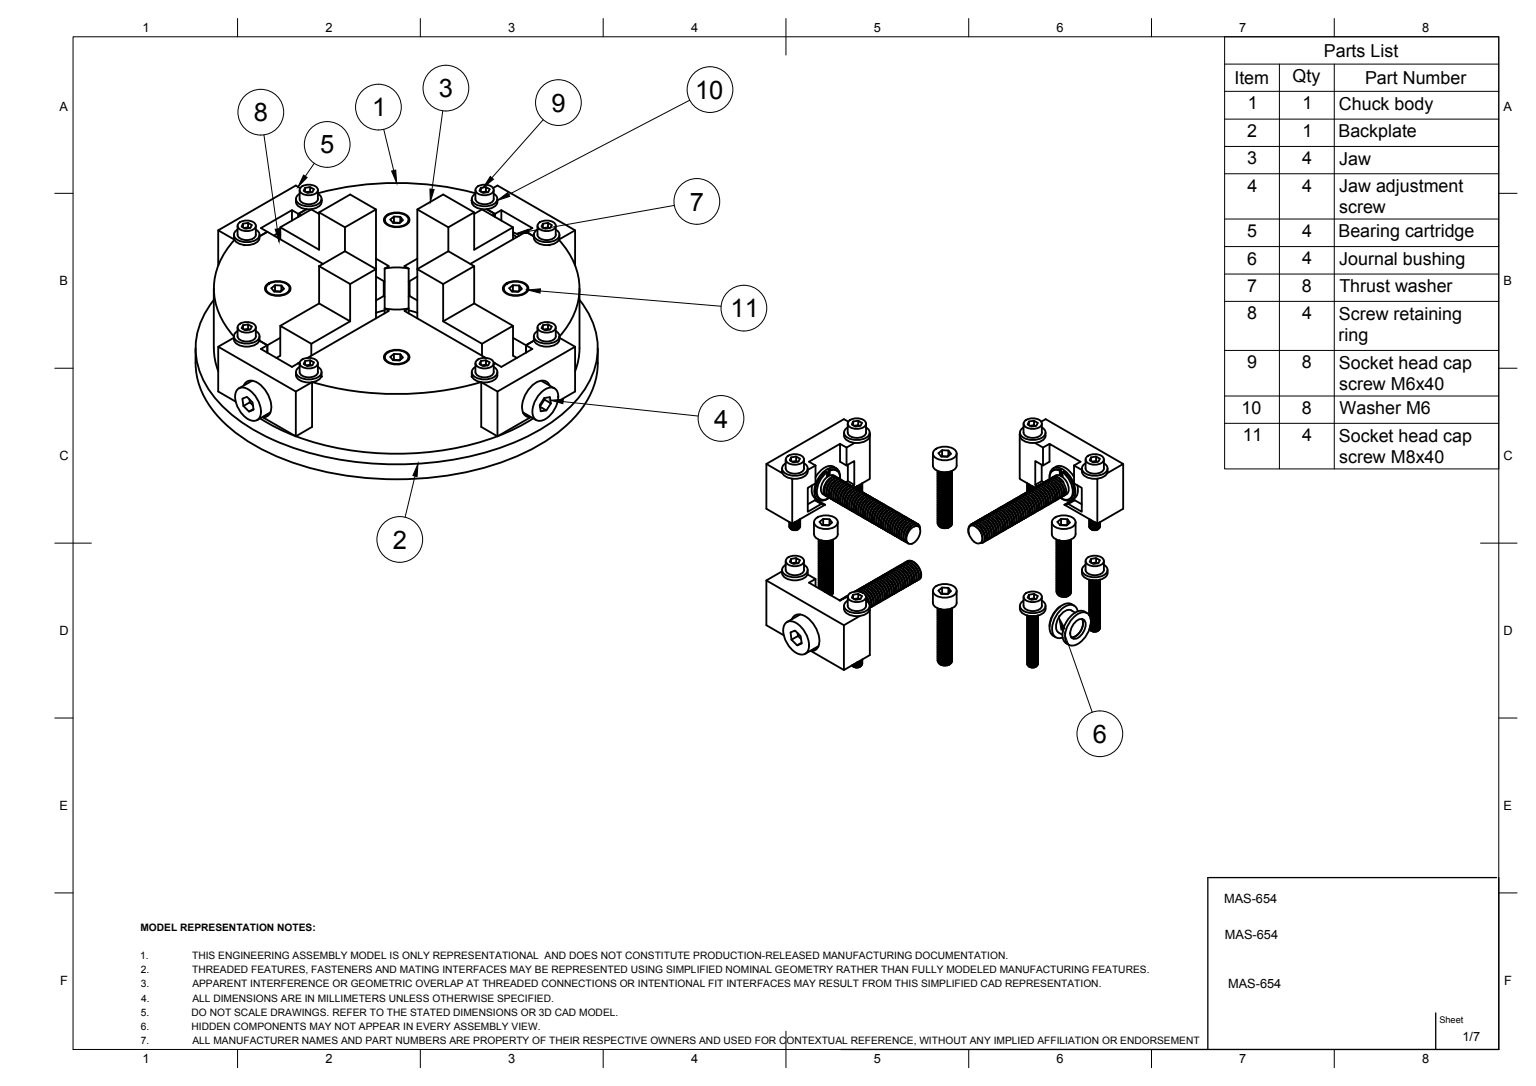
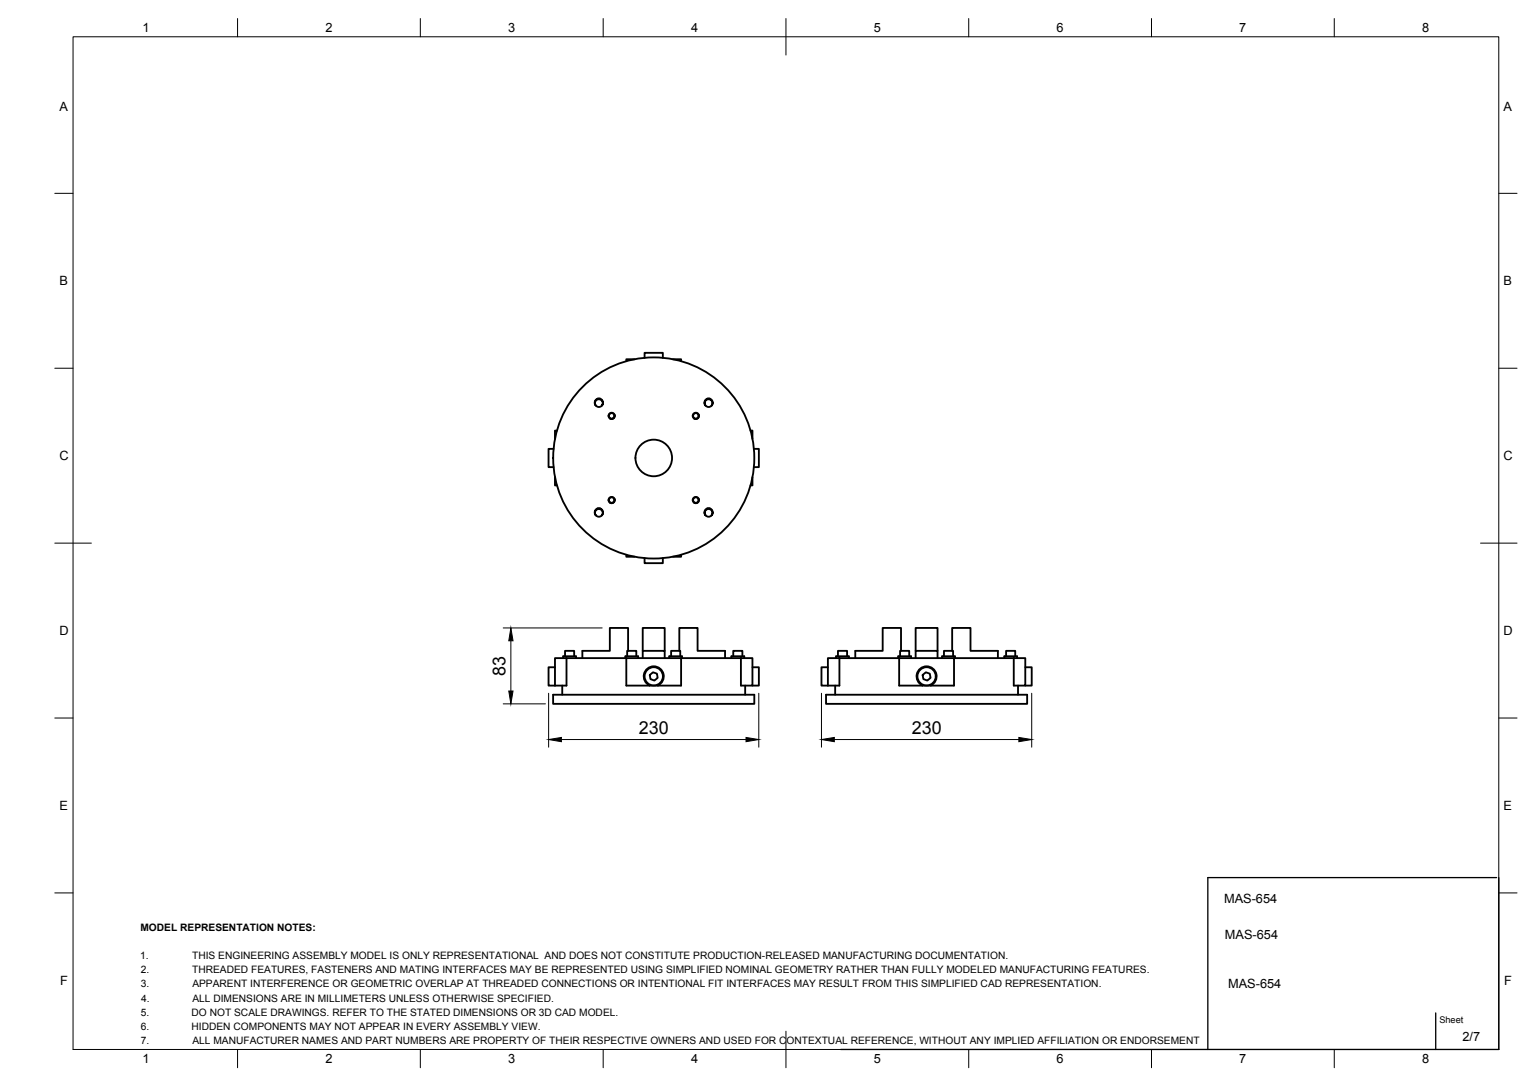
ISO-10303-21;
HEADER;
/* Generated by software containing ST-Developer
 * from STEP Tools, Inc. (www.steptools.com) 
 */

FILE_DESCRIPTION(
/* description */ ('Independent four-jaw lathe chuck,200mm body,40mm bore,36\X2\2013\X0\7
6mm nominal opposed jaw opening. Four shared machined T-jaws and model
ed partial M12x1.75 feed screws, native independent screw/slider links
, removable bolted bronze-bearing cartridges, fully captured ring/wash
er/head thrust stacks and registered bolted backplate. Custom spindle 
interface; no compatibility, speed, grip force or safety rating assign
ed.'),
/* implementation_level */ '2;1');

FILE_NAME(
/* name */ 'MAS-654.step',
/* time_stamp */ '2026-11-09T20:24:54-08:00',
/* author */ (''),
/* organization */ (''),
/* preprocessor_version */ 'ST-DEVELOPER v20.2',
/* originating_system */ 'Autodesk Translation Framework v15.17.0.0',
/* authorisation */ '');

FILE_SCHEMA (('AUTOMOTIVE_DESIGN { 1 0 10303 214 3 1 1 }'));
ENDSEC;

DATA;
#10=MECHANICAL_DESIGN_GEOMETRIC_PRESENTATION_REPRESENTATION('',(#236,#237,
#238,#239,#240,#241,#242,#243,#244,#245,#246),#69491);
#11=ITEM_DEFINED_TRANSFORMATION($,$,#14865,#15813);
#12=ITEM_DEFINED_TRANSFORMATION($,$,#15193,#15814);
#13=ITEM_DEFINED_TRANSFORMATION($,$,#15370,#15815);
#14=ITEM_DEFINED_TRANSFORMATION($,$,#15482,#15816);
#15=ITEM_DEFINED_TRANSFORMATION($,$,#15446,#15817);
#16=ITEM_DEFINED_TRANSFORMATION($,$,#15597,#15818);
#17=ITEM_DEFINED_TRANSFORMATION($,$,#15606,#15819);
#18=ITEM_DEFINED_TRANSFORMATION($,$,#15586,#15820);
#19=ITEM_DEFINED_TRANSFORMATION($,$,#15615,#15821);
#20=ITEM_DEFINED_TRANSFORMATION($,$,#15715,#15822);
#21=ITEM_DEFINED_TRANSFORMATION($,$,#15724,#15823);
#22=ITEM_DEFINED_TRANSFORMATION($,$,#15606,#15824);
#23=ITEM_DEFINED_TRANSFORMATION($,$,#15615,#15825);
#24=ITEM_DEFINED_TRANSFORMATION($,$,#15715,#15826);
#25=ITEM_DEFINED_TRANSFORMATION($,$,#15370,#15827);
#26=ITEM_DEFINED_TRANSFORMATION($,$,#15446,#15828);
#27=ITEM_DEFINED_TRANSFORMATION($,$,#15482,#15829);
#28=ITEM_DEFINED_TRANSFORMATION($,$,#15586,#15830);
#29=ITEM_DEFINED_TRANSFORMATION($,$,#15597,#15831);
#30=ITEM_DEFINED_TRANSFORMATION($,$,#15606,#15832);
#31=ITEM_DEFINED_TRANSFORMATION($,$,#15606,#15833);
#32=ITEM_DEFINED_TRANSFORMATION($,$,#15615,#15834);
#33=ITEM_DEFINED_TRANSFORMATION($,$,#15715,#15835);
#34=ITEM_DEFINED_TRANSFORMATION($,$,#15615,#15836);
#35=ITEM_DEFINED_TRANSFORMATION($,$,#15715,#15837);
#36=ITEM_DEFINED_TRANSFORMATION($,$,#15370,#15838);
#37=ITEM_DEFINED_TRANSFORMATION($,$,#15446,#15839);
#38=ITEM_DEFINED_TRANSFORMATION($,$,#15482,#15840);
#39=ITEM_DEFINED_TRANSFORMATION($,$,#15586,#15841);
#40=ITEM_DEFINED_TRANSFORMATION($,$,#15597,#15842);
#41=ITEM_DEFINED_TRANSFORMATION($,$,#15606,#15843);
#42=ITEM_DEFINED_TRANSFORMATION($,$,#15606,#15844);
#43=ITEM_DEFINED_TRANSFORMATION($,$,#15615,#15845);
#44=ITEM_DEFINED_TRANSFORMATION($,$,#15715,#15846);
#45=ITEM_DEFINED_TRANSFORMATION($,$,#15615,#15847);
#46=ITEM_DEFINED_TRANSFORMATION($,$,#15715,#15848);
#47=ITEM_DEFINED_TRANSFORMATION($,$,#15370,#15849);
#48=ITEM_DEFINED_TRANSFORMATION($,$,#15446,#15850);
#49=ITEM_DEFINED_TRANSFORMATION($,$,#15482,#15851);
#50=ITEM_DEFINED_TRANSFORMATION($,$,#15586,#15852);
#51=ITEM_DEFINED_TRANSFORMATION($,$,#15597,#15853);
#52=ITEM_DEFINED_TRANSFORMATION($,$,#15606,#15854);
#53=ITEM_DEFINED_TRANSFORMATION($,$,#15606,#15855);
#54=ITEM_DEFINED_TRANSFORMATION($,$,#15615,#15856);
#55=ITEM_DEFINED_TRANSFORMATION($,$,#15715,#15857);
#56=ITEM_DEFINED_TRANSFORMATION($,$,#15615,#15858);
#57=ITEM_DEFINED_TRANSFORMATION($,$,#15715,#15859);
#58=ITEM_DEFINED_TRANSFORMATION($,$,#15724,#15860);
#59=ITEM_DEFINED_TRANSFORMATION($,$,#15724,#15861);
#60=ITEM_DEFINED_TRANSFORMATION($,$,#15724,#15862);
#61=(
REPRESENTATION_RELATIONSHIP($,$,#69571,#69570)
REPRESENTATION_RELATIONSHIP_WITH_TRANSFORMATION(#11)
SHAPE_REPRESENTATION_RELATIONSHIP()
);
#62=(
REPRESENTATION_RELATIONSHIP($,$,#69572,#69570)
REPRESENTATION_RELATIONSHIP_WITH_TRANSFORMATION(#12)
SHAPE_REPRESENTATION_RELATIONSHIP()
);
#63=(
REPRESENTATION_RELATIONSHIP($,$,#69573,#69570)
REPRESENTATION_RELATIONSHIP_WITH_TRANSFORMATION(#13)
SHAPE_REPRESENTATION_RELATIONSHIP()
);
#64=(
REPRESENTATION_RELATIONSHIP($,$,#69575,#69570)
REPRESENTATION_RELATIONSHIP_WITH_TRANSFORMATION(#14)
SHAPE_REPRESENTATION_RELATIONSHIP()
);
#65=(
REPRESENTATION_RELATIONSHIP($,$,#69574,#69570)
REPRESENTATION_RELATIONSHIP_WITH_TRANSFORMATION(#15)
SHAPE_REPRESENTATION_RELATIONSHIP()
);
#66=(
REPRESENTATION_RELATIONSHIP($,$,#69577,#69570)
REPRESENTATION_RELATIONSHIP_WITH_TRANSFORMATION(#16)
SHAPE_REPRESENTATION_RELATIONSHIP()
);
#67=(
REPRESENTATION_RELATIONSHIP($,$,#69578,#69570)
REPRESENTATION_RELATIONSHIP_WITH_TRANSFORMATION(#17)
SHAPE_REPRESENTATION_RELATIONSHIP()
);
#68=(
REPRESENTATION_RELATIONSHIP($,$,#69576,#69570)
REPRESENTATION_RELATIONSHIP_WITH_TRANSFORMATION(#18)
SHAPE_REPRESENTATION_RELATIONSHIP()
);
#69=(
REPRESENTATION_RELATIONSHIP($,$,#69579,#69570)
REPRESENTATION_RELATIONSHIP_WITH_TRANSFORMATION(#19)
SHAPE_REPRESENTATION_RELATIONSHIP()
);
#70=(
REPRESENTATION_RELATIONSHIP($,$,#69580,#69570)
REPRESENTATION_RELATIONSHIP_WITH_TRANSFORMATION(#20)
SHAPE_REPRESENTATION_RELATIONSHIP()
);
#71=(
REPRESENTATION_RELATIONSHIP($,$,#69581,#69570)
REPRESENTATION_RELATIONSHIP_WITH_TRANSFORMATION(#21)
SHAPE_REPRESENTATION_RELATIONSHIP()
);
#72=(
REPRESENTATION_RELATIONSHIP($,$,#69578,#69570)
REPRESENTATION_RELATIONSHIP_WITH_TRANSFORMATION(#22)
SHAPE_REPRESENTATION_RELATIONSHIP()
);
#73=(
REPRESENTATION_RELATIONSHIP($,$,#69579,#69570)
REPRESENTATION_RELATIONSHIP_WITH_TRANSFORMATION(#23)
SHAPE_REPRESENTATION_RELATIONSHIP()
);
#74=(
REPRESENTATION_RELATIONSHIP($,$,#69580,#69570)
REPRESENTATION_RELATIONSHIP_WITH_TRANSFORMATION(#24)
SHAPE_REPRESENTATION_RELATIONSHIP()
);
#75=(
REPRESENTATION_RELATIONSHIP($,$,#69573,#69570)
REPRESENTATION_RELATIONSHIP_WITH_TRANSFORMATION(#25)
SHAPE_REPRESENTATION_RELATIONSHIP()
);
#76=(
REPRESENTATION_RELATIONSHIP($,$,#69574,#69570)
REPRESENTATION_RELATIONSHIP_WITH_TRANSFORMATION(#26)
SHAPE_REPRESENTATION_RELATIONSHIP()
);
#77=(
REPRESENTATION_RELATIONSHIP($,$,#69575,#69570)
REPRESENTATION_RELATIONSHIP_WITH_TRANSFORMATION(#27)
SHAPE_REPRESENTATION_RELATIONSHIP()
);
#78=(
REPRESENTATION_RELATIONSHIP($,$,#69576,#69570)
REPRESENTATION_RELATIONSHIP_WITH_TRANSFORMATION(#28)
SHAPE_REPRESENTATION_RELATIONSHIP()
);
#79=(
REPRESENTATION_RELATIONSHIP($,$,#69577,#69570)
REPRESENTATION_RELATIONSHIP_WITH_TRANSFORMATION(#29)
SHAPE_REPRESENTATION_RELATIONSHIP()
);
#80=(
REPRESENTATION_RELATIONSHIP($,$,#69578,#69570)
REPRESENTATION_RELATIONSHIP_WITH_TRANSFORMATION(#30)
SHAPE_REPRESENTATION_RELATIONSHIP()
);
#81=(
REPRESENTATION_RELATIONSHIP($,$,#69578,#69570)
REPRESENTATION_RELATIONSHIP_WITH_TRANSFORMATION(#31)
SHAPE_REPRESENTATION_RELATIONSHIP()
);
#82=(
REPRESENTATION_RELATIONSHIP($,$,#69579,#69570)
REPRESENTATION_RELATIONSHIP_WITH_TRANSFORMATION(#32)
SHAPE_REPRESENTATION_RELATIONSHIP()
);
#83=(
REPRESENTATION_RELATIONSHIP($,$,#69580,#69570)
REPRESENTATION_RELATIONSHIP_WITH_TRANSFORMATION(#33)
SHAPE_REPRESENTATION_RELATIONSHIP()
);
#84=(
REPRESENTATION_RELATIONSHIP($,$,#69579,#69570)
REPRESENTATION_RELATIONSHIP_WITH_TRANSFORMATION(#34)
SHAPE_REPRESENTATION_RELATIONSHIP()
);
#85=(
REPRESENTATION_RELATIONSHIP($,$,#69580,#69570)
REPRESENTATION_RELATIONSHIP_WITH_TRANSFORMATION(#35)
SHAPE_REPRESENTATION_RELATIONSHIP()
);
#86=(
REPRESENTATION_RELATIONSHIP($,$,#69573,#69570)
REPRESENTATION_RELATIONSHIP_WITH_TRANSFORMATION(#36)
SHAPE_REPRESENTATION_RELATIONSHIP()
);
#87=(
REPRESENTATION_RELATIONSHIP($,$,#69574,#69570)
REPRESENTATION_RELATIONSHIP_WITH_TRANSFORMATION(#37)
SHAPE_REPRESENTATION_RELATIONSHIP()
);
#88=(
REPRESENTATION_RELATIONSHIP($,$,#69575,#69570)
REPRESENTATION_RELATIONSHIP_WITH_TRANSFORMATION(#38)
SHAPE_REPRESENTATION_RELATIONSHIP()
);
#89=(
REPRESENTATION_RELATIONSHIP($,$,#69576,#69570)
REPRESENTATION_RELATIONSHIP_WITH_TRANSFORMATION(#39)
SHAPE_REPRESENTATION_RELATIONSHIP()
);
#90=(
REPRESENTATION_RELATIONSHIP($,$,#69577,#69570)
REPRESENTATION_RELATIONSHIP_WITH_TRANSFORMATION(#40)
SHAPE_REPRESENTATION_RELATIONSHIP()
);
#91=(
REPRESENTATION_RELATIONSHIP($,$,#69578,#69570)
REPRESENTATION_RELATIONSHIP_WITH_TRANSFORMATION(#41)
SHAPE_REPRESENTATION_RELATIONSHIP()
);
#92=(
REPRESENTATION_RELATIONSHIP($,$,#69578,#69570)
REPRESENTATION_RELATIONSHIP_WITH_TRANSFORMATION(#42)
SHAPE_REPRESENTATION_RELATIONSHIP()
);
#93=(
REPRESENTATION_RELATIONSHIP($,$,#69579,#69570)
REPRESENTATION_RELATIONSHIP_WITH_TRANSFORMATION(#43)
SHAPE_REPRESENTATION_RELATIONSHIP()
);
#94=(
REPRESENTATION_RELATIONSHIP($,$,#69580,#69570)
REPRESENTATION_RELATIONSHIP_WITH_TRANSFORMATION(#44)
SHAPE_REPRESENTATION_RELATIONSHIP()
);
#95=(
REPRESENTATION_RELATIONSHIP($,$,#69579,#69570)
REPRESENTATION_RELATIONSHIP_WITH_TRANSFORMATION(#45)
SHAPE_REPRESENTATION_RELATIONSHIP()
);
#96=(
REPRESENTATION_RELATIONSHIP($,$,#69580,#69570)
REPRESENTATION_RELATIONSHIP_WITH_TRANSFORMATION(#46)
SHAPE_REPRESENTATION_RELATIONSHIP()
);
#97=(
REPRESENTATION_RELATIONSHIP($,$,#69573,#69570)
REPRESENTATION_RELATIONSHIP_WITH_TRANSFORMATION(#47)
SHAPE_REPRESENTATION_RELATIONSHIP()
);
#98=(
REPRESENTATION_RELATIONSHIP($,$,#69574,#69570)
REPRESENTATION_RELATIONSHIP_WITH_TRANSFORMATION(#48)
SHAPE_REPRESENTATION_RELATIONSHIP()
);
#99=(
REPRESENTATION_RELATIONSHIP($,$,#69575,#69570)
REPRESENTATION_RELATIONSHIP_WITH_TRANSFORMATION(#49)
SHAPE_REPRESENTATION_RELATIONSHIP()
);
#100=(
REPRESENTATION_RELATIONSHIP($,$,#69576,#69570)
REPRESENTATION_RELATIONSHIP_WITH_TRANSFORMATION(#50)
SHAPE_REPRESENTATION_RELATIONSHIP()
);
#101=(
REPRESENTATION_RELATIONSHIP($,$,#69577,#69570)
REPRESENTATION_RELATIONSHIP_WITH_TRANSFORMATION(#51)
SHAPE_REPRESENTATION_RELATIONSHIP()
);
#102=(
REPRESENTATION_RELATIONSHIP($,$,#69578,#69570)
REPRESENTATION_RELATIONSHIP_WITH_TRANSFORMATION(#52)
SHAPE_REPRESENTATION_RELATIONSHIP()
);
#103=(
REPRESENTATION_RELATIONSHIP($,$,#69578,#69570)
REPRESENTATION_RELATIONSHIP_WITH_TRANSFORMATION(#53)
SHAPE_REPRESENTATION_RELATIONSHIP()
);
#104=(
REPRESENTATION_RELATIONSHIP($,$,#69579,#69570)
REPRESENTATION_RELATIONSHIP_WITH_TRANSFORMATION(#54)
SHAPE_REPRESENTATION_RELATIONSHIP()
);
#105=(
REPRESENTATION_RELATIONSHIP($,$,#69580,#69570)
REPRESENTATION_RELATIONSHIP_WITH_TRANSFORMATION(#55)
SHAPE_REPRESENTATION_RELATIONSHIP()
);
#106=(
REPRESENTATION_RELATIONSHIP($,$,#69579,#69570)
REPRESENTATION_RELATIONSHIP_WITH_TRANSFORMATION(#56)
SHAPE_REPRESENTATION_RELATIONSHIP()
);
#107=(
REPRESENTATION_RELATIONSHIP($,$,#69580,#69570)
REPRESENTATION_RELATIONSHIP_WITH_TRANSFORMATION(#57)
SHAPE_REPRESENTATION_RELATIONSHIP()
);
#108=(
REPRESENTATION_RELATIONSHIP($,$,#69581,#69570)
REPRESENTATION_RELATIONSHIP_WITH_TRANSFORMATION(#58)
SHAPE_REPRESENTATION_RELATIONSHIP()
);
#109=(
REPRESENTATION_RELATIONSHIP($,$,#69581,#69570)
REPRESENTATION_RELATIONSHIP_WITH_TRANSFORMATION(#59)
SHAPE_REPRESENTATION_RELATIONSHIP()
);
#110=(
REPRESENTATION_RELATIONSHIP($,$,#69581,#69570)
REPRESENTATION_RELATIONSHIP_WITH_TRANSFORMATION(#60)
SHAPE_REPRESENTATION_RELATIONSHIP()
);
#111=CONTEXT_DEPENDENT_SHAPE_REPRESENTATION(#61,#69520);
#112=CONTEXT_DEPENDENT_SHAPE_REPRESENTATION(#62,#69521);
#113=CONTEXT_DEPENDENT_SHAPE_REPRESENTATION(#63,#69522);
#114=CONTEXT_DEPENDENT_SHAPE_REPRESENTATION(#64,#69523);
#115=CONTEXT_DEPENDENT_SHAPE_REPRESENTATION(#65,#69524);
#116=CONTEXT_DEPENDENT_SHAPE_REPRESENTATION(#66,#69525);
#117=CONTEXT_DEPENDENT_SHAPE_REPRESENTATION(#67,#69526);
#118=CONTEXT_DEPENDENT_SHAPE_REPRESENTATION(#68,#69527);
#119=CONTEXT_DEPENDENT_SHAPE_REPRESENTATION(#69,#69528);
#120=CONTEXT_DEPENDENT_SHAPE_REPRESENTATION(#70,#69529);
#121=CONTEXT_DEPENDENT_SHAPE_REPRESENTATION(#71,#69530);
#122=CONTEXT_DEPENDENT_SHAPE_REPRESENTATION(#72,#69531);
#123=CONTEXT_DEPENDENT_SHAPE_REPRESENTATION(#73,#69532);
#124=CONTEXT_DEPENDENT_SHAPE_REPRESENTATION(#74,#69533);
#125=CONTEXT_DEPENDENT_SHAPE_REPRESENTATION(#75,#69534);
#126=CONTEXT_DEPENDENT_SHAPE_REPRESENTATION(#76,#69535);
#127=CONTEXT_DEPENDENT_SHAPE_REPRESENTATION(#77,#69536);
#128=CONTEXT_DEPENDENT_SHAPE_REPRESENTATION(#78,#69537);
#129=CONTEXT_DEPENDENT_SHAPE_REPRESENTATION(#79,#69538);
#130=CONTEXT_DEPENDENT_SHAPE_REPRESENTATION(#80,#69539);
#131=CONTEXT_DEPENDENT_SHAPE_REPRESENTATION(#81,#69540);
#132=CONTEXT_DEPENDENT_SHAPE_REPRESENTATION(#82,#69541);
#133=CONTEXT_DEPENDENT_SHAPE_REPRESENTATION(#83,#69542);
#134=CONTEXT_DEPENDENT_SHAPE_REPRESENTATION(#84,#69543);
#135=CONTEXT_DEPENDENT_SHAPE_REPRESENTATION(#85,#69544);
#136=CONTEXT_DEPENDENT_SHAPE_REPRESENTATION(#86,#69545);
#137=CONTEXT_DEPENDENT_SHAPE_REPRESENTATION(#87,#69546);
#138=CONTEXT_DEPENDENT_SHAPE_REPRESENTATION(#88,#69547);
#139=CONTEXT_DEPENDENT_SHAPE_REPRESENTATION(#89,#69548);
#140=CONTEXT_DEPENDENT_SHAPE_REPRESENTATION(#90,#69549);
#141=CONTEXT_DEPENDENT_SHAPE_REPRESENTATION(#91,#69550);
#142=CONTEXT_DEPENDENT_SHAPE_REPRESENTATION(#92,#69551);
#143=CONTEXT_DEPENDENT_SHAPE_REPRESENTATION(#93,#69552);
#144=CONTEXT_DEPENDENT_SHAPE_REPRESENTATION(#94,#69553);
#145=CONTEXT_DEPENDENT_SHAPE_REPRESENTATION(#95,#69554);
#146=CONTEXT_DEPENDENT_SHAPE_REPRESENTATION(#96,#69555);
#147=CONTEXT_DEPENDENT_SHAPE_REPRESENTATION(#97,#69556);
#148=CONTEXT_DEPENDENT_SHAPE_REPRESENTATION(#98,#69557);
#149=CONTEXT_DEPENDENT_SHAPE_REPRESENTATION(#99,#69558);
#150=CONTEXT_DEPENDENT_SHAPE_REPRESENTATION(#100,#69559);
#151=CONTEXT_DEPENDENT_SHAPE_REPRESENTATION(#101,#69560);
#152=CONTEXT_DEPENDENT_SHAPE_REPRESENTATION(#102,#69561);
#153=CONTEXT_DEPENDENT_SHAPE_REPRESENTATION(#103,#69562);
#154=CONTEXT_DEPENDENT_SHAPE_REPRESENTATION(#104,#69563);
#155=CONTEXT_DEPENDENT_SHAPE_REPRESENTATION(#105,#69564);
#156=CONTEXT_DEPENDENT_SHAPE_REPRESENTATION(#106,#69565);
#157=CONTEXT_DEPENDENT_SHAPE_REPRESENTATION(#107,#69566);
#158=CONTEXT_DEPENDENT_SHAPE_REPRESENTATION(#108,#69567);
#159=CONTEXT_DEPENDENT_SHAPE_REPRESENTATION(#109,#69568);
#160=CONTEXT_DEPENDENT_SHAPE_REPRESENTATION(#110,#69569);
#161=NEXT_ASSEMBLY_USAGE_OCCURRENCE('Chuck body:1','Chuck body:1',
'Chuck body:1',#69583,#69584,'Chuck body:1');
#162=NEXT_ASSEMBLY_USAGE_OCCURRENCE('Backplate:1','Backplate:1',
'Backplate:1',#69583,#69585,'Backplate:1');
#163=NEXT_ASSEMBLY_USAGE_OCCURRENCE('Jaw:1','Jaw:1','Jaw:1',#69583,#69586,
'Jaw:1');
#164=NEXT_ASSEMBLY_USAGE_OCCURRENCE('Jaw adjustment screw:1',
'Jaw adjustment screw:1','Jaw adjustment screw:1',#69583,#69588,
'Jaw adjustment screw:1');
#165=NEXT_ASSEMBLY_USAGE_OCCURRENCE('Bearing cartridge:1',
'Bearing cartridge:1','Bearing cartridge:1',#69583,#69587,
'Bearing cartridge:1');
#166=NEXT_ASSEMBLY_USAGE_OCCURRENCE('Journal bushing:1',
'Journal bushing:1','Journal bushing:1',#69583,#69590,
'Journal bushing:1');
#167=NEXT_ASSEMBLY_USAGE_OCCURRENCE('Thrust washer:1','Thrust washer:1',
'Thrust washer:1',#69583,#69591,'Thrust washer:1');
#168=NEXT_ASSEMBLY_USAGE_OCCURRENCE('Screw retaining ring:1',
'Screw retaining ring:1','Screw retaining ring:1',#69583,#69589,
'Screw retaining ring:1');
#169=NEXT_ASSEMBLY_USAGE_OCCURRENCE('Socket head cap screw M6x40:1',
'Socket head cap screw M6x40:1','Socket head cap screw M6x40:1',#69583,
#69592,'Socket head cap screw M6x40:1');
#170=NEXT_ASSEMBLY_USAGE_OCCURRENCE('Washer M6:1','Washer M6:1',
'Washer M6:1',#69583,#69593,'Washer M6:1');
#171=NEXT_ASSEMBLY_USAGE_OCCURRENCE('Socket head cap screw M8x40:1',
'Socket head cap screw M8x40:1','Socket head cap screw M8x40:1',#69583,
#69594,'Socket head cap screw M8x40:1');
#172=NEXT_ASSEMBLY_USAGE_OCCURRENCE('Thrust washer:2','Thrust washer:2',
'Thrust washer:2',#69583,#69591,'Thrust washer:2');
#173=NEXT_ASSEMBLY_USAGE_OCCURRENCE('Socket head cap screw M6x40:2',
'Socket head cap screw M6x40:2','Socket head cap screw M6x40:2',#69583,
#69592,'Socket head cap screw M6x40:2');
#174=NEXT_ASSEMBLY_USAGE_OCCURRENCE('Washer M6:2','Washer M6:2',
'Washer M6:2',#69583,#69593,'Washer M6:2');
#175=NEXT_ASSEMBLY_USAGE_OCCURRENCE('Jaw:2','Jaw:2','Jaw:2',#69583,#69586,
'Jaw:2');
#176=NEXT_ASSEMBLY_USAGE_OCCURRENCE('Bearing cartridge:2',
'Bearing cartridge:2','Bearing cartridge:2',#69583,#69587,
'Bearing cartridge:2');
#177=NEXT_ASSEMBLY_USAGE_OCCURRENCE('Jaw adjustment screw:2',
'Jaw adjustment screw:2','Jaw adjustment screw:2',#69583,#69588,
'Jaw adjustment screw:2');
#178=NEXT_ASSEMBLY_USAGE_OCCURRENCE('Screw retaining ring:2',
'Screw retaining ring:2','Screw retaining ring:2',#69583,#69589,
'Screw retaining ring:2');
#179=NEXT_ASSEMBLY_USAGE_OCCURRENCE('Journal bushing:2',
'Journal bushing:2','Journal bushing:2',#69583,#69590,
'Journal bushing:2');
#180=NEXT_ASSEMBLY_USAGE_OCCURRENCE('Thrust washer:3','Thrust washer:3',
'Thrust washer:3',#69583,#69591,'Thrust washer:3');
#181=NEXT_ASSEMBLY_USAGE_OCCURRENCE('Thrust washer:4','Thrust washer:4',
'Thrust washer:4',#69583,#69591,'Thrust washer:4');
#182=NEXT_ASSEMBLY_USAGE_OCCURRENCE('Socket head cap screw M6x40:3',
'Socket head cap screw M6x40:3','Socket head cap screw M6x40:3',#69583,
#69592,'Socket head cap screw M6x40:3');
#183=NEXT_ASSEMBLY_USAGE_OCCURRENCE('Washer M6:3','Washer M6:3',
'Washer M6:3',#69583,#69593,'Washer M6:3');
#184=NEXT_ASSEMBLY_USAGE_OCCURRENCE('Socket head cap screw M6x40:4',
'Socket head cap screw M6x40:4','Socket head cap screw M6x40:4',#69583,
#69592,'Socket head cap screw M6x40:4');
#185=NEXT_ASSEMBLY_USAGE_OCCURRENCE('Washer M6:4','Washer M6:4',
'Washer M6:4',#69583,#69593,'Washer M6:4');
#186=NEXT_ASSEMBLY_USAGE_OCCURRENCE('Jaw:3','Jaw:3','Jaw:3',#69583,#69586,
'Jaw:3');
#187=NEXT_ASSEMBLY_USAGE_OCCURRENCE('Bearing cartridge:3',
'Bearing cartridge:3','Bearing cartridge:3',#69583,#69587,
'Bearing cartridge:3');
#188=NEXT_ASSEMBLY_USAGE_OCCURRENCE('Jaw adjustment screw:3',
'Jaw adjustment screw:3','Jaw adjustment screw:3',#69583,#69588,
'Jaw adjustment screw:3');
#189=NEXT_ASSEMBLY_USAGE_OCCURRENCE('Screw retaining ring:3',
'Screw retaining ring:3','Screw retaining ring:3',#69583,#69589,
'Screw retaining ring:3');
#190=NEXT_ASSEMBLY_USAGE_OCCURRENCE('Journal bushing:3',
'Journal bushing:3','Journal bushing:3',#69583,#69590,
'Journal bushing:3');
#191=NEXT_ASSEMBLY_USAGE_OCCURRENCE('Thrust washer:5','Thrust washer:5',
'Thrust washer:5',#69583,#69591,'Thrust washer:5');
#192=NEXT_ASSEMBLY_USAGE_OCCURRENCE('Thrust washer:6','Thrust washer:6',
'Thrust washer:6',#69583,#69591,'Thrust washer:6');
#193=NEXT_ASSEMBLY_USAGE_OCCURRENCE('Socket head cap screw M6x40:5',
'Socket head cap screw M6x40:5','Socket head cap screw M6x40:5',#69583,
#69592,'Socket head cap screw M6x40:5');
#194=NEXT_ASSEMBLY_USAGE_OCCURRENCE('Washer M6:5','Washer M6:5',
'Washer M6:5',#69583,#69593,'Washer M6:5');
#195=NEXT_ASSEMBLY_USAGE_OCCURRENCE('Socket head cap screw M6x40:6',
'Socket head cap screw M6x40:6','Socket head cap screw M6x40:6',#69583,
#69592,'Socket head cap screw M6x40:6');
#196=NEXT_ASSEMBLY_USAGE_OCCURRENCE('Washer M6:6','Washer M6:6',
'Washer M6:6',#69583,#69593,'Washer M6:6');
#197=NEXT_ASSEMBLY_USAGE_OCCURRENCE('Jaw:4','Jaw:4','Jaw:4',#69583,#69586,
'Jaw:4');
#198=NEXT_ASSEMBLY_USAGE_OCCURRENCE('Bearing cartridge:4',
'Bearing cartridge:4','Bearing cartridge:4',#69583,#69587,
'Bearing cartridge:4');
#199=NEXT_ASSEMBLY_USAGE_OCCURRENCE('Jaw adjustment screw:4',
'Jaw adjustment screw:4','Jaw adjustment screw:4',#69583,#69588,
'Jaw adjustment screw:4');
#200=NEXT_ASSEMBLY_USAGE_OCCURRENCE('Screw retaining ring:4',
'Screw retaining ring:4','Screw retaining ring:4',#69583,#69589,
'Screw retaining ring:4');
#201=NEXT_ASSEMBLY_USAGE_OCCURRENCE('Journal bushing:4',
'Journal bushing:4','Journal bushing:4',#69583,#69590,
'Journal bushing:4');
#202=NEXT_ASSEMBLY_USAGE_OCCURRENCE('Thrust washer:7','Thrust washer:7',
'Thrust washer:7',#69583,#69591,'Thrust washer:7');
#203=NEXT_ASSEMBLY_USAGE_OCCURRENCE('Thrust washer:8','Thrust washer:8',
'Thrust washer:8',#69583,#69591,'Thrust washer:8');
#204=NEXT_ASSEMBLY_USAGE_OCCURRENCE('Socket head cap screw M6x40:7',
'Socket head cap screw M6x40:7','Socket head cap screw M6x40:7',#69583,
#69592,'Socket head cap screw M6x40:7');
#205=NEXT_ASSEMBLY_USAGE_OCCURRENCE('Washer M6:7','Washer M6:7',
'Washer M6:7',#69583,#69593,'Washer M6:7');
#206=NEXT_ASSEMBLY_USAGE_OCCURRENCE('Socket head cap screw M6x40:8',
'Socket head cap screw M6x40:8','Socket head cap screw M6x40:8',#69583,
#69592,'Socket head cap screw M6x40:8');
#207=NEXT_ASSEMBLY_USAGE_OCCURRENCE('Washer M6:8','Washer M6:8',
'Washer M6:8',#69583,#69593,'Washer M6:8');
#208=NEXT_ASSEMBLY_USAGE_OCCURRENCE('Socket head cap screw M8x40:2',
'Socket head cap screw M8x40:2','Socket head cap screw M8x40:2',#69583,
#69594,'Socket head cap screw M8x40:2');
#209=NEXT_ASSEMBLY_USAGE_OCCURRENCE('Socket head cap screw M8x40:3',
'Socket head cap screw M8x40:3','Socket head cap screw M8x40:3',#69583,
#69594,'Socket head cap screw M8x40:3');
#210=NEXT_ASSEMBLY_USAGE_OCCURRENCE('Socket head cap screw M8x40:4',
'Socket head cap screw M8x40:4','Socket head cap screw M8x40:4',#69583,
#69594,'Socket head cap screw M8x40:4');
#211=CONICAL_SURFACE('',#15696,2.5,0.785398163397448);
#212=CONICAL_SURFACE('',#15793,3.5,0.785398163397448);
#213=CONICAL_SURFACE('',#15796,3.5,0.785398163397448);
#214=SHAPE_REPRESENTATION_RELATIONSHIP('SRR','None',#69571,#225);
#215=SHAPE_REPRESENTATION_RELATIONSHIP('SRR','None',#69572,#226);
#216=SHAPE_REPRESENTATION_RELATIONSHIP('SRR','None',#69573,#227);
#217=SHAPE_REPRESENTATION_RELATIONSHIP('SRR','None',#69574,#228);
#218=SHAPE_REPRESENTATION_RELATIONSHIP('SRR','None',#69575,#229);
#219=SHAPE_REPRESENTATION_RELATIONSHIP('SRR','None',#69576,#230);
#220=SHAPE_REPRESENTATION_RELATIONSHIP('SRR','None',#69577,#231);
#221=SHAPE_REPRESENTATION_RELATIONSHIP('SRR','None',#69578,#232);
#222=SHAPE_REPRESENTATION_RELATIONSHIP('SRR','None',#69579,#233);
#223=SHAPE_REPRESENTATION_RELATIONSHIP('SRR','None',#69580,#234);
#224=SHAPE_REPRESENTATION_RELATIONSHIP('SRR','None',#69581,#235);
#225=ADVANCED_BREP_SHAPE_REPRESENTATION('',(#247),#69480);
#226=ADVANCED_BREP_SHAPE_REPRESENTATION('',(#248),#69481);
#227=ADVANCED_BREP_SHAPE_REPRESENTATION('',(#249),#69482);
#228=ADVANCED_BREP_SHAPE_REPRESENTATION('',(#250),#69483);
#229=ADVANCED_BREP_SHAPE_REPRESENTATION('',(#251),#69484);
#230=ADVANCED_BREP_SHAPE_REPRESENTATION('',(#252),#69485);
#231=ADVANCED_BREP_SHAPE_REPRESENTATION('',(#253),#69486);
#232=ADVANCED_BREP_SHAPE_REPRESENTATION('',(#254),#69487);
#233=ADVANCED_BREP_SHAPE_REPRESENTATION('',(#255),#69488);
#234=ADVANCED_BREP_SHAPE_REPRESENTATION('',(#256),#69489);
#235=ADVANCED_BREP_SHAPE_REPRESENTATION('',(#257),#69490);
#236=STYLED_ITEM('',(#69635),#247);
#237=STYLED_ITEM('',(#69636),#248);
#238=STYLED_ITEM('',(#69637),#249);
#239=STYLED_ITEM('',(#69638),#250);
#240=STYLED_ITEM('',(#69639),#251);
#241=STYLED_ITEM('',(#69640),#252);
#242=STYLED_ITEM('',(#69641),#253);
#243=STYLED_ITEM('',(#69642),#254);
#244=STYLED_ITEM('',(#69640),#255);
#245=STYLED_ITEM('',(#69643),#256);
#246=STYLED_ITEM('',(#69640),#257);
#247=MANIFOLD_SOLID_BREP('Body1',#14731);
#248=MANIFOLD_SOLID_BREP('Body1',#14732);
#249=MANIFOLD_SOLID_BREP('Body1',#14733);
#250=MANIFOLD_SOLID_BREP('Body1',#14734);
#251=MANIFOLD_SOLID_BREP('Body1',#14735);
#252=MANIFOLD_SOLID_BREP('Body1',#14736);
#253=MANIFOLD_SOLID_BREP('Body1',#14737);
#254=MANIFOLD_SOLID_BREP('Body1',#14738);
#255=MANIFOLD_SOLID_BREP('Body1',#14739);
#256=MANIFOLD_SOLID_BREP('Body1',#14740);
#257=MANIFOLD_SOLID_BREP('Body1',#14741);
#258=B_SPLINE_SURFACE_WITH_KNOTS('',3,3,((#24006,#24007,#24008,#24009,#24010,
#24011,#24012,#24013,#24014,#24015,#24016,#24017,#24018,#24019,#24020,#24021,
#24022,#24023,#24024,#24025,#24026,#24027,#24028,#24029,#24030,#24031,#24032,
#24033,#24034,#24035,#24036,#24037,#24038,#24039,#24040,#24041,#24042,#24043,
#24044,#24045,#24046,#24047,#24048,#24049,#24050,#24051,#24052,#24053,#24054,
#24055,#24056,#24057,#24058,#24059,#24060,#24061,#24062,#24063,#24064,#24065,
#24066,#24067),(#24068,#24069,#24070,#24071,#24072,#24073,#24074,#24075,
#24076,#24077,#24078,#24079,#24080,#24081,#24082,#24083,#24084,#24085,#24086,
#24087,#24088,#24089,#24090,#24091,#24092,#24093,#24094,#24095,#24096,#24097,
#24098,#24099,#24100,#24101,#24102,#24103,#24104,#24105,#24106,#24107,#24108,
#24109,#24110,#24111,#24112,#24113,#24114,#24115,#24116,#24117,#24118,#24119,
#24120,#24121,#24122,#24123,#24124,#24125,#24126,#24127,#24128,#24129),
(#24130,#24131,#24132,#24133,#24134,#24135,#24136,#24137,#24138,#24139,
#24140,#24141,#24142,#24143,#24144,#24145,#24146,#24147,#24148,#24149,#24150,
#24151,#24152,#24153,#24154,#24155,#24156,#24157,#24158,#24159,#24160,#24161,
#24162,#24163,#24164,#24165,#24166,#24167,#24168,#24169,#24170,#24171,#24172,
#24173,#24174,#24175,#24176,#24177,#24178,#24179,#24180,#24181,#24182,#24183,
#24184,#24185,#24186,#24187,#24188,#24189,#24190,#24191),(#24192,#24193,
#24194,#24195,#24196,#24197,#24198,#24199,#24200,#24201,#24202,#24203,#24204,
#24205,#24206,#24207,#24208,#24209,#24210,#24211,#24212,#24213,#24214,#24215,
#24216,#24217,#24218,#24219,#24220,#24221,#24222,#24223,#24224,#24225,#24226,
#24227,#24228,#24229,#24230,#24231,#24232,#24233,#24234,#24235,#24236,#24237,
#24238,#24239,#24240,#24241,#24242,#24243,#24244,#24245,#24246,#24247,#24248,
#24249,#24250,#24251,#24252,#24253)),.UNSPECIFIED.,.F.,.F.,.F.,(4,4),(4,
1,1,1,1,1,1,1,1,1,1,1,1,1,1,1,1,1,1,1,1,1,1,1,1,1,1,1,1,1,1,1,1,1,1,1,1,
1,1,1,1,1,1,1,1,1,1,1,1,1,1,1,1,1,1,1,1,1,1,4),(0.,0.0642013499338865),
(11.8589888623078,12.8516263649797,13.8442638676517,14.8369013703236,15.8295388729956,
16.8221763756675,17.8148138783395,18.8074513810114,19.8000888836834,20.7927263863553,
21.7853638890272,22.7780013916992,23.7706388943711,24.7632763970431,25.755913899715,
26.748551402387,27.7411889050589,28.7338264077309,29.7264639104028,30.7191014130747,
31.7117389157467,32.7043764184186,33.6970139210906,34.6896514237625,35.6822889264345,
36.6749264291064,37.6675639317784,38.6602014344503,39.6528389371222,40.6454764397942,
41.6381139424661,42.6307514451381,43.62338894781,44.616026450482,45.6086639531539,
46.6013014558259,47.5939389584978,48.5865764611697,49.5792139638417,50.5718514665136,
51.5644889691856,52.5571264718575,53.5497639745295,54.5424014772014,55.5350389798734,
56.5276764825453,57.5203139852172,58.5129514878892,59.5055889905611,60.4982264932331,
61.490863995905,62.483501498577,63.4761390012489,64.4687765039209,65.4614140065928,
66.4540515092648,67.4466890119367,68.4393265146086,69.4319640172806,70.4246015199525),
 .UNSPECIFIED.);
#259=B_SPLINE_SURFACE_WITH_KNOTS('',3,3,((#24370,#24371,#24372,#24373,#24374,
#24375,#24376,#24377,#24378,#24379,#24380,#24381,#24382,#24383,#24384,#24385,
#24386,#24387,#24388,#24389,#24390,#24391,#24392,#24393,#24394,#24395,#24396,
#24397,#24398,#24399,#24400,#24401,#24402,#24403,#24404,#24405,#24406,#24407,
#24408,#24409,#24410,#24411,#24412,#24413,#24414,#24415,#24416,#24417,#24418,
#24419,#24420,#24421,#24422,#24423,#24424,#24425,#24426,#24427,#24428,#24429,
#24430,#24431),(#24432,#24433,#24434,#24435,#24436,#24437,#24438,#24439,
#24440,#24441,#24442,#24443,#24444,#24445,#24446,#24447,#24448,#24449,#24450,
#24451,#24452,#24453,#24454,#24455,#24456,#24457,#24458,#24459,#24460,#24461,
#24462,#24463,#24464,#24465,#24466,#24467,#24468,#24469,#24470,#24471,#24472,
#24473,#24474,#24475,#24476,#24477,#24478,#24479,#24480,#24481,#24482,#24483,
#24484,#24485,#24486,#24487,#24488,#24489,#24490,#24491,#24492,#24493),
(#24494,#24495,#24496,#24497,#24498,#24499,#24500,#24501,#24502,#24503,
#24504,#24505,#24506,#24507,#24508,#24509,#24510,#24511,#24512,#24513,#24514,
#24515,#24516,#24517,#24518,#24519,#24520,#24521,#24522,#24523,#24524,#24525,
#24526,#24527,#24528,#24529,#24530,#24531,#24532,#24533,#24534,#24535,#24536,
#24537,#24538,#24539,#24540,#24541,#24542,#24543,#24544,#24545,#24546,#24547,
#24548,#24549,#24550,#24551,#24552,#24553,#24554,#24555),(#24556,#24557,
#24558,#24559,#24560,#24561,#24562,#24563,#24564,#24565,#24566,#24567,#24568,
#24569,#24570,#24571,#24572,#24573,#24574,#24575,#24576,#24577,#24578,#24579,
#24580,#24581,#24582,#24583,#24584,#24585,#24586,#24587,#24588,#24589,#24590,
#24591,#24592,#24593,#24594,#24595,#24596,#24597,#24598,#24599,#24600,#24601,
#24602,#24603,#24604,#24605,#24606,#24607,#24608,#24609,#24610,#24611,#24612,
#24613,#24614,#24615,#24616,#24617)),.UNSPECIFIED.,.F.,.F.,.F.,(4,4),(4,
1,1,1,1,1,1,1,1,1,1,1,1,1,1,1,1,1,1,1,1,1,1,1,1,1,1,1,1,1,1,1,1,1,1,1,1,
1,1,1,1,1,1,1,1,1,1,1,1,1,1,1,1,1,1,1,1,1,1,4),(0.,0.0642013499338865),
(14.3984001269718,15.3910376296438,16.3836751323157,17.3763126349877,18.3689501376596,
19.3615876403316,20.3542251430035,21.3468626456754,22.3395001483474,23.3321376510193,
24.3247751536913,25.3174126563632,26.3100501590352,27.3026876617071,28.2953251643791,
29.287962667051,30.2806001697229,31.2732376723949,32.2658751750668,33.2585126777388,
34.2511501804107,35.2437876830827,36.2364251857546,37.2290626884266,38.2217001910985,
39.2143376937704,40.2069751964424,41.1996126991143,42.1922502017863,43.1848877044582,
44.1775252071302,45.1701627098021,46.1628002124741,47.155437715146,48.1480752178179,
49.1407127204899,50.1333502231618,51.1259877258338,52.1186252285057,53.1112627311777,
54.1039002338496,55.0965377365216,56.0891752391935,57.0818127418655,58.0744502445374,
59.0670877472093,60.0597252498813,61.0523627525532,62.0450002552252,63.0376377578971,
64.0302752605691,65.022912763241,66.015550265913,67.0081877685849,68.0008252712568,
68.9934627739288,69.9861002766007,70.9787377792727,71.9713752819446,72.9640127846166),
 .UNSPECIFIED.);
#260=B_SPLINE_SURFACE_WITH_KNOTS('',3,3,((#24943,#24944,#24945,#24946,#24947,
#24948,#24949,#24950,#24951,#24952,#24953,#24954,#24955,#24956,#24957,#24958,
#24959,#24960,#24961,#24962,#24963,#24964,#24965,#24966,#24967,#24968,#24969,
#24970,#24971,#24972,#24973,#24974,#24975,#24976,#24977,#24978,#24979,#24980,
#24981,#24982,#24983,#24984,#24985,#24986,#24987,#24988,#24989,#24990,#24991,
#24992,#24993,#24994,#24995,#24996,#24997,#24998,#24999,#25000,#25001,#25002,
#25003,#25004),(#25005,#25006,#25007,#25008,#25009,#25010,#25011,#25012,
#25013,#25014,#25015,#25016,#25017,#25018,#25019,#25020,#25021,#25022,#25023,
#25024,#25025,#25026,#25027,#25028,#25029,#25030,#25031,#25032,#25033,#25034,
#25035,#25036,#25037,#25038,#25039,#25040,#25041,#25042,#25043,#25044,#25045,
#25046,#25047,#25048,#25049,#25050,#25051,#25052,#25053,#25054,#25055,#25056,
#25057,#25058,#25059,#25060,#25061,#25062,#25063,#25064,#25065,#25066),
(#25067,#25068,#25069,#25070,#25071,#25072,#25073,#25074,#25075,#25076,
#25077,#25078,#25079,#25080,#25081,#25082,#25083,#25084,#25085,#25086,#25087,
#25088,#25089,#25090,#25091,#25092,#25093,#25094,#25095,#25096,#25097,#25098,
#25099,#25100,#25101,#25102,#25103,#25104,#25105,#25106,#25107,#25108,#25109,
#25110,#25111,#25112,#25113,#25114,#25115,#25116,#25117,#25118,#25119,#25120,
#25121,#25122,#25123,#25124,#25125,#25126,#25127,#25128),(#25129,#25130,
#25131,#25132,#25133,#25134,#25135,#25136,#25137,#25138,#25139,#25140,#25141,
#25142,#25143,#25144,#25145,#25146,#25147,#25148,#25149,#25150,#25151,#25152,
#25153,#25154,#25155,#25156,#25157,#25158,#25159,#25160,#25161,#25162,#25163,
#25164,#25165,#25166,#25167,#25168,#25169,#25170,#25171,#25172,#25173,#25174,
#25175,#25176,#25177,#25178,#25179,#25180,#25181,#25182,#25183,#25184,#25185,
#25186,#25187,#25188,#25189,#25190)),.UNSPECIFIED.,.F.,.F.,.F.,(4,4),(4,
1,1,1,1,1,1,1,1,1,1,1,1,1,1,1,1,1,1,1,1,1,1,1,1,1,1,1,1,1,1,1,1,1,1,1,1,
1,1,1,1,1,1,1,1,1,1,1,1,1,1,1,1,1,1,1,1,1,1,4),(0.,0.0642013499338865),
(11.8589888623078,12.8516263649797,13.8442638676517,14.8369013703236,15.8295388729956,
16.8221763756675,17.8148138783395,18.8074513810114,19.8000888836834,20.7927263863553,
21.7853638890272,22.7780013916992,23.7706388943711,24.7632763970431,25.755913899715,
26.748551402387,27.7411889050589,28.7338264077309,29.7264639104028,30.7191014130747,
31.7117389157467,32.7043764184186,33.6970139210906,34.6896514237625,35.6822889264345,
36.6749264291064,37.6675639317784,38.6602014344503,39.6528389371222,40.6454764397942,
41.6381139424661,42.6307514451381,43.62338894781,44.616026450482,45.6086639531539,
46.6013014558259,47.5939389584978,48.5865764611697,49.5792139638417,50.5718514665136,
51.5644889691856,52.5571264718575,53.5497639745295,54.5424014772014,55.5350389798734,
56.5276764825453,57.5203139852172,58.5129514878892,59.5055889905611,60.4982264932331,
61.490863995905,62.483501498577,63.4761390012489,64.4687765039209,65.4614140065928,
66.4540515092647,67.4466890119367,68.4393265146086,69.4319640172806,70.4246015199525),
 .UNSPECIFIED.);
#261=B_SPLINE_SURFACE_WITH_KNOTS('',3,3,((#25307,#25308,#25309,#25310,#25311,
#25312,#25313,#25314,#25315,#25316,#25317,#25318,#25319,#25320,#25321,#25322,
#25323,#25324,#25325,#25326,#25327,#25328,#25329,#25330,#25331,#25332,#25333,
#25334,#25335,#25336,#25337,#25338,#25339,#25340,#25341,#25342,#25343,#25344,
#25345,#25346,#25347,#25348,#25349,#25350,#25351,#25352,#25353,#25354,#25355,
#25356,#25357,#25358,#25359,#25360,#25361,#25362,#25363,#25364,#25365,#25366,
#25367,#25368),(#25369,#25370,#25371,#25372,#25373,#25374,#25375,#25376,
#25377,#25378,#25379,#25380,#25381,#25382,#25383,#25384,#25385,#25386,#25387,
#25388,#25389,#25390,#25391,#25392,#25393,#25394,#25395,#25396,#25397,#25398,
#25399,#25400,#25401,#25402,#25403,#25404,#25405,#25406,#25407,#25408,#25409,
#25410,#25411,#25412,#25413,#25414,#25415,#25416,#25417,#25418,#25419,#25420,
#25421,#25422,#25423,#25424,#25425,#25426,#25427,#25428,#25429,#25430),
(#25431,#25432,#25433,#25434,#25435,#25436,#25437,#25438,#25439,#25440,
#25441,#25442,#25443,#25444,#25445,#25446,#25447,#25448,#25449,#25450,#25451,
#25452,#25453,#25454,#25455,#25456,#25457,#25458,#25459,#25460,#25461,#25462,
#25463,#25464,#25465,#25466,#25467,#25468,#25469,#25470,#25471,#25472,#25473,
#25474,#25475,#25476,#25477,#25478,#25479,#25480,#25481,#25482,#25483,#25484,
#25485,#25486,#25487,#25488,#25489,#25490,#25491,#25492),(#25493,#25494,
#25495,#25496,#25497,#25498,#25499,#25500,#25501,#25502,#25503,#25504,#25505,
#25506,#25507,#25508,#25509,#25510,#25511,#25512,#25513,#25514,#25515,#25516,
#25517,#25518,#25519,#25520,#25521,#25522,#25523,#25524,#25525,#25526,#25527,
#25528,#25529,#25530,#25531,#25532,#25533,#25534,#25535,#25536,#25537,#25538,
#25539,#25540,#25541,#25542,#25543,#25544,#25545,#25546,#25547,#25548,#25549,
#25550,#25551,#25552,#25553,#25554)),.UNSPECIFIED.,.F.,.F.,.F.,(4,4),(4,
1,1,1,1,1,1,1,1,1,1,1,1,1,1,1,1,1,1,1,1,1,1,1,1,1,1,1,1,1,1,1,1,1,1,1,1,
1,1,1,1,1,1,1,1,1,1,1,1,1,1,1,1,1,1,1,1,1,1,4),(0.,0.0642013499338865),
(14.3984001269718,15.3910376296438,16.3836751323157,17.3763126349877,18.3689501376596,
19.3615876403316,20.3542251430035,21.3468626456754,22.3395001483474,23.3321376510193,
24.3247751536913,25.3174126563632,26.3100501590352,27.3026876617071,28.2953251643791,
29.287962667051,30.280600169723,31.2732376723949,32.2658751750668,33.2585126777388,
34.2511501804107,35.2437876830827,36.2364251857546,37.2290626884266,38.2217001910985,
39.2143376937705,40.2069751964424,41.1996126991143,42.1922502017863,43.1848877044582,
44.1775252071302,45.1701627098021,46.1628002124741,47.155437715146,48.148075217818,
49.1407127204899,50.1333502231619,51.1259877258338,52.1186252285057,53.1112627311777,
54.1039002338496,55.0965377365216,56.0891752391935,57.0818127418655,58.0744502445374,
59.0670877472094,60.0597252498813,61.0523627525533,62.0450002552252,63.0376377578971,
64.0302752605691,65.022912763241,66.015550265913,67.0081877685849,68.0008252712569,
68.9934627739288,69.9861002766008,70.9787377792727,71.9713752819446,72.9640127846166),
 .UNSPECIFIED.);
#262=B_SPLINE_SURFACE_WITH_KNOTS('',3,3,((#25880,#25881,#25882,#25883,#25884,
#25885,#25886,#25887,#25888,#25889,#25890,#25891,#25892,#25893,#25894,#25895,
#25896,#25897,#25898,#25899,#25900,#25901,#25902,#25903,#25904,#25905,#25906,
#25907,#25908,#25909,#25910,#25911,#25912,#25913,#25914,#25915,#25916,#25917,
#25918,#25919,#25920,#25921,#25922,#25923,#25924,#25925,#25926,#25927,#25928,
#25929,#25930,#25931,#25932,#25933,#25934,#25935,#25936,#25937,#25938,#25939,
#25940,#25941),(#25942,#25943,#25944,#25945,#25946,#25947,#25948,#25949,
#25950,#25951,#25952,#25953,#25954,#25955,#25956,#25957,#25958,#25959,#25960,
#25961,#25962,#25963,#25964,#25965,#25966,#25967,#25968,#25969,#25970,#25971,
#25972,#25973,#25974,#25975,#25976,#25977,#25978,#25979,#25980,#25981,#25982,
#25983,#25984,#25985,#25986,#25987,#25988,#25989,#25990,#25991,#25992,#25993,
#25994,#25995,#25996,#25997,#25998,#25999,#26000,#26001,#26002,#26003),
(#26004,#26005,#26006,#26007,#26008,#26009,#26010,#26011,#26012,#26013,
#26014,#26015,#26016,#26017,#26018,#26019,#26020,#26021,#26022,#26023,#26024,
#26025,#26026,#26027,#26028,#26029,#26030,#26031,#26032,#26033,#26034,#26035,
#26036,#26037,#26038,#26039,#26040,#26041,#26042,#26043,#26044,#26045,#26046,
#26047,#26048,#26049,#26050,#26051,#26052,#26053,#26054,#26055,#26056,#26057,
#26058,#26059,#26060,#26061,#26062,#26063,#26064,#26065),(#26066,#26067,
#26068,#26069,#26070,#26071,#26072,#26073,#26074,#26075,#26076,#26077,#26078,
#26079,#26080,#26081,#26082,#26083,#26084,#26085,#26086,#26087,#26088,#26089,
#26090,#26091,#26092,#26093,#26094,#26095,#26096,#26097,#26098,#26099,#26100,
#26101,#26102,#26103,#26104,#26105,#26106,#26107,#26108,#26109,#26110,#26111,
#26112,#26113,#26114,#26115,#26116,#26117,#26118,#26119,#26120,#26121,#26122,
#26123,#26124,#26125,#26126,#26127)),.UNSPECIFIED.,.F.,.F.,.F.,(4,4),(4,
1,1,1,1,1,1,1,1,1,1,1,1,1,1,1,1,1,1,1,1,1,1,1,1,1,1,1,1,1,1,1,1,1,1,1,1,
1,1,1,1,1,1,1,1,1,1,1,1,1,1,1,1,1,1,1,1,1,1,4),(0.,0.0642013499338865),
(11.8589888623078,12.8516263649797,13.8442638676517,14.8369013703236,15.8295388729956,
16.8221763756675,17.8148138783395,18.8074513810114,19.8000888836834,20.7927263863553,
21.7853638890272,22.7780013916992,23.7706388943711,24.7632763970431,25.755913899715,
26.748551402387,27.7411889050589,28.7338264077309,29.7264639104028,30.7191014130747,
31.7117389157467,32.7043764184186,33.6970139210906,34.6896514237625,35.6822889264345,
36.6749264291064,37.6675639317784,38.6602014344503,39.6528389371222,40.6454764397942,
41.6381139424661,42.6307514451381,43.62338894781,44.616026450482,45.6086639531539,
46.6013014558259,47.5939389584978,48.5865764611697,49.5792139638417,50.5718514665136,
51.5644889691856,52.5571264718575,53.5497639745295,54.5424014772014,55.5350389798734,
56.5276764825453,57.5203139852172,58.5129514878892,59.5055889905611,60.4982264932331,
61.490863995905,62.483501498577,63.4761390012489,64.4687765039209,65.4614140065928,
66.4540515092647,67.4466890119367,68.4393265146086,69.4319640172806,70.4246015199525),
 .UNSPECIFIED.);
#263=B_SPLINE_SURFACE_WITH_KNOTS('',3,3,((#26244,#26245,#26246,#26247,#26248,
#26249,#26250,#26251,#26252,#26253,#26254,#26255,#26256,#26257,#26258,#26259,
#26260,#26261,#26262,#26263,#26264,#26265,#26266,#26267,#26268,#26269,#26270,
#26271,#26272,#26273,#26274,#26275,#26276,#26277,#26278,#26279,#26280,#26281,
#26282,#26283,#26284,#26285,#26286,#26287,#26288,#26289,#26290,#26291,#26292,
#26293,#26294,#26295,#26296,#26297,#26298,#26299,#26300,#26301,#26302,#26303,
#26304,#26305),(#26306,#26307,#26308,#26309,#26310,#26311,#26312,#26313,
#26314,#26315,#26316,#26317,#26318,#26319,#26320,#26321,#26322,#26323,#26324,
#26325,#26326,#26327,#26328,#26329,#26330,#26331,#26332,#26333,#26334,#26335,
#26336,#26337,#26338,#26339,#26340,#26341,#26342,#26343,#26344,#26345,#26346,
#26347,#26348,#26349,#26350,#26351,#26352,#26353,#26354,#26355,#26356,#26357,
#26358,#26359,#26360,#26361,#26362,#26363,#26364,#26365,#26366,#26367),
(#26368,#26369,#26370,#26371,#26372,#26373,#26374,#26375,#26376,#26377,
#26378,#26379,#26380,#26381,#26382,#26383,#26384,#26385,#26386,#26387,#26388,
#26389,#26390,#26391,#26392,#26393,#26394,#26395,#26396,#26397,#26398,#26399,
#26400,#26401,#26402,#26403,#26404,#26405,#26406,#26407,#26408,#26409,#26410,
#26411,#26412,#26413,#26414,#26415,#26416,#26417,#26418,#26419,#26420,#26421,
#26422,#26423,#26424,#26425,#26426,#26427,#26428,#26429),(#26430,#26431,
#26432,#26433,#26434,#26435,#26436,#26437,#26438,#26439,#26440,#26441,#26442,
#26443,#26444,#26445,#26446,#26447,#26448,#26449,#26450,#26451,#26452,#26453,
#26454,#26455,#26456,#26457,#26458,#26459,#26460,#26461,#26462,#26463,#26464,
#26465,#26466,#26467,#26468,#26469,#26470,#26471,#26472,#26473,#26474,#26475,
#26476,#26477,#26478,#26479,#26480,#26481,#26482,#26483,#26484,#26485,#26486,
#26487,#26488,#26489,#26490,#26491)),.UNSPECIFIED.,.F.,.F.,.F.,(4,4),(4,
1,1,1,1,1,1,1,1,1,1,1,1,1,1,1,1,1,1,1,1,1,1,1,1,1,1,1,1,1,1,1,1,1,1,1,1,
1,1,1,1,1,1,1,1,1,1,1,1,1,1,1,1,1,1,1,1,1,1,4),(0.,0.0642013499338865),
(14.3984001269718,15.3910376296438,16.3836751323157,17.3763126349877,18.3689501376596,
19.3615876403316,20.3542251430035,21.3468626456755,22.3395001483474,23.3321376510193,
24.3247751536913,25.3174126563632,26.3100501590352,27.3026876617071,28.2953251643791,
29.287962667051,30.280600169723,31.2732376723949,32.2658751750668,33.2585126777388,
34.2511501804107,35.2437876830827,36.2364251857546,37.2290626884266,38.2217001910985,
39.2143376937705,40.2069751964424,41.1996126991143,42.1922502017863,43.1848877044582,
44.1775252071302,45.1701627098021,46.1628002124741,47.155437715146,48.148075217818,
49.1407127204899,50.1333502231619,51.1259877258338,52.1186252285057,53.1112627311777,
54.1039002338496,55.0965377365216,56.0891752391935,57.0818127418655,58.0744502445374,
59.0670877472094,60.0597252498813,61.0523627525533,62.0450002552252,63.0376377578971,
64.0302752605691,65.022912763241,66.015550265913,67.0081877685849,68.0008252712569,
68.9934627739288,69.9861002766008,70.9787377792727,71.9713752819446,72.9640127846166),
 .UNSPECIFIED.);
#264=B_SPLINE_SURFACE_WITH_KNOTS('',3,3,((#26817,#26818,#26819,#26820,#26821,
#26822,#26823,#26824,#26825,#26826,#26827,#26828,#26829,#26830,#26831,#26832,
#26833,#26834,#26835,#26836,#26837,#26838,#26839,#26840,#26841,#26842,#26843,
#26844,#26845,#26846,#26847,#26848,#26849,#26850,#26851,#26852,#26853,#26854,
#26855,#26856,#26857,#26858,#26859,#26860,#26861,#26862,#26863,#26864,#26865,
#26866,#26867,#26868,#26869,#26870,#26871,#26872,#26873,#26874,#26875,#26876,
#26877,#26878),(#26879,#26880,#26881,#26882,#26883,#26884,#26885,#26886,
#26887,#26888,#26889,#26890,#26891,#26892,#26893,#26894,#26895,#26896,#26897,
#26898,#26899,#26900,#26901,#26902,#26903,#26904,#26905,#26906,#26907,#26908,
#26909,#26910,#26911,#26912,#26913,#26914,#26915,#26916,#26917,#26918,#26919,
#26920,#26921,#26922,#26923,#26924,#26925,#26926,#26927,#26928,#26929,#26930,
#26931,#26932,#26933,#26934,#26935,#26936,#26937,#26938,#26939,#26940),
(#26941,#26942,#26943,#26944,#26945,#26946,#26947,#26948,#26949,#26950,
#26951,#26952,#26953,#26954,#26955,#26956,#26957,#26958,#26959,#26960,#26961,
#26962,#26963,#26964,#26965,#26966,#26967,#26968,#26969,#26970,#26971,#26972,
#26973,#26974,#26975,#26976,#26977,#26978,#26979,#26980,#26981,#26982,#26983,
#26984,#26985,#26986,#26987,#26988,#26989,#26990,#26991,#26992,#26993,#26994,
#26995,#26996,#26997,#26998,#26999,#27000,#27001,#27002),(#27003,#27004,
#27005,#27006,#27007,#27008,#27009,#27010,#27011,#27012,#27013,#27014,#27015,
#27016,#27017,#27018,#27019,#27020,#27021,#27022,#27023,#27024,#27025,#27026,
#27027,#27028,#27029,#27030,#27031,#27032,#27033,#27034,#27035,#27036,#27037,
#27038,#27039,#27040,#27041,#27042,#27043,#27044,#27045,#27046,#27047,#27048,
#27049,#27050,#27051,#27052,#27053,#27054,#27055,#27056,#27057,#27058,#27059,
#27060,#27061,#27062,#27063,#27064)),.UNSPECIFIED.,.F.,.F.,.F.,(4,4),(4,
1,1,1,1,1,1,1,1,1,1,1,1,1,1,1,1,1,1,1,1,1,1,1,1,1,1,1,1,1,1,1,1,1,1,1,1,
1,1,1,1,1,1,1,1,1,1,1,1,1,1,1,1,1,1,1,1,1,1,4),(0.,0.0642013499338865),
(11.8589888623078,12.8516263649797,13.8442638676517,14.8369013703236,15.8295388729956,
16.8221763756675,17.8148138783395,18.8074513810114,19.8000888836834,20.7927263863553,
21.7853638890272,22.7780013916992,23.7706388943711,24.7632763970431,25.755913899715,
26.748551402387,27.7411889050589,28.7338264077309,29.7264639104028,30.7191014130747,
31.7117389157467,32.7043764184186,33.6970139210906,34.6896514237625,35.6822889264345,
36.6749264291064,37.6675639317784,38.6602014344503,39.6528389371222,40.6454764397942,
41.6381139424661,42.6307514451381,43.62338894781,44.616026450482,45.6086639531539,
46.6013014558259,47.5939389584978,48.5865764611697,49.5792139638417,50.5718514665136,
51.5644889691856,52.5571264718575,53.5497639745295,54.5424014772014,55.5350389798734,
56.5276764825453,57.5203139852172,58.5129514878892,59.5055889905611,60.4982264932331,
61.490863995905,62.483501498577,63.4761390012489,64.4687765039209,65.4614140065928,
66.4540515092647,67.4466890119367,68.4393265146086,69.4319640172806,70.4246015199525),
 .UNSPECIFIED.);
#265=B_SPLINE_SURFACE_WITH_KNOTS('',3,3,((#27181,#27182,#27183,#27184,#27185,
#27186,#27187,#27188,#27189,#27190,#27191,#27192,#27193,#27194,#27195,#27196,
#27197,#27198,#27199,#27200,#27201,#27202,#27203,#27204,#27205,#27206,#27207,
#27208,#27209,#27210,#27211,#27212,#27213,#27214,#27215,#27216,#27217,#27218,
#27219,#27220,#27221,#27222,#27223,#27224,#27225,#27226,#27227,#27228,#27229,
#27230,#27231,#27232,#27233,#27234,#27235,#27236,#27237,#27238,#27239,#27240,
#27241,#27242),(#27243,#27244,#27245,#27246,#27247,#27248,#27249,#27250,
#27251,#27252,#27253,#27254,#27255,#27256,#27257,#27258,#27259,#27260,#27261,
#27262,#27263,#27264,#27265,#27266,#27267,#27268,#27269,#27270,#27271,#27272,
#27273,#27274,#27275,#27276,#27277,#27278,#27279,#27280,#27281,#27282,#27283,
#27284,#27285,#27286,#27287,#27288,#27289,#27290,#27291,#27292,#27293,#27294,
#27295,#27296,#27297,#27298,#27299,#27300,#27301,#27302,#27303,#27304),
(#27305,#27306,#27307,#27308,#27309,#27310,#27311,#27312,#27313,#27314,
#27315,#27316,#27317,#27318,#27319,#27320,#27321,#27322,#27323,#27324,#27325,
#27326,#27327,#27328,#27329,#27330,#27331,#27332,#27333,#27334,#27335,#27336,
#27337,#27338,#27339,#27340,#27341,#27342,#27343,#27344,#27345,#27346,#27347,
#27348,#27349,#27350,#27351,#27352,#27353,#27354,#27355,#27356,#27357,#27358,
#27359,#27360,#27361,#27362,#27363,#27364,#27365,#27366),(#27367,#27368,
#27369,#27370,#27371,#27372,#27373,#27374,#27375,#27376,#27377,#27378,#27379,
#27380,#27381,#27382,#27383,#27384,#27385,#27386,#27387,#27388,#27389,#27390,
#27391,#27392,#27393,#27394,#27395,#27396,#27397,#27398,#27399,#27400,#27401,
#27402,#27403,#27404,#27405,#27406,#27407,#27408,#27409,#27410,#27411,#27412,
#27413,#27414,#27415,#27416,#27417,#27418,#27419,#27420,#27421,#27422,#27423,
#27424,#27425,#27426,#27427,#27428)),.UNSPECIFIED.,.F.,.F.,.F.,(4,4),(4,
1,1,1,1,1,1,1,1,1,1,1,1,1,1,1,1,1,1,1,1,1,1,1,1,1,1,1,1,1,1,1,1,1,1,1,1,
1,1,1,1,1,1,1,1,1,1,1,1,1,1,1,1,1,1,1,1,1,1,4),(0.,0.0642013499338865),
(14.3984001269718,15.3910376296438,16.3836751323157,17.3763126349877,18.3689501376596,
19.3615876403316,20.3542251430035,21.3468626456754,22.3395001483474,23.3321376510193,
24.3247751536913,25.3174126563632,26.3100501590352,27.3026876617071,28.2953251643791,
29.287962667051,30.2806001697229,31.2732376723949,32.2658751750668,33.2585126777388,
34.2511501804107,35.2437876830827,36.2364251857546,37.2290626884266,38.2217001910985,
39.2143376937704,40.2069751964424,41.1996126991143,42.1922502017863,43.1848877044582,
44.1775252071302,45.1701627098021,46.1628002124741,47.155437715146,48.1480752178179,
49.1407127204899,50.1333502231618,51.1259877258338,52.1186252285057,53.1112627311777,
54.1039002338496,55.0965377365216,56.0891752391935,57.0818127418654,58.0744502445374,
59.0670877472093,60.0597252498813,61.0523627525532,62.0450002552252,63.0376377578971,
64.0302752605691,65.022912763241,66.0155502659129,67.0081877685849,68.0008252712568,
68.9934627739288,69.9861002766007,70.9787377792727,71.9713752819446,72.9640127846166),
 .UNSPECIFIED.);
#266=B_SPLINE_SURFACE_WITH_KNOTS('',3,3,((#27754,#27755,#27756,#27757,#27758,
#27759,#27760,#27761,#27762,#27763,#27764,#27765,#27766,#27767,#27768,#27769,
#27770,#27771,#27772,#27773,#27774,#27775,#27776,#27777,#27778,#27779,#27780,
#27781,#27782,#27783,#27784,#27785,#27786,#27787,#27788,#27789,#27790,#27791,
#27792,#27793,#27794,#27795,#27796,#27797,#27798,#27799,#27800,#27801,#27802,
#27803,#27804,#27805,#27806,#27807,#27808,#27809,#27810,#27811,#27812,#27813,
#27814,#27815),(#27816,#27817,#27818,#27819,#27820,#27821,#27822,#27823,
#27824,#27825,#27826,#27827,#27828,#27829,#27830,#27831,#27832,#27833,#27834,
#27835,#27836,#27837,#27838,#27839,#27840,#27841,#27842,#27843,#27844,#27845,
#27846,#27847,#27848,#27849,#27850,#27851,#27852,#27853,#27854,#27855,#27856,
#27857,#27858,#27859,#27860,#27861,#27862,#27863,#27864,#27865,#27866,#27867,
#27868,#27869,#27870,#27871,#27872,#27873,#27874,#27875,#27876,#27877),
(#27878,#27879,#27880,#27881,#27882,#27883,#27884,#27885,#27886,#27887,
#27888,#27889,#27890,#27891,#27892,#27893,#27894,#27895,#27896,#27897,#27898,
#27899,#27900,#27901,#27902,#27903,#27904,#27905,#27906,#27907,#27908,#27909,
#27910,#27911,#27912,#27913,#27914,#27915,#27916,#27917,#27918,#27919,#27920,
#27921,#27922,#27923,#27924,#27925,#27926,#27927,#27928,#27929,#27930,#27931,
#27932,#27933,#27934,#27935,#27936,#27937,#27938,#27939),(#27940,#27941,
#27942,#27943,#27944,#27945,#27946,#27947,#27948,#27949,#27950,#27951,#27952,
#27953,#27954,#27955,#27956,#27957,#27958,#27959,#27960,#27961,#27962,#27963,
#27964,#27965,#27966,#27967,#27968,#27969,#27970,#27971,#27972,#27973,#27974,
#27975,#27976,#27977,#27978,#27979,#27980,#27981,#27982,#27983,#27984,#27985,
#27986,#27987,#27988,#27989,#27990,#27991,#27992,#27993,#27994,#27995,#27996,
#27997,#27998,#27999,#28000,#28001)),.UNSPECIFIED.,.F.,.F.,.F.,(4,4),(4,
1,1,1,1,1,1,1,1,1,1,1,1,1,1,1,1,1,1,1,1,1,1,1,1,1,1,1,1,1,1,1,1,1,1,1,1,
1,1,1,1,1,1,1,1,1,1,1,1,1,1,1,1,1,1,1,1,1,1,4),(0.,0.0642013499338865),
(11.8589888623078,12.8516263649797,13.8442638676517,14.8369013703236,15.8295388729956,
16.8221763756675,17.8148138783395,18.8074513810114,19.8000888836834,20.7927263863553,
21.7853638890272,22.7780013916992,23.7706388943711,24.7632763970431,25.755913899715,
26.748551402387,27.7411889050589,28.7338264077309,29.7264639104028,30.7191014130747,
31.7117389157467,32.7043764184186,33.6970139210906,34.6896514237625,35.6822889264345,
36.6749264291064,37.6675639317784,38.6602014344503,39.6528389371222,40.6454764397942,
41.6381139424661,42.6307514451381,43.62338894781,44.616026450482,45.6086639531539,
46.6013014558259,47.5939389584978,48.5865764611697,49.5792139638417,50.5718514665136,
51.5644889691856,52.5571264718575,53.5497639745295,54.5424014772014,55.5350389798734,
56.5276764825453,57.5203139852172,58.5129514878892,59.5055889905611,60.4982264932331,
61.490863995905,62.483501498577,63.4761390012489,64.4687765039209,65.4614140065928,
66.4540515092647,67.4466890119367,68.4393265146086,69.4319640172806,70.4246015199525),
 .UNSPECIFIED.);
#267=B_SPLINE_SURFACE_WITH_KNOTS('',3,3,((#28118,#28119,#28120,#28121,#28122,
#28123,#28124,#28125,#28126,#28127,#28128,#28129,#28130,#28131,#28132,#28133,
#28134,#28135,#28136,#28137,#28138,#28139,#28140,#28141,#28142,#28143,#28144,
#28145,#28146,#28147,#28148,#28149,#28150,#28151,#28152,#28153,#28154,#28155,
#28156,#28157,#28158,#28159,#28160,#28161,#28162,#28163,#28164,#28165,#28166,
#28167,#28168,#28169,#28170,#28171,#28172,#28173,#28174,#28175,#28176,#28177,
#28178,#28179),(#28180,#28181,#28182,#28183,#28184,#28185,#28186,#28187,
#28188,#28189,#28190,#28191,#28192,#28193,#28194,#28195,#28196,#28197,#28198,
#28199,#28200,#28201,#28202,#28203,#28204,#28205,#28206,#28207,#28208,#28209,
#28210,#28211,#28212,#28213,#28214,#28215,#28216,#28217,#28218,#28219,#28220,
#28221,#28222,#28223,#28224,#28225,#28226,#28227,#28228,#28229,#28230,#28231,
#28232,#28233,#28234,#28235,#28236,#28237,#28238,#28239,#28240,#28241),
(#28242,#28243,#28244,#28245,#28246,#28247,#28248,#28249,#28250,#28251,
#28252,#28253,#28254,#28255,#28256,#28257,#28258,#28259,#28260,#28261,#28262,
#28263,#28264,#28265,#28266,#28267,#28268,#28269,#28270,#28271,#28272,#28273,
#28274,#28275,#28276,#28277,#28278,#28279,#28280,#28281,#28282,#28283,#28284,
#28285,#28286,#28287,#28288,#28289,#28290,#28291,#28292,#28293,#28294,#28295,
#28296,#28297,#28298,#28299,#28300,#28301,#28302,#28303),(#28304,#28305,
#28306,#28307,#28308,#28309,#28310,#28311,#28312,#28313,#28314,#28315,#28316,
#28317,#28318,#28319,#28320,#28321,#28322,#28323,#28324,#28325,#28326,#28327,
#28328,#28329,#28330,#28331,#28332,#28333,#28334,#28335,#28336,#28337,#28338,
#28339,#28340,#28341,#28342,#28343,#28344,#28345,#28346,#28347,#28348,#28349,
#28350,#28351,#28352,#28353,#28354,#28355,#28356,#28357,#28358,#28359,#28360,
#28361,#28362,#28363,#28364,#28365)),.UNSPECIFIED.,.F.,.F.,.F.,(4,4),(4,
1,1,1,1,1,1,1,1,1,1,1,1,1,1,1,1,1,1,1,1,1,1,1,1,1,1,1,1,1,1,1,1,1,1,1,1,
1,1,1,1,1,1,1,1,1,1,1,1,1,1,1,1,1,1,1,1,1,1,4),(0.,0.0642013499338865),
(14.3984001269718,15.3910376296438,16.3836751323157,17.3763126349877,18.3689501376596,
19.3615876403316,20.3542251430035,21.3468626456754,22.3395001483474,23.3321376510193,
24.3247751536913,25.3174126563632,26.3100501590352,27.3026876617071,28.2953251643791,
29.287962667051,30.280600169723,31.2732376723949,32.2658751750668,33.2585126777388,
34.2511501804107,35.2437876830827,36.2364251857546,37.2290626884266,38.2217001910985,
39.2143376937705,40.2069751964424,41.1996126991143,42.1922502017863,43.1848877044582,
44.1775252071302,45.1701627098021,46.1628002124741,47.155437715146,48.148075217818,
49.1407127204899,50.1333502231619,51.1259877258338,52.1186252285057,53.1112627311777,
54.1039002338496,55.0965377365216,56.0891752391935,57.0818127418655,58.0744502445374,
59.0670877472094,60.0597252498813,61.0523627525533,62.0450002552252,63.0376377578971,
64.0302752605691,65.022912763241,66.015550265913,67.0081877685849,68.0008252712569,
68.9934627739288,69.9861002766008,70.9787377792727,71.9713752819446,72.9640127846166),
 .UNSPECIFIED.);
#268=B_SPLINE_SURFACE_WITH_KNOTS('',3,3,((#28691,#28692,#28693,#28694,#28695,
#28696,#28697,#28698,#28699,#28700,#28701,#28702,#28703,#28704,#28705,#28706,
#28707,#28708,#28709,#28710,#28711,#28712,#28713,#28714,#28715,#28716,#28717,
#28718,#28719,#28720,#28721,#28722,#28723,#28724,#28725,#28726,#28727,#28728,
#28729,#28730,#28731,#28732,#28733,#28734,#28735,#28736,#28737,#28738,#28739,
#28740,#28741,#28742,#28743,#28744,#28745,#28746,#28747,#28748,#28749,#28750,
#28751,#28752),(#28753,#28754,#28755,#28756,#28757,#28758,#28759,#28760,
#28761,#28762,#28763,#28764,#28765,#28766,#28767,#28768,#28769,#28770,#28771,
#28772,#28773,#28774,#28775,#28776,#28777,#28778,#28779,#28780,#28781,#28782,
#28783,#28784,#28785,#28786,#28787,#28788,#28789,#28790,#28791,#28792,#28793,
#28794,#28795,#28796,#28797,#28798,#28799,#28800,#28801,#28802,#28803,#28804,
#28805,#28806,#28807,#28808,#28809,#28810,#28811,#28812,#28813,#28814),
(#28815,#28816,#28817,#28818,#28819,#28820,#28821,#28822,#28823,#28824,
#28825,#28826,#28827,#28828,#28829,#28830,#28831,#28832,#28833,#28834,#28835,
#28836,#28837,#28838,#28839,#28840,#28841,#28842,#28843,#28844,#28845,#28846,
#28847,#28848,#28849,#28850,#28851,#28852,#28853,#28854,#28855,#28856,#28857,
#28858,#28859,#28860,#28861,#28862,#28863,#28864,#28865,#28866,#28867,#28868,
#28869,#28870,#28871,#28872,#28873,#28874,#28875,#28876),(#28877,#28878,
#28879,#28880,#28881,#28882,#28883,#28884,#28885,#28886,#28887,#28888,#28889,
#28890,#28891,#28892,#28893,#28894,#28895,#28896,#28897,#28898,#28899,#28900,
#28901,#28902,#28903,#28904,#28905,#28906,#28907,#28908,#28909,#28910,#28911,
#28912,#28913,#28914,#28915,#28916,#28917,#28918,#28919,#28920,#28921,#28922,
#28923,#28924,#28925,#28926,#28927,#28928,#28929,#28930,#28931,#28932,#28933,
#28934,#28935,#28936,#28937,#28938)),.UNSPECIFIED.,.F.,.F.,.F.,(4,4),(4,
1,1,1,1,1,1,1,1,1,1,1,1,1,1,1,1,1,1,1,1,1,1,1,1,1,1,1,1,1,1,1,1,1,1,1,1,
1,1,1,1,1,1,1,1,1,1,1,1,1,1,1,1,1,1,1,1,1,1,4),(0.,0.0642013499338865),
(11.8589888623078,12.8516263649797,13.8442638676517,14.8369013703236,15.8295388729956,
16.8221763756675,17.8148138783395,18.8074513810114,19.8000888836834,20.7927263863553,
21.7853638890272,22.7780013916992,23.7706388943711,24.7632763970431,25.755913899715,
26.748551402387,27.7411889050589,28.7338264077309,29.7264639104028,30.7191014130747,
31.7117389157467,32.7043764184186,33.6970139210906,34.6896514237625,35.6822889264345,
36.6749264291064,37.6675639317784,38.6602014344503,39.6528389371222,40.6454764397942,
41.6381139424661,42.6307514451381,43.62338894781,44.616026450482,45.6086639531539,
46.6013014558259,47.5939389584978,48.5865764611697,49.5792139638417,50.5718514665136,
51.5644889691856,52.5571264718575,53.5497639745295,54.5424014772014,55.5350389798734,
56.5276764825453,57.5203139852172,58.5129514878892,59.5055889905611,60.4982264932331,
61.490863995905,62.483501498577,63.4761390012489,64.4687765039209,65.4614140065928,
66.4540515092647,67.4466890119367,68.4393265146086,69.4319640172806,70.4246015199525),
 .UNSPECIFIED.);
#269=B_SPLINE_SURFACE_WITH_KNOTS('',3,3,((#29055,#29056,#29057,#29058,#29059,
#29060,#29061,#29062,#29063,#29064,#29065,#29066,#29067,#29068,#29069,#29070,
#29071,#29072,#29073,#29074,#29075,#29076,#29077,#29078,#29079,#29080,#29081,
#29082,#29083,#29084,#29085,#29086,#29087,#29088,#29089,#29090,#29091,#29092,
#29093,#29094,#29095,#29096,#29097,#29098,#29099,#29100,#29101,#29102,#29103,
#29104,#29105,#29106,#29107,#29108,#29109,#29110,#29111,#29112,#29113,#29114,
#29115,#29116),(#29117,#29118,#29119,#29120,#29121,#29122,#29123,#29124,
#29125,#29126,#29127,#29128,#29129,#29130,#29131,#29132,#29133,#29134,#29135,
#29136,#29137,#29138,#29139,#29140,#29141,#29142,#29143,#29144,#29145,#29146,
#29147,#29148,#29149,#29150,#29151,#29152,#29153,#29154,#29155,#29156,#29157,
#29158,#29159,#29160,#29161,#29162,#29163,#29164,#29165,#29166,#29167,#29168,
#29169,#29170,#29171,#29172,#29173,#29174,#29175,#29176,#29177,#29178),
(#29179,#29180,#29181,#29182,#29183,#29184,#29185,#29186,#29187,#29188,
#29189,#29190,#29191,#29192,#29193,#29194,#29195,#29196,#29197,#29198,#29199,
#29200,#29201,#29202,#29203,#29204,#29205,#29206,#29207,#29208,#29209,#29210,
#29211,#29212,#29213,#29214,#29215,#29216,#29217,#29218,#29219,#29220,#29221,
#29222,#29223,#29224,#29225,#29226,#29227,#29228,#29229,#29230,#29231,#29232,
#29233,#29234,#29235,#29236,#29237,#29238,#29239,#29240),(#29241,#29242,
#29243,#29244,#29245,#29246,#29247,#29248,#29249,#29250,#29251,#29252,#29253,
#29254,#29255,#29256,#29257,#29258,#29259,#29260,#29261,#29262,#29263,#29264,
#29265,#29266,#29267,#29268,#29269,#29270,#29271,#29272,#29273,#29274,#29275,
#29276,#29277,#29278,#29279,#29280,#29281,#29282,#29283,#29284,#29285,#29286,
#29287,#29288,#29289,#29290,#29291,#29292,#29293,#29294,#29295,#29296,#29297,
#29298,#29299,#29300,#29301,#29302)),.UNSPECIFIED.,.F.,.F.,.F.,(4,4),(4,
1,1,1,1,1,1,1,1,1,1,1,1,1,1,1,1,1,1,1,1,1,1,1,1,1,1,1,1,1,1,1,1,1,1,1,1,
1,1,1,1,1,1,1,1,1,1,1,1,1,1,1,1,1,1,1,1,1,1,4),(0.,0.0642013499338865),
(14.3984001269718,15.3910376296438,16.3836751323157,17.3763126349877,18.3689501376596,
19.3615876403316,20.3542251430035,21.3468626456754,22.3395001483474,23.3321376510193,
24.3247751536913,25.3174126563632,26.3100501590352,27.3026876617071,28.2953251643791,
29.287962667051,30.280600169723,31.2732376723949,32.2658751750668,33.2585126777388,
34.2511501804107,35.2437876830827,36.2364251857546,37.2290626884266,38.2217001910985,
39.2143376937705,40.2069751964424,41.1996126991143,42.1922502017863,43.1848877044582,
44.1775252071302,45.1701627098021,46.1628002124741,47.155437715146,48.148075217818,
49.1407127204899,50.1333502231619,51.1259877258338,52.1186252285057,53.1112627311777,
54.1039002338496,55.0965377365216,56.0891752391935,57.0818127418655,58.0744502445374,
59.0670877472094,60.0597252498813,61.0523627525533,62.0450002552252,63.0376377578971,
64.0302752605691,65.022912763241,66.015550265913,67.0081877685849,68.0008252712569,
68.9934627739288,69.9861002766008,70.9787377792727,71.9713752819446,72.9640127846166),
 .UNSPECIFIED.);
#270=B_SPLINE_SURFACE_WITH_KNOTS('',3,3,((#29628,#29629,#29630,#29631,#29632,
#29633,#29634,#29635,#29636,#29637,#29638,#29639,#29640,#29641,#29642,#29643,
#29644,#29645,#29646,#29647,#29648,#29649,#29650,#29651,#29652,#29653,#29654,
#29655,#29656,#29657,#29658,#29659,#29660,#29661,#29662,#29663,#29664,#29665,
#29666,#29667,#29668,#29669,#29670,#29671,#29672,#29673,#29674,#29675,#29676,
#29677,#29678,#29679,#29680,#29681,#29682,#29683,#29684,#29685,#29686,#29687,
#29688,#29689),(#29690,#29691,#29692,#29693,#29694,#29695,#29696,#29697,
#29698,#29699,#29700,#29701,#29702,#29703,#29704,#29705,#29706,#29707,#29708,
#29709,#29710,#29711,#29712,#29713,#29714,#29715,#29716,#29717,#29718,#29719,
#29720,#29721,#29722,#29723,#29724,#29725,#29726,#29727,#29728,#29729,#29730,
#29731,#29732,#29733,#29734,#29735,#29736,#29737,#29738,#29739,#29740,#29741,
#29742,#29743,#29744,#29745,#29746,#29747,#29748,#29749,#29750,#29751),
(#29752,#29753,#29754,#29755,#29756,#29757,#29758,#29759,#29760,#29761,
#29762,#29763,#29764,#29765,#29766,#29767,#29768,#29769,#29770,#29771,#29772,
#29773,#29774,#29775,#29776,#29777,#29778,#29779,#29780,#29781,#29782,#29783,
#29784,#29785,#29786,#29787,#29788,#29789,#29790,#29791,#29792,#29793,#29794,
#29795,#29796,#29797,#29798,#29799,#29800,#29801,#29802,#29803,#29804,#29805,
#29806,#29807,#29808,#29809,#29810,#29811,#29812,#29813),(#29814,#29815,
#29816,#29817,#29818,#29819,#29820,#29821,#29822,#29823,#29824,#29825,#29826,
#29827,#29828,#29829,#29830,#29831,#29832,#29833,#29834,#29835,#29836,#29837,
#29838,#29839,#29840,#29841,#29842,#29843,#29844,#29845,#29846,#29847,#29848,
#29849,#29850,#29851,#29852,#29853,#29854,#29855,#29856,#29857,#29858,#29859,
#29860,#29861,#29862,#29863,#29864,#29865,#29866,#29867,#29868,#29869,#29870,
#29871,#29872,#29873,#29874,#29875)),.UNSPECIFIED.,.F.,.F.,.F.,(4,4),(4,
1,1,1,1,1,1,1,1,1,1,1,1,1,1,1,1,1,1,1,1,1,1,1,1,1,1,1,1,1,1,1,1,1,1,1,1,
1,1,1,1,1,1,1,1,1,1,1,1,1,1,1,1,1,1,1,1,1,1,4),(0.,0.0642013499338865),
(11.8589888623078,12.8516263649797,13.8442638676517,14.8369013703236,15.8295388729956,
16.8221763756675,17.8148138783395,18.8074513810114,19.8000888836834,20.7927263863553,
21.7853638890272,22.7780013916992,23.7706388943711,24.7632763970431,25.755913899715,
26.748551402387,27.7411889050589,28.7338264077309,29.7264639104028,30.7191014130747,
31.7117389157467,32.7043764184186,33.6970139210906,34.6896514237625,35.6822889264345,
36.6749264291064,37.6675639317784,38.6602014344503,39.6528389371222,40.6454764397942,
41.6381139424661,42.6307514451381,43.62338894781,44.616026450482,45.6086639531539,
46.6013014558259,47.5939389584978,48.5865764611697,49.5792139638417,50.5718514665136,
51.5644889691856,52.5571264718575,53.5497639745295,54.5424014772014,55.5350389798734,
56.5276764825453,57.5203139852172,58.5129514878892,59.5055889905611,60.4982264932331,
61.490863995905,62.483501498577,63.4761390012489,64.4687765039209,65.4614140065928,
66.4540515092647,67.4466890119367,68.4393265146086,69.4319640172806,70.4246015199525),
 .UNSPECIFIED.);
#271=B_SPLINE_SURFACE_WITH_KNOTS('',3,3,((#29992,#29993,#29994,#29995,#29996,
#29997,#29998,#29999,#30000,#30001,#30002,#30003,#30004,#30005,#30006,#30007,
#30008,#30009,#30010,#30011,#30012,#30013,#30014,#30015,#30016,#30017,#30018,
#30019,#30020,#30021,#30022,#30023,#30024,#30025,#30026,#30027,#30028,#30029,
#30030,#30031,#30032,#30033,#30034,#30035,#30036,#30037,#30038,#30039,#30040,
#30041,#30042,#30043,#30044,#30045,#30046,#30047,#30048,#30049,#30050,#30051,
#30052,#30053),(#30054,#30055,#30056,#30057,#30058,#30059,#30060,#30061,
#30062,#30063,#30064,#30065,#30066,#30067,#30068,#30069,#30070,#30071,#30072,
#30073,#30074,#30075,#30076,#30077,#30078,#30079,#30080,#30081,#30082,#30083,
#30084,#30085,#30086,#30087,#30088,#30089,#30090,#30091,#30092,#30093,#30094,
#30095,#30096,#30097,#30098,#30099,#30100,#30101,#30102,#30103,#30104,#30105,
#30106,#30107,#30108,#30109,#30110,#30111,#30112,#30113,#30114,#30115),
(#30116,#30117,#30118,#30119,#30120,#30121,#30122,#30123,#30124,#30125,
#30126,#30127,#30128,#30129,#30130,#30131,#30132,#30133,#30134,#30135,#30136,
#30137,#30138,#30139,#30140,#30141,#30142,#30143,#30144,#30145,#30146,#30147,
#30148,#30149,#30150,#30151,#30152,#30153,#30154,#30155,#30156,#30157,#30158,
#30159,#30160,#30161,#30162,#30163,#30164,#30165,#30166,#30167,#30168,#30169,
#30170,#30171,#30172,#30173,#30174,#30175,#30176,#30177),(#30178,#30179,
#30180,#30181,#30182,#30183,#30184,#30185,#30186,#30187,#30188,#30189,#30190,
#30191,#30192,#30193,#30194,#30195,#30196,#30197,#30198,#30199,#30200,#30201,
#30202,#30203,#30204,#30205,#30206,#30207,#30208,#30209,#30210,#30211,#30212,
#30213,#30214,#30215,#30216,#30217,#30218,#30219,#30220,#30221,#30222,#30223,
#30224,#30225,#30226,#30227,#30228,#30229,#30230,#30231,#30232,#30233,#30234,
#30235,#30236,#30237,#30238,#30239)),.UNSPECIFIED.,.F.,.F.,.F.,(4,4),(4,
1,1,1,1,1,1,1,1,1,1,1,1,1,1,1,1,1,1,1,1,1,1,1,1,1,1,1,1,1,1,1,1,1,1,1,1,
1,1,1,1,1,1,1,1,1,1,1,1,1,1,1,1,1,1,1,1,1,1,4),(0.,0.0642013499338865),
(14.3984001269718,15.3910376296438,16.3836751323157,17.3763126349877,18.3689501376596,
19.3615876403316,20.3542251430035,21.3468626456754,22.3395001483474,23.3321376510193,
24.3247751536913,25.3174126563632,26.3100501590352,27.3026876617071,28.2953251643791,
29.287962667051,30.2806001697229,31.2732376723949,32.2658751750668,33.2585126777388,
34.2511501804107,35.2437876830827,36.2364251857546,37.2290626884266,38.2217001910985,
39.2143376937704,40.2069751964424,41.1996126991143,42.1922502017863,43.1848877044582,
44.1775252071302,45.1701627098021,46.1628002124741,47.155437715146,48.1480752178179,
49.1407127204899,50.1333502231618,51.1259877258338,52.1186252285057,53.1112627311777,
54.1039002338496,55.0965377365216,56.0891752391935,57.0818127418654,58.0744502445374,
59.0670877472093,60.0597252498813,61.0523627525532,62.0450002552252,63.0376377578971,
64.0302752605691,65.022912763241,66.0155502659129,67.0081877685849,68.0008252712568,
68.9934627739288,69.9861002766007,70.9787377792727,71.9713752819446,72.9640127846166),
 .UNSPECIFIED.);
#272=B_SPLINE_SURFACE_WITH_KNOTS('',3,3,((#30565,#30566,#30567,#30568,#30569,
#30570,#30571,#30572,#30573,#30574,#30575,#30576,#30577,#30578,#30579,#30580,
#30581,#30582,#30583,#30584,#30585,#30586,#30587,#30588,#30589,#30590,#30591,
#30592,#30593,#30594,#30595,#30596,#30597,#30598,#30599,#30600,#30601,#30602,
#30603,#30604,#30605,#30606,#30607,#30608,#30609,#30610,#30611,#30612,#30613,
#30614,#30615,#30616,#30617,#30618,#30619,#30620,#30621,#30622,#30623,#30624,
#30625,#30626),(#30627,#30628,#30629,#30630,#30631,#30632,#30633,#30634,
#30635,#30636,#30637,#30638,#30639,#30640,#30641,#30642,#30643,#30644,#30645,
#30646,#30647,#30648,#30649,#30650,#30651,#30652,#30653,#30654,#30655,#30656,
#30657,#30658,#30659,#30660,#30661,#30662,#30663,#30664,#30665,#30666,#30667,
#30668,#30669,#30670,#30671,#30672,#30673,#30674,#30675,#30676,#30677,#30678,
#30679,#30680,#30681,#30682,#30683,#30684,#30685,#30686,#30687,#30688),
(#30689,#30690,#30691,#30692,#30693,#30694,#30695,#30696,#30697,#30698,
#30699,#30700,#30701,#30702,#30703,#30704,#30705,#30706,#30707,#30708,#30709,
#30710,#30711,#30712,#30713,#30714,#30715,#30716,#30717,#30718,#30719,#30720,
#30721,#30722,#30723,#30724,#30725,#30726,#30727,#30728,#30729,#30730,#30731,
#30732,#30733,#30734,#30735,#30736,#30737,#30738,#30739,#30740,#30741,#30742,
#30743,#30744,#30745,#30746,#30747,#30748,#30749,#30750),(#30751,#30752,
#30753,#30754,#30755,#30756,#30757,#30758,#30759,#30760,#30761,#30762,#30763,
#30764,#30765,#30766,#30767,#30768,#30769,#30770,#30771,#30772,#30773,#30774,
#30775,#30776,#30777,#30778,#30779,#30780,#30781,#30782,#30783,#30784,#30785,
#30786,#30787,#30788,#30789,#30790,#30791,#30792,#30793,#30794,#30795,#30796,
#30797,#30798,#30799,#30800,#30801,#30802,#30803,#30804,#30805,#30806,#30807,
#30808,#30809,#30810,#30811,#30812)),.UNSPECIFIED.,.F.,.F.,.F.,(4,4),(4,
1,1,1,1,1,1,1,1,1,1,1,1,1,1,1,1,1,1,1,1,1,1,1,1,1,1,1,1,1,1,1,1,1,1,1,1,
1,1,1,1,1,1,1,1,1,1,1,1,1,1,1,1,1,1,1,1,1,1,4),(0.,0.0642013499338865),
(11.8589888623078,12.8516263649797,13.8442638676517,14.8369013703236,15.8295388729956,
16.8221763756675,17.8148138783395,18.8074513810114,19.8000888836834,20.7927263863553,
21.7853638890272,22.7780013916992,23.7706388943711,24.7632763970431,25.755913899715,
26.748551402387,27.7411889050589,28.7338264077309,29.7264639104028,30.7191014130747,
31.7117389157467,32.7043764184186,33.6970139210906,34.6896514237625,35.6822889264345,
36.6749264291064,37.6675639317784,38.6602014344503,39.6528389371222,40.6454764397942,
41.6381139424661,42.6307514451381,43.62338894781,44.616026450482,45.6086639531539,
46.6013014558259,47.5939389584978,48.5865764611697,49.5792139638417,50.5718514665136,
51.5644889691856,52.5571264718575,53.5497639745295,54.5424014772014,55.5350389798734,
56.5276764825453,57.5203139852172,58.5129514878892,59.5055889905611,60.4982264932331,
61.490863995905,62.483501498577,63.4761390012489,64.4687765039209,65.4614140065928,
66.4540515092647,67.4466890119367,68.4393265146086,69.4319640172806,70.4246015199525),
 .UNSPECIFIED.);
#273=B_SPLINE_SURFACE_WITH_KNOTS('',3,3,((#30929,#30930,#30931,#30932,#30933,
#30934,#30935,#30936,#30937,#30938,#30939,#30940,#30941,#30942,#30943,#30944,
#30945,#30946,#30947,#30948,#30949,#30950,#30951,#30952,#30953,#30954,#30955,
#30956,#30957,#30958,#30959,#30960,#30961,#30962,#30963,#30964,#30965,#30966,
#30967,#30968,#30969,#30970,#30971,#30972,#30973,#30974,#30975,#30976,#30977,
#30978,#30979,#30980,#30981,#30982,#30983,#30984,#30985,#30986,#30987,#30988,
#30989,#30990),(#30991,#30992,#30993,#30994,#30995,#30996,#30997,#30998,
#30999,#31000,#31001,#31002,#31003,#31004,#31005,#31006,#31007,#31008,#31009,
#31010,#31011,#31012,#31013,#31014,#31015,#31016,#31017,#31018,#31019,#31020,
#31021,#31022,#31023,#31024,#31025,#31026,#31027,#31028,#31029,#31030,#31031,
#31032,#31033,#31034,#31035,#31036,#31037,#31038,#31039,#31040,#31041,#31042,
#31043,#31044,#31045,#31046,#31047,#31048,#31049,#31050,#31051,#31052),
(#31053,#31054,#31055,#31056,#31057,#31058,#31059,#31060,#31061,#31062,
#31063,#31064,#31065,#31066,#31067,#31068,#31069,#31070,#31071,#31072,#31073,
#31074,#31075,#31076,#31077,#31078,#31079,#31080,#31081,#31082,#31083,#31084,
#31085,#31086,#31087,#31088,#31089,#31090,#31091,#31092,#31093,#31094,#31095,
#31096,#31097,#31098,#31099,#31100,#31101,#31102,#31103,#31104,#31105,#31106,
#31107,#31108,#31109,#31110,#31111,#31112,#31113,#31114),(#31115,#31116,
#31117,#31118,#31119,#31120,#31121,#31122,#31123,#31124,#31125,#31126,#31127,
#31128,#31129,#31130,#31131,#31132,#31133,#31134,#31135,#31136,#31137,#31138,
#31139,#31140,#31141,#31142,#31143,#31144,#31145,#31146,#31147,#31148,#31149,
#31150,#31151,#31152,#31153,#31154,#31155,#31156,#31157,#31158,#31159,#31160,
#31161,#31162,#31163,#31164,#31165,#31166,#31167,#31168,#31169,#31170,#31171,
#31172,#31173,#31174,#31175,#31176)),.UNSPECIFIED.,.F.,.F.,.F.,(4,4),(4,
1,1,1,1,1,1,1,1,1,1,1,1,1,1,1,1,1,1,1,1,1,1,1,1,1,1,1,1,1,1,1,1,1,1,1,1,
1,1,1,1,1,1,1,1,1,1,1,1,1,1,1,1,1,1,1,1,1,1,4),(0.,0.0642013499338865),
(14.3984001269718,15.3910376296438,16.3836751323157,17.3763126349877,18.3689501376596,
19.3615876403316,20.3542251430035,21.3468626456754,22.3395001483474,23.3321376510193,
24.3247751536913,25.3174126563632,26.3100501590352,27.3026876617071,28.2953251643791,
29.287962667051,30.2806001697229,31.2732376723949,32.2658751750668,33.2585126777388,
34.2511501804107,35.2437876830827,36.2364251857546,37.2290626884266,38.2217001910985,
39.2143376937704,40.2069751964424,41.1996126991143,42.1922502017863,43.1848877044582,
44.1775252071302,45.1701627098021,46.1628002124741,47.155437715146,48.1480752178179,
49.1407127204899,50.1333502231618,51.1259877258338,52.1186252285057,53.1112627311777,
54.1039002338496,55.0965377365216,56.0891752391935,57.0818127418655,58.0744502445374,
59.0670877472093,60.0597252498813,61.0523627525532,62.0450002552252,63.0376377578971,
64.0302752605691,65.022912763241,66.015550265913,67.0081877685849,68.0008252712568,
68.9934627739288,69.9861002766007,70.9787377792727,71.9713752819446,72.9640127846166),
 .UNSPECIFIED.);
#274=B_SPLINE_SURFACE_WITH_KNOTS('',3,3,((#35745,#35746,#35747,#35748,#35749,
#35750,#35751,#35752,#35753,#35754,#35755,#35756,#35757,#35758,#35759,#35760,
#35761,#35762,#35763,#35764,#35765,#35766,#35767,#35768,#35769,#35770,#35771,
#35772,#35773,#35774,#35775,#35776,#35777,#35778,#35779,#35780,#35781,#35782,
#35783,#35784,#35785,#35786,#35787,#35788,#35789,#35790,#35791,#35792,#35793,
#35794,#35795,#35796,#35797,#35798,#35799,#35800,#35801,#35802,#35803,#35804,
#35805,#35806,#35807,#35808),(#35809,#35810,#35811,#35812,#35813,#35814,
#35815,#35816,#35817,#35818,#35819,#35820,#35821,#35822,#35823,#35824,#35825,
#35826,#35827,#35828,#35829,#35830,#35831,#35832,#35833,#35834,#35835,#35836,
#35837,#35838,#35839,#35840,#35841,#35842,#35843,#35844,#35845,#35846,#35847,
#35848,#35849,#35850,#35851,#35852,#35853,#35854,#35855,#35856,#35857,#35858,
#35859,#35860,#35861,#35862,#35863,#35864,#35865,#35866,#35867,#35868,#35869,
#35870,#35871,#35872),(#35873,#35874,#35875,#35876,#35877,#35878,#35879,
#35880,#35881,#35882,#35883,#35884,#35885,#35886,#35887,#35888,#35889,#35890,
#35891,#35892,#35893,#35894,#35895,#35896,#35897,#35898,#35899,#35900,#35901,
#35902,#35903,#35904,#35905,#35906,#35907,#35908,#35909,#35910,#35911,#35912,
#35913,#35914,#35915,#35916,#35917,#35918,#35919,#35920,#35921,#35922,#35923,
#35924,#35925,#35926,#35927,#35928,#35929,#35930,#35931,#35932,#35933,#35934,
#35935,#35936),(#35937,#35938,#35939,#35940,#35941,#35942,#35943,#35944,
#35945,#35946,#35947,#35948,#35949,#35950,#35951,#35952,#35953,#35954,#35955,
#35956,#35957,#35958,#35959,#35960,#35961,#35962,#35963,#35964,#35965,#35966,
#35967,#35968,#35969,#35970,#35971,#35972,#35973,#35974,#35975,#35976,#35977,
#35978,#35979,#35980,#35981,#35982,#35983,#35984,#35985,#35986,#35987,#35988,
#35989,#35990,#35991,#35992,#35993,#35994,#35995,#35996,#35997,#35998,#35999,
#36000)),.UNSPECIFIED.,.F.,.F.,.F.,(4,4),(4,1,1,1,1,1,1,1,1,1,1,1,1,1,1,
1,1,1,1,1,1,1,1,1,1,1,1,1,1,1,1,1,1,1,1,1,1,1,1,1,1,1,1,1,1,1,1,1,1,1,1,
1,1,1,1,1,1,1,1,1,1,4),(0.,0.0965329650085053),(11.8529428644271,12.3426821320026,
12.8324213995782,13.3221606671538,13.8118999347294,14.301639202305,14.7913784698806,
15.2811177374562,15.7708570050318,16.2605962726074,16.750335540183,17.2400748077586,
17.7298140753341,18.2195533429097,18.7092926104853,19.1990318780609,19.6887711456365,
20.1785104132121,20.6682496807877,21.1579889483633,21.6477282159389,22.1374674835145,
22.6272067510901,23.1169460186656,23.6066852862412,24.0964245538168,24.5861638213924,
25.075903088968,25.5656423565436,26.0553816241192,26.5451208916948,27.524599426846,
28.5040779619971,29.4835564971483,29.9732957647239,30.4630350322995,30.9527742998751,
31.4425135674507,31.9322528350263,32.4219921026019,32.9117313701775,33.4014706377531,
33.8912099053287,34.3809491729042,34.8706884404798,35.3604277080554,35.850166975631,
36.3399062432066,36.8296455107822,37.3193847783578,37.8091240459334,38.298863313509,
38.7886025810846,39.2783418486601,39.7680811162357,40.2578203838113,40.7475596513869,
41.2372989189625,41.7270381865381,42.2167774541137,42.7065167216893,43.1962559892649),
 .UNSPECIFIED.);
#275=B_SPLINE_SURFACE_WITH_KNOTS('',3,3,((#36150,#36151,#36152,#36153,#36154,
#36155,#36156,#36157,#36158,#36159,#36160,#36161,#36162,#36163,#36164,#36165,
#36166,#36167,#36168,#36169,#36170,#36171,#36172,#36173,#36174,#36175,#36176,
#36177,#36178,#36179,#36180,#36181,#36182,#36183,#36184,#36185,#36186,#36187,
#36188,#36189,#36190,#36191,#36192,#36193,#36194,#36195,#36196,#36197,#36198,
#36199,#36200,#36201,#36202,#36203,#36204,#36205,#36206,#36207,#36208,#36209,
#36210,#36211,#36212,#36213),(#36214,#36215,#36216,#36217,#36218,#36219,
#36220,#36221,#36222,#36223,#36224,#36225,#36226,#36227,#36228,#36229,#36230,
#36231,#36232,#36233,#36234,#36235,#36236,#36237,#36238,#36239,#36240,#36241,
#36242,#36243,#36244,#36245,#36246,#36247,#36248,#36249,#36250,#36251,#36252,
#36253,#36254,#36255,#36256,#36257,#36258,#36259,#36260,#36261,#36262,#36263,
#36264,#36265,#36266,#36267,#36268,#36269,#36270,#36271,#36272,#36273,#36274,
#36275,#36276,#36277),(#36278,#36279,#36280,#36281,#36282,#36283,#36284,
#36285,#36286,#36287,#36288,#36289,#36290,#36291,#36292,#36293,#36294,#36295,
#36296,#36297,#36298,#36299,#36300,#36301,#36302,#36303,#36304,#36305,#36306,
#36307,#36308,#36309,#36310,#36311,#36312,#36313,#36314,#36315,#36316,#36317,
#36318,#36319,#36320,#36321,#36322,#36323,#36324,#36325,#36326,#36327,#36328,
#36329,#36330,#36331,#36332,#36333,#36334,#36335,#36336,#36337,#36338,#36339,
#36340,#36341),(#36342,#36343,#36344,#36345,#36346,#36347,#36348,#36349,
#36350,#36351,#36352,#36353,#36354,#36355,#36356,#36357,#36358,#36359,#36360,
#36361,#36362,#36363,#36364,#36365,#36366,#36367,#36368,#36369,#36370,#36371,
#36372,#36373,#36374,#36375,#36376,#36377,#36378,#36379,#36380,#36381,#36382,
#36383,#36384,#36385,#36386,#36387,#36388,#36389,#36390,#36391,#36392,#36393,
#36394,#36395,#36396,#36397,#36398,#36399,#36400,#36401,#36402,#36403,#36404,
#36405)),.UNSPECIFIED.,.F.,.F.,.F.,(4,4),(4,1,1,1,1,1,1,1,1,1,1,1,1,1,1,
1,1,1,1,1,1,1,1,1,1,1,1,1,1,1,1,1,1,1,1,1,1,1,1,1,1,1,1,1,1,1,1,1,1,1,1,
1,1,1,1,1,1,1,1,1,1,4),(0.,0.0965329650085053),(14.399609326548,14.8893485941236,
15.3790878616992,15.8688271292748,16.3585663968504,16.848305664426,17.3380449320016,
17.8277841995772,18.3175234671527,18.8072627347283,19.2970020023039,19.7867412698795,
20.2764805374551,20.7662198050307,21.2559590726063,21.7456983401819,22.2354376077575,
22.7251768753331,23.2149161429087,23.7046554104842,24.1943946780598,24.6841339456354,
25.173873213211,25.6636124807866,26.1533517483622,26.6430910159378,27.1328302835134,
27.622569551089,28.1123088186646,28.6020480862402,29.0917873538157,30.0712658889669,
31.0507444241181,32.0302229592693,32.5199622268449,33.0097014944205,33.4994407619961,
33.9891800295717,34.4789192971472,34.9686585647228,35.4583978322984,35.948137099874,
36.4378763674496,36.9276156350252,37.4173549026008,37.9070941701764,38.396833437752,
38.8865727053276,39.3763119729032,39.8660512404787,40.3557905080543,40.8455297756299,
41.3352690432055,41.8250083107811,42.3147475783567,42.8044868459323,43.2942261135079,
43.7839653810835,44.2737046486591,44.7634439162347,45.2531831838103,45.7429224513858),
 .UNSPECIFIED.);
#276=B_SPLINE_SURFACE_WITH_KNOTS('',3,3,((#36810,#36811,#36812,#36813,#36814,
#36815,#36816,#36817,#36818,#36819,#36820,#36821,#36822,#36823,#36824,#36825,
#36826,#36827,#36828,#36829,#36830,#36831,#36832,#36833,#36834,#36835,#36836,
#36837,#36838,#36839,#36840,#36841,#36842,#36843,#36844,#36845,#36846,#36847,
#36848,#36849,#36850,#36851,#36852,#36853,#36854,#36855,#36856,#36857,#36858,
#36859,#36860,#36861,#36862,#36863,#36864,#36865,#36866,#36867,#36868,#36869,
#36870,#36871,#36872,#36873),(#36874,#36875,#36876,#36877,#36878,#36879,
#36880,#36881,#36882,#36883,#36884,#36885,#36886,#36887,#36888,#36889,#36890,
#36891,#36892,#36893,#36894,#36895,#36896,#36897,#36898,#36899,#36900,#36901,
#36902,#36903,#36904,#36905,#36906,#36907,#36908,#36909,#36910,#36911,#36912,
#36913,#36914,#36915,#36916,#36917,#36918,#36919,#36920,#36921,#36922,#36923,
#36924,#36925,#36926,#36927,#36928,#36929,#36930,#36931,#36932,#36933,#36934,
#36935,#36936,#36937),(#36938,#36939,#36940,#36941,#36942,#36943,#36944,
#36945,#36946,#36947,#36948,#36949,#36950,#36951,#36952,#36953,#36954,#36955,
#36956,#36957,#36958,#36959,#36960,#36961,#36962,#36963,#36964,#36965,#36966,
#36967,#36968,#36969,#36970,#36971,#36972,#36973,#36974,#36975,#36976,#36977,
#36978,#36979,#36980,#36981,#36982,#36983,#36984,#36985,#36986,#36987,#36988,
#36989,#36990,#36991,#36992,#36993,#36994,#36995,#36996,#36997,#36998,#36999,
#37000,#37001),(#37002,#37003,#37004,#37005,#37006,#37007,#37008,#37009,
#37010,#37011,#37012,#37013,#37014,#37015,#37016,#37017,#37018,#37019,#37020,
#37021,#37022,#37023,#37024,#37025,#37026,#37027,#37028,#37029,#37030,#37031,
#37032,#37033,#37034,#37035,#37036,#37037,#37038,#37039,#37040,#37041,#37042,
#37043,#37044,#37045,#37046,#37047,#37048,#37049,#37050,#37051,#37052,#37053,
#37054,#37055,#37056,#37057,#37058,#37059,#37060,#37061,#37062,#37063,#37064,
#37065)),.UNSPECIFIED.,.F.,.F.,.F.,(4,4),(4,1,1,1,1,1,1,1,1,1,1,1,1,1,1,
1,1,1,1,1,1,1,1,1,1,1,1,1,1,1,1,1,1,1,1,1,1,1,1,1,1,1,1,1,1,1,1,1,1,1,1,
1,1,1,1,1,1,1,1,1,1,4),(0.,0.0965329650085053),(11.8529428644271,12.3426821320026,
12.8324213995782,13.3221606671538,13.8118999347294,14.301639202305,14.7913784698806,
15.2811177374562,15.7708570050318,16.2605962726074,16.750335540183,17.2400748077586,
17.7298140753341,18.2195533429097,18.7092926104853,19.1990318780609,19.6887711456365,
20.1785104132121,20.6682496807877,21.1579889483633,21.6477282159389,22.1374674835145,
22.6272067510901,23.1169460186656,23.6066852862412,24.0964245538168,24.5861638213924,
25.075903088968,25.5656423565436,26.0553816241192,26.5451208916948,27.524599426846,
28.5040779619971,29.4835564971483,29.9732957647239,30.4630350322995,30.9527742998751,
31.4425135674507,31.9322528350263,32.4219921026019,32.9117313701775,33.4014706377531,
33.8912099053287,34.3809491729042,34.8706884404798,35.3604277080554,35.850166975631,
36.3399062432066,36.8296455107822,37.3193847783578,37.8091240459334,38.298863313509,
38.7886025810846,39.2783418486601,39.7680811162357,40.2578203838113,40.7475596513869,
41.2372989189625,41.7270381865381,42.2167774541137,42.7065167216893,43.1962559892649),
 .UNSPECIFIED.);
#277=B_SPLINE_SURFACE_WITH_KNOTS('',3,3,((#37215,#37216,#37217,#37218,#37219,
#37220,#37221,#37222,#37223,#37224,#37225,#37226,#37227,#37228,#37229,#37230,
#37231,#37232,#37233,#37234,#37235,#37236,#37237,#37238,#37239,#37240,#37241,
#37242,#37243,#37244,#37245,#37246,#37247,#37248,#37249,#37250,#37251,#37252,
#37253,#37254,#37255,#37256,#37257,#37258,#37259,#37260,#37261,#37262,#37263,
#37264,#37265,#37266,#37267,#37268,#37269,#37270,#37271,#37272,#37273,#37274,
#37275,#37276,#37277,#37278),(#37279,#37280,#37281,#37282,#37283,#37284,
#37285,#37286,#37287,#37288,#37289,#37290,#37291,#37292,#37293,#37294,#37295,
#37296,#37297,#37298,#37299,#37300,#37301,#37302,#37303,#37304,#37305,#37306,
#37307,#37308,#37309,#37310,#37311,#37312,#37313,#37314,#37315,#37316,#37317,
#37318,#37319,#37320,#37321,#37322,#37323,#37324,#37325,#37326,#37327,#37328,
#37329,#37330,#37331,#37332,#37333,#37334,#37335,#37336,#37337,#37338,#37339,
#37340,#37341,#37342),(#37343,#37344,#37345,#37346,#37347,#37348,#37349,
#37350,#37351,#37352,#37353,#37354,#37355,#37356,#37357,#37358,#37359,#37360,
#37361,#37362,#37363,#37364,#37365,#37366,#37367,#37368,#37369,#37370,#37371,
#37372,#37373,#37374,#37375,#37376,#37377,#37378,#37379,#37380,#37381,#37382,
#37383,#37384,#37385,#37386,#37387,#37388,#37389,#37390,#37391,#37392,#37393,
#37394,#37395,#37396,#37397,#37398,#37399,#37400,#37401,#37402,#37403,#37404,
#37405,#37406),(#37407,#37408,#37409,#37410,#37411,#37412,#37413,#37414,
#37415,#37416,#37417,#37418,#37419,#37420,#37421,#37422,#37423,#37424,#37425,
#37426,#37427,#37428,#37429,#37430,#37431,#37432,#37433,#37434,#37435,#37436,
#37437,#37438,#37439,#37440,#37441,#37442,#37443,#37444,#37445,#37446,#37447,
#37448,#37449,#37450,#37451,#37452,#37453,#37454,#37455,#37456,#37457,#37458,
#37459,#37460,#37461,#37462,#37463,#37464,#37465,#37466,#37467,#37468,#37469,
#37470)),.UNSPECIFIED.,.F.,.F.,.F.,(4,4),(4,1,1,1,1,1,1,1,1,1,1,1,1,1,1,
1,1,1,1,1,1,1,1,1,1,1,1,1,1,1,1,1,1,1,1,1,1,1,1,1,1,1,1,1,1,1,1,1,1,1,1,
1,1,1,1,1,1,1,1,1,1,4),(0.,0.0965329650085053),(14.399609326548,14.8893485941236,
15.3790878616992,15.8688271292748,16.3585663968504,16.848305664426,17.3380449320016,
17.8277841995772,18.3175234671527,18.8072627347283,19.2970020023039,19.7867412698795,
20.2764805374551,20.7662198050307,21.2559590726063,21.7456983401819,22.2354376077575,
22.7251768753331,23.2149161429087,23.7046554104842,24.1943946780598,24.6841339456354,
25.173873213211,25.6636124807866,26.1533517483622,26.6430910159378,27.1328302835134,
27.622569551089,28.1123088186646,28.6020480862402,29.0917873538157,30.0712658889669,
31.0507444241181,32.0302229592693,32.5199622268449,33.0097014944205,33.4994407619961,
33.9891800295717,34.4789192971472,34.9686585647228,35.4583978322984,35.948137099874,
36.4378763674496,36.9276156350252,37.4173549026008,37.9070941701764,38.396833437752,
38.8865727053276,39.3763119729032,39.8660512404787,40.3557905080543,40.8455297756299,
41.3352690432055,41.8250083107811,42.3147475783567,42.8044868459323,43.2942261135079,
43.7839653810835,44.2737046486591,44.7634439162347,45.2531831838103,45.7429224513858),
 .UNSPECIFIED.);
#278=B_SPLINE_SURFACE_WITH_KNOTS('',3,3,((#37875,#37876,#37877,#37878,#37879,
#37880,#37881,#37882,#37883,#37884,#37885,#37886,#37887,#37888,#37889,#37890,
#37891,#37892,#37893,#37894,#37895,#37896,#37897,#37898,#37899,#37900,#37901,
#37902,#37903,#37904,#37905,#37906,#37907,#37908,#37909,#37910,#37911,#37912,
#37913,#37914,#37915,#37916,#37917,#37918,#37919,#37920,#37921,#37922,#37923,
#37924,#37925,#37926,#37927,#37928,#37929,#37930,#37931,#37932,#37933,#37934,
#37935,#37936,#37937,#37938),(#37939,#37940,#37941,#37942,#37943,#37944,
#37945,#37946,#37947,#37948,#37949,#37950,#37951,#37952,#37953,#37954,#37955,
#37956,#37957,#37958,#37959,#37960,#37961,#37962,#37963,#37964,#37965,#37966,
#37967,#37968,#37969,#37970,#37971,#37972,#37973,#37974,#37975,#37976,#37977,
#37978,#37979,#37980,#37981,#37982,#37983,#37984,#37985,#37986,#37987,#37988,
#37989,#37990,#37991,#37992,#37993,#37994,#37995,#37996,#37997,#37998,#37999,
#38000,#38001,#38002),(#38003,#38004,#38005,#38006,#38007,#38008,#38009,
#38010,#38011,#38012,#38013,#38014,#38015,#38016,#38017,#38018,#38019,#38020,
#38021,#38022,#38023,#38024,#38025,#38026,#38027,#38028,#38029,#38030,#38031,
#38032,#38033,#38034,#38035,#38036,#38037,#38038,#38039,#38040,#38041,#38042,
#38043,#38044,#38045,#38046,#38047,#38048,#38049,#38050,#38051,#38052,#38053,
#38054,#38055,#38056,#38057,#38058,#38059,#38060,#38061,#38062,#38063,#38064,
#38065,#38066),(#38067,#38068,#38069,#38070,#38071,#38072,#38073,#38074,
#38075,#38076,#38077,#38078,#38079,#38080,#38081,#38082,#38083,#38084,#38085,
#38086,#38087,#38088,#38089,#38090,#38091,#38092,#38093,#38094,#38095,#38096,
#38097,#38098,#38099,#38100,#38101,#38102,#38103,#38104,#38105,#38106,#38107,
#38108,#38109,#38110,#38111,#38112,#38113,#38114,#38115,#38116,#38117,#38118,
#38119,#38120,#38121,#38122,#38123,#38124,#38125,#38126,#38127,#38128,#38129,
#38130)),.UNSPECIFIED.,.F.,.F.,.F.,(4,4),(4,1,1,1,1,1,1,1,1,1,1,1,1,1,1,
1,1,1,1,1,1,1,1,1,1,1,1,1,1,1,1,1,1,1,1,1,1,1,1,1,1,1,1,1,1,1,1,1,1,1,1,
1,1,1,1,1,1,1,1,1,1,4),(0.,0.0965329650085053),(11.8529428644271,12.3426821320026,
12.8324213995782,13.3221606671538,13.8118999347294,14.301639202305,14.7913784698806,
15.2811177374562,15.7708570050318,16.2605962726074,16.750335540183,17.2400748077586,
17.7298140753341,18.2195533429097,18.7092926104853,19.1990318780609,19.6887711456365,
20.1785104132121,20.6682496807877,21.1579889483633,21.6477282159389,22.1374674835145,
22.6272067510901,23.1169460186656,23.6066852862412,24.0964245538168,24.5861638213924,
25.075903088968,25.5656423565436,26.0553816241192,26.5451208916948,27.524599426846,
28.5040779619971,29.4835564971483,29.9732957647239,30.4630350322995,30.9527742998751,
31.4425135674507,31.9322528350263,32.4219921026019,32.9117313701775,33.4014706377531,
33.8912099053287,34.3809491729042,34.8706884404798,35.3604277080554,35.850166975631,
36.3399062432066,36.8296455107822,37.3193847783578,37.8091240459334,38.298863313509,
38.7886025810846,39.2783418486601,39.7680811162357,40.2578203838113,40.7475596513869,
41.2372989189625,41.7270381865381,42.2167774541137,42.7065167216893,43.1962559892649),
 .UNSPECIFIED.);
#279=B_SPLINE_SURFACE_WITH_KNOTS('',3,3,((#38280,#38281,#38282,#38283,#38284,
#38285,#38286,#38287,#38288,#38289,#38290,#38291,#38292,#38293,#38294,#38295,
#38296,#38297,#38298,#38299,#38300,#38301,#38302,#38303,#38304,#38305,#38306,
#38307,#38308,#38309,#38310,#38311,#38312,#38313,#38314,#38315,#38316,#38317,
#38318,#38319,#38320,#38321,#38322,#38323,#38324,#38325,#38326,#38327,#38328,
#38329,#38330,#38331,#38332,#38333,#38334,#38335,#38336,#38337,#38338,#38339,
#38340,#38341,#38342,#38343),(#38344,#38345,#38346,#38347,#38348,#38349,
#38350,#38351,#38352,#38353,#38354,#38355,#38356,#38357,#38358,#38359,#38360,
#38361,#38362,#38363,#38364,#38365,#38366,#38367,#38368,#38369,#38370,#38371,
#38372,#38373,#38374,#38375,#38376,#38377,#38378,#38379,#38380,#38381,#38382,
#38383,#38384,#38385,#38386,#38387,#38388,#38389,#38390,#38391,#38392,#38393,
#38394,#38395,#38396,#38397,#38398,#38399,#38400,#38401,#38402,#38403,#38404,
#38405,#38406,#38407),(#38408,#38409,#38410,#38411,#38412,#38413,#38414,
#38415,#38416,#38417,#38418,#38419,#38420,#38421,#38422,#38423,#38424,#38425,
#38426,#38427,#38428,#38429,#38430,#38431,#38432,#38433,#38434,#38435,#38436,
#38437,#38438,#38439,#38440,#38441,#38442,#38443,#38444,#38445,#38446,#38447,
#38448,#38449,#38450,#38451,#38452,#38453,#38454,#38455,#38456,#38457,#38458,
#38459,#38460,#38461,#38462,#38463,#38464,#38465,#38466,#38467,#38468,#38469,
#38470,#38471),(#38472,#38473,#38474,#38475,#38476,#38477,#38478,#38479,
#38480,#38481,#38482,#38483,#38484,#38485,#38486,#38487,#38488,#38489,#38490,
#38491,#38492,#38493,#38494,#38495,#38496,#38497,#38498,#38499,#38500,#38501,
#38502,#38503,#38504,#38505,#38506,#38507,#38508,#38509,#38510,#38511,#38512,
#38513,#38514,#38515,#38516,#38517,#38518,#38519,#38520,#38521,#38522,#38523,
#38524,#38525,#38526,#38527,#38528,#38529,#38530,#38531,#38532,#38533,#38534,
#38535)),.UNSPECIFIED.,.F.,.F.,.F.,(4,4),(4,1,1,1,1,1,1,1,1,1,1,1,1,1,1,
1,1,1,1,1,1,1,1,1,1,1,1,1,1,1,1,1,1,1,1,1,1,1,1,1,1,1,1,1,1,1,1,1,1,1,1,
1,1,1,1,1,1,1,1,1,1,4),(0.,0.0965329650085053),(14.399609326548,14.8893485941236,
15.3790878616992,15.8688271292748,16.3585663968504,16.848305664426,17.3380449320016,
17.8277841995772,18.3175234671527,18.8072627347283,19.2970020023039,19.7867412698795,
20.2764805374551,20.7662198050307,21.2559590726063,21.7456983401819,22.2354376077575,
22.7251768753331,23.2149161429087,23.7046554104842,24.1943946780598,24.6841339456354,
25.173873213211,25.6636124807866,26.1533517483622,26.6430910159378,27.1328302835134,
27.622569551089,28.1123088186646,28.6020480862402,29.0917873538157,30.0712658889669,
31.0507444241181,32.0302229592693,32.5199622268449,33.0097014944205,33.4994407619961,
33.9891800295717,34.4789192971472,34.9686585647228,35.4583978322984,35.948137099874,
36.4378763674496,36.9276156350252,37.4173549026008,37.9070941701764,38.396833437752,
38.8865727053276,39.3763119729032,39.8660512404787,40.3557905080543,40.8455297756299,
41.3352690432055,41.8250083107811,42.3147475783567,42.8044868459323,43.2942261135079,
43.7839653810835,44.2737046486591,44.7634439162347,45.2531831838103,45.7429224513858),
 .UNSPECIFIED.);
#280=B_SPLINE_SURFACE_WITH_KNOTS('',3,3,((#38940,#38941,#38942,#38943,#38944,
#38945,#38946,#38947,#38948,#38949,#38950,#38951,#38952,#38953,#38954,#38955,
#38956,#38957,#38958,#38959,#38960,#38961,#38962,#38963,#38964,#38965,#38966,
#38967,#38968,#38969,#38970,#38971,#38972,#38973,#38974,#38975,#38976,#38977,
#38978,#38979,#38980,#38981,#38982,#38983,#38984,#38985,#38986,#38987,#38988,
#38989,#38990,#38991,#38992,#38993,#38994,#38995,#38996,#38997,#38998,#38999,
#39000,#39001,#39002,#39003),(#39004,#39005,#39006,#39007,#39008,#39009,
#39010,#39011,#39012,#39013,#39014,#39015,#39016,#39017,#39018,#39019,#39020,
#39021,#39022,#39023,#39024,#39025,#39026,#39027,#39028,#39029,#39030,#39031,
#39032,#39033,#39034,#39035,#39036,#39037,#39038,#39039,#39040,#39041,#39042,
#39043,#39044,#39045,#39046,#39047,#39048,#39049,#39050,#39051,#39052,#39053,
#39054,#39055,#39056,#39057,#39058,#39059,#39060,#39061,#39062,#39063,#39064,
#39065,#39066,#39067),(#39068,#39069,#39070,#39071,#39072,#39073,#39074,
#39075,#39076,#39077,#39078,#39079,#39080,#39081,#39082,#39083,#39084,#39085,
#39086,#39087,#39088,#39089,#39090,#39091,#39092,#39093,#39094,#39095,#39096,
#39097,#39098,#39099,#39100,#39101,#39102,#39103,#39104,#39105,#39106,#39107,
#39108,#39109,#39110,#39111,#39112,#39113,#39114,#39115,#39116,#39117,#39118,
#39119,#39120,#39121,#39122,#39123,#39124,#39125,#39126,#39127,#39128,#39129,
#39130,#39131),(#39132,#39133,#39134,#39135,#39136,#39137,#39138,#39139,
#39140,#39141,#39142,#39143,#39144,#39145,#39146,#39147,#39148,#39149,#39150,
#39151,#39152,#39153,#39154,#39155,#39156,#39157,#39158,#39159,#39160,#39161,
#39162,#39163,#39164,#39165,#39166,#39167,#39168,#39169,#39170,#39171,#39172,
#39173,#39174,#39175,#39176,#39177,#39178,#39179,#39180,#39181,#39182,#39183,
#39184,#39185,#39186,#39187,#39188,#39189,#39190,#39191,#39192,#39193,#39194,
#39195)),.UNSPECIFIED.,.F.,.F.,.F.,(4,4),(4,1,1,1,1,1,1,1,1,1,1,1,1,1,1,
1,1,1,1,1,1,1,1,1,1,1,1,1,1,1,1,1,1,1,1,1,1,1,1,1,1,1,1,1,1,1,1,1,1,1,1,
1,1,1,1,1,1,1,1,1,1,4),(0.,0.0965329650085053),(11.8529428644271,12.3426821320026,
12.8324213995782,13.3221606671538,13.8118999347294,14.301639202305,14.7913784698806,
15.2811177374562,15.7708570050318,16.2605962726074,16.750335540183,17.2400748077586,
17.7298140753341,18.2195533429097,18.7092926104853,19.1990318780609,19.6887711456365,
20.1785104132121,20.6682496807877,21.1579889483633,21.6477282159389,22.1374674835145,
22.6272067510901,23.1169460186656,23.6066852862412,24.0964245538168,24.5861638213924,
25.075903088968,25.5656423565436,26.0553816241192,26.5451208916948,27.524599426846,
28.5040779619972,29.4835564971483,29.9732957647239,30.4630350322995,30.9527742998751,
31.4425135674507,31.9322528350263,32.4219921026019,32.9117313701775,33.4014706377531,
33.8912099053287,34.3809491729042,34.8706884404798,35.3604277080554,35.850166975631,
36.3399062432066,36.8296455107822,37.3193847783578,37.8091240459334,38.298863313509,
38.7886025810846,39.2783418486602,39.7680811162357,40.2578203838113,40.7475596513869,
41.2372989189625,41.7270381865381,42.2167774541137,42.7065167216893,43.1962559892649),
 .UNSPECIFIED.);
#281=B_SPLINE_SURFACE_WITH_KNOTS('',3,3,((#39345,#39346,#39347,#39348,#39349,
#39350,#39351,#39352,#39353,#39354,#39355,#39356,#39357,#39358,#39359,#39360,
#39361,#39362,#39363,#39364,#39365,#39366,#39367,#39368,#39369,#39370,#39371,
#39372,#39373,#39374,#39375,#39376,#39377,#39378,#39379,#39380,#39381,#39382,
#39383,#39384,#39385,#39386,#39387,#39388,#39389,#39390,#39391,#39392,#39393,
#39394,#39395,#39396,#39397,#39398,#39399,#39400,#39401,#39402,#39403,#39404,
#39405,#39406,#39407,#39408),(#39409,#39410,#39411,#39412,#39413,#39414,
#39415,#39416,#39417,#39418,#39419,#39420,#39421,#39422,#39423,#39424,#39425,
#39426,#39427,#39428,#39429,#39430,#39431,#39432,#39433,#39434,#39435,#39436,
#39437,#39438,#39439,#39440,#39441,#39442,#39443,#39444,#39445,#39446,#39447,
#39448,#39449,#39450,#39451,#39452,#39453,#39454,#39455,#39456,#39457,#39458,
#39459,#39460,#39461,#39462,#39463,#39464,#39465,#39466,#39467,#39468,#39469,
#39470,#39471,#39472),(#39473,#39474,#39475,#39476,#39477,#39478,#39479,
#39480,#39481,#39482,#39483,#39484,#39485,#39486,#39487,#39488,#39489,#39490,
#39491,#39492,#39493,#39494,#39495,#39496,#39497,#39498,#39499,#39500,#39501,
#39502,#39503,#39504,#39505,#39506,#39507,#39508,#39509,#39510,#39511,#39512,
#39513,#39514,#39515,#39516,#39517,#39518,#39519,#39520,#39521,#39522,#39523,
#39524,#39525,#39526,#39527,#39528,#39529,#39530,#39531,#39532,#39533,#39534,
#39535,#39536),(#39537,#39538,#39539,#39540,#39541,#39542,#39543,#39544,
#39545,#39546,#39547,#39548,#39549,#39550,#39551,#39552,#39553,#39554,#39555,
#39556,#39557,#39558,#39559,#39560,#39561,#39562,#39563,#39564,#39565,#39566,
#39567,#39568,#39569,#39570,#39571,#39572,#39573,#39574,#39575,#39576,#39577,
#39578,#39579,#39580,#39581,#39582,#39583,#39584,#39585,#39586,#39587,#39588,
#39589,#39590,#39591,#39592,#39593,#39594,#39595,#39596,#39597,#39598,#39599,
#39600)),.UNSPECIFIED.,.F.,.F.,.F.,(4,4),(4,1,1,1,1,1,1,1,1,1,1,1,1,1,1,
1,1,1,1,1,1,1,1,1,1,1,1,1,1,1,1,1,1,1,1,1,1,1,1,1,1,1,1,1,1,1,1,1,1,1,1,
1,1,1,1,1,1,1,1,1,1,4),(0.,0.0965329650085053),(14.399609326548,14.8893485941236,
15.3790878616992,15.8688271292748,16.3585663968504,16.848305664426,17.3380449320016,
17.8277841995772,18.3175234671527,18.8072627347283,19.2970020023039,19.7867412698795,
20.2764805374551,20.7662198050307,21.2559590726063,21.7456983401819,22.2354376077575,
22.7251768753331,23.2149161429087,23.7046554104842,24.1943946780598,24.6841339456354,
25.173873213211,25.6636124807866,26.1533517483622,26.6430910159378,27.1328302835134,
27.622569551089,28.1123088186646,28.6020480862402,29.0917873538157,30.0712658889669,
31.0507444241181,32.0302229592693,32.5199622268449,33.0097014944205,33.4994407619961,
33.9891800295717,34.4789192971472,34.9686585647228,35.4583978322984,35.948137099874,
36.4378763674496,36.9276156350252,37.4173549026008,37.9070941701764,38.396833437752,
38.8865727053276,39.3763119729032,39.8660512404787,40.3557905080543,40.8455297756299,
41.3352690432055,41.8250083107811,42.3147475783567,42.8044868459323,43.2942261135079,
43.7839653810835,44.2737046486591,44.7634439162347,45.2531831838103,45.7429224513858),
 .UNSPECIFIED.);
#282=B_SPLINE_SURFACE_WITH_KNOTS('',3,3,((#39975,#39976,#39977,#39978,#39979,
#39980,#39981,#39982,#39983,#39984,#39985,#39986,#39987,#39988,#39989,#39990,
#39991,#39992,#39993,#39994,#39995,#39996,#39997,#39998,#39999,#40000,#40001,
#40002,#40003,#40004,#40005,#40006,#40007,#40008,#40009,#40010,#40011,#40012,
#40013,#40014,#40015,#40016,#40017,#40018,#40019,#40020,#40021,#40022,#40023,
#40024,#40025),(#40026,#40027,#40028,#40029,#40030,#40031,#40032,#40033,
#40034,#40035,#40036,#40037,#40038,#40039,#40040,#40041,#40042,#40043,#40044,
#40045,#40046,#40047,#40048,#40049,#40050,#40051,#40052,#40053,#40054,#40055,
#40056,#40057,#40058,#40059,#40060,#40061,#40062,#40063,#40064,#40065,#40066,
#40067,#40068,#40069,#40070,#40071,#40072,#40073,#40074,#40075,#40076),
(#40077,#40078,#40079,#40080,#40081,#40082,#40083,#40084,#40085,#40086,
#40087,#40088,#40089,#40090,#40091,#40092,#40093,#40094,#40095,#40096,#40097,
#40098,#40099,#40100,#40101,#40102,#40103,#40104,#40105,#40106,#40107,#40108,
#40109,#40110,#40111,#40112,#40113,#40114,#40115,#40116,#40117,#40118,#40119,
#40120,#40121,#40122,#40123,#40124,#40125,#40126,#40127),(#40128,#40129,
#40130,#40131,#40132,#40133,#40134,#40135,#40136,#40137,#40138,#40139,#40140,
#40141,#40142,#40143,#40144,#40145,#40146,#40147,#40148,#40149,#40150,#40151,
#40152,#40153,#40154,#40155,#40156,#40157,#40158,#40159,#40160,#40161,#40162,
#40163,#40164,#40165,#40166,#40167,#40168,#40169,#40170,#40171,#40172,#40173,
#40174,#40175,#40176,#40177,#40178)),.UNSPECIFIED.,.F.,.F.,.F.,(4,4),(4,
1,1,1,1,1,1,1,1,1,1,1,1,1,1,1,1,1,1,1,1,1,1,1,1,1,1,1,1,1,1,1,1,1,1,1,1,
1,1,1,1,1,1,1,1,1,1,1,4),(0.,0.0802805549308171),(11.8575378228164,12.8420504191595,
13.8265630155026,14.8110756118456,15.7955882081887,16.7801008045318,17.7646134008748,
18.7491259972179,19.733638593561,20.718151189904,21.7026637862471,22.6871763825902,
23.6716889789332,24.6562015752763,25.6407141716194,26.6252267679624,27.6097393643055,
28.5942519606485,29.5787645569916,30.5632771533347,31.5477897496777,32.5323023460208,
33.5168149423639,34.5013275387069,35.48584013505,36.4703527313931,37.4548653277361,
38.4393779240792,39.4238905204223,40.4084031167653,41.3929157131084,42.3774283094515,
43.3619409057945,44.3464535021376,45.3309660984807,46.3154786948237,47.2999912911668,
48.2845038875099,49.2690164838529,50.253529080196,51.2380416765391,52.2225542728821,
53.2070668692252,54.1915794655683,55.1760920619113,56.1606046582544,57.1451172545975,
58.1296298509405,59.1141424472836),.UNSPECIFIED.);
#283=B_SPLINE_SURFACE_WITH_KNOTS('',3,3,((#40298,#40299,#40300,#40301,#40302,
#40303,#40304,#40305,#40306,#40307,#40308,#40309,#40310,#40311,#40312,#40313,
#40314,#40315,#40316,#40317,#40318,#40319,#40320,#40321,#40322,#40323,#40324,
#40325,#40326,#40327,#40328,#40329,#40330,#40331,#40332,#40333,#40334,#40335,
#40336,#40337,#40338,#40339,#40340,#40341,#40342,#40343,#40344,#40345,#40346,
#40347,#40348),(#40349,#40350,#40351,#40352,#40353,#40354,#40355,#40356,
#40357,#40358,#40359,#40360,#40361,#40362,#40363,#40364,#40365,#40366,#40367,
#40368,#40369,#40370,#40371,#40372,#40373,#40374,#40375,#40376,#40377,#40378,
#40379,#40380,#40381,#40382,#40383,#40384,#40385,#40386,#40387,#40388,#40389,
#40390,#40391,#40392,#40393,#40394,#40395,#40396,#40397,#40398,#40399),
(#40400,#40401,#40402,#40403,#40404,#40405,#40406,#40407,#40408,#40409,
#40410,#40411,#40412,#40413,#40414,#40415,#40416,#40417,#40418,#40419,#40420,
#40421,#40422,#40423,#40424,#40425,#40426,#40427,#40428,#40429,#40430,#40431,
#40432,#40433,#40434,#40435,#40436,#40437,#40438,#40439,#40440,#40441,#40442,
#40443,#40444,#40445,#40446,#40447,#40448,#40449,#40450),(#40451,#40452,
#40453,#40454,#40455,#40456,#40457,#40458,#40459,#40460,#40461,#40462,#40463,
#40464,#40465,#40466,#40467,#40468,#40469,#40470,#40471,#40472,#40473,#40474,
#40475,#40476,#40477,#40478,#40479,#40480,#40481,#40482,#40483,#40484,#40485,
#40486,#40487,#40488,#40489,#40490,#40491,#40492,#40493,#40494,#40495,#40496,
#40497,#40498,#40499,#40500,#40501)),.UNSPECIFIED.,.F.,.F.,.F.,(4,4),(4,
1,1,1,1,1,1,1,1,1,1,1,1,1,1,1,1,1,1,1,1,1,1,1,1,1,1,1,1,1,1,1,1,1,1,1,1,
1,1,1,1,1,1,1,1,1,1,1,4),(0.,0.0802805549308171),(14.3991256467175,15.3836382430606,
16.3681508394037,17.3526634357467,18.3371760320898,19.3216886284329,20.3062012247759,
21.290713821119,22.2752264174621,23.2597390138051,24.2442516101482,25.2287642064913,
26.2132768028343,27.1977893991774,28.1823019955205,29.1668145918635,30.1513271882066,
31.1358397845497,32.1203523808927,33.1048649772358,34.0893775735789,35.0738901699219,
36.058402766265,37.0429153626081,38.0274279589511,39.0119405552942,39.9964531516373,
40.9809657479803,41.9654783443234,42.9499909406665,43.9345035370095,44.9190161333526,
45.9035287296957,46.8880413260387,47.8725539223818,48.8570665187248,49.8415791150679,
50.826091711411,51.810604307754,52.7951169040971,53.7796295004402,54.7641420967832,
55.7486546931263,56.7331672894694,57.7176798858124,58.7021924821555,59.6867050784986,
60.6712176748416,61.6557302711847),.UNSPECIFIED.);
#284=B_SPLINE_SURFACE_WITH_KNOTS('',3,3,((#40848,#40849,#40850,#40851,#40852,
#40853,#40854,#40855,#40856,#40857,#40858,#40859,#40860,#40861,#40862,#40863,
#40864,#40865,#40866,#40867,#40868,#40869,#40870,#40871,#40872,#40873,#40874,
#40875,#40876,#40877,#40878,#40879,#40880,#40881,#40882,#40883,#40884,#40885,
#40886,#40887,#40888,#40889,#40890,#40891,#40892,#40893,#40894,#40895,#40896,
#40897,#40898),(#40899,#40900,#40901,#40902,#40903,#40904,#40905,#40906,
#40907,#40908,#40909,#40910,#40911,#40912,#40913,#40914,#40915,#40916,#40917,
#40918,#40919,#40920,#40921,#40922,#40923,#40924,#40925,#40926,#40927,#40928,
#40929,#40930,#40931,#40932,#40933,#40934,#40935,#40936,#40937,#40938,#40939,
#40940,#40941,#40942,#40943,#40944,#40945,#40946,#40947,#40948,#40949),
(#40950,#40951,#40952,#40953,#40954,#40955,#40956,#40957,#40958,#40959,
#40960,#40961,#40962,#40963,#40964,#40965,#40966,#40967,#40968,#40969,#40970,
#40971,#40972,#40973,#40974,#40975,#40976,#40977,#40978,#40979,#40980,#40981,
#40982,#40983,#40984,#40985,#40986,#40987,#40988,#40989,#40990,#40991,#40992,
#40993,#40994,#40995,#40996,#40997,#40998,#40999,#41000),(#41001,#41002,
#41003,#41004,#41005,#41006,#41007,#41008,#41009,#41010,#41011,#41012,#41013,
#41014,#41015,#41016,#41017,#41018,#41019,#41020,#41021,#41022,#41023,#41024,
#41025,#41026,#41027,#41028,#41029,#41030,#41031,#41032,#41033,#41034,#41035,
#41036,#41037,#41038,#41039,#41040,#41041,#41042,#41043,#41044,#41045,#41046,
#41047,#41048,#41049,#41050,#41051)),.UNSPECIFIED.,.F.,.F.,.F.,(4,4),(4,
1,1,1,1,1,1,1,1,1,1,1,1,1,1,1,1,1,1,1,1,1,1,1,1,1,1,1,1,1,1,1,1,1,1,1,1,
1,1,1,1,1,1,1,1,1,1,1,4),(0.,0.0802805549308171),(11.8575378228164,12.8420504191595,
13.8265630155026,14.8110756118456,15.7955882081887,16.7801008045318,17.7646134008748,
18.7491259972179,19.733638593561,20.718151189904,21.7026637862471,22.6871763825901,
23.6716889789332,24.6562015752763,25.6407141716193,26.6252267679624,27.6097393643055,
28.5942519606485,29.5787645569916,30.5632771533347,31.5477897496777,32.5323023460208,
33.5168149423639,34.5013275387069,35.48584013505,36.4703527313931,37.4548653277361,
38.4393779240792,39.4238905204223,40.4084031167653,41.3929157131084,42.3774283094515,
43.3619409057945,44.3464535021376,45.3309660984807,46.3154786948237,47.2999912911668,
48.2845038875099,49.2690164838529,50.253529080196,51.2380416765391,52.2225542728821,
53.2070668692252,54.1915794655683,55.1760920619113,56.1606046582544,57.1451172545975,
58.1296298509405,59.1141424472836),.UNSPECIFIED.);
#285=B_SPLINE_SURFACE_WITH_KNOTS('',3,3,((#41171,#41172,#41173,#41174,#41175,
#41176,#41177,#41178,#41179,#41180,#41181,#41182,#41183,#41184,#41185,#41186,
#41187,#41188,#41189,#41190,#41191,#41192,#41193,#41194,#41195,#41196,#41197,
#41198,#41199,#41200,#41201,#41202,#41203,#41204,#41205,#41206,#41207,#41208,
#41209,#41210,#41211,#41212,#41213,#41214,#41215,#41216,#41217,#41218,#41219,
#41220,#41221),(#41222,#41223,#41224,#41225,#41226,#41227,#41228,#41229,
#41230,#41231,#41232,#41233,#41234,#41235,#41236,#41237,#41238,#41239,#41240,
#41241,#41242,#41243,#41244,#41245,#41246,#41247,#41248,#41249,#41250,#41251,
#41252,#41253,#41254,#41255,#41256,#41257,#41258,#41259,#41260,#41261,#41262,
#41263,#41264,#41265,#41266,#41267,#41268,#41269,#41270,#41271,#41272),
(#41273,#41274,#41275,#41276,#41277,#41278,#41279,#41280,#41281,#41282,
#41283,#41284,#41285,#41286,#41287,#41288,#41289,#41290,#41291,#41292,#41293,
#41294,#41295,#41296,#41297,#41298,#41299,#41300,#41301,#41302,#41303,#41304,
#41305,#41306,#41307,#41308,#41309,#41310,#41311,#41312,#41313,#41314,#41315,
#41316,#41317,#41318,#41319,#41320,#41321,#41322,#41323),(#41324,#41325,
#41326,#41327,#41328,#41329,#41330,#41331,#41332,#41333,#41334,#41335,#41336,
#41337,#41338,#41339,#41340,#41341,#41342,#41343,#41344,#41345,#41346,#41347,
#41348,#41349,#41350,#41351,#41352,#41353,#41354,#41355,#41356,#41357,#41358,
#41359,#41360,#41361,#41362,#41363,#41364,#41365,#41366,#41367,#41368,#41369,
#41370,#41371,#41372,#41373,#41374)),.UNSPECIFIED.,.F.,.F.,.F.,(4,4),(4,
1,1,1,1,1,1,1,1,1,1,1,1,1,1,1,1,1,1,1,1,1,1,1,1,1,1,1,1,1,1,1,1,1,1,1,1,
1,1,1,1,1,1,1,1,1,1,1,4),(0.,0.0802805549308171),(14.3991256467175,15.3836382430606,
16.3681508394037,17.3526634357467,18.3371760320898,19.3216886284329,20.3062012247759,
21.290713821119,22.2752264174621,23.2597390138051,24.2442516101482,25.2287642064913,
26.2132768028343,27.1977893991774,28.1823019955205,29.1668145918635,30.1513271882066,
31.1358397845497,32.1203523808927,33.1048649772358,34.0893775735789,35.0738901699219,
36.058402766265,37.0429153626081,38.0274279589511,39.0119405552942,39.9964531516373,
40.9809657479803,41.9654783443234,42.9499909406665,43.9345035370095,44.9190161333526,
45.9035287296957,46.8880413260387,47.8725539223818,48.8570665187248,49.8415791150679,
50.826091711411,51.810604307754,52.7951169040971,53.7796295004402,54.7641420967832,
55.7486546931263,56.7331672894694,57.7176798858124,58.7021924821555,59.6867050784986,
60.6712176748416,61.6557302711847),.UNSPECIFIED.);
#286=B_SPLINE_SURFACE_WITH_KNOTS('',3,3,((#41721,#41722,#41723,#41724,#41725,
#41726,#41727,#41728,#41729,#41730,#41731,#41732,#41733,#41734,#41735,#41736,
#41737,#41738,#41739,#41740,#41741,#41742,#41743,#41744,#41745,#41746,#41747,
#41748,#41749,#41750,#41751,#41752,#41753,#41754,#41755,#41756,#41757,#41758,
#41759,#41760,#41761,#41762,#41763,#41764,#41765,#41766,#41767,#41768,#41769,
#41770,#41771),(#41772,#41773,#41774,#41775,#41776,#41777,#41778,#41779,
#41780,#41781,#41782,#41783,#41784,#41785,#41786,#41787,#41788,#41789,#41790,
#41791,#41792,#41793,#41794,#41795,#41796,#41797,#41798,#41799,#41800,#41801,
#41802,#41803,#41804,#41805,#41806,#41807,#41808,#41809,#41810,#41811,#41812,
#41813,#41814,#41815,#41816,#41817,#41818,#41819,#41820,#41821,#41822),
(#41823,#41824,#41825,#41826,#41827,#41828,#41829,#41830,#41831,#41832,
#41833,#41834,#41835,#41836,#41837,#41838,#41839,#41840,#41841,#41842,#41843,
#41844,#41845,#41846,#41847,#41848,#41849,#41850,#41851,#41852,#41853,#41854,
#41855,#41856,#41857,#41858,#41859,#41860,#41861,#41862,#41863,#41864,#41865,
#41866,#41867,#41868,#41869,#41870,#41871,#41872,#41873),(#41874,#41875,
#41876,#41877,#41878,#41879,#41880,#41881,#41882,#41883,#41884,#41885,#41886,
#41887,#41888,#41889,#41890,#41891,#41892,#41893,#41894,#41895,#41896,#41897,
#41898,#41899,#41900,#41901,#41902,#41903,#41904,#41905,#41906,#41907,#41908,
#41909,#41910,#41911,#41912,#41913,#41914,#41915,#41916,#41917,#41918,#41919,
#41920,#41921,#41922,#41923,#41924)),.UNSPECIFIED.,.F.,.F.,.F.,(4,4),(4,
1,1,1,1,1,1,1,1,1,1,1,1,1,1,1,1,1,1,1,1,1,1,1,1,1,1,1,1,1,1,1,1,1,1,1,1,
1,1,1,1,1,1,1,1,1,1,1,4),(0.,0.0802805549308171),(11.8575378228164,12.8420504191595,
13.8265630155026,14.8110756118456,15.7955882081887,16.7801008045318,17.7646134008748,
18.7491259972179,19.733638593561,20.718151189904,21.7026637862471,22.6871763825901,
23.6716889789332,24.6562015752763,25.6407141716193,26.6252267679624,27.6097393643055,
28.5942519606485,29.5787645569916,30.5632771533347,31.5477897496777,32.5323023460208,
33.5168149423639,34.5013275387069,35.48584013505,36.4703527313931,37.4548653277361,
38.4393779240792,39.4238905204223,40.4084031167653,41.3929157131084,42.3774283094515,
43.3619409057945,44.3464535021376,45.3309660984807,46.3154786948237,47.2999912911668,
48.2845038875099,49.2690164838529,50.253529080196,51.2380416765391,52.2225542728821,
53.2070668692252,54.1915794655683,55.1760920619113,56.1606046582544,57.1451172545975,
58.1296298509405,59.1141424472836),.UNSPECIFIED.);
#287=B_SPLINE_SURFACE_WITH_KNOTS('',3,3,((#42044,#42045,#42046,#42047,#42048,
#42049,#42050,#42051,#42052,#42053,#42054,#42055,#42056,#42057,#42058,#42059,
#42060,#42061,#42062,#42063,#42064,#42065,#42066,#42067,#42068,#42069,#42070,
#42071,#42072,#42073,#42074,#42075,#42076,#42077,#42078,#42079,#42080,#42081,
#42082,#42083,#42084,#42085,#42086,#42087,#42088,#42089,#42090,#42091,#42092,
#42093,#42094),(#42095,#42096,#42097,#42098,#42099,#42100,#42101,#42102,
#42103,#42104,#42105,#42106,#42107,#42108,#42109,#42110,#42111,#42112,#42113,
#42114,#42115,#42116,#42117,#42118,#42119,#42120,#42121,#42122,#42123,#42124,
#42125,#42126,#42127,#42128,#42129,#42130,#42131,#42132,#42133,#42134,#42135,
#42136,#42137,#42138,#42139,#42140,#42141,#42142,#42143,#42144,#42145),
(#42146,#42147,#42148,#42149,#42150,#42151,#42152,#42153,#42154,#42155,
#42156,#42157,#42158,#42159,#42160,#42161,#42162,#42163,#42164,#42165,#42166,
#42167,#42168,#42169,#42170,#42171,#42172,#42173,#42174,#42175,#42176,#42177,
#42178,#42179,#42180,#42181,#42182,#42183,#42184,#42185,#42186,#42187,#42188,
#42189,#42190,#42191,#42192,#42193,#42194,#42195,#42196),(#42197,#42198,
#42199,#42200,#42201,#42202,#42203,#42204,#42205,#42206,#42207,#42208,#42209,
#42210,#42211,#42212,#42213,#42214,#42215,#42216,#42217,#42218,#42219,#42220,
#42221,#42222,#42223,#42224,#42225,#42226,#42227,#42228,#42229,#42230,#42231,
#42232,#42233,#42234,#42235,#42236,#42237,#42238,#42239,#42240,#42241,#42242,
#42243,#42244,#42245,#42246,#42247)),.UNSPECIFIED.,.F.,.F.,.F.,(4,4),(4,
1,1,1,1,1,1,1,1,1,1,1,1,1,1,1,1,1,1,1,1,1,1,1,1,1,1,1,1,1,1,1,1,1,1,1,1,
1,1,1,1,1,1,1,1,1,1,1,4),(0.,0.0802805549308171),(14.3991256467175,15.3836382430606,
16.3681508394037,17.3526634357467,18.3371760320898,19.3216886284329,20.3062012247759,
21.290713821119,22.2752264174621,23.2597390138051,24.2442516101482,25.2287642064913,
26.2132768028343,27.1977893991774,28.1823019955205,29.1668145918635,30.1513271882066,
31.1358397845496,32.1203523808927,33.1048649772358,34.0893775735788,35.0738901699219,
36.058402766265,37.042915362608,38.0274279589511,39.0119405552942,39.9964531516372,
40.9809657479803,41.9654783443234,42.9499909406664,43.9345035370095,44.9190161333526,
45.9035287296956,46.8880413260387,47.8725539223818,48.8570665187248,49.8415791150679,
50.826091711411,51.810604307754,52.7951169040971,53.7796295004402,54.7641420967832,
55.7486546931263,56.7331672894694,57.7176798858124,58.7021924821555,59.6867050784986,
60.6712176748416,61.6557302711847),.UNSPECIFIED.);
#288=B_SPLINE_SURFACE_WITH_KNOTS('',3,3,((#42594,#42595,#42596,#42597,#42598,
#42599,#42600,#42601,#42602,#42603,#42604,#42605,#42606,#42607,#42608,#42609,
#42610,#42611,#42612,#42613,#42614,#42615,#42616,#42617,#42618,#42619,#42620,
#42621,#42622,#42623,#42624,#42625,#42626,#42627,#42628,#42629,#42630,#42631,
#42632,#42633,#42634,#42635,#42636,#42637,#42638,#42639,#42640,#42641,#42642,
#42643,#42644),(#42645,#42646,#42647,#42648,#42649,#42650,#42651,#42652,
#42653,#42654,#42655,#42656,#42657,#42658,#42659,#42660,#42661,#42662,#42663,
#42664,#42665,#42666,#42667,#42668,#42669,#42670,#42671,#42672,#42673,#42674,
#42675,#42676,#42677,#42678,#42679,#42680,#42681,#42682,#42683,#42684,#42685,
#42686,#42687,#42688,#42689,#42690,#42691,#42692,#42693,#42694,#42695),
(#42696,#42697,#42698,#42699,#42700,#42701,#42702,#42703,#42704,#42705,
#42706,#42707,#42708,#42709,#42710,#42711,#42712,#42713,#42714,#42715,#42716,
#42717,#42718,#42719,#42720,#42721,#42722,#42723,#42724,#42725,#42726,#42727,
#42728,#42729,#42730,#42731,#42732,#42733,#42734,#42735,#42736,#42737,#42738,
#42739,#42740,#42741,#42742,#42743,#42744,#42745,#42746),(#42747,#42748,
#42749,#42750,#42751,#42752,#42753,#42754,#42755,#42756,#42757,#42758,#42759,
#42760,#42761,#42762,#42763,#42764,#42765,#42766,#42767,#42768,#42769,#42770,
#42771,#42772,#42773,#42774,#42775,#42776,#42777,#42778,#42779,#42780,#42781,
#42782,#42783,#42784,#42785,#42786,#42787,#42788,#42789,#42790,#42791,#42792,
#42793,#42794,#42795,#42796,#42797)),.UNSPECIFIED.,.F.,.F.,.F.,(4,4),(4,
1,1,1,1,1,1,1,1,1,1,1,1,1,1,1,1,1,1,1,1,1,1,1,1,1,1,1,1,1,1,1,1,1,1,1,1,
1,1,1,1,1,1,1,1,1,1,1,4),(0.,0.0802805549308171),(11.8575378228164,12.8420504191595,
13.8265630155026,14.8110756118456,15.7955882081887,16.7801008045318,17.7646134008748,
18.7491259972179,19.733638593561,20.718151189904,21.7026637862471,22.6871763825901,
23.6716889789332,24.6562015752763,25.6407141716193,26.6252267679624,27.6097393643055,
28.5942519606485,29.5787645569916,30.5632771533347,31.5477897496777,32.5323023460208,
33.5168149423639,34.5013275387069,35.48584013505,36.4703527313931,37.4548653277361,
38.4393779240792,39.4238905204223,40.4084031167653,41.3929157131084,42.3774283094515,
43.3619409057945,44.3464535021376,45.3309660984807,46.3154786948237,47.2999912911668,
48.2845038875099,49.2690164838529,50.253529080196,51.2380416765391,52.2225542728821,
53.2070668692252,54.1915794655683,55.1760920619113,56.1606046582544,57.1451172545975,
58.1296298509405,59.1141424472836),.UNSPECIFIED.);
#289=B_SPLINE_SURFACE_WITH_KNOTS('',3,3,((#42917,#42918,#42919,#42920,#42921,
#42922,#42923,#42924,#42925,#42926,#42927,#42928,#42929,#42930,#42931,#42932,
#42933,#42934,#42935,#42936,#42937,#42938,#42939,#42940,#42941,#42942,#42943,
#42944,#42945,#42946,#42947,#42948,#42949,#42950,#42951,#42952,#42953,#42954,
#42955,#42956,#42957,#42958,#42959,#42960,#42961,#42962,#42963,#42964,#42965,
#42966,#42967),(#42968,#42969,#42970,#42971,#42972,#42973,#42974,#42975,
#42976,#42977,#42978,#42979,#42980,#42981,#42982,#42983,#42984,#42985,#42986,
#42987,#42988,#42989,#42990,#42991,#42992,#42993,#42994,#42995,#42996,#42997,
#42998,#42999,#43000,#43001,#43002,#43003,#43004,#43005,#43006,#43007,#43008,
#43009,#43010,#43011,#43012,#43013,#43014,#43015,#43016,#43017,#43018),
(#43019,#43020,#43021,#43022,#43023,#43024,#43025,#43026,#43027,#43028,
#43029,#43030,#43031,#43032,#43033,#43034,#43035,#43036,#43037,#43038,#43039,
#43040,#43041,#43042,#43043,#43044,#43045,#43046,#43047,#43048,#43049,#43050,
#43051,#43052,#43053,#43054,#43055,#43056,#43057,#43058,#43059,#43060,#43061,
#43062,#43063,#43064,#43065,#43066,#43067,#43068,#43069),(#43070,#43071,
#43072,#43073,#43074,#43075,#43076,#43077,#43078,#43079,#43080,#43081,#43082,
#43083,#43084,#43085,#43086,#43087,#43088,#43089,#43090,#43091,#43092,#43093,
#43094,#43095,#43096,#43097,#43098,#43099,#43100,#43101,#43102,#43103,#43104,
#43105,#43106,#43107,#43108,#43109,#43110,#43111,#43112,#43113,#43114,#43115,
#43116,#43117,#43118,#43119,#43120)),.UNSPECIFIED.,.F.,.F.,.F.,(4,4),(4,
1,1,1,1,1,1,1,1,1,1,1,1,1,1,1,1,1,1,1,1,1,1,1,1,1,1,1,1,1,1,1,1,1,1,1,1,
1,1,1,1,1,1,1,1,1,1,1,4),(0.,0.0802805549308171),(14.3991256467175,15.3836382430606,
16.3681508394037,17.3526634357467,18.3371760320898,19.3216886284329,20.3062012247759,
21.290713821119,22.2752264174621,23.2597390138051,24.2442516101482,25.2287642064913,
26.2132768028343,27.1977893991774,28.1823019955205,29.1668145918635,30.1513271882066,
31.1358397845497,32.1203523808927,33.1048649772358,34.0893775735789,35.0738901699219,
36.058402766265,37.0429153626081,38.0274279589511,39.0119405552942,39.9964531516373,
40.9809657479803,41.9654783443234,42.9499909406665,43.9345035370095,44.9190161333526,
45.9035287296957,46.8880413260387,47.8725539223818,48.8570665187248,49.8415791150679,
50.826091711411,51.810604307754,52.7951169040971,53.7796295004402,54.7641420967832,
55.7486546931263,56.7331672894694,57.7176798858124,58.7021924821555,59.6867050784986,
60.6712176748416,61.6557302711847),.UNSPECIFIED.);
#290=B_SPLINE_SURFACE_WITH_KNOTS('',3,3,((#46765,#46766,#46767,#46768,#46769,
#46770,#46771,#46772,#46773,#46774,#46775,#46776,#46777,#46778,#46779,#46780,
#46781,#46782,#46783,#46784,#46785,#46786,#46787,#46788,#46789,#46790,#46791,
#46792,#46793,#46794,#46795,#46796,#46797,#46798,#46799,#46800,#46801,#46802,
#46803,#46804,#46805,#46806,#46807,#46808,#46809,#46810,#46811,#46812,#46813,
#46814,#46815,#46816,#46817,#46818,#46819,#46820,#46821,#46822,#46823,#46824,
#46825,#46826,#46827,#46828,#46829,#46830,#46831,#46832,#46833,#46834,#46835,
#46836,#46837,#46838,#46839,#46840,#46841,#46842,#46843,#46844,#46845,#46846,
#46847,#46848,#46849,#46850,#46851,#46852,#46853,#46854,#46855,#46856,#46857,
#46858,#46859,#46860,#46861,#46862,#46863,#46864,#46865,#46866,#46867,#46868,
#46869,#46870,#46871,#46872,#46873,#46874,#46875,#46876,#46877,#46878,#46879,
#46880,#46881,#46882,#46883,#46884,#46885,#46886,#46887,#46888,#46889,#46890,
#46891,#46892,#46893,#46894,#46895,#46896,#46897,#46898,#46899,#46900,#46901,
#46902,#46903,#46904,#46905,#46906,#46907,#46908,#46909,#46910,#46911,#46912,
#46913,#46914,#46915,#46916,#46917,#46918,#46919,#46920,#46921,#46922,#46923,
#46924,#46925,#46926,#46927,#46928,#46929,#46930,#46931,#46932,#46933,#46934,
#46935,#46936,#46937,#46938,#46939,#46940,#46941,#46942,#46943,#46944,#46945,
#46946,#46947,#46948,#46949,#46950,#46951,#46952,#46953,#46954,#46955,#46956,
#46957,#46958,#46959,#46960,#46961,#46962,#46963,#46964,#46965,#46966,#46967,
#46968,#46969,#46970,#46971,#46972,#46973,#46974,#46975,#46976,#46977,#46978,
#46979,#46980,#46981,#46982,#46983,#46984,#46985,#46986,#46987,#46988,#46989,
#46990,#46991,#46992,#46993,#46994,#46995,#46996,#46997,#46998,#46999,#47000,
#47001,#47002,#47003,#47004,#47005,#47006,#47007,#47008,#47009,#47010,#47011,
#47012,#47013,#47014,#47015,#47016,#47017,#47018,#47019,#47020,#47021,#47022,
#47023,#47024,#47025,#47026,#47027,#47028,#47029,#47030,#47031,#47032,#47033,
#47034,#47035,#47036,#47037,#47038,#47039,#47040,#47041,#47042,#47043,#47044,
#47045,#47046,#47047,#47048,#47049,#47050,#47051,#47052,#47053,#47054,#47055,
#47056,#47057,#47058,#47059,#47060,#47061,#47062,#47063,#47064,#47065,#47066,
#47067,#47068,#47069,#47070,#47071,#47072,#47073,#47074,#47075,#47076,#47077,
#47078,#47079,#47080,#47081,#47082,#47083,#47084,#47085,#47086,#47087,#47088,
#47089,#47090,#47091,#47092,#47093,#47094,#47095,#47096,#47097,#47098,#47099,
#47100,#47101,#47102,#47103,#47104,#47105,#47106,#47107,#47108,#47109,#47110,
#47111,#47112,#47113,#47114,#47115,#47116,#47117,#47118,#47119,#47120,#47121,
#47122,#47123,#47124,#47125,#47126,#47127,#47128,#47129,#47130,#47131),
(#47132,#47133,#47134,#47135,#47136,#47137,#47138,#47139,#47140,#47141,
#47142,#47143,#47144,#47145,#47146,#47147,#47148,#47149,#47150,#47151,#47152,
#47153,#47154,#47155,#47156,#47157,#47158,#47159,#47160,#47161,#47162,#47163,
#47164,#47165,#47166,#47167,#47168,#47169,#47170,#47171,#47172,#47173,#47174,
#47175,#47176,#47177,#47178,#47179,#47180,#47181,#47182,#47183,#47184,#47185,
#47186,#47187,#47188,#47189,#47190,#47191,#47192,#47193,#47194,#47195,#47196,
#47197,#47198,#47199,#47200,#47201,#47202,#47203,#47204,#47205,#47206,#47207,
#47208,#47209,#47210,#47211,#47212,#47213,#47214,#47215,#47216,#47217,#47218,
#47219,#47220,#47221,#47222,#47223,#47224,#47225,#47226,#47227,#47228,#47229,
#47230,#47231,#47232,#47233,#47234,#47235,#47236,#47237,#47238,#47239,#47240,
#47241,#47242,#47243,#47244,#47245,#47246,#47247,#47248,#47249,#47250,#47251,
#47252,#47253,#47254,#47255,#47256,#47257,#47258,#47259,#47260,#47261,#47262,
#47263,#47264,#47265,#47266,#47267,#47268,#47269,#47270,#47271,#47272,#47273,
#47274,#47275,#47276,#47277,#47278,#47279,#47280,#47281,#47282,#47283,#47284,
#47285,#47286,#47287,#47288,#47289,#47290,#47291,#47292,#47293,#47294,#47295,
#47296,#47297,#47298,#47299,#47300,#47301,#47302,#47303,#47304,#47305,#47306,
#47307,#47308,#47309,#47310,#47311,#47312,#47313,#47314,#47315,#47316,#47317,
#47318,#47319,#47320,#47321,#47322,#47323,#47324,#47325,#47326,#47327,#47328,
#47329,#47330,#47331,#47332,#47333,#47334,#47335,#47336,#47337,#47338,#47339,
#47340,#47341,#47342,#47343,#47344,#47345,#47346,#47347,#47348,#47349,#47350,
#47351,#47352,#47353,#47354,#47355,#47356,#47357,#47358,#47359,#47360,#47361,
#47362,#47363,#47364,#47365,#47366,#47367,#47368,#47369,#47370,#47371,#47372,
#47373,#47374,#47375,#47376,#47377,#47378,#47379,#47380,#47381,#47382,#47383,
#47384,#47385,#47386,#47387,#47388,#47389,#47390,#47391,#47392,#47393,#47394,
#47395,#47396,#47397,#47398,#47399,#47400,#47401,#47402,#47403,#47404,#47405,
#47406,#47407,#47408,#47409,#47410,#47411,#47412,#47413,#47414,#47415,#47416,
#47417,#47418,#47419,#47420,#47421,#47422,#47423,#47424,#47425,#47426,#47427,
#47428,#47429,#47430,#47431,#47432,#47433,#47434,#47435,#47436,#47437,#47438,
#47439,#47440,#47441,#47442,#47443,#47444,#47445,#47446,#47447,#47448,#47449,
#47450,#47451,#47452,#47453,#47454,#47455,#47456,#47457,#47458,#47459,#47460,
#47461,#47462,#47463,#47464,#47465,#47466,#47467,#47468,#47469,#47470,#47471,
#47472,#47473,#47474,#47475,#47476,#47477,#47478,#47479,#47480,#47481,#47482,
#47483,#47484,#47485,#47486,#47487,#47488,#47489,#47490,#47491,#47492,#47493,
#47494,#47495,#47496,#47497,#47498),(#47499,#47500,#47501,#47502,#47503,
#47504,#47505,#47506,#47507,#47508,#47509,#47510,#47511,#47512,#47513,#47514,
#47515,#47516,#47517,#47518,#47519,#47520,#47521,#47522,#47523,#47524,#47525,
#47526,#47527,#47528,#47529,#47530,#47531,#47532,#47533,#47534,#47535,#47536,
#47537,#47538,#47539,#47540,#47541,#47542,#47543,#47544,#47545,#47546,#47547,
#47548,#47549,#47550,#47551,#47552,#47553,#47554,#47555,#47556,#47557,#47558,
#47559,#47560,#47561,#47562,#47563,#47564,#47565,#47566,#47567,#47568,#47569,
#47570,#47571,#47572,#47573,#47574,#47575,#47576,#47577,#47578,#47579,#47580,
#47581,#47582,#47583,#47584,#47585,#47586,#47587,#47588,#47589,#47590,#47591,
#47592,#47593,#47594,#47595,#47596,#47597,#47598,#47599,#47600,#47601,#47602,
#47603,#47604,#47605,#47606,#47607,#47608,#47609,#47610,#47611,#47612,#47613,
#47614,#47615,#47616,#47617,#47618,#47619,#47620,#47621,#47622,#47623,#47624,
#47625,#47626,#47627,#47628,#47629,#47630,#47631,#47632,#47633,#47634,#47635,
#47636,#47637,#47638,#47639,#47640,#47641,#47642,#47643,#47644,#47645,#47646,
#47647,#47648,#47649,#47650,#47651,#47652,#47653,#47654,#47655,#47656,#47657,
#47658,#47659,#47660,#47661,#47662,#47663,#47664,#47665,#47666,#47667,#47668,
#47669,#47670,#47671,#47672,#47673,#47674,#47675,#47676,#47677,#47678,#47679,
#47680,#47681,#47682,#47683,#47684,#47685,#47686,#47687,#47688,#47689,#47690,
#47691,#47692,#47693,#47694,#47695,#47696,#47697,#47698,#47699,#47700,#47701,
#47702,#47703,#47704,#47705,#47706,#47707,#47708,#47709,#47710,#47711,#47712,
#47713,#47714,#47715,#47716,#47717,#47718,#47719,#47720,#47721,#47722,#47723,
#47724,#47725,#47726,#47727,#47728,#47729,#47730,#47731,#47732,#47733,#47734,
#47735,#47736,#47737,#47738,#47739,#47740,#47741,#47742,#47743,#47744,#47745,
#47746,#47747,#47748,#47749,#47750,#47751,#47752,#47753,#47754,#47755,#47756,
#47757,#47758,#47759,#47760,#47761,#47762,#47763,#47764,#47765,#47766,#47767,
#47768,#47769,#47770,#47771,#47772,#47773,#47774,#47775,#47776,#47777,#47778,
#47779,#47780,#47781,#47782,#47783,#47784,#47785,#47786,#47787,#47788,#47789,
#47790,#47791,#47792,#47793,#47794,#47795,#47796,#47797,#47798,#47799,#47800,
#47801,#47802,#47803,#47804,#47805,#47806,#47807,#47808,#47809,#47810,#47811,
#47812,#47813,#47814,#47815,#47816,#47817,#47818,#47819,#47820,#47821,#47822,
#47823,#47824,#47825,#47826,#47827,#47828,#47829,#47830,#47831,#47832,#47833,
#47834,#47835,#47836,#47837,#47838,#47839,#47840,#47841,#47842,#47843,#47844,
#47845,#47846,#47847,#47848,#47849,#47850,#47851,#47852,#47853,#47854,#47855,
#47856,#47857,#47858,#47859,#47860,#47861,#47862,#47863,#47864,#47865),
(#47866,#47867,#47868,#47869,#47870,#47871,#47872,#47873,#47874,#47875,
#47876,#47877,#47878,#47879,#47880,#47881,#47882,#47883,#47884,#47885,#47886,
#47887,#47888,#47889,#47890,#47891,#47892,#47893,#47894,#47895,#47896,#47897,
#47898,#47899,#47900,#47901,#47902,#47903,#47904,#47905,#47906,#47907,#47908,
#47909,#47910,#47911,#47912,#47913,#47914,#47915,#47916,#47917,#47918,#47919,
#47920,#47921,#47922,#47923,#47924,#47925,#47926,#47927,#47928,#47929,#47930,
#47931,#47932,#47933,#47934,#47935,#47936,#47937,#47938,#47939,#47940,#47941,
#47942,#47943,#47944,#47945,#47946,#47947,#47948,#47949,#47950,#47951,#47952,
#47953,#47954,#47955,#47956,#47957,#47958,#47959,#47960,#47961,#47962,#47963,
#47964,#47965,#47966,#47967,#47968,#47969,#47970,#47971,#47972,#47973,#47974,
#47975,#47976,#47977,#47978,#47979,#47980,#47981,#47982,#47983,#47984,#47985,
#47986,#47987,#47988,#47989,#47990,#47991,#47992,#47993,#47994,#47995,#47996,
#47997,#47998,#47999,#48000,#48001,#48002,#48003,#48004,#48005,#48006,#48007,
#48008,#48009,#48010,#48011,#48012,#48013,#48014,#48015,#48016,#48017,#48018,
#48019,#48020,#48021,#48022,#48023,#48024,#48025,#48026,#48027,#48028,#48029,
#48030,#48031,#48032,#48033,#48034,#48035,#48036,#48037,#48038,#48039,#48040,
#48041,#48042,#48043,#48044,#48045,#48046,#48047,#48048,#48049,#48050,#48051,
#48052,#48053,#48054,#48055,#48056,#48057,#48058,#48059,#48060,#48061,#48062,
#48063,#48064,#48065,#48066,#48067,#48068,#48069,#48070,#48071,#48072,#48073,
#48074,#48075,#48076,#48077,#48078,#48079,#48080,#48081,#48082,#48083,#48084,
#48085,#48086,#48087,#48088,#48089,#48090,#48091,#48092,#48093,#48094,#48095,
#48096,#48097,#48098,#48099,#48100,#48101,#48102,#48103,#48104,#48105,#48106,
#48107,#48108,#48109,#48110,#48111,#48112,#48113,#48114,#48115,#48116,#48117,
#48118,#48119,#48120,#48121,#48122,#48123,#48124,#48125,#48126,#48127,#48128,
#48129,#48130,#48131,#48132,#48133,#48134,#48135,#48136,#48137,#48138,#48139,
#48140,#48141,#48142,#48143,#48144,#48145,#48146,#48147,#48148,#48149,#48150,
#48151,#48152,#48153,#48154,#48155,#48156,#48157,#48158,#48159,#48160,#48161,
#48162,#48163,#48164,#48165,#48166,#48167,#48168,#48169,#48170,#48171,#48172,
#48173,#48174,#48175,#48176,#48177,#48178,#48179,#48180,#48181,#48182,#48183,
#48184,#48185,#48186,#48187,#48188,#48189,#48190,#48191,#48192,#48193,#48194,
#48195,#48196,#48197,#48198,#48199,#48200,#48201,#48202,#48203,#48204,#48205,
#48206,#48207,#48208,#48209,#48210,#48211,#48212,#48213,#48214,#48215,#48216,
#48217,#48218,#48219,#48220,#48221,#48222,#48223,#48224,#48225,#48226,#48227,
#48228,#48229,#48230,#48231,#48232)),.UNSPECIFIED.,.F.,.F.,.F.,(4,4),(4,
1,1,1,1,1,1,1,1,1,1,1,1,1,1,1,1,1,1,1,1,1,1,1,1,1,1,1,1,1,1,1,1,1,1,1,1,
1,1,1,1,1,1,1,1,1,1,1,1,1,1,1,1,1,1,1,1,1,1,1,1,1,1,1,1,1,1,1,1,1,1,1,1,
1,1,1,1,1,1,1,1,1,1,1,1,1,1,1,1,1,1,1,1,1,1,1,1,1,1,1,1,1,1,1,1,1,1,1,1,
1,1,1,1,1,1,1,1,1,1,1,1,1,1,1,1,1,1,1,1,1,1,1,1,1,1,1,1,1,1,1,1,1,1,1,1,
1,1,1,1,1,1,1,1,1,1,1,1,1,1,1,1,1,1,1,1,1,1,1,1,1,1,1,1,1,1,1,1,1,1,1,1,
1,1,1,1,1,1,1,1,1,1,1,1,1,1,1,1,1,1,1,1,1,1,1,1,1,1,1,1,1,1,1,1,1,1,1,1,
1,1,1,1,1,1,1,1,1,1,1,1,1,1,1,1,1,1,1,1,1,1,1,1,1,1,1,1,1,1,1,1,1,1,1,1,
1,1,1,1,1,1,1,1,1,1,1,1,1,1,1,1,1,1,1,1,1,1,1,1,1,1,1,1,1,1,1,1,1,1,1,1,
1,1,1,1,1,1,1,1,1,1,1,1,1,1,1,1,1,1,1,1,1,1,1,1,1,1,1,1,1,1,1,1,1,1,1,1,
1,1,1,1,1,1,1,1,1,1,1,1,1,1,1,1,1,1,1,1,1,1,1,1,1,1,1,1,1,1,1,1,1,1,1,1,
1,1,1,4),(0.,0.112756507572734),(11.8517336648509,12.3504803140147,12.8492269631785,
13.3479736123423,13.8467202615061,14.3454669106698,14.8442135598336,15.3429602089974,
15.8417068581612,16.340453507325,16.8392001564888,17.3379468056525,17.8366934548163,
18.3354401039801,18.8341867531439,19.3329334023077,19.8316800514714,20.3304267006352,
20.829173349799,21.3279199989628,21.8266666481266,22.3254132972903,22.8241599464541,
23.3229065956179,23.8216532447817,24.3203998939455,24.8191465431093,25.317893192273,
25.8166398414368,26.3153864906006,26.8141331397644,27.3128797889282,27.8116264380919,
28.3103730872557,28.8091197364195,29.3078663855833,29.8066130347471,30.3053596839108,
30.8041063330746,31.3028529822384,31.8015996314022,32.300346280566,32.7990929297298,
33.2978395788935,33.7965862280573,34.2953328772211,34.7940795263849,35.2928261755487,
35.7915728247124,36.2903194738762,36.78906612304,37.2878127722038,37.7865594213676,
38.2853060705313,38.7840527196951,39.2827993688589,39.7815460180227,40.2802926671865,
40.7790393163503,41.277785965514,41.7765326146778,42.2752792638416,42.7740259130054,
43.2727725621692,43.7715192113329,44.2702658604967,44.7690125096605,45.2677591588243,
45.7665058079881,46.2652524571519,46.7639991063156,47.2627457554794,47.7614924046432,
48.260239053807,48.7589857029708,49.2577323521345,49.7564790012983,50.2552256504621,
50.7539722996259,51.2527189487897,51.7514655979534,52.2502122471172,52.748958896281,
53.2477055454448,53.7464521946086,54.2451988437724,54.7439454929361,55.2426921420999,
55.7414387912637,56.2401854404275,56.7389320895913,57.237678738755,57.7364253879188,
58.2351720370826,58.7339186862464,59.2326653354102,59.731411984574,60.2301586337377,
60.7289052829015,61.2276519320653,61.7263985812291,62.2251452303929,62.7238918795566,
63.2226385287204,63.7213851778842,64.220131827048,64.7188784762118,65.2176251253755,
65.7163717745393,66.2151184237031,66.7138650728669,67.2126117220307,67.7113583711945,
68.2101050203582,68.708851669522,69.2075983186858,69.7063449678496,70.2050916170134,
70.7038382661771,71.2025849153409,71.7013315645047,72.2000782136685,72.6988248628323,
73.197571511996,73.6963181611598,74.1950648103236,74.6938114594874,75.1925581086512,
75.6913047578149,76.1900514069787,76.6887980561425,77.1875447053063,77.6862913544701,
78.1850380036339,78.6837846527976,79.1825313019614,79.6812779511252,80.180024600289,
80.6787712494528,81.1775178986165,81.6762645477803,82.1750111969441,82.6737578461079,
83.1725044952717,83.6712511444355,84.1699977935992,84.668744442763,85.1674910919268,
85.6662377410906,86.1649843902544,86.6637310394181,87.1624776885819,87.6612243377457,
88.1599709869095,88.6587176360733,89.1574642852371,89.6562109344008,90.1549575835646,
90.6537042327284,91.1524508818922,91.651197531056,92.1499441802197,92.6486908293835,
93.1474374785473,93.6461841277111,94.1449307768749,94.6436774260386,95.1424240752024,
95.6411707243662,96.13991737353,96.6386640226938,97.1374106718576,97.6361573210213,
98.1349039701851,98.6336506193489,99.1323972685127,99.6311439176765,100.12989056684,
100.628637216004,101.127383865168,101.626130514332,102.124877163495,102.623623812659,
103.122370461823,103.621117110987,104.11986376015,104.618610409314,105.117357058478,
105.616103707642,106.114850356806,106.613597005969,107.112343655133,107.611090304297,
108.109836953461,108.608583602625,109.107330251788,109.606076900952,110.104823550116,
110.60357019928,111.102316848443,111.601063497607,112.099810146771,112.598556795935,
113.097303445099,113.596050094262,114.094796743426,114.59354339259,115.092290041754,
115.591036690917,116.089783340081,116.588529989245,117.087276638409,117.586023287573,
118.084769936736,118.5835165859,119.082263235064,119.581009884228,120.079756533392,
120.578503182555,121.077249831719,121.575996480883,122.074743130047,122.57348977921,
123.072236428374,123.570983077538,124.069729726702,124.568476375866,125.067223025029,
125.565969674193,126.064716323357,126.563462972521,127.062209621684,127.560956270848,
128.059702920012,128.558449569176,129.05719621834,129.555942867503,130.054689516667,
130.553436165831,131.052182814995,131.550929464158,132.049676113322,132.548422762486,
133.04716941165,133.545916060814,134.044662709977,134.543409359141,135.042156008305,
135.540902657469,136.039649306632,136.538395955796,137.03714260496,137.535889254124,
138.034635903288,138.533382552451,139.032129201615,139.530875850779,140.029622499943,
140.528369149107,141.02711579827,141.525862447434,142.024609096598,142.523355745762,
143.022102394925,143.520849044089,144.019595693253,144.518342342417,145.017088991581,
145.515835640744,146.014582289908,146.513328939072,147.012075588236,147.510822237399,
148.009568886563,148.508315535727,149.007062184891,149.505808834055,150.004555483218,
150.503302132382,151.002048781546,151.50079543071,151.999542079873,152.498288729037,
152.997035378201,153.495782027365,153.994528676529,154.493275325692,154.992021974856,
155.49076862402,155.989515273184,156.488261922348,156.987008571511,157.485755220675,
157.984501869839,158.483248519003,158.981995168166,159.48074181733,159.979488466494,
160.478235115658,160.976981764822,161.475728413985,161.974475063149,162.473221712313,
162.971968361477,163.47071501064,163.969461659804,164.468208308968,164.966954958132,
165.465701607296,165.964448256459,166.463194905623,166.961941554787,167.460688203951,
167.959434853114,168.458181502278,168.956928151442,169.455674800606,169.95442144977,
170.453168098933,170.951914748097,171.450661397261,171.949408046425,172.448154695589,
172.946901344752,173.445647993916,173.94439464308,174.443141292244,174.941887941407,
175.440634590571,175.939381239735,176.438127888899,176.936874538063,177.435621187226,
177.93436783639,178.433114485554,178.931861134718,179.430607783881,179.929354433045,
180.428101082209,180.926847731373,181.425594380537,181.9243410297,182.423087678864,
182.921834328028,183.420580977192,183.919327626356,184.418074275519,184.916820924683,
185.415567573847,185.914314223011,186.413060872174,186.911807521338,187.410554170502,
187.909300819666,188.40804746883,188.906794117993,189.405540767157,189.904287416321,
190.403034065485,190.901780714648,191.400527363812,191.899274012976,192.39802066214,
192.896767311304,193.395513960467),.UNSPECIFIED.);
#291=B_SPLINE_SURFACE_WITH_KNOTS('',3,3,((#48500,#48501,#48502,#48503,#48504,
#48505,#48506,#48507,#48508,#48509,#48510,#48511,#48512,#48513,#48514,#48515,
#48516,#48517,#48518,#48519,#48520,#48521,#48522,#48523,#48524,#48525,#48526,
#48527,#48528,#48529,#48530,#48531,#48532,#48533,#48534,#48535,#48536,#48537,
#48538,#48539,#48540,#48541,#48542,#48543,#48544,#48545,#48546,#48547,#48548,
#48549,#48550,#48551,#48552,#48553,#48554,#48555,#48556,#48557,#48558,#48559,
#48560,#48561,#48562,#48563,#48564,#48565,#48566,#48567,#48568,#48569,#48570,
#48571,#48572,#48573,#48574,#48575,#48576,#48577,#48578,#48579,#48580,#48581,
#48582,#48583,#48584,#48585,#48586,#48587,#48588,#48589,#48590,#48591,#48592,
#48593,#48594,#48595,#48596,#48597,#48598,#48599,#48600,#48601,#48602,#48603,
#48604,#48605,#48606,#48607,#48608,#48609,#48610,#48611,#48612,#48613,#48614,
#48615,#48616,#48617,#48618,#48619,#48620,#48621,#48622,#48623,#48624,#48625,
#48626,#48627,#48628,#48629,#48630,#48631,#48632,#48633,#48634,#48635,#48636,
#48637,#48638,#48639,#48640,#48641,#48642,#48643,#48644,#48645,#48646,#48647,
#48648,#48649,#48650,#48651,#48652,#48653,#48654,#48655,#48656,#48657,#48658,
#48659,#48660,#48661,#48662,#48663,#48664,#48665,#48666,#48667,#48668,#48669,
#48670,#48671,#48672,#48673,#48674,#48675,#48676,#48677,#48678,#48679,#48680,
#48681,#48682,#48683,#48684,#48685,#48686,#48687,#48688,#48689,#48690,#48691,
#48692,#48693,#48694,#48695,#48696,#48697,#48698,#48699,#48700,#48701,#48702,
#48703,#48704,#48705,#48706,#48707,#48708,#48709,#48710,#48711,#48712,#48713,
#48714,#48715,#48716,#48717,#48718,#48719,#48720,#48721,#48722,#48723,#48724,
#48725,#48726,#48727,#48728,#48729,#48730,#48731,#48732,#48733,#48734,#48735,
#48736,#48737,#48738,#48739,#48740,#48741,#48742,#48743,#48744,#48745,#48746,
#48747,#48748,#48749,#48750,#48751,#48752,#48753,#48754,#48755,#48756,#48757,
#48758,#48759,#48760,#48761,#48762,#48763,#48764,#48765,#48766,#48767,#48768,
#48769,#48770,#48771,#48772,#48773,#48774,#48775,#48776,#48777,#48778,#48779,
#48780,#48781,#48782,#48783,#48784,#48785,#48786,#48787,#48788,#48789,#48790,
#48791,#48792,#48793,#48794,#48795,#48796,#48797,#48798,#48799,#48800,#48801,
#48802,#48803,#48804,#48805,#48806,#48807,#48808,#48809,#48810,#48811,#48812,
#48813,#48814,#48815,#48816,#48817,#48818,#48819,#48820,#48821,#48822,#48823,
#48824,#48825,#48826,#48827,#48828,#48829,#48830,#48831,#48832,#48833,#48834,
#48835,#48836,#48837,#48838,#48839,#48840,#48841,#48842,#48843,#48844,#48845,
#48846,#48847,#48848,#48849,#48850,#48851,#48852,#48853,#48854,#48855,#48856,
#48857,#48858,#48859,#48860,#48861,#48862,#48863,#48864,#48865,#48866),
(#48867,#48868,#48869,#48870,#48871,#48872,#48873,#48874,#48875,#48876,
#48877,#48878,#48879,#48880,#48881,#48882,#48883,#48884,#48885,#48886,#48887,
#48888,#48889,#48890,#48891,#48892,#48893,#48894,#48895,#48896,#48897,#48898,
#48899,#48900,#48901,#48902,#48903,#48904,#48905,#48906,#48907,#48908,#48909,
#48910,#48911,#48912,#48913,#48914,#48915,#48916,#48917,#48918,#48919,#48920,
#48921,#48922,#48923,#48924,#48925,#48926,#48927,#48928,#48929,#48930,#48931,
#48932,#48933,#48934,#48935,#48936,#48937,#48938,#48939,#48940,#48941,#48942,
#48943,#48944,#48945,#48946,#48947,#48948,#48949,#48950,#48951,#48952,#48953,
#48954,#48955,#48956,#48957,#48958,#48959,#48960,#48961,#48962,#48963,#48964,
#48965,#48966,#48967,#48968,#48969,#48970,#48971,#48972,#48973,#48974,#48975,
#48976,#48977,#48978,#48979,#48980,#48981,#48982,#48983,#48984,#48985,#48986,
#48987,#48988,#48989,#48990,#48991,#48992,#48993,#48994,#48995,#48996,#48997,
#48998,#48999,#49000,#49001,#49002,#49003,#49004,#49005,#49006,#49007,#49008,
#49009,#49010,#49011,#49012,#49013,#49014,#49015,#49016,#49017,#49018,#49019,
#49020,#49021,#49022,#49023,#49024,#49025,#49026,#49027,#49028,#49029,#49030,
#49031,#49032,#49033,#49034,#49035,#49036,#49037,#49038,#49039,#49040,#49041,
#49042,#49043,#49044,#49045,#49046,#49047,#49048,#49049,#49050,#49051,#49052,
#49053,#49054,#49055,#49056,#49057,#49058,#49059,#49060,#49061,#49062,#49063,
#49064,#49065,#49066,#49067,#49068,#49069,#49070,#49071,#49072,#49073,#49074,
#49075,#49076,#49077,#49078,#49079,#49080,#49081,#49082,#49083,#49084,#49085,
#49086,#49087,#49088,#49089,#49090,#49091,#49092,#49093,#49094,#49095,#49096,
#49097,#49098,#49099,#49100,#49101,#49102,#49103,#49104,#49105,#49106,#49107,
#49108,#49109,#49110,#49111,#49112,#49113,#49114,#49115,#49116,#49117,#49118,
#49119,#49120,#49121,#49122,#49123,#49124,#49125,#49126,#49127,#49128,#49129,
#49130,#49131,#49132,#49133,#49134,#49135,#49136,#49137,#49138,#49139,#49140,
#49141,#49142,#49143,#49144,#49145,#49146,#49147,#49148,#49149,#49150,#49151,
#49152,#49153,#49154,#49155,#49156,#49157,#49158,#49159,#49160,#49161,#49162,
#49163,#49164,#49165,#49166,#49167,#49168,#49169,#49170,#49171,#49172,#49173,
#49174,#49175,#49176,#49177,#49178,#49179,#49180,#49181,#49182,#49183,#49184,
#49185,#49186,#49187,#49188,#49189,#49190,#49191,#49192,#49193,#49194,#49195,
#49196,#49197,#49198,#49199,#49200,#49201,#49202,#49203,#49204,#49205,#49206,
#49207,#49208,#49209,#49210,#49211,#49212,#49213,#49214,#49215,#49216,#49217,
#49218,#49219,#49220,#49221,#49222,#49223,#49224,#49225,#49226,#49227,#49228,
#49229,#49230,#49231,#49232,#49233),(#49234,#49235,#49236,#49237,#49238,
#49239,#49240,#49241,#49242,#49243,#49244,#49245,#49246,#49247,#49248,#49249,
#49250,#49251,#49252,#49253,#49254,#49255,#49256,#49257,#49258,#49259,#49260,
#49261,#49262,#49263,#49264,#49265,#49266,#49267,#49268,#49269,#49270,#49271,
#49272,#49273,#49274,#49275,#49276,#49277,#49278,#49279,#49280,#49281,#49282,
#49283,#49284,#49285,#49286,#49287,#49288,#49289,#49290,#49291,#49292,#49293,
#49294,#49295,#49296,#49297,#49298,#49299,#49300,#49301,#49302,#49303,#49304,
#49305,#49306,#49307,#49308,#49309,#49310,#49311,#49312,#49313,#49314,#49315,
#49316,#49317,#49318,#49319,#49320,#49321,#49322,#49323,#49324,#49325,#49326,
#49327,#49328,#49329,#49330,#49331,#49332,#49333,#49334,#49335,#49336,#49337,
#49338,#49339,#49340,#49341,#49342,#49343,#49344,#49345,#49346,#49347,#49348,
#49349,#49350,#49351,#49352,#49353,#49354,#49355,#49356,#49357,#49358,#49359,
#49360,#49361,#49362,#49363,#49364,#49365,#49366,#49367,#49368,#49369,#49370,
#49371,#49372,#49373,#49374,#49375,#49376,#49377,#49378,#49379,#49380,#49381,
#49382,#49383,#49384,#49385,#49386,#49387,#49388,#49389,#49390,#49391,#49392,
#49393,#49394,#49395,#49396,#49397,#49398,#49399,#49400,#49401,#49402,#49403,
#49404,#49405,#49406,#49407,#49408,#49409,#49410,#49411,#49412,#49413,#49414,
#49415,#49416,#49417,#49418,#49419,#49420,#49421,#49422,#49423,#49424,#49425,
#49426,#49427,#49428,#49429,#49430,#49431,#49432,#49433,#49434,#49435,#49436,
#49437,#49438,#49439,#49440,#49441,#49442,#49443,#49444,#49445,#49446,#49447,
#49448,#49449,#49450,#49451,#49452,#49453,#49454,#49455,#49456,#49457,#49458,
#49459,#49460,#49461,#49462,#49463,#49464,#49465,#49466,#49467,#49468,#49469,
#49470,#49471,#49472,#49473,#49474,#49475,#49476,#49477,#49478,#49479,#49480,
#49481,#49482,#49483,#49484,#49485,#49486,#49487,#49488,#49489,#49490,#49491,
#49492,#49493,#49494,#49495,#49496,#49497,#49498,#49499,#49500,#49501,#49502,
#49503,#49504,#49505,#49506,#49507,#49508,#49509,#49510,#49511,#49512,#49513,
#49514,#49515,#49516,#49517,#49518,#49519,#49520,#49521,#49522,#49523,#49524,
#49525,#49526,#49527,#49528,#49529,#49530,#49531,#49532,#49533,#49534,#49535,
#49536,#49537,#49538,#49539,#49540,#49541,#49542,#49543,#49544,#49545,#49546,
#49547,#49548,#49549,#49550,#49551,#49552,#49553,#49554,#49555,#49556,#49557,
#49558,#49559,#49560,#49561,#49562,#49563,#49564,#49565,#49566,#49567,#49568,
#49569,#49570,#49571,#49572,#49573,#49574,#49575,#49576,#49577,#49578,#49579,
#49580,#49581,#49582,#49583,#49584,#49585,#49586,#49587,#49588,#49589,#49590,
#49591,#49592,#49593,#49594,#49595,#49596,#49597,#49598,#49599,#49600),
(#49601,#49602,#49603,#49604,#49605,#49606,#49607,#49608,#49609,#49610,
#49611,#49612,#49613,#49614,#49615,#49616,#49617,#49618,#49619,#49620,#49621,
#49622,#49623,#49624,#49625,#49626,#49627,#49628,#49629,#49630,#49631,#49632,
#49633,#49634,#49635,#49636,#49637,#49638,#49639,#49640,#49641,#49642,#49643,
#49644,#49645,#49646,#49647,#49648,#49649,#49650,#49651,#49652,#49653,#49654,
#49655,#49656,#49657,#49658,#49659,#49660,#49661,#49662,#49663,#49664,#49665,
#49666,#49667,#49668,#49669,#49670,#49671,#49672,#49673,#49674,#49675,#49676,
#49677,#49678,#49679,#49680,#49681,#49682,#49683,#49684,#49685,#49686,#49687,
#49688,#49689,#49690,#49691,#49692,#49693,#49694,#49695,#49696,#49697,#49698,
#49699,#49700,#49701,#49702,#49703,#49704,#49705,#49706,#49707,#49708,#49709,
#49710,#49711,#49712,#49713,#49714,#49715,#49716,#49717,#49718,#49719,#49720,
#49721,#49722,#49723,#49724,#49725,#49726,#49727,#49728,#49729,#49730,#49731,
#49732,#49733,#49734,#49735,#49736,#49737,#49738,#49739,#49740,#49741,#49742,
#49743,#49744,#49745,#49746,#49747,#49748,#49749,#49750,#49751,#49752,#49753,
#49754,#49755,#49756,#49757,#49758,#49759,#49760,#49761,#49762,#49763,#49764,
#49765,#49766,#49767,#49768,#49769,#49770,#49771,#49772,#49773,#49774,#49775,
#49776,#49777,#49778,#49779,#49780,#49781,#49782,#49783,#49784,#49785,#49786,
#49787,#49788,#49789,#49790,#49791,#49792,#49793,#49794,#49795,#49796,#49797,
#49798,#49799,#49800,#49801,#49802,#49803,#49804,#49805,#49806,#49807,#49808,
#49809,#49810,#49811,#49812,#49813,#49814,#49815,#49816,#49817,#49818,#49819,
#49820,#49821,#49822,#49823,#49824,#49825,#49826,#49827,#49828,#49829,#49830,
#49831,#49832,#49833,#49834,#49835,#49836,#49837,#49838,#49839,#49840,#49841,
#49842,#49843,#49844,#49845,#49846,#49847,#49848,#49849,#49850,#49851,#49852,
#49853,#49854,#49855,#49856,#49857,#49858,#49859,#49860,#49861,#49862,#49863,
#49864,#49865,#49866,#49867,#49868,#49869,#49870,#49871,#49872,#49873,#49874,
#49875,#49876,#49877,#49878,#49879,#49880,#49881,#49882,#49883,#49884,#49885,
#49886,#49887,#49888,#49889,#49890,#49891,#49892,#49893,#49894,#49895,#49896,
#49897,#49898,#49899,#49900,#49901,#49902,#49903,#49904,#49905,#49906,#49907,
#49908,#49909,#49910,#49911,#49912,#49913,#49914,#49915,#49916,#49917,#49918,
#49919,#49920,#49921,#49922,#49923,#49924,#49925,#49926,#49927,#49928,#49929,
#49930,#49931,#49932,#49933,#49934,#49935,#49936,#49937,#49938,#49939,#49940,
#49941,#49942,#49943,#49944,#49945,#49946,#49947,#49948,#49949,#49950,#49951,
#49952,#49953,#49954,#49955,#49956,#49957,#49958,#49959,#49960,#49961,#49962,
#49963,#49964,#49965,#49966,#49967)),.UNSPECIFIED.,.F.,.F.,.F.,(4,4),(4,
1,1,1,1,1,1,1,1,1,1,1,1,1,1,1,1,1,1,1,1,1,1,1,1,1,1,1,1,1,1,1,1,1,1,1,1,
1,1,1,1,1,1,1,1,1,1,1,1,1,1,1,1,1,1,1,1,1,1,1,1,1,1,1,1,1,1,1,1,1,1,1,1,
1,1,1,1,1,1,1,1,1,1,1,1,1,1,1,1,1,1,1,1,1,1,1,1,1,1,1,1,1,1,1,1,1,1,1,1,
1,1,1,1,1,1,1,1,1,1,1,1,1,1,1,1,1,1,1,1,1,1,1,1,1,1,1,1,1,1,1,1,1,1,1,1,
1,1,1,1,1,1,1,1,1,1,1,1,1,1,1,1,1,1,1,1,1,1,1,1,1,1,1,1,1,1,1,1,1,1,1,1,
1,1,1,1,1,1,1,1,1,1,1,1,1,1,1,1,1,1,1,1,1,1,1,1,1,1,1,1,1,1,1,1,1,1,1,1,
1,1,1,1,1,1,1,1,1,1,1,1,1,1,1,1,1,1,1,1,1,1,1,1,1,1,1,1,1,1,1,1,1,1,1,1,
1,1,1,1,1,1,1,1,1,1,1,1,1,1,1,1,1,1,1,1,1,1,1,1,1,1,1,1,1,1,1,1,1,1,1,1,
1,1,1,1,1,1,1,1,1,1,1,1,1,1,1,1,1,1,1,1,1,1,1,1,1,1,1,1,1,1,1,1,1,1,1,1,
1,1,1,1,1,1,1,1,1,1,1,1,1,1,1,1,1,1,1,1,1,1,1,1,1,1,1,1,1,1,1,1,1,1,1,1,
1,1,1,4),(0.,0.112756507572734),(14.3984001269719,14.8971467761357,15.3958934252995,
15.8946400744633,16.393386723627,16.8921333727908,17.3908800219546,17.8896266711184,
18.3883733202822,18.887119969446,19.3858666186097,19.8846132677735,20.3833599169373,
20.8821065661011,21.3808532152649,21.8795998644286,22.3783465135924,22.8770931627562,
23.37583981192,23.8745864610838,24.3733331102476,24.8720797594113,25.3708264085751,
25.8695730577389,26.3683197069027,26.8670663560665,27.3658130052302,27.864559654394,
28.3633063035578,28.8620529527216,29.3607996018854,29.8595462510491,30.3582929002129,
30.8570395493767,31.3557861985405,31.8545328477043,32.353279496868,32.8520261460318,
33.3507727951956,33.8495194443594,34.3482660935232,34.847012742687,35.3457593918507,
35.8445060410145,36.3432526901783,36.8419993393421,37.3407459885059,37.8394926376697,
38.3382392868334,38.8369859359972,39.335732585161,39.8344792343248,40.3332258834886,
40.8319725326523,41.3307191818161,41.8294658309799,42.3282124801437,42.8269591293075,
43.3257057784712,43.824452427635,44.3231990767988,44.8219457259626,45.3206923751264,
45.8194390242901,46.3181856734539,46.8169323226177,47.3156789717815,47.8144256209453,
48.313172270109,48.8119189192728,49.3106655684366,49.8094122176004,50.3081588667642,
50.806905515928,51.3056521650917,51.8043988142555,52.3031454634193,52.8018921125831,
53.3006387617469,53.7993854109106,54.2981320600744,54.7968787092382,55.295625358402,
55.7943720075658,56.2931186567296,56.7918653058933,57.2906119550571,57.7893586042209,
58.2881052533847,58.7868519025485,59.2855985517122,59.784345200876,60.2830918500398,
60.7818384992036,61.2805851483674,61.7793317975311,62.2780784466949,62.7768250958587,
63.2755717450225,63.7743183941863,64.2730650433501,64.7718116925138,65.2705583416776,
65.7693049908414,66.2680516400052,66.766798289169,67.2655449383327,67.7642915874965,
68.2630382366603,68.7617848858241,69.2605315349879,69.7592781841516,70.2580248333154,
70.7567714824792,71.255518131643,71.7542647808068,72.2530114299706,72.7517580791343,
73.2505047282981,73.7492513774619,74.2479980266257,74.7467446757895,75.2454913249532,
75.744237974117,76.2429846232808,76.7417312724446,77.2404779216084,77.7392245707722,
78.2379712199359,78.7367178690997,79.2354645182635,79.7342111674273,80.2329578165911,
80.7317044657548,81.2304511149186,81.7291977640824,82.2279444132462,82.72669106241,
83.2254377115737,83.7241843607375,84.2229310099013,84.7216776590651,85.2204243082289,
85.7191709573926,86.2179176065564,86.7166642557202,87.215410904884,87.7141575540478,
88.2129042032116,88.7116508523753,89.2103975015391,89.7091441507029,90.2078907998667,
90.7066374490305,91.2053840981942,91.704130747358,92.2028773965218,92.7016240456856,
93.2003706948494,93.6991173440131,94.1978639931769,94.6966106423407,95.1953572915045,
95.6941039406683,96.1928505898321,96.6915972389958,97.1903438881596,97.6890905373234,
98.1878371864872,98.686583835651,99.1853304848147,99.6840771339785,100.182823783142,
100.681570432306,101.18031708147,101.679063730634,102.177810379797,102.676557028961,
103.175303678125,103.674050327289,104.172796976453,104.671543625616,105.17029027478,
105.669036923944,106.167783573108,106.666530222271,107.165276871435,107.664023520599,
108.162770169763,108.661516818927,109.16026346809,109.659010117254,110.157756766418,
110.656503415582,111.155250064746,111.653996713909,112.152743363073,112.651490012237,
113.150236661401,113.648983310564,114.147729959728,114.646476608892,115.145223258056,
115.64396990722,116.142716556383,116.641463205547,117.140209854711,117.638956503875,
118.137703153038,118.636449802202,119.135196451366,119.63394310053,120.132689749694,
120.631436398857,121.130183048021,121.628929697185,122.127676346349,122.626422995512,
123.125169644676,123.62391629384,124.122662943004,124.621409592168,125.120156241331,
125.618902890495,126.117649539659,126.616396188823,127.115142837986,127.61388948715,
128.112636136314,128.611382785478,129.110129434642,129.608876083805,130.107622732969,
130.606369382133,131.105116031297,131.603862680461,132.102609329624,132.601355978788,
133.100102627952,133.598849277116,134.097595926279,134.596342575443,135.095089224607,
135.593835873771,136.092582522935,136.591329172098,137.090075821262,137.588822470426,
138.08756911959,138.586315768753,139.085062417917,139.583809067081,140.082555716245,
140.581302365409,141.080049014572,141.578795663736,142.0775423129,142.576288962064,
143.075035611227,143.573782260391,144.072528909555,144.571275558719,145.070022207883,
145.568768857046,146.06751550621,146.566262155374,147.065008804538,147.563755453702,
148.062502102865,148.561248752029,149.059995401193,149.558742050357,150.05748869952,
150.556235348684,151.054981997848,151.553728647012,152.052475296176,152.551221945339,
153.049968594503,153.548715243667,154.047461892831,154.546208541994,155.044955191158,
155.543701840322,156.042448489486,156.54119513865,157.039941787813,157.538688436977,
158.037435086141,158.536181735305,159.034928384469,159.533675033632,160.032421682796,
160.53116833196,161.029914981124,161.528661630287,162.027408279451,162.526154928615,
163.024901577779,163.523648226943,164.022394876106,164.52114152527,165.019888174434,
165.518634823598,166.017381472761,166.516128121925,167.014874771089,167.513621420253,
168.012368069417,168.51111471858,169.009861367744,169.508608016908,170.007354666072,
170.506101315235,171.004847964399,171.503594613563,172.002341262727,172.501087911891,
172.999834561054,173.498581210218,173.997327859382,174.496074508546,174.99482115771,
175.493567806873,175.992314456037,176.491061105201,176.989807754365,177.488554403528,
177.987301052692,178.486047701856,178.98479435102,179.483541000184,179.982287649347,
180.481034298511,180.979780947675,181.478527596839,181.977274246002,182.476020895166,
182.97476754433,183.473514193494,183.972260842658,184.471007491821,184.969754140985,
185.468500790149,185.967247439313,186.465994088476,186.96474073764,187.463487386804,
187.962234035968,188.460980685132,188.959727334295,189.458473983459,189.957220632623,
190.455967281787,190.954713930951,191.453460580114,191.952207229278,192.450953878442,
192.949700527606,193.448447176769,193.947193825933,194.445940475097,194.944687124261,
195.443433773425,195.942180422588),.UNSPECIFIED.);
#292=B_SPLINE_SURFACE_WITH_KNOTS('',3,3,((#55167,#55168,#55169,#55170,#55171,
#55172,#55173,#55174,#55175,#55176,#55177,#55178,#55179,#55180,#55181,#55182,
#55183,#55184,#55185,#55186,#55187,#55188,#55189,#55190,#55191,#55192,#55193,
#55194,#55195,#55196,#55197,#55198,#55199,#55200,#55201,#55202,#55203,#55204,
#55205,#55206,#55207,#55208,#55209,#55210,#55211,#55212,#55213,#55214,#55215,
#55216,#55217,#55218,#55219,#55220,#55221,#55222,#55223,#55224,#55225,#55226,
#55227,#55228,#55229,#55230,#55231,#55232,#55233,#55234,#55235,#55236,#55237,
#55238,#55239,#55240,#55241,#55242,#55243,#55244,#55245,#55246,#55247,#55248,
#55249,#55250,#55251,#55252,#55253,#55254,#55255,#55256,#55257,#55258,#55259,
#55260,#55261,#55262,#55263,#55264,#55265,#55266,#55267,#55268,#55269,#55270,
#55271,#55272,#55273,#55274,#55275,#55276,#55277,#55278,#55279,#55280,#55281,
#55282,#55283,#55284,#55285,#55286,#55287,#55288,#55289,#55290,#55291,#55292,
#55293,#55294,#55295,#55296,#55297,#55298,#55299,#55300,#55301,#55302,#55303,
#55304,#55305,#55306,#55307,#55308,#55309,#55310,#55311,#55312,#55313,#55314,
#55315,#55316,#55317,#55318,#55319,#55320,#55321,#55322,#55323,#55324,#55325,
#55326,#55327,#55328,#55329,#55330,#55331,#55332,#55333,#55334,#55335,#55336,
#55337,#55338,#55339,#55340,#55341,#55342,#55343,#55344,#55345,#55346,#55347,
#55348,#55349,#55350,#55351,#55352,#55353,#55354,#55355,#55356,#55357,#55358,
#55359,#55360,#55361,#55362,#55363,#55364,#55365,#55366,#55367,#55368,#55369,
#55370,#55371,#55372,#55373,#55374,#55375,#55376,#55377,#55378,#55379,#55380,
#55381,#55382,#55383,#55384,#55385,#55386,#55387,#55388,#55389,#55390,#55391,
#55392,#55393,#55394,#55395,#55396,#55397,#55398,#55399,#55400,#55401,#55402,
#55403,#55404,#55405,#55406,#55407,#55408,#55409,#55410,#55411,#55412,#55413,
#55414,#55415,#55416,#55417,#55418,#55419,#55420,#55421,#55422,#55423,#55424,
#55425,#55426,#55427,#55428,#55429,#55430,#55431,#55432,#55433,#55434,#55435,
#55436,#55437,#55438,#55439,#55440,#55441,#55442,#55443,#55444,#55445,#55446,
#55447,#55448,#55449,#55450,#55451,#55452,#55453,#55454,#55455,#55456,#55457,
#55458,#55459,#55460,#55461,#55462,#55463,#55464,#55465,#55466,#55467,#55468,
#55469,#55470,#55471,#55472,#55473,#55474,#55475,#55476,#55477,#55478,#55479,
#55480,#55481,#55482,#55483,#55484,#55485,#55486,#55487,#55488,#55489,#55490,
#55491,#55492,#55493,#55494,#55495,#55496,#55497,#55498,#55499,#55500,#55501,
#55502,#55503,#55504,#55505,#55506,#55507,#55508,#55509,#55510,#55511,#55512,
#55513,#55514,#55515,#55516,#55517,#55518,#55519,#55520,#55521,#55522,#55523,
#55524,#55525,#55526,#55527,#55528,#55529,#55530,#55531,#55532,#55533,#55534,
#55535,#55536,#55537,#55538,#55539,#55540,#55541,#55542,#55543,#55544,#55545,
#55546,#55547,#55548,#55549,#55550,#55551,#55552,#55553,#55554,#55555,#55556,
#55557,#55558,#55559,#55560,#55561,#55562,#55563,#55564,#55565,#55566,#55567,
#55568,#55569,#55570,#55571,#55572,#55573,#55574,#55575,#55576,#55577,#55578,
#55579,#55580,#55581,#55582,#55583,#55584,#55585,#55586,#55587,#55588,#55589,
#55590,#55591,#55592,#55593,#55594,#55595,#55596,#55597,#55598,#55599,#55600,
#55601,#55602,#55603,#55604,#55605,#55606,#55607,#55608,#55609,#55610,#55611,
#55612,#55613,#55614,#55615,#55616,#55617,#55618,#55619,#55620,#55621,#55622,
#55623,#55624,#55625,#55626,#55627,#55628,#55629,#55630,#55631,#55632,#55633),
(#55634,#55635,#55636,#55637,#55638,#55639,#55640,#55641,#55642,#55643,
#55644,#55645,#55646,#55647,#55648,#55649,#55650,#55651,#55652,#55653,#55654,
#55655,#55656,#55657,#55658,#55659,#55660,#55661,#55662,#55663,#55664,#55665,
#55666,#55667,#55668,#55669,#55670,#55671,#55672,#55673,#55674,#55675,#55676,
#55677,#55678,#55679,#55680,#55681,#55682,#55683,#55684,#55685,#55686,#55687,
#55688,#55689,#55690,#55691,#55692,#55693,#55694,#55695,#55696,#55697,#55698,
#55699,#55700,#55701,#55702,#55703,#55704,#55705,#55706,#55707,#55708,#55709,
#55710,#55711,#55712,#55713,#55714,#55715,#55716,#55717,#55718,#55719,#55720,
#55721,#55722,#55723,#55724,#55725,#55726,#55727,#55728,#55729,#55730,#55731,
#55732,#55733,#55734,#55735,#55736,#55737,#55738,#55739,#55740,#55741,#55742,
#55743,#55744,#55745,#55746,#55747,#55748,#55749,#55750,#55751,#55752,#55753,
#55754,#55755,#55756,#55757,#55758,#55759,#55760,#55761,#55762,#55763,#55764,
#55765,#55766,#55767,#55768,#55769,#55770,#55771,#55772,#55773,#55774,#55775,
#55776,#55777,#55778,#55779,#55780,#55781,#55782,#55783,#55784,#55785,#55786,
#55787,#55788,#55789,#55790,#55791,#55792,#55793,#55794,#55795,#55796,#55797,
#55798,#55799,#55800,#55801,#55802,#55803,#55804,#55805,#55806,#55807,#55808,
#55809,#55810,#55811,#55812,#55813,#55814,#55815,#55816,#55817,#55818,#55819,
#55820,#55821,#55822,#55823,#55824,#55825,#55826,#55827,#55828,#55829,#55830,
#55831,#55832,#55833,#55834,#55835,#55836,#55837,#55838,#55839,#55840,#55841,
#55842,#55843,#55844,#55845,#55846,#55847,#55848,#55849,#55850,#55851,#55852,
#55853,#55854,#55855,#55856,#55857,#55858,#55859,#55860,#55861,#55862,#55863,
#55864,#55865,#55866,#55867,#55868,#55869,#55870,#55871,#55872,#55873,#55874,
#55875,#55876,#55877,#55878,#55879,#55880,#55881,#55882,#55883,#55884,#55885,
#55886,#55887,#55888,#55889,#55890,#55891,#55892,#55893,#55894,#55895,#55896,
#55897,#55898,#55899,#55900,#55901,#55902,#55903,#55904,#55905,#55906,#55907,
#55908,#55909,#55910,#55911,#55912,#55913,#55914,#55915,#55916,#55917,#55918,
#55919,#55920,#55921,#55922,#55923,#55924,#55925,#55926,#55927,#55928,#55929,
#55930,#55931,#55932,#55933,#55934,#55935,#55936,#55937,#55938,#55939,#55940,
#55941,#55942,#55943,#55944,#55945,#55946,#55947,#55948,#55949,#55950,#55951,
#55952,#55953,#55954,#55955,#55956,#55957,#55958,#55959,#55960,#55961,#55962,
#55963,#55964,#55965,#55966,#55967,#55968,#55969,#55970,#55971,#55972,#55973,
#55974,#55975,#55976,#55977,#55978,#55979,#55980,#55981,#55982,#55983,#55984,
#55985,#55986,#55987,#55988,#55989,#55990,#55991,#55992,#55993,#55994,#55995,
#55996,#55997,#55998,#55999,#56000,#56001,#56002,#56003,#56004,#56005,#56006,
#56007,#56008,#56009,#56010,#56011,#56012,#56013,#56014,#56015,#56016,#56017,
#56018,#56019,#56020,#56021,#56022,#56023,#56024,#56025,#56026,#56027,#56028,
#56029,#56030,#56031,#56032,#56033,#56034,#56035,#56036,#56037,#56038,#56039,
#56040,#56041,#56042,#56043,#56044,#56045,#56046,#56047,#56048,#56049,#56050,
#56051,#56052,#56053,#56054,#56055,#56056,#56057,#56058,#56059,#56060,#56061,
#56062,#56063,#56064,#56065,#56066,#56067,#56068,#56069,#56070,#56071,#56072,
#56073,#56074,#56075,#56076,#56077,#56078,#56079,#56080,#56081,#56082,#56083,
#56084,#56085,#56086,#56087,#56088,#56089,#56090,#56091,#56092,#56093,#56094,
#56095,#56096,#56097,#56098,#56099,#56100),(#56101,#56102,#56103,#56104,
#56105,#56106,#56107,#56108,#56109,#56110,#56111,#56112,#56113,#56114,#56115,
#56116,#56117,#56118,#56119,#56120,#56121,#56122,#56123,#56124,#56125,#56126,
#56127,#56128,#56129,#56130,#56131,#56132,#56133,#56134,#56135,#56136,#56137,
#56138,#56139,#56140,#56141,#56142,#56143,#56144,#56145,#56146,#56147,#56148,
#56149,#56150,#56151,#56152,#56153,#56154,#56155,#56156,#56157,#56158,#56159,
#56160,#56161,#56162,#56163,#56164,#56165,#56166,#56167,#56168,#56169,#56170,
#56171,#56172,#56173,#56174,#56175,#56176,#56177,#56178,#56179,#56180,#56181,
#56182,#56183,#56184,#56185,#56186,#56187,#56188,#56189,#56190,#56191,#56192,
#56193,#56194,#56195,#56196,#56197,#56198,#56199,#56200,#56201,#56202,#56203,
#56204,#56205,#56206,#56207,#56208,#56209,#56210,#56211,#56212,#56213,#56214,
#56215,#56216,#56217,#56218,#56219,#56220,#56221,#56222,#56223,#56224,#56225,
#56226,#56227,#56228,#56229,#56230,#56231,#56232,#56233,#56234,#56235,#56236,
#56237,#56238,#56239,#56240,#56241,#56242,#56243,#56244,#56245,#56246,#56247,
#56248,#56249,#56250,#56251,#56252,#56253,#56254,#56255,#56256,#56257,#56258,
#56259,#56260,#56261,#56262,#56263,#56264,#56265,#56266,#56267,#56268,#56269,
#56270,#56271,#56272,#56273,#56274,#56275,#56276,#56277,#56278,#56279,#56280,
#56281,#56282,#56283,#56284,#56285,#56286,#56287,#56288,#56289,#56290,#56291,
#56292,#56293,#56294,#56295,#56296,#56297,#56298,#56299,#56300,#56301,#56302,
#56303,#56304,#56305,#56306,#56307,#56308,#56309,#56310,#56311,#56312,#56313,
#56314,#56315,#56316,#56317,#56318,#56319,#56320,#56321,#56322,#56323,#56324,
#56325,#56326,#56327,#56328,#56329,#56330,#56331,#56332,#56333,#56334,#56335,
#56336,#56337,#56338,#56339,#56340,#56341,#56342,#56343,#56344,#56345,#56346,
#56347,#56348,#56349,#56350,#56351,#56352,#56353,#56354,#56355,#56356,#56357,
#56358,#56359,#56360,#56361,#56362,#56363,#56364,#56365,#56366,#56367,#56368,
#56369,#56370,#56371,#56372,#56373,#56374,#56375,#56376,#56377,#56378,#56379,
#56380,#56381,#56382,#56383,#56384,#56385,#56386,#56387,#56388,#56389,#56390,
#56391,#56392,#56393,#56394,#56395,#56396,#56397,#56398,#56399,#56400,#56401,
#56402,#56403,#56404,#56405,#56406,#56407,#56408,#56409,#56410,#56411,#56412,
#56413,#56414,#56415,#56416,#56417,#56418,#56419,#56420,#56421,#56422,#56423,
#56424,#56425,#56426,#56427,#56428,#56429,#56430,#56431,#56432,#56433,#56434,
#56435,#56436,#56437,#56438,#56439,#56440,#56441,#56442,#56443,#56444,#56445,
#56446,#56447,#56448,#56449,#56450,#56451,#56452,#56453,#56454,#56455,#56456,
#56457,#56458,#56459,#56460,#56461,#56462,#56463,#56464,#56465,#56466,#56467,
#56468,#56469,#56470,#56471,#56472,#56473,#56474,#56475,#56476,#56477,#56478,
#56479,#56480,#56481,#56482,#56483,#56484,#56485,#56486,#56487,#56488,#56489,
#56490,#56491,#56492,#56493,#56494,#56495,#56496,#56497,#56498,#56499,#56500,
#56501,#56502,#56503,#56504,#56505,#56506,#56507,#56508,#56509,#56510,#56511,
#56512,#56513,#56514,#56515,#56516,#56517,#56518,#56519,#56520,#56521,#56522,
#56523,#56524,#56525,#56526,#56527,#56528,#56529,#56530,#56531,#56532,#56533,
#56534,#56535,#56536,#56537,#56538,#56539,#56540,#56541,#56542,#56543,#56544,
#56545,#56546,#56547,#56548,#56549,#56550,#56551,#56552,#56553,#56554,#56555,
#56556,#56557,#56558,#56559,#56560,#56561,#56562,#56563,#56564,#56565,#56566,
#56567),(#56568,#56569,#56570,#56571,#56572,#56573,#56574,#56575,#56576,
#56577,#56578,#56579,#56580,#56581,#56582,#56583,#56584,#56585,#56586,#56587,
#56588,#56589,#56590,#56591,#56592,#56593,#56594,#56595,#56596,#56597,#56598,
#56599,#56600,#56601,#56602,#56603,#56604,#56605,#56606,#56607,#56608,#56609,
#56610,#56611,#56612,#56613,#56614,#56615,#56616,#56617,#56618,#56619,#56620,
#56621,#56622,#56623,#56624,#56625,#56626,#56627,#56628,#56629,#56630,#56631,
#56632,#56633,#56634,#56635,#56636,#56637,#56638,#56639,#56640,#56641,#56642,
#56643,#56644,#56645,#56646,#56647,#56648,#56649,#56650,#56651,#56652,#56653,
#56654,#56655,#56656,#56657,#56658,#56659,#56660,#56661,#56662,#56663,#56664,
#56665,#56666,#56667,#56668,#56669,#56670,#56671,#56672,#56673,#56674,#56675,
#56676,#56677,#56678,#56679,#56680,#56681,#56682,#56683,#56684,#56685,#56686,
#56687,#56688,#56689,#56690,#56691,#56692,#56693,#56694,#56695,#56696,#56697,
#56698,#56699,#56700,#56701,#56702,#56703,#56704,#56705,#56706,#56707,#56708,
#56709,#56710,#56711,#56712,#56713,#56714,#56715,#56716,#56717,#56718,#56719,
#56720,#56721,#56722,#56723,#56724,#56725,#56726,#56727,#56728,#56729,#56730,
#56731,#56732,#56733,#56734,#56735,#56736,#56737,#56738,#56739,#56740,#56741,
#56742,#56743,#56744,#56745,#56746,#56747,#56748,#56749,#56750,#56751,#56752,
#56753,#56754,#56755,#56756,#56757,#56758,#56759,#56760,#56761,#56762,#56763,
#56764,#56765,#56766,#56767,#56768,#56769,#56770,#56771,#56772,#56773,#56774,
#56775,#56776,#56777,#56778,#56779,#56780,#56781,#56782,#56783,#56784,#56785,
#56786,#56787,#56788,#56789,#56790,#56791,#56792,#56793,#56794,#56795,#56796,
#56797,#56798,#56799,#56800,#56801,#56802,#56803,#56804,#56805,#56806,#56807,
#56808,#56809,#56810,#56811,#56812,#56813,#56814,#56815,#56816,#56817,#56818,
#56819,#56820,#56821,#56822,#56823,#56824,#56825,#56826,#56827,#56828,#56829,
#56830,#56831,#56832,#56833,#56834,#56835,#56836,#56837,#56838,#56839,#56840,
#56841,#56842,#56843,#56844,#56845,#56846,#56847,#56848,#56849,#56850,#56851,
#56852,#56853,#56854,#56855,#56856,#56857,#56858,#56859,#56860,#56861,#56862,
#56863,#56864,#56865,#56866,#56867,#56868,#56869,#56870,#56871,#56872,#56873,
#56874,#56875,#56876,#56877,#56878,#56879,#56880,#56881,#56882,#56883,#56884,
#56885,#56886,#56887,#56888,#56889,#56890,#56891,#56892,#56893,#56894,#56895,
#56896,#56897,#56898,#56899,#56900,#56901,#56902,#56903,#56904,#56905,#56906,
#56907,#56908,#56909,#56910,#56911,#56912,#56913,#56914,#56915,#56916,#56917,
#56918,#56919,#56920,#56921,#56922,#56923,#56924,#56925,#56926,#56927,#56928,
#56929,#56930,#56931,#56932,#56933,#56934,#56935,#56936,#56937,#56938,#56939,
#56940,#56941,#56942,#56943,#56944,#56945,#56946,#56947,#56948,#56949,#56950,
#56951,#56952,#56953,#56954,#56955,#56956,#56957,#56958,#56959,#56960,#56961,
#56962,#56963,#56964,#56965,#56966,#56967,#56968,#56969,#56970,#56971,#56972,
#56973,#56974,#56975,#56976,#56977,#56978,#56979,#56980,#56981,#56982,#56983,
#56984,#56985,#56986,#56987,#56988,#56989,#56990,#56991,#56992,#56993,#56994,
#56995,#56996,#56997,#56998,#56999,#57000,#57001,#57002,#57003,#57004,#57005,
#57006,#57007,#57008,#57009,#57010,#57011,#57012,#57013,#57014,#57015,#57016,
#57017,#57018,#57019,#57020,#57021,#57022,#57023,#57024,#57025,#57026,#57027,
#57028,#57029,#57030,#57031,#57032,#57033,#57034)),.UNSPECIFIED.,.F.,.F.,
 .F.,(4,4),(4,1,1,1,1,1,1,1,1,1,1,1,1,1,1,1,1,1,1,1,1,1,1,1,1,1,1,1,1,1,
1,1,1,1,1,1,1,1,1,1,1,1,1,1,1,1,1,1,1,1,1,1,1,1,1,1,1,1,1,1,1,1,1,1,1,1,
1,1,1,1,1,1,1,1,1,1,1,1,1,1,1,1,1,1,1,1,1,1,1,1,1,1,1,1,1,1,1,1,1,1,1,1,
1,1,1,1,1,1,1,1,1,1,1,1,1,1,1,1,1,1,1,1,1,1,1,1,1,1,1,1,1,1,1,1,1,1,1,1,
1,1,1,1,1,1,1,1,1,1,1,1,1,1,1,1,1,1,1,1,1,1,1,1,1,1,1,1,1,1,1,1,1,1,1,1,
1,1,1,1,1,1,1,1,1,1,1,1,1,1,1,1,1,1,1,1,1,1,1,1,1,1,1,1,1,1,1,1,1,1,1,1,
1,1,1,1,1,1,1,1,1,1,1,1,1,1,1,1,1,1,1,1,1,1,1,1,1,1,1,1,1,1,1,1,1,1,1,1,
1,1,1,1,1,1,1,1,1,1,1,1,1,1,1,1,1,1,1,1,1,1,1,1,1,1,1,1,1,1,1,1,1,1,1,1,
1,1,1,1,1,1,1,1,1,1,1,1,1,1,1,1,1,1,1,1,1,1,1,1,1,1,1,1,1,1,1,1,1,1,1,1,
1,1,1,1,1,1,1,1,1,1,1,1,1,1,1,1,1,1,1,1,1,1,1,1,1,1,1,1,1,1,1,1,1,1,1,1,
1,1,1,1,1,1,1,1,1,1,1,1,1,1,1,1,1,1,1,1,1,1,1,1,1,1,1,1,1,1,1,1,1,1,1,1,
1,1,1,1,1,1,1,1,1,1,1,1,1,1,1,1,1,1,1,1,1,1,1,1,1,1,1,1,1,1,1,1,1,1,1,1,
1,1,1,1,1,1,1,1,1,1,1,1,1,1,1,1,1,1,1,1,1,1,1,1,1,1,1,1,1,1,1,1,1,1,1,1,
1,1,4),(0.,0.115296848757168),(8.30592286723195,8.80561008027367,9.30529729331538,
9.80498450635709,10.3046717193988,10.8043589324405,11.3040461454822,11.8037333585239,
12.3034205715656,12.8031077846074,13.3027949976491,13.8024822106908,14.3021694237325,
14.8018566367742,15.3015438498159,15.8012310628576,16.3009182758993,16.800605488941,
17.3002927019828,17.7999799150245,18.2996671280662,18.7993543411079,19.2990415541496,
19.7987287671913,20.298415980233,20.7981031932747,21.2977904063164,21.7974776193581,
22.2971648323999,22.7968520454416,23.2965392584833,23.796226471525,24.2959136845667,
24.7956008976084,25.2952881106501,25.7949753236918,26.2946625367335,26.7943497497753,
27.294036962817,27.7937241758587,28.2934113889004,28.7930986019421,29.2927858149838,
29.7924730280255,30.2921602410672,30.7918474541089,31.2915346671507,31.7912218801924,
32.2909090932341,32.7905963062758,33.2902835193175,33.7899707323592,34.2896579454009,
34.7893451584426,35.2890323714843,35.7887195845261,36.2884067975678,36.7880940106095,
37.2877812236512,37.7874684366929,38.2871556497346,38.7868428627763,39.286530075818,
39.7862172888597,40.2859045019015,40.7855917149432,41.2852789279849,41.7849661410266,
42.2846533540683,42.78434056711,43.2840277801517,43.7837149931934,44.2834022062351,
44.7830894192769,45.2827766323186,45.7824638453603,46.282151058402,46.7818382714437,
47.2815254844854,47.7812126975271,48.2808999105688,48.7805871236105,49.2802743366523,
49.779961549694,50.2796487627357,50.7793359757774,51.2790231888191,51.7787104018608,
52.2783976149025,52.7780848279442,53.2777720409859,53.7774592540276,54.2771464670694,
54.7768336801111,55.2765208931528,55.7762081061945,56.2758953192362,56.7755825322779,
57.2752697453196,57.7749569583613,58.274644171403,58.7743313844448,59.2740185974865,
59.7737058105282,60.2733930235699,60.7730802366116,61.2727674496533,61.772454662695,
62.2721418757367,62.7718290887784,63.2715163018202,63.7712035148619,64.2708907279036,
64.7705779409453,65.270265153987,65.7699523670287,66.2696395800704,66.7693267931121,
67.2690140061538,67.7687012191955,68.2683884322373,68.768075645279,69.2677628583207,
69.7674500713624,70.2671372844041,70.7668244974458,71.2665117104875,71.7661989235292,
72.265886136571,72.7655733496127,73.2652605626544,73.7649477756961,74.2646349887378,
74.7643222017795,75.2640094148212,75.7636966278629,76.2633838409046,76.7630710539463,
77.2627582669881,77.7624454800298,78.2621326930715,78.7618199061132,79.2615071191549,
79.7611943321966,80.2608815452383,80.76056875828,81.2602559713218,81.7599431843635,
82.2596303974052,82.7593176104469,83.2590048234886,83.7586920365303,84.258379249572,
84.7580664626137,85.2577536756554,85.7574408886971,86.2571281017389,86.7568153147806,
87.2565025278223,87.756189740864,88.2558769539057,88.7555641669474,89.2552513799891,
89.7549385930308,90.2546258060726,90.7543130191143,91.254000232156,91.7536874451977,
92.2533746582394,92.7530618712811,93.2527490843228,93.7524362973645,94.2521235104062,
94.7518107234479,95.2514979364897,95.7511851495314,96.2508723625731,96.7505595756148,
97.2502467886565,97.7499340016982,98.2496212147399,98.7493084277816,99.2489956408234,
99.7486828538651,100.248370066907,100.748057279948,101.24774449299,101.747431706032,
102.247118919074,102.746806132115,103.246493345157,103.746180558199,104.24586777124,
104.745554984282,105.245242197324,105.744929410366,106.244616623407,106.744303836449,
107.243991049491,107.743678262532,108.243365475574,108.743052688616,109.242739901658,
109.742427114699,110.242114327741,110.741801540783,111.241488753824,111.741175966866,
112.240863179908,112.74055039295,113.240237605991,113.739924819033,114.239612032075,
114.739299245116,115.238986458158,115.7386736712,116.238360884242,116.738048097283,
117.237735310325,117.737422523367,118.237109736408,118.73679694945,119.236484162492,
119.736171375533,120.235858588575,120.735545801617,121.235233014659,121.7349202277,
122.234607440742,122.734294653784,123.233981866825,123.733669079867,124.233356292909,
124.733043505951,125.232730718992,125.732417932034,126.232105145076,126.731792358117,
127.231479571159,127.731166784201,128.230853997243,128.730541210284,129.230228423326,
129.729915636368,130.229602849409,130.729290062451,131.228977275493,131.728664488535,
132.228351701576,132.728038914618,133.22772612766,133.727413340701,134.227100553743,
134.726787766785,135.226474979827,135.726162192868,136.22584940591,136.725536618952,
137.225223831993,137.724911045035,138.224598258077,138.724285471118,139.22397268416,
139.723659897202,140.223347110244,140.723034323285,141.222721536327,141.722408749369,
142.22209596241,142.721783175452,143.221470388494,143.721157601536,144.220844814577,
144.720532027619,145.220219240661,145.719906453702,146.219593666744,146.719280879786,
147.218968092828,147.718655305869,148.218342518911,148.718029731953,149.217716944994,
149.717404158036,150.217091371078,150.71677858412,151.216465797161,151.716153010203,
152.215840223245,152.715527436286,153.215214649328,153.71490186237,154.214589075412,
154.714276288453,155.213963501495,155.713650714537,156.213337927578,156.71302514062,
157.212712353662,157.712399566704,158.212086779745,158.711773992787,159.211461205829,
159.71114841887,160.210835631912,160.710522844954,161.210210057995,161.709897271037,
162.209584484079,162.709271697121,163.208958910162,163.708646123204,164.208333336246,
164.708020549287,165.207707762329,165.707394975371,166.207082188413,166.706769401454,
167.206456614496,167.706143827538,168.205831040579,168.705518253621,169.205205466663,
169.704892679705,170.204579892746,170.704267105788,171.20395431883,171.703641531871,
172.203328744913,172.703015957955,173.202703170997,173.702390384038,174.20207759708,
174.701764810122,175.201452023163,175.701139236205,176.200826449247,176.700513662289,
177.20020087533,177.699888088372,178.199575301414,178.699262514455,179.198949727497,
179.698636940539,180.198324153581,180.698011366622,181.197698579664,181.697385792706,
182.197073005747,182.696760218789,183.196447431831,183.696134644872,184.195821857914,
184.695509070956,185.195196283998,185.694883497039,186.194570710081,186.694257923123,
187.193945136164,187.693632349206,188.193319562248,188.69300677529,189.192693988331,
189.692381201373,190.192068414415,190.691755627456,191.191442840498,191.69113005354,
192.190817266582,192.690504479623,193.190191692665,193.689878905707,194.189566118748,
194.68925333179,195.188940544832,195.688627757874,196.188314970915,196.688002183957,
197.187689396999,197.68737661004,198.187063823082,198.686751036124,199.186438249166,
199.686125462207,200.185812675249,200.685499888291,201.185187101332,201.684874314374,
202.184561527416,202.684248740457,203.183935953499,203.683623166541,204.183310379583,
204.682997592624,205.182684805666,205.682372018708,206.182059231749,206.681746444791,
207.181433657833,207.681120870875,208.180808083916,208.680495296958,209.18018251,
209.679869723041,210.179556936083,210.679244149125,211.178931362167,211.678618575208,
212.17830578825,212.677993001292,213.177680214333,213.677367427375,214.177054640417,
214.676741853459,215.1764290665,215.676116279542,216.175803492584,216.675490705625,
217.175177918667,217.674865131709,218.174552344751,218.674239557792,219.173926770834,
219.673613983876,220.173301196917,220.672988409959,221.172675623001,221.672362836043,
222.172050049084,222.671737262126,223.171424475168,223.671111688209,224.170798901251,
224.670486114293,225.170173327334,225.669860540376,226.169547753418,226.66923496646,
227.168922179501,227.668609392543,228.168296605585,228.667983818626,229.167671031668,
229.66735824471,230.167045457752,230.666732670793,231.166419883835,231.666107096877,
232.165794309918,232.66548152296,233.165168736002,233.664855949044,234.164543162085,
234.664230375127,235.163917588169,235.66360480121,236.163292014252,236.662979227294,
237.162666440336,237.662353653377,238.162040866419,238.661728079461,239.161415292502,
239.661102505544,240.160789718586),.UNSPECIFIED.);
#293=B_SPLINE_SURFACE_WITH_KNOTS('',3,3,((#57211,#57212,#57213,#57214,#57215,
#57216,#57217,#57218,#57219,#57220,#57221,#57222,#57223,#57224,#57225,#57226,
#57227,#57228,#57229,#57230,#57231,#57232,#57233,#57234,#57235,#57236,#57237,
#57238,#57239,#57240,#57241,#57242,#57243,#57244,#57245,#57246,#57247,#57248,
#57249,#57250,#57251,#57252,#57253,#57254,#57255,#57256,#57257,#57258,#57259,
#57260,#57261,#57262,#57263,#57264,#57265,#57266,#57267,#57268,#57269,#57270,
#57271,#57272,#57273,#57274,#57275,#57276,#57277,#57278,#57279,#57280,#57281,
#57282,#57283,#57284,#57285,#57286,#57287,#57288,#57289,#57290,#57291,#57292,
#57293,#57294,#57295,#57296,#57297,#57298,#57299,#57300,#57301,#57302,#57303,
#57304,#57305,#57306,#57307,#57308,#57309,#57310,#57311,#57312,#57313,#57314,
#57315,#57316,#57317,#57318,#57319,#57320,#57321,#57322,#57323,#57324,#57325,
#57326,#57327,#57328,#57329,#57330,#57331,#57332,#57333,#57334,#57335,#57336,
#57337,#57338,#57339,#57340,#57341,#57342,#57343,#57344,#57345,#57346,#57347,
#57348,#57349,#57350,#57351,#57352,#57353,#57354,#57355,#57356,#57357,#57358,
#57359,#57360,#57361,#57362,#57363,#57364,#57365,#57366,#57367,#57368,#57369,
#57370,#57371,#57372,#57373,#57374,#57375,#57376,#57377,#57378,#57379,#57380,
#57381,#57382,#57383,#57384,#57385,#57386,#57387,#57388,#57389,#57390,#57391,
#57392,#57393,#57394,#57395,#57396,#57397,#57398,#57399,#57400,#57401,#57402,
#57403,#57404,#57405,#57406,#57407,#57408,#57409,#57410,#57411,#57412,#57413,
#57414,#57415,#57416,#57417,#57418,#57419,#57420,#57421,#57422,#57423,#57424,
#57425,#57426,#57427,#57428,#57429,#57430,#57431,#57432,#57433,#57434,#57435,
#57436,#57437,#57438,#57439,#57440,#57441,#57442,#57443,#57444,#57445,#57446,
#57447,#57448,#57449,#57450,#57451,#57452,#57453,#57454,#57455,#57456,#57457,
#57458,#57459,#57460,#57461,#57462,#57463,#57464,#57465,#57466,#57467,#57468,
#57469,#57470,#57471,#57472,#57473,#57474,#57475,#57476,#57477,#57478,#57479,
#57480,#57481,#57482,#57483,#57484,#57485,#57486,#57487,#57488,#57489,#57490,
#57491,#57492,#57493,#57494,#57495,#57496,#57497,#57498,#57499,#57500,#57501,
#57502,#57503,#57504,#57505,#57506,#57507,#57508,#57509,#57510,#57511,#57512,
#57513,#57514,#57515,#57516,#57517,#57518,#57519,#57520,#57521,#57522,#57523,
#57524,#57525,#57526,#57527,#57528,#57529,#57530,#57531,#57532,#57533,#57534,
#57535,#57536,#57537,#57538,#57539,#57540,#57541,#57542,#57543,#57544,#57545,
#57546,#57547,#57548,#57549,#57550,#57551,#57552,#57553,#57554,#57555,#57556,
#57557,#57558,#57559,#57560,#57561,#57562,#57563,#57564,#57565,#57566,#57567,
#57568,#57569,#57570,#57571,#57572,#57573,#57574,#57575,#57576,#57577,#57578,
#57579,#57580,#57581,#57582,#57583,#57584,#57585,#57586,#57587,#57588,#57589,
#57590,#57591,#57592,#57593,#57594,#57595,#57596,#57597,#57598,#57599,#57600,
#57601,#57602,#57603,#57604,#57605,#57606,#57607,#57608,#57609,#57610,#57611,
#57612,#57613,#57614,#57615,#57616,#57617,#57618,#57619,#57620,#57621,#57622,
#57623,#57624,#57625,#57626,#57627,#57628,#57629,#57630,#57631,#57632,#57633,
#57634,#57635,#57636,#57637,#57638,#57639,#57640,#57641,#57642,#57643,#57644,
#57645,#57646,#57647,#57648,#57649,#57650,#57651,#57652,#57653,#57654,#57655,
#57656,#57657,#57658,#57659,#57660,#57661,#57662,#57663,#57664,#57665,#57666,
#57667,#57668,#57669,#57670,#57671,#57672,#57673,#57674,#57675,#57676,#57677),
(#57678,#57679,#57680,#57681,#57682,#57683,#57684,#57685,#57686,#57687,
#57688,#57689,#57690,#57691,#57692,#57693,#57694,#57695,#57696,#57697,#57698,
#57699,#57700,#57701,#57702,#57703,#57704,#57705,#57706,#57707,#57708,#57709,
#57710,#57711,#57712,#57713,#57714,#57715,#57716,#57717,#57718,#57719,#57720,
#57721,#57722,#57723,#57724,#57725,#57726,#57727,#57728,#57729,#57730,#57731,
#57732,#57733,#57734,#57735,#57736,#57737,#57738,#57739,#57740,#57741,#57742,
#57743,#57744,#57745,#57746,#57747,#57748,#57749,#57750,#57751,#57752,#57753,
#57754,#57755,#57756,#57757,#57758,#57759,#57760,#57761,#57762,#57763,#57764,
#57765,#57766,#57767,#57768,#57769,#57770,#57771,#57772,#57773,#57774,#57775,
#57776,#57777,#57778,#57779,#57780,#57781,#57782,#57783,#57784,#57785,#57786,
#57787,#57788,#57789,#57790,#57791,#57792,#57793,#57794,#57795,#57796,#57797,
#57798,#57799,#57800,#57801,#57802,#57803,#57804,#57805,#57806,#57807,#57808,
#57809,#57810,#57811,#57812,#57813,#57814,#57815,#57816,#57817,#57818,#57819,
#57820,#57821,#57822,#57823,#57824,#57825,#57826,#57827,#57828,#57829,#57830,
#57831,#57832,#57833,#57834,#57835,#57836,#57837,#57838,#57839,#57840,#57841,
#57842,#57843,#57844,#57845,#57846,#57847,#57848,#57849,#57850,#57851,#57852,
#57853,#57854,#57855,#57856,#57857,#57858,#57859,#57860,#57861,#57862,#57863,
#57864,#57865,#57866,#57867,#57868,#57869,#57870,#57871,#57872,#57873,#57874,
#57875,#57876,#57877,#57878,#57879,#57880,#57881,#57882,#57883,#57884,#57885,
#57886,#57887,#57888,#57889,#57890,#57891,#57892,#57893,#57894,#57895,#57896,
#57897,#57898,#57899,#57900,#57901,#57902,#57903,#57904,#57905,#57906,#57907,
#57908,#57909,#57910,#57911,#57912,#57913,#57914,#57915,#57916,#57917,#57918,
#57919,#57920,#57921,#57922,#57923,#57924,#57925,#57926,#57927,#57928,#57929,
#57930,#57931,#57932,#57933,#57934,#57935,#57936,#57937,#57938,#57939,#57940,
#57941,#57942,#57943,#57944,#57945,#57946,#57947,#57948,#57949,#57950,#57951,
#57952,#57953,#57954,#57955,#57956,#57957,#57958,#57959,#57960,#57961,#57962,
#57963,#57964,#57965,#57966,#57967,#57968,#57969,#57970,#57971,#57972,#57973,
#57974,#57975,#57976,#57977,#57978,#57979,#57980,#57981,#57982,#57983,#57984,
#57985,#57986,#57987,#57988,#57989,#57990,#57991,#57992,#57993,#57994,#57995,
#57996,#57997,#57998,#57999,#58000,#58001,#58002,#58003,#58004,#58005,#58006,
#58007,#58008,#58009,#58010,#58011,#58012,#58013,#58014,#58015,#58016,#58017,
#58018,#58019,#58020,#58021,#58022,#58023,#58024,#58025,#58026,#58027,#58028,
#58029,#58030,#58031,#58032,#58033,#58034,#58035,#58036,#58037,#58038,#58039,
#58040,#58041,#58042,#58043,#58044,#58045,#58046,#58047,#58048,#58049,#58050,
#58051,#58052,#58053,#58054,#58055,#58056,#58057,#58058,#58059,#58060,#58061,
#58062,#58063,#58064,#58065,#58066,#58067,#58068,#58069,#58070,#58071,#58072,
#58073,#58074,#58075,#58076,#58077,#58078,#58079,#58080,#58081,#58082,#58083,
#58084,#58085,#58086,#58087,#58088,#58089,#58090,#58091,#58092,#58093,#58094,
#58095,#58096,#58097,#58098,#58099,#58100,#58101,#58102,#58103,#58104,#58105,
#58106,#58107,#58108,#58109,#58110,#58111,#58112,#58113,#58114,#58115,#58116,
#58117,#58118,#58119,#58120,#58121,#58122,#58123,#58124,#58125,#58126,#58127,
#58128,#58129,#58130,#58131,#58132,#58133,#58134,#58135,#58136,#58137,#58138,
#58139,#58140,#58141,#58142,#58143,#58144),(#58145,#58146,#58147,#58148,
#58149,#58150,#58151,#58152,#58153,#58154,#58155,#58156,#58157,#58158,#58159,
#58160,#58161,#58162,#58163,#58164,#58165,#58166,#58167,#58168,#58169,#58170,
#58171,#58172,#58173,#58174,#58175,#58176,#58177,#58178,#58179,#58180,#58181,
#58182,#58183,#58184,#58185,#58186,#58187,#58188,#58189,#58190,#58191,#58192,
#58193,#58194,#58195,#58196,#58197,#58198,#58199,#58200,#58201,#58202,#58203,
#58204,#58205,#58206,#58207,#58208,#58209,#58210,#58211,#58212,#58213,#58214,
#58215,#58216,#58217,#58218,#58219,#58220,#58221,#58222,#58223,#58224,#58225,
#58226,#58227,#58228,#58229,#58230,#58231,#58232,#58233,#58234,#58235,#58236,
#58237,#58238,#58239,#58240,#58241,#58242,#58243,#58244,#58245,#58246,#58247,
#58248,#58249,#58250,#58251,#58252,#58253,#58254,#58255,#58256,#58257,#58258,
#58259,#58260,#58261,#58262,#58263,#58264,#58265,#58266,#58267,#58268,#58269,
#58270,#58271,#58272,#58273,#58274,#58275,#58276,#58277,#58278,#58279,#58280,
#58281,#58282,#58283,#58284,#58285,#58286,#58287,#58288,#58289,#58290,#58291,
#58292,#58293,#58294,#58295,#58296,#58297,#58298,#58299,#58300,#58301,#58302,
#58303,#58304,#58305,#58306,#58307,#58308,#58309,#58310,#58311,#58312,#58313,
#58314,#58315,#58316,#58317,#58318,#58319,#58320,#58321,#58322,#58323,#58324,
#58325,#58326,#58327,#58328,#58329,#58330,#58331,#58332,#58333,#58334,#58335,
#58336,#58337,#58338,#58339,#58340,#58341,#58342,#58343,#58344,#58345,#58346,
#58347,#58348,#58349,#58350,#58351,#58352,#58353,#58354,#58355,#58356,#58357,
#58358,#58359,#58360,#58361,#58362,#58363,#58364,#58365,#58366,#58367,#58368,
#58369,#58370,#58371,#58372,#58373,#58374,#58375,#58376,#58377,#58378,#58379,
#58380,#58381,#58382,#58383,#58384,#58385,#58386,#58387,#58388,#58389,#58390,
#58391,#58392,#58393,#58394,#58395,#58396,#58397,#58398,#58399,#58400,#58401,
#58402,#58403,#58404,#58405,#58406,#58407,#58408,#58409,#58410,#58411,#58412,
#58413,#58414,#58415,#58416,#58417,#58418,#58419,#58420,#58421,#58422,#58423,
#58424,#58425,#58426,#58427,#58428,#58429,#58430,#58431,#58432,#58433,#58434,
#58435,#58436,#58437,#58438,#58439,#58440,#58441,#58442,#58443,#58444,#58445,
#58446,#58447,#58448,#58449,#58450,#58451,#58452,#58453,#58454,#58455,#58456,
#58457,#58458,#58459,#58460,#58461,#58462,#58463,#58464,#58465,#58466,#58467,
#58468,#58469,#58470,#58471,#58472,#58473,#58474,#58475,#58476,#58477,#58478,
#58479,#58480,#58481,#58482,#58483,#58484,#58485,#58486,#58487,#58488,#58489,
#58490,#58491,#58492,#58493,#58494,#58495,#58496,#58497,#58498,#58499,#58500,
#58501,#58502,#58503,#58504,#58505,#58506,#58507,#58508,#58509,#58510,#58511,
#58512,#58513,#58514,#58515,#58516,#58517,#58518,#58519,#58520,#58521,#58522,
#58523,#58524,#58525,#58526,#58527,#58528,#58529,#58530,#58531,#58532,#58533,
#58534,#58535,#58536,#58537,#58538,#58539,#58540,#58541,#58542,#58543,#58544,
#58545,#58546,#58547,#58548,#58549,#58550,#58551,#58552,#58553,#58554,#58555,
#58556,#58557,#58558,#58559,#58560,#58561,#58562,#58563,#58564,#58565,#58566,
#58567,#58568,#58569,#58570,#58571,#58572,#58573,#58574,#58575,#58576,#58577,
#58578,#58579,#58580,#58581,#58582,#58583,#58584,#58585,#58586,#58587,#58588,
#58589,#58590,#58591,#58592,#58593,#58594,#58595,#58596,#58597,#58598,#58599,
#58600,#58601,#58602,#58603,#58604,#58605,#58606,#58607,#58608,#58609,#58610,
#58611),(#58612,#58613,#58614,#58615,#58616,#58617,#58618,#58619,#58620,
#58621,#58622,#58623,#58624,#58625,#58626,#58627,#58628,#58629,#58630,#58631,
#58632,#58633,#58634,#58635,#58636,#58637,#58638,#58639,#58640,#58641,#58642,
#58643,#58644,#58645,#58646,#58647,#58648,#58649,#58650,#58651,#58652,#58653,
#58654,#58655,#58656,#58657,#58658,#58659,#58660,#58661,#58662,#58663,#58664,
#58665,#58666,#58667,#58668,#58669,#58670,#58671,#58672,#58673,#58674,#58675,
#58676,#58677,#58678,#58679,#58680,#58681,#58682,#58683,#58684,#58685,#58686,
#58687,#58688,#58689,#58690,#58691,#58692,#58693,#58694,#58695,#58696,#58697,
#58698,#58699,#58700,#58701,#58702,#58703,#58704,#58705,#58706,#58707,#58708,
#58709,#58710,#58711,#58712,#58713,#58714,#58715,#58716,#58717,#58718,#58719,
#58720,#58721,#58722,#58723,#58724,#58725,#58726,#58727,#58728,#58729,#58730,
#58731,#58732,#58733,#58734,#58735,#58736,#58737,#58738,#58739,#58740,#58741,
#58742,#58743,#58744,#58745,#58746,#58747,#58748,#58749,#58750,#58751,#58752,
#58753,#58754,#58755,#58756,#58757,#58758,#58759,#58760,#58761,#58762,#58763,
#58764,#58765,#58766,#58767,#58768,#58769,#58770,#58771,#58772,#58773,#58774,
#58775,#58776,#58777,#58778,#58779,#58780,#58781,#58782,#58783,#58784,#58785,
#58786,#58787,#58788,#58789,#58790,#58791,#58792,#58793,#58794,#58795,#58796,
#58797,#58798,#58799,#58800,#58801,#58802,#58803,#58804,#58805,#58806,#58807,
#58808,#58809,#58810,#58811,#58812,#58813,#58814,#58815,#58816,#58817,#58818,
#58819,#58820,#58821,#58822,#58823,#58824,#58825,#58826,#58827,#58828,#58829,
#58830,#58831,#58832,#58833,#58834,#58835,#58836,#58837,#58838,#58839,#58840,
#58841,#58842,#58843,#58844,#58845,#58846,#58847,#58848,#58849,#58850,#58851,
#58852,#58853,#58854,#58855,#58856,#58857,#58858,#58859,#58860,#58861,#58862,
#58863,#58864,#58865,#58866,#58867,#58868,#58869,#58870,#58871,#58872,#58873,
#58874,#58875,#58876,#58877,#58878,#58879,#58880,#58881,#58882,#58883,#58884,
#58885,#58886,#58887,#58888,#58889,#58890,#58891,#58892,#58893,#58894,#58895,
#58896,#58897,#58898,#58899,#58900,#58901,#58902,#58903,#58904,#58905,#58906,
#58907,#58908,#58909,#58910,#58911,#58912,#58913,#58914,#58915,#58916,#58917,
#58918,#58919,#58920,#58921,#58922,#58923,#58924,#58925,#58926,#58927,#58928,
#58929,#58930,#58931,#58932,#58933,#58934,#58935,#58936,#58937,#58938,#58939,
#58940,#58941,#58942,#58943,#58944,#58945,#58946,#58947,#58948,#58949,#58950,
#58951,#58952,#58953,#58954,#58955,#58956,#58957,#58958,#58959,#58960,#58961,
#58962,#58963,#58964,#58965,#58966,#58967,#58968,#58969,#58970,#58971,#58972,
#58973,#58974,#58975,#58976,#58977,#58978,#58979,#58980,#58981,#58982,#58983,
#58984,#58985,#58986,#58987,#58988,#58989,#58990,#58991,#58992,#58993,#58994,
#58995,#58996,#58997,#58998,#58999,#59000,#59001,#59002,#59003,#59004,#59005,
#59006,#59007,#59008,#59009,#59010,#59011,#59012,#59013,#59014,#59015,#59016,
#59017,#59018,#59019,#59020,#59021,#59022,#59023,#59024,#59025,#59026,#59027,
#59028,#59029,#59030,#59031,#59032,#59033,#59034,#59035,#59036,#59037,#59038,
#59039,#59040,#59041,#59042,#59043,#59044,#59045,#59046,#59047,#59048,#59049,
#59050,#59051,#59052,#59053,#59054,#59055,#59056,#59057,#59058,#59059,#59060,
#59061,#59062,#59063,#59064,#59065,#59066,#59067,#59068,#59069,#59070,#59071,
#59072,#59073,#59074,#59075,#59076,#59077,#59078)),.UNSPECIFIED.,.F.,.F.,
 .F.,(4,4),(4,1,1,1,1,1,1,1,1,1,1,1,1,1,1,1,1,1,1,1,1,1,1,1,1,1,1,1,1,1,
1,1,1,1,1,1,1,1,1,1,1,1,1,1,1,1,1,1,1,1,1,1,1,1,1,1,1,1,1,1,1,1,1,1,1,1,
1,1,1,1,1,1,1,1,1,1,1,1,1,1,1,1,1,1,1,1,1,1,1,1,1,1,1,1,1,1,1,1,1,1,1,1,
1,1,1,1,1,1,1,1,1,1,1,1,1,1,1,1,1,1,1,1,1,1,1,1,1,1,1,1,1,1,1,1,1,1,1,1,
1,1,1,1,1,1,1,1,1,1,1,1,1,1,1,1,1,1,1,1,1,1,1,1,1,1,1,1,1,1,1,1,1,1,1,1,
1,1,1,1,1,1,1,1,1,1,1,1,1,1,1,1,1,1,1,1,1,1,1,1,1,1,1,1,1,1,1,1,1,1,1,1,
1,1,1,1,1,1,1,1,1,1,1,1,1,1,1,1,1,1,1,1,1,1,1,1,1,1,1,1,1,1,1,1,1,1,1,1,
1,1,1,1,1,1,1,1,1,1,1,1,1,1,1,1,1,1,1,1,1,1,1,1,1,1,1,1,1,1,1,1,1,1,1,1,
1,1,1,1,1,1,1,1,1,1,1,1,1,1,1,1,1,1,1,1,1,1,1,1,1,1,1,1,1,1,1,1,1,1,1,1,
1,1,1,1,1,1,1,1,1,1,1,1,1,1,1,1,1,1,1,1,1,1,1,1,1,1,1,1,1,1,1,1,1,1,1,1,
1,1,1,1,1,1,1,1,1,1,1,1,1,1,1,1,1,1,1,1,1,1,1,1,1,1,1,1,1,1,1,1,1,1,1,1,
1,1,1,1,1,1,1,1,1,1,1,1,1,1,1,1,1,1,1,1,1,1,1,1,1,1,1,1,1,1,1,1,1,1,1,1,
1,1,1,1,1,1,1,1,1,1,1,1,1,1,1,1,1,1,1,1,1,1,1,1,1,1,1,1,1,1,1,1,1,1,1,1,
1,1,4),(0.,0.115296848757168),(11.6154215191109,12.1151087321526,12.6147959451943,
13.114483158236,13.6141703712778,14.1138575843195,14.6135447973612,15.1132320104029,
15.6129192234446,16.1126064364863,16.612293649528,17.1119808625697,17.6116680756114,
18.1113552886532,18.6110425016949,19.1107297147366,19.6104169277783,20.11010414082,
20.6097913538617,21.1094785669034,21.6091657799451,22.1088529929868,22.6085402060286,
23.1082274190703,23.607914632112,24.1076018451537,24.6072890581954,25.1069762712371,
25.6066634842788,26.1063506973205,26.6060379103622,27.1057251234039,27.6054123364457,
28.1050995494874,28.6047867625291,29.1044739755708,29.6041611886125,30.1038484016542,
30.6035356146959,31.1032228277376,31.6029100407793,32.1025972538211,32.6022844668628,
33.1019716799045,33.6016588929462,34.1013461059879,34.6010333190296,35.1007205320713,
35.600407745113,36.1000949581547,36.5997821711965,37.0994693842382,37.5991565972799,
38.0988438103216,38.5985310233633,39.098218236405,39.5979054494467,40.0975926624884,
40.5972798755301,41.0969670885719,41.5966543016136,42.0963415146553,42.596028727697,
43.0957159407387,43.5954031537804,44.0950903668221,44.5947775798638,45.0944647929055,
45.5941520059473,46.093839218989,46.5935264320307,47.0932136450724,47.5929008581141,
48.0925880711558,48.5922752841975,49.0919624972392,49.5916497102809,50.0913369233227,
50.5910241363644,51.0907113494061,51.5903985624478,52.0900857754895,52.5897729885312,
53.0894602015729,53.5891474146146,54.0888346276563,54.588521840698,55.0882090537398,
55.5878962667815,56.0875834798232,56.5872706928649,57.0869579059066,57.5866451189483,
58.08633233199,58.5860195450317,59.0857067580734,59.5853939711152,60.0850811841569,
60.5847683971986,61.0844556102403,61.584142823282,62.0838300363237,62.5835172493654,
63.0832044624071,63.5828916754488,64.0825788884906,64.5822661015323,65.081953314574,
65.5816405276157,66.0813277406574,66.5810149536991,67.0807021667408,67.5803893797825,
68.0800765928242,68.579763805866,69.0794510189077,69.5791382319494,70.0788254449911,
70.5785126580328,71.0781998710745,71.5778870841162,72.0775742971579,72.5772615101996,
73.0769487232413,73.5766359362831,74.0763231493248,74.5760103623665,75.0756975754082,
75.5753847884499,76.0750720014916,76.5747592145333,77.074446427575,77.5741336406168,
78.0738208536585,78.5735080667002,79.0731952797419,79.5728824927836,80.0725697058253,
80.572256918867,81.0719441319087,81.5716313449504,82.0713185579921,82.5710057710339,
83.0706929840756,83.5703801971173,84.070067410159,84.5697546232007,85.0694418362424,
85.5691290492841,86.0688162623258,86.5685034753675,87.0681906884093,87.567877901451,
88.0675651144927,88.5672523275344,89.0669395405761,89.5666267536178,90.0663139666595,
90.5660011797012,91.0656883927429,91.5653756057847,92.0650628188264,92.5647500318681,
93.0644372449098,93.5641244579515,94.0638116709932,94.5634988840349,95.0631860970766,
95.5628733101183,96.06256052316,96.5622477362018,97.0619349492435,97.5616221622852,
98.0613093753269,98.5609965883686,99.0606838014103,99.560371014452,100.060058227494,
100.559745440535,101.059432653577,101.559119866619,102.058807079661,102.558494292702,
103.058181505744,103.557868718786,104.057555931827,104.557243144869,105.056930357911,
105.556617570953,106.056304783994,106.555991997036,107.055679210078,107.555366423119,
108.055053636161,108.554740849203,109.054428062245,109.554115275286,110.053802488328,
110.55348970137,111.053176914411,111.552864127453,112.052551340495,112.552238553537,
113.051925766578,113.55161297962,114.051300192662,114.550987405703,115.050674618745,
115.550361831787,116.050049044828,116.54973625787,117.049423470912,117.549110683954,
118.048797896995,118.548485110037,119.048172323079,119.54785953612,120.047546749162,
120.547233962204,121.046921175246,121.546608388287,122.046295601329,122.545982814371,
123.045670027412,123.545357240454,124.045044453496,124.544731666538,125.044418879579,
125.544106092621,126.043793305663,126.543480518704,127.043167731746,127.542854944788,
128.04254215783,128.542229370871,129.041916583913,129.541603796955,130.041291009996,
130.540978223038,131.04066543608,131.540352649122,132.040039862163,132.539727075205,
133.039414288247,133.539101501288,134.03878871433,134.538475927372,135.038163140414,
135.537850353455,136.037537566497,136.537224779539,137.03691199258,137.536599205622,
138.036286418664,138.535973631705,139.035660844747,139.535348057789,140.035035270831,
140.534722483872,141.034409696914,141.534096909956,142.033784122997,142.533471336039,
143.033158549081,143.532845762123,144.032532975164,144.532220188206,145.031907401248,
145.531594614289,146.031281827331,146.530969040373,147.030656253415,147.530343466456,
148.030030679498,148.52971789254,149.029405105581,149.529092318623,150.028779531665,
150.528466744707,151.028153957748,151.52784117079,152.027528383832,152.527215596873,
153.026902809915,153.526590022957,154.026277235998,154.52596444904,155.025651662082,
155.525338875124,156.025026088165,156.524713301207,157.024400514249,157.52408772729,
158.023774940332,158.523462153374,159.023149366416,159.522836579457,160.022523792499,
160.522211005541,161.021898218582,161.521585431624,162.021272644666,162.520959857708,
163.020647070749,163.520334283791,164.020021496833,164.519708709874,165.019395922916,
165.519083135958,166.018770349,166.518457562041,167.018144775083,167.517831988125,
168.017519201166,168.517206414208,169.01689362725,169.516580840292,170.016268053333,
170.515955266375,171.015642479417,171.515329692458,172.0150169055,172.514704118542,
173.014391331584,173.514078544625,174.013765757667,174.513452970709,175.01314018375,
175.512827396792,176.012514609834,176.512201822876,177.011889035917,177.511576248959,
178.011263462001,178.510950675042,179.010637888084,179.510325101126,180.010012314167,
180.509699527209,181.009386740251,181.509073953293,182.008761166334,182.508448379376,
183.008135592418,183.507822805459,184.007510018501,184.507197231543,185.006884444585,
185.506571657626,186.006258870668,186.50594608371,187.005633296751,187.505320509793,
188.005007722835,188.504694935877,189.004382148918,189.50406936196,190.003756575002,
190.503443788043,191.003131001085,191.502818214127,192.002505427169,192.50219264021,
193.001879853252,193.501567066294,194.001254279335,194.500941492377,195.000628705419,
195.500315918461,196.000003131502,196.499690344544,196.999377557586,197.499064770627,
197.998751983669,198.498439196711,198.998126409752,199.497813622794,199.997500835836,
200.497188048878,200.996875261919,201.496562474961,201.996249688003,202.495936901044,
202.995624114086,203.495311327128,203.99499854017,204.494685753211,204.994372966253,
205.494060179295,205.993747392336,206.493434605378,206.99312181842,207.492809031462,
207.992496244503,208.492183457545,208.991870670587,209.491557883628,209.99124509667,
210.490932309712,210.990619522754,211.490306735795,211.989993948837,212.489681161879,
212.98936837492,213.489055587962,213.988742801004,214.488430014046,214.988117227087,
215.487804440129,215.987491653171,216.487178866212,216.986866079254,217.486553292296,
217.986240505338,218.485927718379,218.985614931421,219.485302144463,219.984989357504,
220.484676570546,220.984363783588,221.484050996629,221.983738209671,222.483425422713,
222.983112635755,223.482799848796,223.982487061838,224.48217427488,224.981861487921,
225.481548700963,225.981235914005,226.480923127047,226.980610340088,227.48029755313,
227.979984766172,228.479671979213,228.979359192255,229.479046405297,229.978733618339,
230.47842083138,230.978108044422,231.477795257464,231.977482470505,232.477169683547,
232.976856896589,233.476544109631,233.976231322672,234.475918535714,234.975605748756,
235.475292961797,235.974980174839,236.474667387881,236.974354600923,237.474041813964,
237.973729027006,238.473416240048,238.973103453089,239.472790666131,239.972477879173,
240.472165092214,240.971852305256,241.471539518298,241.97122673134,242.470913944381,
242.970601157423,243.470288370465),.UNSPECIFIED.);
#294=B_SPLINE_SURFACE_WITH_KNOTS('',3,3,((#62492,#62493,#62494,#62495,#62496,
#62497,#62498,#62499,#62500,#62501,#62502,#62503,#62504,#62505,#62506,#62507,
#62508,#62509,#62510,#62511,#62512,#62513,#62514,#62515,#62516,#62517,#62518,
#62519,#62520,#62521,#62522,#62523,#62524,#62525,#62526,#62527,#62528,#62529,
#62530,#62531,#62532,#62533,#62534,#62535,#62536,#62537,#62538,#62539,#62540,
#62541,#62542,#62543,#62544,#62545,#62546,#62547,#62548,#62549,#62550,#62551,
#62552,#62553,#62554,#62555,#62556,#62557,#62558,#62559,#62560,#62561,#62562,
#62563,#62564,#62565,#62566,#62567,#62568,#62569,#62570,#62571,#62572,#62573,
#62574,#62575,#62576,#62577,#62578,#62579,#62580,#62581,#62582,#62583,#62584,
#62585,#62586,#62587,#62588,#62589,#62590,#62591,#62592,#62593,#62594,#62595,
#62596,#62597,#62598,#62599,#62600,#62601,#62602,#62603,#62604,#62605,#62606,
#62607,#62608,#62609,#62610,#62611,#62612,#62613,#62614,#62615,#62616,#62617,
#62618,#62619,#62620,#62621,#62622,#62623,#62624,#62625,#62626,#62627,#62628,
#62629,#62630,#62631,#62632,#62633,#62634,#62635,#62636,#62637,#62638,#62639,
#62640,#62641,#62642,#62643,#62644,#62645,#62646,#62647,#62648,#62649,#62650,
#62651,#62652,#62653,#62654,#62655,#62656,#62657,#62658,#62659,#62660,#62661,
#62662,#62663,#62664,#62665,#62666,#62667,#62668,#62669,#62670,#62671,#62672,
#62673,#62674,#62675,#62676,#62677,#62678,#62679,#62680,#62681,#62682,#62683,
#62684,#62685,#62686,#62687,#62688,#62689,#62690,#62691,#62692,#62693,#62694,
#62695,#62696,#62697,#62698,#62699,#62700,#62701,#62702,#62703,#62704,#62705,
#62706,#62707,#62708,#62709,#62710,#62711,#62712,#62713,#62714,#62715,#62716,
#62717,#62718,#62719,#62720,#62721,#62722,#62723,#62724,#62725,#62726,#62727,
#62728,#62729,#62730,#62731,#62732,#62733,#62734,#62735,#62736,#62737,#62738,
#62739,#62740,#62741,#62742,#62743),(#62744,#62745,#62746,#62747,#62748,
#62749,#62750,#62751,#62752,#62753,#62754,#62755,#62756,#62757,#62758,#62759,
#62760,#62761,#62762,#62763,#62764,#62765,#62766,#62767,#62768,#62769,#62770,
#62771,#62772,#62773,#62774,#62775,#62776,#62777,#62778,#62779,#62780,#62781,
#62782,#62783,#62784,#62785,#62786,#62787,#62788,#62789,#62790,#62791,#62792,
#62793,#62794,#62795,#62796,#62797,#62798,#62799,#62800,#62801,#62802,#62803,
#62804,#62805,#62806,#62807,#62808,#62809,#62810,#62811,#62812,#62813,#62814,
#62815,#62816,#62817,#62818,#62819,#62820,#62821,#62822,#62823,#62824,#62825,
#62826,#62827,#62828,#62829,#62830,#62831,#62832,#62833,#62834,#62835,#62836,
#62837,#62838,#62839,#62840,#62841,#62842,#62843,#62844,#62845,#62846,#62847,
#62848,#62849,#62850,#62851,#62852,#62853,#62854,#62855,#62856,#62857,#62858,
#62859,#62860,#62861,#62862,#62863,#62864,#62865,#62866,#62867,#62868,#62869,
#62870,#62871,#62872,#62873,#62874,#62875,#62876,#62877,#62878,#62879,#62880,
#62881,#62882,#62883,#62884,#62885,#62886,#62887,#62888,#62889,#62890,#62891,
#62892,#62893,#62894,#62895,#62896,#62897,#62898,#62899,#62900,#62901,#62902,
#62903,#62904,#62905,#62906,#62907,#62908,#62909,#62910,#62911,#62912,#62913,
#62914,#62915,#62916,#62917,#62918,#62919,#62920,#62921,#62922,#62923,#62924,
#62925,#62926,#62927,#62928,#62929,#62930,#62931,#62932,#62933,#62934,#62935,
#62936,#62937,#62938,#62939,#62940,#62941,#62942,#62943,#62944,#62945,#62946,
#62947,#62948,#62949,#62950,#62951,#62952,#62953,#62954,#62955,#62956,#62957,
#62958,#62959,#62960,#62961,#62962,#62963,#62964,#62965,#62966,#62967,#62968,
#62969,#62970,#62971,#62972,#62973,#62974,#62975,#62976,#62977,#62978,#62979,
#62980,#62981,#62982,#62983,#62984,#62985,#62986,#62987,#62988,#62989,#62990,
#62991,#62992,#62993,#62994,#62995),(#62996,#62997,#62998,#62999,#63000,
#63001,#63002,#63003,#63004,#63005,#63006,#63007,#63008,#63009,#63010,#63011,
#63012,#63013,#63014,#63015,#63016,#63017,#63018,#63019,#63020,#63021,#63022,
#63023,#63024,#63025,#63026,#63027,#63028,#63029,#63030,#63031,#63032,#63033,
#63034,#63035,#63036,#63037,#63038,#63039,#63040,#63041,#63042,#63043,#63044,
#63045,#63046,#63047,#63048,#63049,#63050,#63051,#63052,#63053,#63054,#63055,
#63056,#63057,#63058,#63059,#63060,#63061,#63062,#63063,#63064,#63065,#63066,
#63067,#63068,#63069,#63070,#63071,#63072,#63073,#63074,#63075,#63076,#63077,
#63078,#63079,#63080,#63081,#63082,#63083,#63084,#63085,#63086,#63087,#63088,
#63089,#63090,#63091,#63092,#63093,#63094,#63095,#63096,#63097,#63098,#63099,
#63100,#63101,#63102,#63103,#63104,#63105,#63106,#63107,#63108,#63109,#63110,
#63111,#63112,#63113,#63114,#63115,#63116,#63117,#63118,#63119,#63120,#63121,
#63122,#63123,#63124,#63125,#63126,#63127,#63128,#63129,#63130,#63131,#63132,
#63133,#63134,#63135,#63136,#63137,#63138,#63139,#63140,#63141,#63142,#63143,
#63144,#63145,#63146,#63147,#63148,#63149,#63150,#63151,#63152,#63153,#63154,
#63155,#63156,#63157,#63158,#63159,#63160,#63161,#63162,#63163,#63164,#63165,
#63166,#63167,#63168,#63169,#63170,#63171,#63172,#63173,#63174,#63175,#63176,
#63177,#63178,#63179,#63180,#63181,#63182,#63183,#63184,#63185,#63186,#63187,
#63188,#63189,#63190,#63191,#63192,#63193,#63194,#63195,#63196,#63197,#63198,
#63199,#63200,#63201,#63202,#63203,#63204,#63205,#63206,#63207,#63208,#63209,
#63210,#63211,#63212,#63213,#63214,#63215,#63216,#63217,#63218,#63219,#63220,
#63221,#63222,#63223,#63224,#63225,#63226,#63227,#63228,#63229,#63230,#63231,
#63232,#63233,#63234,#63235,#63236,#63237,#63238,#63239,#63240,#63241,#63242,
#63243,#63244,#63245,#63246,#63247),(#63248,#63249,#63250,#63251,#63252,
#63253,#63254,#63255,#63256,#63257,#63258,#63259,#63260,#63261,#63262,#63263,
#63264,#63265,#63266,#63267,#63268,#63269,#63270,#63271,#63272,#63273,#63274,
#63275,#63276,#63277,#63278,#63279,#63280,#63281,#63282,#63283,#63284,#63285,
#63286,#63287,#63288,#63289,#63290,#63291,#63292,#63293,#63294,#63295,#63296,
#63297,#63298,#63299,#63300,#63301,#63302,#63303,#63304,#63305,#63306,#63307,
#63308,#63309,#63310,#63311,#63312,#63313,#63314,#63315,#63316,#63317,#63318,
#63319,#63320,#63321,#63322,#63323,#63324,#63325,#63326,#63327,#63328,#63329,
#63330,#63331,#63332,#63333,#63334,#63335,#63336,#63337,#63338,#63339,#63340,
#63341,#63342,#63343,#63344,#63345,#63346,#63347,#63348,#63349,#63350,#63351,
#63352,#63353,#63354,#63355,#63356,#63357,#63358,#63359,#63360,#63361,#63362,
#63363,#63364,#63365,#63366,#63367,#63368,#63369,#63370,#63371,#63372,#63373,
#63374,#63375,#63376,#63377,#63378,#63379,#63380,#63381,#63382,#63383,#63384,
#63385,#63386,#63387,#63388,#63389,#63390,#63391,#63392,#63393,#63394,#63395,
#63396,#63397,#63398,#63399,#63400,#63401,#63402,#63403,#63404,#63405,#63406,
#63407,#63408,#63409,#63410,#63411,#63412,#63413,#63414,#63415,#63416,#63417,
#63418,#63419,#63420,#63421,#63422,#63423,#63424,#63425,#63426,#63427,#63428,
#63429,#63430,#63431,#63432,#63433,#63434,#63435,#63436,#63437,#63438,#63439,
#63440,#63441,#63442,#63443,#63444,#63445,#63446,#63447,#63448,#63449,#63450,
#63451,#63452,#63453,#63454,#63455,#63456,#63457,#63458,#63459,#63460,#63461,
#63462,#63463,#63464,#63465,#63466,#63467,#63468,#63469,#63470,#63471,#63472,
#63473,#63474,#63475,#63476,#63477,#63478,#63479,#63480,#63481,#63482,#63483,
#63484,#63485,#63486,#63487,#63488,#63489,#63490,#63491,#63492,#63493,#63494,
#63495,#63496,#63497,#63498,#63499)),.UNSPECIFIED.,.F.,.F.,.F.,(4,4),(4,
1,1,1,1,1,1,1,1,1,1,1,1,1,1,1,1,1,1,1,1,1,1,1,1,1,1,1,1,1,1,1,1,1,1,1,1,
1,1,1,1,1,1,1,1,1,1,1,1,1,1,1,1,1,1,1,1,1,1,1,1,1,1,1,1,1,1,1,1,1,1,1,1,
1,1,1,1,1,1,1,1,1,1,1,1,1,1,1,1,1,1,1,1,1,1,1,1,1,1,1,1,1,1,1,1,1,1,1,1,
1,1,1,1,1,1,1,1,1,1,1,1,1,1,1,1,1,1,1,1,1,1,1,1,1,1,1,1,1,1,1,1,1,1,1,1,
1,1,1,1,1,1,1,1,1,1,1,1,1,1,1,1,1,1,1,1,1,1,1,1,1,1,1,1,1,1,1,1,1,1,1,1,
1,1,1,1,1,1,1,1,1,1,1,1,1,1,1,1,1,1,1,1,1,1,1,1,1,1,1,1,1,1,1,1,1,1,1,1,
1,1,1,1,1,1,1,1,1,1,1,1,1,1,1,1,1,1,1,1,1,1,1,1,1,1,1,1,1,1,1,1,4),(0.,
0.0658467982010768),(11.6150328478187,12.6149992660887,13.6149656843588,
14.6149321026288,15.6148985208988,16.6148649391689,17.6148313574389,18.614797775709,
19.614764193979,20.614730612249,21.6146970305191,22.6146634487891,23.6146298670591,
24.6145962853292,25.6145627035992,26.6145291218693,27.6144955401393,28.6144619584093,
29.6144283766794,30.6143947949494,31.6143612132194,32.6143276314895,33.6142940497595,
34.6142604680296,35.6142268862996,36.6141933045696,37.6141597228397,38.6141261411097,
39.6140925593798,40.6140589776498,41.6140253959198,42.6139918141899,43.6139582324599,
44.6139246507299,45.613891069,46.61385748727,47.6138239055401,48.6137903238101,
49.6137567420801,50.6137231603502,51.6136895786202,52.6136559968902,53.6136224151603,
54.6135888334303,55.6135552517004,56.6135216699704,57.6134880882404,58.6134545065105,
59.6134209247805,60.6133873430505,61.6133537613206,62.6133201795906,63.6132865978607,
64.6132530161307,65.6132194344007,66.6131858526708,67.6131522709408,68.6131186892109,
69.6130851074809,70.6130515257509,71.613017944021,72.612984362291,73.612950780561,
74.6129171988311,75.6128836171011,76.6128500353712,77.6128164536412,78.6127828719112,
79.6127492901813,80.6127157084513,81.6126821267214,82.6126485449914,83.6126149632614,
84.6125813815315,85.6125477998015,86.6125142180715,87.6124806363416,88.6124470546116,
89.6124134728817,90.6123798911517,91.6123463094217,92.6123127276918,93.6122791459618,
94.6122455642318,95.6122119825019,96.6121784007719,97.612144819042,98.612111237312,
99.612077655582,100.612044073852,101.612010492122,102.611976910392,103.611943328662,
104.611909746932,105.611876165202,106.611842583472,107.611809001742,108.611775420012,
109.611741838282,110.611708256552,111.611674674822,112.611641093093,113.611607511363,
114.611573929633,115.611540347903,116.611506766173,117.611473184443,118.611439602713,
119.611406020983,120.611372439253,121.611338857523,122.611305275793,123.611271694063,
124.611238112333,125.611204530603,126.611170948873,127.611137367143,128.611103785413,
129.611070203683,130.611036621953,131.611003040223,132.610969458493,133.610935876763,
134.610902295033,135.610868713303,136.610835131573,137.610801549843,138.610767968113,
139.610734386384,140.610700804654,141.610667222924,142.610633641194,143.610600059464,
144.610566477734,145.610532896004,146.610499314274,147.610465732544,148.610432150814,
149.610398569084,150.610364987354,151.610331405624,152.610297823894,153.610264242164,
154.610230660434,155.610197078704,156.610163496974,157.610129915244,158.610096333514,
159.610062751784,160.610029170054,161.609995588324,162.609962006594,163.609928424864,
164.609894843134,165.609861261405,166.609827679675,167.609794097945,168.609760516215,
169.609726934485,170.609693352755,171.609659771025,172.609626189295,173.609592607565,
174.609559025835,175.609525444105,176.609491862375,177.609458280645,178.609424698915,
179.609391117185,180.609357535455,181.609323953725,182.609290371995,183.609256790265,
184.609223208535,185.609189626805,186.609156045075,187.609122463345,188.609088881615,
189.609055299885,190.609021718155,191.608988136425,192.608954554696,193.608920972966,
194.608887391236,195.608853809506,196.608820227776,197.608786646046,198.608753064316,
199.608719482586,200.608685900856,201.608652319126,202.608618737396,203.608585155666,
204.608551573936,205.608517992206,206.608484410476,207.608450828746,208.608417247016,
209.608383665286,210.608350083556,211.608316501826,212.608282920096,213.608249338366,
214.608215756636,215.608182174906,216.608148593176,217.608115011447,218.608081429717,
219.608047847987,220.608014266257,221.607980684527,222.607947102797,223.607913521067,
224.607879939337,225.607846357607,226.607812775877,227.607779194147,228.607745612417,
229.607712030687,230.607678448957,231.607644867227,232.607611285497,233.607577703767,
234.607544122037,235.607510540307,236.607476958577,237.607443376847,238.607409795117,
239.607376213387,240.607342631657,241.607309049927,242.607275468197,243.607241886467,
244.607208304738,245.607174723008,246.607141141278,247.607107559548,248.607073977818,
249.607040396088,250.607006814358,251.606973232628,252.606939650898,253.606906069168,
254.606872487438,255.606838905708,256.606805323978,257.606771742248,258.606738160518,
259.606704578788,260.606670997058),.UNSPECIFIED.);
#295=B_SPLINE_SURFACE_WITH_KNOTS('',3,3,((#63634,#63635,#63636,#63637,#63638,
#63639,#63640,#63641,#63642,#63643,#63644,#63645,#63646,#63647,#63648,#63649,
#63650,#63651,#63652,#63653,#63654,#63655,#63656,#63657,#63658,#63659,#63660,
#63661,#63662,#63663,#63664,#63665,#63666,#63667,#63668,#63669,#63670,#63671,
#63672,#63673,#63674,#63675,#63676,#63677,#63678,#63679,#63680,#63681,#63682,
#63683,#63684,#63685,#63686,#63687,#63688,#63689,#63690,#63691,#63692,#63693,
#63694,#63695,#63696,#63697,#63698,#63699,#63700,#63701,#63702,#63703,#63704,
#63705,#63706,#63707,#63708,#63709,#63710,#63711,#63712,#63713,#63714,#63715,
#63716,#63717,#63718,#63719,#63720,#63721,#63722,#63723,#63724,#63725,#63726,
#63727,#63728,#63729,#63730,#63731,#63732,#63733,#63734,#63735,#63736,#63737,
#63738,#63739,#63740,#63741,#63742,#63743,#63744,#63745,#63746,#63747,#63748,
#63749,#63750,#63751,#63752,#63753,#63754,#63755,#63756,#63757,#63758,#63759,
#63760,#63761,#63762,#63763,#63764,#63765,#63766,#63767,#63768,#63769,#63770,
#63771,#63772,#63773,#63774,#63775,#63776,#63777,#63778,#63779,#63780,#63781,
#63782,#63783,#63784,#63785,#63786,#63787,#63788,#63789,#63790,#63791,#63792,
#63793,#63794,#63795,#63796,#63797,#63798,#63799,#63800,#63801,#63802,#63803,
#63804,#63805,#63806,#63807,#63808,#63809,#63810,#63811,#63812,#63813,#63814,
#63815,#63816,#63817,#63818,#63819,#63820,#63821,#63822,#63823,#63824,#63825,
#63826,#63827,#63828,#63829,#63830,#63831,#63832,#63833,#63834,#63835,#63836,
#63837,#63838,#63839,#63840,#63841,#63842,#63843,#63844,#63845,#63846,#63847,
#63848,#63849,#63850,#63851,#63852,#63853,#63854,#63855,#63856,#63857,#63858,
#63859,#63860,#63861,#63862,#63863,#63864,#63865,#63866,#63867,#63868,#63869,
#63870,#63871,#63872,#63873,#63874,#63875,#63876,#63877,#63878,#63879,#63880,
#63881,#63882,#63883,#63884,#63885,#63886,#63887,#63888),(#63889,#63890,
#63891,#63892,#63893,#63894,#63895,#63896,#63897,#63898,#63899,#63900,#63901,
#63902,#63903,#63904,#63905,#63906,#63907,#63908,#63909,#63910,#63911,#63912,
#63913,#63914,#63915,#63916,#63917,#63918,#63919,#63920,#63921,#63922,#63923,
#63924,#63925,#63926,#63927,#63928,#63929,#63930,#63931,#63932,#63933,#63934,
#63935,#63936,#63937,#63938,#63939,#63940,#63941,#63942,#63943,#63944,#63945,
#63946,#63947,#63948,#63949,#63950,#63951,#63952,#63953,#63954,#63955,#63956,
#63957,#63958,#63959,#63960,#63961,#63962,#63963,#63964,#63965,#63966,#63967,
#63968,#63969,#63970,#63971,#63972,#63973,#63974,#63975,#63976,#63977,#63978,
#63979,#63980,#63981,#63982,#63983,#63984,#63985,#63986,#63987,#63988,#63989,
#63990,#63991,#63992,#63993,#63994,#63995,#63996,#63997,#63998,#63999,#64000,
#64001,#64002,#64003,#64004,#64005,#64006,#64007,#64008,#64009,#64010,#64011,
#64012,#64013,#64014,#64015,#64016,#64017,#64018,#64019,#64020,#64021,#64022,
#64023,#64024,#64025,#64026,#64027,#64028,#64029,#64030,#64031,#64032,#64033,
#64034,#64035,#64036,#64037,#64038,#64039,#64040,#64041,#64042,#64043,#64044,
#64045,#64046,#64047,#64048,#64049,#64050,#64051,#64052,#64053,#64054,#64055,
#64056,#64057,#64058,#64059,#64060,#64061,#64062,#64063,#64064,#64065,#64066,
#64067,#64068,#64069,#64070,#64071,#64072,#64073,#64074,#64075,#64076,#64077,
#64078,#64079,#64080,#64081,#64082,#64083,#64084,#64085,#64086,#64087,#64088,
#64089,#64090,#64091,#64092,#64093,#64094,#64095,#64096,#64097,#64098,#64099,
#64100,#64101,#64102,#64103,#64104,#64105,#64106,#64107,#64108,#64109,#64110,
#64111,#64112,#64113,#64114,#64115,#64116,#64117,#64118,#64119,#64120,#64121,
#64122,#64123,#64124,#64125,#64126,#64127,#64128,#64129,#64130,#64131,#64132,
#64133,#64134,#64135,#64136,#64137,#64138,#64139,#64140,#64141,#64142,#64143),
(#64144,#64145,#64146,#64147,#64148,#64149,#64150,#64151,#64152,#64153,
#64154,#64155,#64156,#64157,#64158,#64159,#64160,#64161,#64162,#64163,#64164,
#64165,#64166,#64167,#64168,#64169,#64170,#64171,#64172,#64173,#64174,#64175,
#64176,#64177,#64178,#64179,#64180,#64181,#64182,#64183,#64184,#64185,#64186,
#64187,#64188,#64189,#64190,#64191,#64192,#64193,#64194,#64195,#64196,#64197,
#64198,#64199,#64200,#64201,#64202,#64203,#64204,#64205,#64206,#64207,#64208,
#64209,#64210,#64211,#64212,#64213,#64214,#64215,#64216,#64217,#64218,#64219,
#64220,#64221,#64222,#64223,#64224,#64225,#64226,#64227,#64228,#64229,#64230,
#64231,#64232,#64233,#64234,#64235,#64236,#64237,#64238,#64239,#64240,#64241,
#64242,#64243,#64244,#64245,#64246,#64247,#64248,#64249,#64250,#64251,#64252,
#64253,#64254,#64255,#64256,#64257,#64258,#64259,#64260,#64261,#64262,#64263,
#64264,#64265,#64266,#64267,#64268,#64269,#64270,#64271,#64272,#64273,#64274,
#64275,#64276,#64277,#64278,#64279,#64280,#64281,#64282,#64283,#64284,#64285,
#64286,#64287,#64288,#64289,#64290,#64291,#64292,#64293,#64294,#64295,#64296,
#64297,#64298,#64299,#64300,#64301,#64302,#64303,#64304,#64305,#64306,#64307,
#64308,#64309,#64310,#64311,#64312,#64313,#64314,#64315,#64316,#64317,#64318,
#64319,#64320,#64321,#64322,#64323,#64324,#64325,#64326,#64327,#64328,#64329,
#64330,#64331,#64332,#64333,#64334,#64335,#64336,#64337,#64338,#64339,#64340,
#64341,#64342,#64343,#64344,#64345,#64346,#64347,#64348,#64349,#64350,#64351,
#64352,#64353,#64354,#64355,#64356,#64357,#64358,#64359,#64360,#64361,#64362,
#64363,#64364,#64365,#64366,#64367,#64368,#64369,#64370,#64371,#64372,#64373,
#64374,#64375,#64376,#64377,#64378,#64379,#64380,#64381,#64382,#64383,#64384,
#64385,#64386,#64387,#64388,#64389,#64390,#64391,#64392,#64393,#64394,#64395,
#64396,#64397,#64398),(#64399,#64400,#64401,#64402,#64403,#64404,#64405,
#64406,#64407,#64408,#64409,#64410,#64411,#64412,#64413,#64414,#64415,#64416,
#64417,#64418,#64419,#64420,#64421,#64422,#64423,#64424,#64425,#64426,#64427,
#64428,#64429,#64430,#64431,#64432,#64433,#64434,#64435,#64436,#64437,#64438,
#64439,#64440,#64441,#64442,#64443,#64444,#64445,#64446,#64447,#64448,#64449,
#64450,#64451,#64452,#64453,#64454,#64455,#64456,#64457,#64458,#64459,#64460,
#64461,#64462,#64463,#64464,#64465,#64466,#64467,#64468,#64469,#64470,#64471,
#64472,#64473,#64474,#64475,#64476,#64477,#64478,#64479,#64480,#64481,#64482,
#64483,#64484,#64485,#64486,#64487,#64488,#64489,#64490,#64491,#64492,#64493,
#64494,#64495,#64496,#64497,#64498,#64499,#64500,#64501,#64502,#64503,#64504,
#64505,#64506,#64507,#64508,#64509,#64510,#64511,#64512,#64513,#64514,#64515,
#64516,#64517,#64518,#64519,#64520,#64521,#64522,#64523,#64524,#64525,#64526,
#64527,#64528,#64529,#64530,#64531,#64532,#64533,#64534,#64535,#64536,#64537,
#64538,#64539,#64540,#64541,#64542,#64543,#64544,#64545,#64546,#64547,#64548,
#64549,#64550,#64551,#64552,#64553,#64554,#64555,#64556,#64557,#64558,#64559,
#64560,#64561,#64562,#64563,#64564,#64565,#64566,#64567,#64568,#64569,#64570,
#64571,#64572,#64573,#64574,#64575,#64576,#64577,#64578,#64579,#64580,#64581,
#64582,#64583,#64584,#64585,#64586,#64587,#64588,#64589,#64590,#64591,#64592,
#64593,#64594,#64595,#64596,#64597,#64598,#64599,#64600,#64601,#64602,#64603,
#64604,#64605,#64606,#64607,#64608,#64609,#64610,#64611,#64612,#64613,#64614,
#64615,#64616,#64617,#64618,#64619,#64620,#64621,#64622,#64623,#64624,#64625,
#64626,#64627,#64628,#64629,#64630,#64631,#64632,#64633,#64634,#64635,#64636,
#64637,#64638,#64639,#64640,#64641,#64642,#64643,#64644,#64645,#64646,#64647,
#64648,#64649,#64650,#64651,#64652,#64653)),.UNSPECIFIED.,.F.,.F.,.F.,(4,
4),(4,1,1,1,1,1,1,1,1,1,1,1,1,1,1,1,1,1,1,1,1,1,1,1,1,1,1,1,1,1,1,1,1,1,
1,1,1,1,1,1,1,1,1,1,1,1,1,1,1,1,1,1,1,1,1,1,1,1,1,1,1,1,1,1,1,1,1,1,1,1,
1,1,1,1,1,1,1,1,1,1,1,1,1,1,1,1,1,1,1,1,1,1,1,1,1,1,1,1,1,1,1,1,1,1,1,1,
1,1,1,1,1,1,1,1,1,1,1,1,1,1,1,1,1,1,1,1,1,1,1,1,1,1,1,1,1,1,1,1,1,1,1,1,
1,1,1,1,1,1,1,1,1,1,1,1,1,1,1,1,1,1,1,1,1,1,1,1,1,1,1,1,1,1,1,1,1,1,1,1,
1,1,1,1,1,1,1,1,1,1,1,1,1,1,1,1,1,1,1,1,1,1,1,1,1,1,1,1,1,1,1,1,1,1,1,1,
1,1,1,1,1,1,1,1,1,1,1,1,1,1,1,1,1,1,1,1,1,1,1,1,1,1,1,1,1,1,1,1,1,1,1,1,
1,1,4),(0.,0.0658467982010768),(8.30747755240138,9.30374849019562,10.3000194279899,
11.2962903657841,12.2925613035783,13.2888322413726,14.2851031791668,15.2813741169611,
16.2776450547553,17.2739159925495,18.2701869303438,19.266457868138,20.2627288059323,
21.2589997437265,22.2552706815207,23.251541619315,24.2478125571092,25.2440834949035,
26.2403544326977,27.236625370492,28.2328963082862,29.2291672460804,30.2254381838747,
31.2217091216689,32.2179800594632,33.2142509972574,34.2105219350516,35.2067928728459,
36.2030638106401,37.1993347484344,38.1956056862286,39.1918766240228,40.1881475618171,
41.1844184996113,42.1806894374056,43.1769603751998,44.1732313129941,45.1695022507883,
46.1657731885825,47.1620441263768,48.158315064171,49.1545860019653,50.1508569397595,
51.1471278775537,52.143398815348,53.1396697531422,54.1359406909365,55.1322116287307,
56.1284825665249,57.1247535043192,58.1210244421134,59.1172953799077,60.1135663177019,
61.1098372554961,62.1061081932904,63.1023791310846,64.0986500688789,65.0949210066731,
66.0911919444674,67.0874628822616,68.0837338200558,69.0800047578501,70.0762756956443,
71.0725466334385,72.0688175712328,73.065088509027,74.0613594468213,75.0576303846155,
76.0539013224098,77.050172260204,78.0464431979982,79.0427141357925,80.0389850735867,
81.035256011381,82.0315269491752,83.0277978869695,84.0240688247637,85.0203397625579,
86.0166107003522,87.0128816381464,88.0091525759407,89.0054235137349,90.0016944515291,
90.9979653893234,91.9942363271176,92.9905072649119,93.9867782027061,94.9830491405003,
95.9793200782946,96.9755910160888,97.9718619538831,98.9681328916773,99.9644038294716,
100.960674767266,101.95694570506,102.953216642854,103.949487580649,104.945758518443,
105.942029456237,106.938300394031,107.934571331825,108.93084226962,109.927113207414,
110.923384145208,111.919655083002,112.915926020797,113.912196958591,114.908467896385,
115.904738834179,116.901009771974,117.897280709768,118.893551647562,119.889822585356,
120.886093523151,121.882364460945,122.878635398739,123.874906336533,124.871177274328,
125.867448212122,126.863719149916,127.85999008771,128.856261025505,129.852531963299,
130.848802901093,131.845073838887,132.841344776681,133.837615714476,134.83388665227,
135.830157590064,136.826428527858,137.822699465653,138.818970403447,139.815241341241,
140.811512279035,141.80778321683,142.804054154624,143.800325092418,144.796596030212,
145.792866968007,146.789137905801,147.785408843595,148.781679781389,149.777950719184,
150.774221656978,151.770492594772,152.766763532566,153.763034470361,154.759305408155,
155.755576345949,156.751847283743,157.748118221538,158.744389159332,159.740660097126,
160.73693103492,161.733201972714,162.729472910509,163.725743848303,164.722014786097,
165.718285723891,166.714556661686,167.71082759948,168.707098537274,169.703369475068,
170.699640412863,171.695911350657,172.692182288451,173.688453226245,174.68472416404,
175.680995101834,176.677266039628,177.673536977422,178.669807915217,179.666078853011,
180.662349790805,181.658620728599,182.654891666394,183.651162604188,184.647433541982,
185.643704479776,186.63997541757,187.636246355365,188.632517293159,189.628788230953,
190.625059168747,191.621330106542,192.617601044336,193.61387198213,194.610142919924,
195.606413857719,196.602684795513,197.598955733307,198.595226671101,199.591497608896,
200.58776854669,201.584039484484,202.580310422278,203.576581360073,204.572852297867,
205.569123235661,206.565394173455,207.56166511125,208.557936049044,209.554206986838,
210.550477924632,211.546748862427,212.543019800221,213.539290738015,214.535561675809,
215.531832613603,216.528103551398,217.524374489192,218.520645426986,219.51691636478,
220.513187302575,221.509458240369,222.505729178163,223.502000115957,224.498271053752,
225.494541991546,226.49081292934,227.487083867134,228.483354804929,229.479625742723,
230.475896680517,231.472167618311,232.468438556106,233.4647094939,234.460980431694,
235.457251369488,236.453522307283,237.449793245077,238.446064182871,239.442335120665,
240.438606058459,241.434876996254,242.431147934048,243.427418871842,244.423689809636,
245.419960747431,246.416231685225,247.412502623019,248.408773560813,249.405044498608,
250.401315436402,251.397586374196,252.39385731199,253.390128249785,254.386399187579,
255.382670125373,256.378941063167,257.375212000962,258.371482938756,259.36775387655),
 .UNSPECIFIED.);
#296=B_SPLINE_SURFACE_WITH_KNOTS('',3,3,((#67508,#67509,#67510,#67511,#67512,
#67513,#67514,#67515,#67516,#67517,#67518,#67519,#67520,#67521,#67522,#67523,
#67524,#67525,#67526,#67527,#67528,#67529,#67530,#67531,#67532,#67533,#67534,
#67535,#67536,#67537,#67538,#67539,#67540,#67541,#67542,#67543,#67544,#67545,
#67546,#67547,#67548,#67549,#67550,#67551,#67552,#67553,#67554,#67555,#67556,
#67557,#67558,#67559,#67560,#67561,#67562,#67563,#67564,#67565,#67566,#67567,
#67568,#67569,#67570,#67571,#67572,#67573,#67574,#67575,#67576,#67577,#67578,
#67579,#67580,#67581,#67582,#67583,#67584,#67585,#67586,#67587,#67588,#67589,
#67590,#67591,#67592,#67593,#67594,#67595,#67596,#67597,#67598,#67599,#67600,
#67601,#67602,#67603,#67604,#67605,#67606,#67607,#67608,#67609,#67610,#67611,
#67612,#67613,#67614,#67615,#67616,#67617,#67618,#67619,#67620,#67621,#67622,
#67623,#67624,#67625,#67626,#67627,#67628,#67629,#67630,#67631,#67632,#67633,
#67634,#67635,#67636,#67637,#67638,#67639,#67640,#67641,#67642,#67643,#67644,
#67645,#67646,#67647,#67648,#67649,#67650,#67651,#67652,#67653,#67654,#67655,
#67656,#67657,#67658,#67659,#67660,#67661,#67662,#67663,#67664,#67665,#67666,
#67667,#67668,#67669,#67670,#67671,#67672,#67673,#67674,#67675,#67676,#67677,
#67678,#67679,#67680,#67681,#67682,#67683,#67684,#67685,#67686,#67687,#67688,
#67689,#67690,#67691,#67692,#67693,#67694,#67695,#67696,#67697,#67698,#67699,
#67700,#67701,#67702,#67703,#67704,#67705,#67706,#67707,#67708,#67709,#67710),
(#67711,#67712,#67713,#67714,#67715,#67716,#67717,#67718,#67719,#67720,
#67721,#67722,#67723,#67724,#67725,#67726,#67727,#67728,#67729,#67730,#67731,
#67732,#67733,#67734,#67735,#67736,#67737,#67738,#67739,#67740,#67741,#67742,
#67743,#67744,#67745,#67746,#67747,#67748,#67749,#67750,#67751,#67752,#67753,
#67754,#67755,#67756,#67757,#67758,#67759,#67760,#67761,#67762,#67763,#67764,
#67765,#67766,#67767,#67768,#67769,#67770,#67771,#67772,#67773,#67774,#67775,
#67776,#67777,#67778,#67779,#67780,#67781,#67782,#67783,#67784,#67785,#67786,
#67787,#67788,#67789,#67790,#67791,#67792,#67793,#67794,#67795,#67796,#67797,
#67798,#67799,#67800,#67801,#67802,#67803,#67804,#67805,#67806,#67807,#67808,
#67809,#67810,#67811,#67812,#67813,#67814,#67815,#67816,#67817,#67818,#67819,
#67820,#67821,#67822,#67823,#67824,#67825,#67826,#67827,#67828,#67829,#67830,
#67831,#67832,#67833,#67834,#67835,#67836,#67837,#67838,#67839,#67840,#67841,
#67842,#67843,#67844,#67845,#67846,#67847,#67848,#67849,#67850,#67851,#67852,
#67853,#67854,#67855,#67856,#67857,#67858,#67859,#67860,#67861,#67862,#67863,
#67864,#67865,#67866,#67867,#67868,#67869,#67870,#67871,#67872,#67873,#67874,
#67875,#67876,#67877,#67878,#67879,#67880,#67881,#67882,#67883,#67884,#67885,
#67886,#67887,#67888,#67889,#67890,#67891,#67892,#67893,#67894,#67895,#67896,
#67897,#67898,#67899,#67900,#67901,#67902,#67903,#67904,#67905,#67906,#67907,
#67908,#67909,#67910,#67911,#67912,#67913),(#67914,#67915,#67916,#67917,
#67918,#67919,#67920,#67921,#67922,#67923,#67924,#67925,#67926,#67927,#67928,
#67929,#67930,#67931,#67932,#67933,#67934,#67935,#67936,#67937,#67938,#67939,
#67940,#67941,#67942,#67943,#67944,#67945,#67946,#67947,#67948,#67949,#67950,
#67951,#67952,#67953,#67954,#67955,#67956,#67957,#67958,#67959,#67960,#67961,
#67962,#67963,#67964,#67965,#67966,#67967,#67968,#67969,#67970,#67971,#67972,
#67973,#67974,#67975,#67976,#67977,#67978,#67979,#67980,#67981,#67982,#67983,
#67984,#67985,#67986,#67987,#67988,#67989,#67990,#67991,#67992,#67993,#67994,
#67995,#67996,#67997,#67998,#67999,#68000,#68001,#68002,#68003,#68004,#68005,
#68006,#68007,#68008,#68009,#68010,#68011,#68012,#68013,#68014,#68015,#68016,
#68017,#68018,#68019,#68020,#68021,#68022,#68023,#68024,#68025,#68026,#68027,
#68028,#68029,#68030,#68031,#68032,#68033,#68034,#68035,#68036,#68037,#68038,
#68039,#68040,#68041,#68042,#68043,#68044,#68045,#68046,#68047,#68048,#68049,
#68050,#68051,#68052,#68053,#68054,#68055,#68056,#68057,#68058,#68059,#68060,
#68061,#68062,#68063,#68064,#68065,#68066,#68067,#68068,#68069,#68070,#68071,
#68072,#68073,#68074,#68075,#68076,#68077,#68078,#68079,#68080,#68081,#68082,
#68083,#68084,#68085,#68086,#68087,#68088,#68089,#68090,#68091,#68092,#68093,
#68094,#68095,#68096,#68097,#68098,#68099,#68100,#68101,#68102,#68103,#68104,
#68105,#68106,#68107,#68108,#68109,#68110,#68111,#68112,#68113,#68114,#68115,
#68116),(#68117,#68118,#68119,#68120,#68121,#68122,#68123,#68124,#68125,
#68126,#68127,#68128,#68129,#68130,#68131,#68132,#68133,#68134,#68135,#68136,
#68137,#68138,#68139,#68140,#68141,#68142,#68143,#68144,#68145,#68146,#68147,
#68148,#68149,#68150,#68151,#68152,#68153,#68154,#68155,#68156,#68157,#68158,
#68159,#68160,#68161,#68162,#68163,#68164,#68165,#68166,#68167,#68168,#68169,
#68170,#68171,#68172,#68173,#68174,#68175,#68176,#68177,#68178,#68179,#68180,
#68181,#68182,#68183,#68184,#68185,#68186,#68187,#68188,#68189,#68190,#68191,
#68192,#68193,#68194,#68195,#68196,#68197,#68198,#68199,#68200,#68201,#68202,
#68203,#68204,#68205,#68206,#68207,#68208,#68209,#68210,#68211,#68212,#68213,
#68214,#68215,#68216,#68217,#68218,#68219,#68220,#68221,#68222,#68223,#68224,
#68225,#68226,#68227,#68228,#68229,#68230,#68231,#68232,#68233,#68234,#68235,
#68236,#68237,#68238,#68239,#68240,#68241,#68242,#68243,#68244,#68245,#68246,
#68247,#68248,#68249,#68250,#68251,#68252,#68253,#68254,#68255,#68256,#68257,
#68258,#68259,#68260,#68261,#68262,#68263,#68264,#68265,#68266,#68267,#68268,
#68269,#68270,#68271,#68272,#68273,#68274,#68275,#68276,#68277,#68278,#68279,
#68280,#68281,#68282,#68283,#68284,#68285,#68286,#68287,#68288,#68289,#68290,
#68291,#68292,#68293,#68294,#68295,#68296,#68297,#68298,#68299,#68300,#68301,
#68302,#68303,#68304,#68305,#68306,#68307,#68308,#68309,#68310,#68311,#68312,
#68313,#68314,#68315,#68316,#68317,#68318,#68319)),.UNSPECIFIED.,.F.,.F.,
 .F.,(4,4),(4,1,1,1,1,1,1,1,1,1,1,1,1,1,1,1,1,1,1,1,1,1,1,1,1,1,1,1,1,1,
1,1,1,1,1,1,1,1,1,1,1,1,1,1,1,1,1,1,1,1,1,1,1,1,1,1,1,1,1,1,1,1,1,1,1,1,
1,1,1,1,1,1,1,1,1,1,1,1,1,1,1,1,1,1,1,1,1,1,1,1,1,1,1,1,1,1,1,1,1,1,1,1,
1,1,1,1,1,1,1,1,1,1,1,1,1,1,1,1,1,1,1,1,1,1,1,1,1,1,1,1,1,1,1,1,1,1,1,1,
1,1,1,1,1,1,1,1,1,1,1,1,1,1,1,1,1,1,1,1,1,1,1,1,1,1,1,1,1,1,1,1,1,1,1,1,
1,1,1,1,1,1,1,1,1,1,1,1,1,1,1,1,1,1,1,1,1,1,1,1,1,1,4),(0.,0.0820126057383863),
(11.6152142277549,12.614925558795,13.614636889835,14.6143482208751,15.6140595519151,
16.6137708829551,17.6134822139952,18.6131935450352,19.6129048760753,20.6126162071153,
21.6123275381553,22.6120388691954,23.6117502002354,24.6114615312754,25.6111728623155,
26.6108841933555,27.6105955243956,28.6103068554356,29.6100181864756,30.6097295175157,
31.6094408485557,32.6091521795958,33.6088635106358,34.6085748416758,35.6082861727159,
36.6079975037559,37.6077088347959,38.607420165836,39.607131496876,40.6068428279161,
41.6065541589561,42.6062654899961,43.6059768210362,44.6056881520762,45.6053994831162,
46.6051108141563,47.6048221451963,48.6045334762364,49.6042448072764,50.6039561383164,
51.6036674693565,52.6033788003965,53.6030901314366,54.6028014624766,55.6025127935166,
56.6022241245567,57.6019354555967,58.6016467866367,59.6013581176768,60.6010694487168,
61.6007807797569,62.6004921107969,63.6002034418369,64.599914772877,65.599626103917,
66.5993374349571,67.5990487659971,68.5987600970371,69.5984714280772,70.5981827591172,
71.5978940901573,72.5976054211973,73.5973167522373,74.5970280832774,75.5967394143174,
76.5964507453574,77.5961620763975,78.5958734074375,79.5955847384776,80.5952960695176,
81.5950074005576,82.5947187315977,83.5944300626377,84.5941413936777,85.5938527247178,
86.5935640557578,87.5932753867979,88.5929867178379,89.5926980488779,90.592409379918,
91.592120710958,92.5918320419981,93.5915433730381,94.5912547040781,95.5909660351182,
96.5906773661582,97.5903886971983,98.5901000282383,99.5898113592783,100.589522690318,
101.589234021358,102.588945352398,103.588656683438,104.588368014479,105.588079345519,
106.587790676559,107.587502007599,108.587213338639,109.586924669679,110.586636000719,
111.586347331759,112.586058662799,113.585769993839,114.585481324879,115.585192655919,
116.584903986959,117.584615317999,118.584326649039,119.584037980079,120.583749311119,
121.583460642159,122.583171973199,123.582883304239,124.582594635279,125.582305966319,
126.582017297359,127.581728628399,128.581439959439,129.581151290479,130.58086262152,
131.58057395256,132.5802852836,133.57999661464,134.57970794568,135.57941927672,
136.57913060776,137.5788419388,138.57855326984,139.57826460088,140.57797593192,
141.57768726296,142.577398594,143.57710992504,144.57682125608,145.57653258712,
146.57624391816,147.5759552492,148.57566658024,149.57537791128,150.57508924232,
151.57480057336,152.5745119044,153.57422323544,154.57393456648,155.57364589752,
156.57335722856,157.573068559601,158.572779890641,159.572491221681,160.572202552721,
161.571913883761,162.571625214801,163.571336545841,164.571047876881,165.570759207921,
166.570470538961,167.570181870001,168.569893201041,169.569604532081,170.569315863121,
171.569027194161,172.568738525201,173.568449856241,174.568161187281,175.567872518321,
176.567583849361,177.567295180401,178.567006511441,179.566717842481,180.566429173521,
181.566140504561,182.565851835602,183.565563166642,184.565274497682,185.564985828722,
186.564697159762,187.564408490802,188.564119821842,189.563831152882,190.563542483922,
191.563253814962,192.562965146002,193.562676477042,194.562387808082,195.562099139122,
196.561810470162,197.561521801202,198.561233132242,199.560944463282,200.560655794322,
201.560367125362,202.560078456402,203.559789787442,204.559501118482,205.559212449522,
206.558923780562,207.558635111602,208.558346442642,209.558057773683,210.557769104723,
211.557480435763),.UNSPECIFIED.);
#297=B_SPLINE_SURFACE_WITH_KNOTS('',3,3,((#68438,#68439,#68440,#68441,#68442,
#68443,#68444,#68445,#68446,#68447,#68448,#68449,#68450,#68451,#68452,#68453,
#68454,#68455,#68456,#68457,#68458,#68459,#68460,#68461,#68462,#68463,#68464,
#68465,#68466,#68467,#68468,#68469,#68470,#68471,#68472,#68473,#68474,#68475,
#68476,#68477,#68478,#68479,#68480,#68481,#68482,#68483,#68484,#68485,#68486,
#68487,#68488,#68489,#68490,#68491,#68492,#68493,#68494,#68495,#68496,#68497,
#68498,#68499,#68500,#68501,#68502,#68503,#68504,#68505,#68506,#68507,#68508,
#68509,#68510,#68511,#68512,#68513,#68514,#68515,#68516,#68517,#68518,#68519,
#68520,#68521,#68522,#68523,#68524,#68525,#68526,#68527,#68528,#68529,#68530,
#68531,#68532,#68533,#68534,#68535,#68536,#68537,#68538,#68539,#68540,#68541,
#68542,#68543,#68544,#68545,#68546,#68547,#68548,#68549,#68550,#68551,#68552,
#68553,#68554,#68555,#68556,#68557,#68558,#68559,#68560,#68561,#68562,#68563,
#68564,#68565,#68566,#68567,#68568,#68569,#68570,#68571,#68572,#68573,#68574,
#68575,#68576,#68577,#68578,#68579,#68580,#68581,#68582,#68583,#68584,#68585,
#68586,#68587,#68588,#68589,#68590,#68591,#68592,#68593,#68594,#68595,#68596,
#68597,#68598,#68599,#68600,#68601,#68602,#68603,#68604,#68605,#68606,#68607,
#68608,#68609,#68610,#68611,#68612,#68613,#68614,#68615,#68616,#68617,#68618,
#68619,#68620,#68621,#68622,#68623,#68624,#68625,#68626,#68627,#68628,#68629,
#68630,#68631,#68632,#68633,#68634,#68635,#68636,#68637,#68638,#68639,#68640,
#68641,#68642,#68643),(#68644,#68645,#68646,#68647,#68648,#68649,#68650,
#68651,#68652,#68653,#68654,#68655,#68656,#68657,#68658,#68659,#68660,#68661,
#68662,#68663,#68664,#68665,#68666,#68667,#68668,#68669,#68670,#68671,#68672,
#68673,#68674,#68675,#68676,#68677,#68678,#68679,#68680,#68681,#68682,#68683,
#68684,#68685,#68686,#68687,#68688,#68689,#68690,#68691,#68692,#68693,#68694,
#68695,#68696,#68697,#68698,#68699,#68700,#68701,#68702,#68703,#68704,#68705,
#68706,#68707,#68708,#68709,#68710,#68711,#68712,#68713,#68714,#68715,#68716,
#68717,#68718,#68719,#68720,#68721,#68722,#68723,#68724,#68725,#68726,#68727,
#68728,#68729,#68730,#68731,#68732,#68733,#68734,#68735,#68736,#68737,#68738,
#68739,#68740,#68741,#68742,#68743,#68744,#68745,#68746,#68747,#68748,#68749,
#68750,#68751,#68752,#68753,#68754,#68755,#68756,#68757,#68758,#68759,#68760,
#68761,#68762,#68763,#68764,#68765,#68766,#68767,#68768,#68769,#68770,#68771,
#68772,#68773,#68774,#68775,#68776,#68777,#68778,#68779,#68780,#68781,#68782,
#68783,#68784,#68785,#68786,#68787,#68788,#68789,#68790,#68791,#68792,#68793,
#68794,#68795,#68796,#68797,#68798,#68799,#68800,#68801,#68802,#68803,#68804,
#68805,#68806,#68807,#68808,#68809,#68810,#68811,#68812,#68813,#68814,#68815,
#68816,#68817,#68818,#68819,#68820,#68821,#68822,#68823,#68824,#68825,#68826,
#68827,#68828,#68829,#68830,#68831,#68832,#68833,#68834,#68835,#68836,#68837,
#68838,#68839,#68840,#68841,#68842,#68843,#68844,#68845,#68846,#68847,#68848,
#68849),(#68850,#68851,#68852,#68853,#68854,#68855,#68856,#68857,#68858,
#68859,#68860,#68861,#68862,#68863,#68864,#68865,#68866,#68867,#68868,#68869,
#68870,#68871,#68872,#68873,#68874,#68875,#68876,#68877,#68878,#68879,#68880,
#68881,#68882,#68883,#68884,#68885,#68886,#68887,#68888,#68889,#68890,#68891,
#68892,#68893,#68894,#68895,#68896,#68897,#68898,#68899,#68900,#68901,#68902,
#68903,#68904,#68905,#68906,#68907,#68908,#68909,#68910,#68911,#68912,#68913,
#68914,#68915,#68916,#68917,#68918,#68919,#68920,#68921,#68922,#68923,#68924,
#68925,#68926,#68927,#68928,#68929,#68930,#68931,#68932,#68933,#68934,#68935,
#68936,#68937,#68938,#68939,#68940,#68941,#68942,#68943,#68944,#68945,#68946,
#68947,#68948,#68949,#68950,#68951,#68952,#68953,#68954,#68955,#68956,#68957,
#68958,#68959,#68960,#68961,#68962,#68963,#68964,#68965,#68966,#68967,#68968,
#68969,#68970,#68971,#68972,#68973,#68974,#68975,#68976,#68977,#68978,#68979,
#68980,#68981,#68982,#68983,#68984,#68985,#68986,#68987,#68988,#68989,#68990,
#68991,#68992,#68993,#68994,#68995,#68996,#68997,#68998,#68999,#69000,#69001,
#69002,#69003,#69004,#69005,#69006,#69007,#69008,#69009,#69010,#69011,#69012,
#69013,#69014,#69015,#69016,#69017,#69018,#69019,#69020,#69021,#69022,#69023,
#69024,#69025,#69026,#69027,#69028,#69029,#69030,#69031,#69032,#69033,#69034,
#69035,#69036,#69037,#69038,#69039,#69040,#69041,#69042,#69043,#69044,#69045,
#69046,#69047,#69048,#69049,#69050,#69051,#69052,#69053,#69054,#69055),
(#69056,#69057,#69058,#69059,#69060,#69061,#69062,#69063,#69064,#69065,
#69066,#69067,#69068,#69069,#69070,#69071,#69072,#69073,#69074,#69075,#69076,
#69077,#69078,#69079,#69080,#69081,#69082,#69083,#69084,#69085,#69086,#69087,
#69088,#69089,#69090,#69091,#69092,#69093,#69094,#69095,#69096,#69097,#69098,
#69099,#69100,#69101,#69102,#69103,#69104,#69105,#69106,#69107,#69108,#69109,
#69110,#69111,#69112,#69113,#69114,#69115,#69116,#69117,#69118,#69119,#69120,
#69121,#69122,#69123,#69124,#69125,#69126,#69127,#69128,#69129,#69130,#69131,
#69132,#69133,#69134,#69135,#69136,#69137,#69138,#69139,#69140,#69141,#69142,
#69143,#69144,#69145,#69146,#69147,#69148,#69149,#69150,#69151,#69152,#69153,
#69154,#69155,#69156,#69157,#69158,#69159,#69160,#69161,#69162,#69163,#69164,
#69165,#69166,#69167,#69168,#69169,#69170,#69171,#69172,#69173,#69174,#69175,
#69176,#69177,#69178,#69179,#69180,#69181,#69182,#69183,#69184,#69185,#69186,
#69187,#69188,#69189,#69190,#69191,#69192,#69193,#69194,#69195,#69196,#69197,
#69198,#69199,#69200,#69201,#69202,#69203,#69204,#69205,#69206,#69207,#69208,
#69209,#69210,#69211,#69212,#69213,#69214,#69215,#69216,#69217,#69218,#69219,
#69220,#69221,#69222,#69223,#69224,#69225,#69226,#69227,#69228,#69229,#69230,
#69231,#69232,#69233,#69234,#69235,#69236,#69237,#69238,#69239,#69240,#69241,
#69242,#69243,#69244,#69245,#69246,#69247,#69248,#69249,#69250,#69251,#69252,
#69253,#69254,#69255,#69256,#69257,#69258,#69259,#69260,#69261)),
 .UNSPECIFIED.,.F.,.F.,.F.,(4,4),(4,1,1,1,1,1,1,1,1,1,1,1,1,1,1,1,1,1,1,
1,1,1,1,1,1,1,1,1,1,1,1,1,1,1,1,1,1,1,1,1,1,1,1,1,1,1,1,1,1,1,1,1,1,1,1,
1,1,1,1,1,1,1,1,1,1,1,1,1,1,1,1,1,1,1,1,1,1,1,1,1,1,1,1,1,1,1,1,1,1,1,1,
1,1,1,1,1,1,1,1,1,1,1,1,1,1,1,1,1,1,1,1,1,1,1,1,1,1,1,1,1,1,1,1,1,1,1,1,
1,1,1,1,1,1,1,1,1,1,1,1,1,1,1,1,1,1,1,1,1,1,1,1,1,1,1,1,1,1,1,1,1,1,1,1,
1,1,1,1,1,1,1,1,1,1,1,1,1,1,1,1,1,1,1,1,1,1,1,1,1,1,1,1,1,1,1,1,1,1,1,1,
1,1,1,1,4),(0.,0.0820126057383863),(8.31473274985819,9.30982372426964,10.3049146986811,
11.3000056730925,12.295096647504,13.2901876219154,14.2852785963269,15.2803695707383,
16.2754605451498,17.2705515195612,18.2656424939726,19.2607334683841,20.2558244427955,
21.250915417207,22.2460063916184,23.2410973660299,24.2361883404413,25.2312793148528,
26.2263702892642,27.2214612636757,28.2165522380871,29.2116432124985,30.20673418691,
31.2018251613214,32.1969161357329,33.1920071101443,34.1870980845558,35.1821890589672,
36.1772800333787,37.1723710077901,38.1674619822016,39.162552956613,40.1576439310244,
41.1527349054359,42.1478258798473,43.1429168542588,44.1380078286702,45.1330988030817,
46.1281897774931,47.1232807519046,48.118371726316,49.1134627007275,50.1085536751389,
51.1036446495503,52.0987356239618,53.0938265983732,54.0889175727847,55.0840085471961,
56.0790995216076,57.074190496019,58.0692814704305,59.0643724448419,60.0594634192534,
61.0545543936648,62.0496453680762,63.0447363424877,64.0398273168991,65.0349182913106,
66.030009265722,67.0251002401335,68.0201912145449,69.0152821889564,70.0103731633678,
71.0054641377792,72.0005551121907,72.9956460866021,73.9907370610136,74.985828035425,
75.9809190098365,76.9760099842479,77.9711009586594,78.9661919330708,79.9612829074823,
80.9563738818937,81.9514648563052,82.9465558307166,83.941646805128,84.9367377795395,
85.9318287539509,86.9269197283624,87.9220107027738,88.9171016771853,89.9121926515967,
90.9072836260082,91.9023746004196,92.897465574831,93.8925565492425,94.8876475236539,
95.8827384980654,96.8778294724768,97.8729204468883,98.8680114212997,99.8631023957112,
100.858193370123,101.853284344534,102.848375318946,103.843466293357,104.838557267768,
105.83364824218,106.828739216591,107.823830191003,108.818921165414,109.814012139826,
110.809103114237,111.804194088649,112.79928506306,113.794376037471,114.789467011883,
115.784557986294,116.779648960706,117.774739935117,118.769830909529,119.76492188394,
120.760012858352,121.755103832763,122.750194807174,123.745285781586,124.740376755997,
125.735467730409,126.73055870482,127.725649679232,128.720740653643,129.715831628055,
130.710922602466,131.706013576877,132.701104551289,133.6961955257,134.691286500112,
135.686377474523,136.681468448935,137.676559423346,138.671650397758,139.666741372169,
140.66183234658,141.656923320992,142.652014295403,143.647105269815,144.642196244226,
145.637287218638,146.632378193049,147.627469167461,148.622560141872,149.617651116283,
150.612742090695,151.607833065106,152.602924039518,153.598015013929,154.593105988341,
155.588196962752,156.583287937164,157.578378911575,158.573469885986,159.568560860398,
160.563651834809,161.558742809221,162.553833783632,163.548924758044,164.544015732455,
165.539106706867,166.534197681278,167.529288655689,168.524379630101,169.519470604512,
170.514561578924,171.509652553335,172.504743527747,173.499834502158,174.49492547657,
175.490016450981,176.485107425392,177.480198399804,178.475289374215,179.470380348627,
180.465471323038,181.46056229745,182.455653271861,183.450744246273,184.445835220684,
185.440926195095,186.436017169507,187.431108143918,188.42619911833,189.421290092741,
190.416381067153,191.411472041564,192.406563015976,193.401653990387,194.396744964798,
195.39183593921,196.386926913621,197.382017888033,198.377108862444,199.372199836856,
200.367290811267,201.362381785679,202.35747276009,203.352563734501,204.347654708913,
205.342745683324,206.337836657736,207.332927632147,208.328018606559,209.32310958097,
210.318200555382),.UNSPECIFIED.);
#298=FACE_BOUND('',#1449,.T.);
#299=FACE_BOUND('',#1452,.T.);
#300=FACE_BOUND('',#1455,.T.);
#301=FACE_BOUND('',#1458,.T.);
#302=FACE_BOUND('',#1507,.T.);
#303=FACE_BOUND('',#1508,.T.);
#304=FACE_BOUND('',#1513,.T.);
#305=FACE_BOUND('',#1514,.T.);
#306=FACE_BOUND('',#1518,.T.);
#307=FACE_BOUND('',#1520,.T.);
#308=FACE_BOUND('',#1528,.T.);
#309=FACE_BOUND('',#1542,.T.);
#310=FACE_BOUND('',#1543,.T.);
#311=FACE_BOUND('',#1550,.T.);
#312=FACE_BOUND('',#1551,.T.);
#313=FACE_BOUND('',#1559,.T.);
#314=FACE_BOUND('',#1575,.T.);
#315=FACE_BOUND('',#1577,.T.);
#316=FACE_BOUND('',#1578,.T.);
#317=FACE_BOUND('',#1579,.T.);
#318=FACE_BOUND('',#1580,.T.);
#319=FACE_BOUND('',#1581,.T.);
#320=FACE_BOUND('',#1582,.T.);
#321=FACE_BOUND('',#1583,.T.);
#322=FACE_BOUND('',#1584,.T.);
#323=FACE_BOUND('',#1585,.T.);
#324=FACE_BOUND('',#1586,.T.);
#325=FACE_BOUND('',#1587,.T.);
#326=FACE_BOUND('',#1588,.T.);
#327=FACE_BOUND('',#1589,.T.);
#328=FACE_BOUND('',#1728,.T.);
#329=FACE_BOUND('',#1732,.T.);
#330=FACE_BOUND('',#1733,.T.);
#331=FACE_BOUND('',#1734,.T.);
#332=FACE_BOUND('',#1735,.T.);
#333=FACE_BOUND('',#1736,.T.);
#334=FACE_BOUND('',#1738,.T.);
#335=FACE_BOUND('',#1739,.T.);
#336=FACE_BOUND('',#1740,.T.);
#337=FACE_BOUND('',#1741,.T.);
#338=FACE_BOUND('',#1742,.T.);
#339=FACE_BOUND('',#1743,.T.);
#340=FACE_BOUND('',#1744,.T.);
#341=FACE_BOUND('',#1745,.T.);
#342=FACE_BOUND('',#1746,.T.);
#343=FACE_BOUND('',#1808,.T.);
#344=FACE_BOUND('',#1820,.T.);
#345=FACE_BOUND('',#1827,.T.);
#346=FACE_BOUND('',#1832,.T.);
#347=FACE_BOUND('',#1835,.T.);
#348=FACE_BOUND('',#1836,.T.);
#349=FACE_BOUND('',#1849,.T.);
#350=FACE_BOUND('',#1850,.T.);
#351=FACE_BOUND('',#1933,.T.);
#352=FACE_BOUND('',#1935,.T.);
#353=FACE_BOUND('',#1943,.T.);
#354=FACE_BOUND('',#1946,.T.);
#355=FACE_BOUND('',#1957,.T.);
#356=FACE_BOUND('',#1959,.T.);
#357=FACE_BOUND('',#1963,.T.);
#358=FACE_BOUND('',#1965,.T.);
#359=FACE_BOUND('',#2057,.T.);
#360=FACE_BOUND('',#2060,.T.);
#361=FACE_BOUND('',#2065,.T.);
#362=FACE_BOUND('',#2067,.T.);
#363=FACE_BOUND('',#2146,.T.);
#364=FACE_BOUND('',#2149,.T.);
#365=PLANE('',#15061);
#366=PLANE('',#15066);
#367=PLANE('',#15071);
#368=PLANE('',#15076);
#369=PLANE('',#15086);
#370=PLANE('',#15089);
#371=PLANE('',#15092);
#372=PLANE('',#15095);
#373=PLANE('',#15098);
#374=PLANE('',#15101);
#375=PLANE('',#15104);
#376=PLANE('',#15107);
#377=PLANE('',#15110);
#378=PLANE('',#15111);
#379=PLANE('',#15112);
#380=PLANE('',#15113);
#381=PLANE('',#15115);
#382=PLANE('',#15116);
#383=PLANE('',#15117);
#384=PLANE('',#15118);
#385=PLANE('',#15120);
#386=PLANE('',#15122);
#387=PLANE('',#15123);
#388=PLANE('',#15126);
#389=PLANE('',#15129);
#390=PLANE('',#15130);
#391=PLANE('',#15131);
#392=PLANE('',#15133);
#393=PLANE('',#15134);
#394=PLANE('',#15135);
#395=PLANE('',#15136);
#396=PLANE('',#15139);
#397=PLANE('',#15140);
#398=PLANE('',#15141);
#399=PLANE('',#15142);
#400=PLANE('',#15149);
#401=PLANE('',#15150);
#402=PLANE('',#15151);
#403=PLANE('',#15152);
#404=PLANE('',#15153);
#405=PLANE('',#15154);
#406=PLANE('',#15155);
#407=PLANE('',#15156);
#408=PLANE('',#15159);
#409=PLANE('',#15160);
#410=PLANE('',#15161);
#411=PLANE('',#15162);
#412=PLANE('',#15163);
#413=PLANE('',#15164);
#414=PLANE('',#15166);
#415=PLANE('',#15167);
#416=PLANE('',#15168);
#417=PLANE('',#15172);
#418=PLANE('',#15173);
#419=PLANE('',#15174);
#420=PLANE('',#15175);
#421=PLANE('',#15176);
#422=PLANE('',#15177);
#423=PLANE('',#15178);
#424=PLANE('',#15179);
#425=PLANE('',#15180);
#426=PLANE('',#15181);
#427=PLANE('',#15182);
#428=PLANE('',#15183);
#429=PLANE('',#15184);
#430=PLANE('',#15185);
#431=PLANE('',#15186);
#432=PLANE('',#15187);
#433=PLANE('',#15191);
#434=PLANE('',#15192);
#435=PLANE('',#15330);
#436=PLANE('',#15333);
#437=PLANE('',#15336);
#438=PLANE('',#15339);
#439=PLANE('',#15342);
#440=PLANE('',#15343);
#441=PLANE('',#15344);
#442=PLANE('',#15345);
#443=PLANE('',#15346);
#444=PLANE('',#15349);
#445=PLANE('',#15352);
#446=PLANE('',#15355);
#447=PLANE('',#15361);
#448=PLANE('',#15368);
#449=PLANE('',#15369);
#450=PLANE('',#15433);
#451=PLANE('',#15435);
#452=PLANE('',#15436);
#453=PLANE('',#15437);
#454=PLANE('',#15438);
#455=PLANE('',#15439);
#456=PLANE('',#15440);
#457=PLANE('',#15441);
#458=PLANE('',#15442);
#459=PLANE('',#15443);
#460=PLANE('',#15444);
#461=PLANE('',#15445);
#462=PLANE('',#15459);
#463=PLANE('',#15461);
#464=PLANE('',#15462);
#465=PLANE('',#15463);
#466=PLANE('',#15464);
#467=PLANE('',#15469);
#468=PLANE('',#15471);
#469=PLANE('',#15472);
#470=PLANE('',#15473);
#471=PLANE('',#15474);
#472=PLANE('',#15475);
#473=PLANE('',#15476);
#474=PLANE('',#15477);
#475=PLANE('',#15478);
#476=PLANE('',#15479);
#477=PLANE('',#15480);
#478=PLANE('',#15481);
#479=PLANE('',#15561);
#480=PLANE('',#15562);
#481=PLANE('',#15563);
#482=PLANE('',#15564);
#483=PLANE('',#15565);
#484=PLANE('',#15566);
#485=PLANE('',#15567);
#486=PLANE('',#15571);
#487=PLANE('',#15572);
#488=PLANE('',#15576);
#489=PLANE('',#15580);
#490=PLANE('',#15584);
#491=PLANE('',#15585);
#492=PLANE('',#15587);
#493=PLANE('',#15588);
#494=PLANE('',#15589);
#495=PLANE('',#15596);
#496=PLANE('',#15604);
#497=PLANE('',#15605);
#498=PLANE('',#15613);
#499=PLANE('',#15614);
#500=PLANE('',#15702);
#501=PLANE('',#15703);
#502=PLANE('',#15704);
#503=PLANE('',#15705);
#504=PLANE('',#15706);
#505=PLANE('',#15707);
#506=PLANE('',#15708);
#507=PLANE('',#15709);
#508=PLANE('',#15713);
#509=PLANE('',#15714);
#510=PLANE('',#15722);
#511=PLANE('',#15723);
#512=PLANE('',#15800);
#513=PLANE('',#15801);
#514=PLANE('',#15802);
#515=PLANE('',#15803);
#516=PLANE('',#15804);
#517=PLANE('',#15805);
#518=PLANE('',#15806);
#519=PLANE('',#15807);
#520=PLANE('',#15811);
#521=PLANE('',#15812);
#522=FACE_OUTER_BOUND('',#1303,.T.);
#523=FACE_OUTER_BOUND('',#1304,.T.);
#524=FACE_OUTER_BOUND('',#1305,.T.);
#525=FACE_OUTER_BOUND('',#1306,.T.);
#526=FACE_OUTER_BOUND('',#1307,.T.);
#527=FACE_OUTER_BOUND('',#1308,.T.);
#528=FACE_OUTER_BOUND('',#1309,.T.);
#529=FACE_OUTER_BOUND('',#1310,.T.);
#530=FACE_OUTER_BOUND('',#1311,.T.);
#531=FACE_OUTER_BOUND('',#1312,.T.);
#532=FACE_OUTER_BOUND('',#1313,.T.);
#533=FACE_OUTER_BOUND('',#1314,.T.);
#534=FACE_OUTER_BOUND('',#1315,.T.);
#535=FACE_OUTER_BOUND('',#1316,.T.);
#536=FACE_OUTER_BOUND('',#1317,.T.);
#537=FACE_OUTER_BOUND('',#1318,.T.);
#538=FACE_OUTER_BOUND('',#1319,.T.);
#539=FACE_OUTER_BOUND('',#1320,.T.);
#540=FACE_OUTER_BOUND('',#1321,.T.);
#541=FACE_OUTER_BOUND('',#1322,.T.);
#542=FACE_OUTER_BOUND('',#1323,.T.);
#543=FACE_OUTER_BOUND('',#1324,.T.);
#544=FACE_OUTER_BOUND('',#1325,.T.);
#545=FACE_OUTER_BOUND('',#1326,.T.);
#546=FACE_OUTER_BOUND('',#1327,.T.);
#547=FACE_OUTER_BOUND('',#1328,.T.);
#548=FACE_OUTER_BOUND('',#1329,.T.);
#549=FACE_OUTER_BOUND('',#1330,.T.);
#550=FACE_OUTER_BOUND('',#1331,.T.);
#551=FACE_OUTER_BOUND('',#1332,.T.);
#552=FACE_OUTER_BOUND('',#1333,.T.);
#553=FACE_OUTER_BOUND('',#1334,.T.);
#554=FACE_OUTER_BOUND('',#1335,.T.);
#555=FACE_OUTER_BOUND('',#1336,.T.);
#556=FACE_OUTER_BOUND('',#1337,.T.);
#557=FACE_OUTER_BOUND('',#1338,.T.);
#558=FACE_OUTER_BOUND('',#1339,.T.);
#559=FACE_OUTER_BOUND('',#1340,.T.);
#560=FACE_OUTER_BOUND('',#1341,.T.);
#561=FACE_OUTER_BOUND('',#1342,.T.);
#562=FACE_OUTER_BOUND('',#1343,.T.);
#563=FACE_OUTER_BOUND('',#1344,.T.);
#564=FACE_OUTER_BOUND('',#1345,.T.);
#565=FACE_OUTER_BOUND('',#1346,.T.);
#566=FACE_OUTER_BOUND('',#1347,.T.);
#567=FACE_OUTER_BOUND('',#1348,.T.);
#568=FACE_OUTER_BOUND('',#1349,.T.);
#569=FACE_OUTER_BOUND('',#1350,.T.);
#570=FACE_OUTER_BOUND('',#1351,.T.);
#571=FACE_OUTER_BOUND('',#1352,.T.);
#572=FACE_OUTER_BOUND('',#1353,.T.);
#573=FACE_OUTER_BOUND('',#1354,.T.);
#574=FACE_OUTER_BOUND('',#1355,.T.);
#575=FACE_OUTER_BOUND('',#1356,.T.);
#576=FACE_OUTER_BOUND('',#1357,.T.);
#577=FACE_OUTER_BOUND('',#1358,.T.);
#578=FACE_OUTER_BOUND('',#1359,.T.);
#579=FACE_OUTER_BOUND('',#1360,.T.);
#580=FACE_OUTER_BOUND('',#1361,.T.);
#581=FACE_OUTER_BOUND('',#1362,.T.);
#582=FACE_OUTER_BOUND('',#1363,.T.);
#583=FACE_OUTER_BOUND('',#1364,.T.);
#584=FACE_OUTER_BOUND('',#1365,.T.);
#585=FACE_OUTER_BOUND('',#1366,.T.);
#586=FACE_OUTER_BOUND('',#1367,.T.);
#587=FACE_OUTER_BOUND('',#1368,.T.);
#588=FACE_OUTER_BOUND('',#1369,.T.);
#589=FACE_OUTER_BOUND('',#1370,.T.);
#590=FACE_OUTER_BOUND('',#1371,.T.);
#591=FACE_OUTER_BOUND('',#1372,.T.);
#592=FACE_OUTER_BOUND('',#1373,.T.);
#593=FACE_OUTER_BOUND('',#1374,.T.);
#594=FACE_OUTER_BOUND('',#1375,.T.);
#595=FACE_OUTER_BOUND('',#1376,.T.);
#596=FACE_OUTER_BOUND('',#1377,.T.);
#597=FACE_OUTER_BOUND('',#1378,.T.);
#598=FACE_OUTER_BOUND('',#1379,.T.);
#599=FACE_OUTER_BOUND('',#1380,.T.);
#600=FACE_OUTER_BOUND('',#1381,.T.);
#601=FACE_OUTER_BOUND('',#1382,.T.);
#602=FACE_OUTER_BOUND('',#1383,.T.);
#603=FACE_OUTER_BOUND('',#1384,.T.);
#604=FACE_OUTER_BOUND('',#1385,.T.);
#605=FACE_OUTER_BOUND('',#1386,.T.);
#606=FACE_OUTER_BOUND('',#1387,.T.);
#607=FACE_OUTER_BOUND('',#1388,.T.);
#608=FACE_OUTER_BOUND('',#1389,.T.);
#609=FACE_OUTER_BOUND('',#1390,.T.);
#610=FACE_OUTER_BOUND('',#1391,.T.);
#611=FACE_OUTER_BOUND('',#1392,.T.);
#612=FACE_OUTER_BOUND('',#1393,.T.);
#613=FACE_OUTER_BOUND('',#1394,.T.);
#614=FACE_OUTER_BOUND('',#1395,.T.);
#615=FACE_OUTER_BOUND('',#1396,.T.);
#616=FACE_OUTER_BOUND('',#1397,.T.);
#617=FACE_OUTER_BOUND('',#1398,.T.);
#618=FACE_OUTER_BOUND('',#1399,.T.);
#619=FACE_OUTER_BOUND('',#1400,.T.);
#620=FACE_OUTER_BOUND('',#1401,.T.);
#621=FACE_OUTER_BOUND('',#1402,.T.);
#622=FACE_OUTER_BOUND('',#1403,.T.);
#623=FACE_OUTER_BOUND('',#1404,.T.);
#624=FACE_OUTER_BOUND('',#1405,.T.);
#625=FACE_OUTER_BOUND('',#1406,.T.);
#626=FACE_OUTER_BOUND('',#1407,.T.);
#627=FACE_OUTER_BOUND('',#1408,.T.);
#628=FACE_OUTER_BOUND('',#1409,.T.);
#629=FACE_OUTER_BOUND('',#1410,.T.);
#630=FACE_OUTER_BOUND('',#1411,.T.);
#631=FACE_OUTER_BOUND('',#1412,.T.);
#632=FACE_OUTER_BOUND('',#1413,.T.);
#633=FACE_OUTER_BOUND('',#1414,.T.);
#634=FACE_OUTER_BOUND('',#1415,.T.);
#635=FACE_OUTER_BOUND('',#1416,.T.);
#636=FACE_OUTER_BOUND('',#1417,.T.);
#637=FACE_OUTER_BOUND('',#1418,.T.);
#638=FACE_OUTER_BOUND('',#1419,.T.);
#639=FACE_OUTER_BOUND('',#1420,.T.);
#640=FACE_OUTER_BOUND('',#1421,.T.);
#641=FACE_OUTER_BOUND('',#1422,.T.);
#642=FACE_OUTER_BOUND('',#1423,.T.);
#643=FACE_OUTER_BOUND('',#1424,.T.);
#644=FACE_OUTER_BOUND('',#1425,.T.);
#645=FACE_OUTER_BOUND('',#1426,.T.);
#646=FACE_OUTER_BOUND('',#1427,.T.);
#647=FACE_OUTER_BOUND('',#1428,.T.);
#648=FACE_OUTER_BOUND('',#1429,.T.);
#649=FACE_OUTER_BOUND('',#1430,.T.);
#650=FACE_OUTER_BOUND('',#1431,.T.);
#651=FACE_OUTER_BOUND('',#1432,.T.);
#652=FACE_OUTER_BOUND('',#1433,.T.);
#653=FACE_OUTER_BOUND('',#1434,.T.);
#654=FACE_OUTER_BOUND('',#1435,.T.);
#655=FACE_OUTER_BOUND('',#1436,.T.);
#656=FACE_OUTER_BOUND('',#1437,.T.);
#657=FACE_OUTER_BOUND('',#1438,.T.);
#658=FACE_OUTER_BOUND('',#1439,.T.);
#659=FACE_OUTER_BOUND('',#1440,.T.);
#660=FACE_OUTER_BOUND('',#1441,.T.);
#661=FACE_OUTER_BOUND('',#1442,.T.);
#662=FACE_OUTER_BOUND('',#1443,.T.);
#663=FACE_OUTER_BOUND('',#1444,.T.);
#664=FACE_OUTER_BOUND('',#1445,.T.);
#665=FACE_OUTER_BOUND('',#1446,.T.);
#666=FACE_OUTER_BOUND('',#1447,.T.);
#667=FACE_OUTER_BOUND('',#1448,.T.);
#668=FACE_OUTER_BOUND('',#1450,.T.);
#669=FACE_OUTER_BOUND('',#1451,.T.);
#670=FACE_OUTER_BOUND('',#1453,.T.);
#671=FACE_OUTER_BOUND('',#1454,.T.);
#672=FACE_OUTER_BOUND('',#1456,.T.);
#673=FACE_OUTER_BOUND('',#1457,.T.);
#674=FACE_OUTER_BOUND('',#1459,.T.);
#675=FACE_OUTER_BOUND('',#1460,.T.);
#676=FACE_OUTER_BOUND('',#1461,.T.);
#677=FACE_OUTER_BOUND('',#1462,.T.);
#678=FACE_OUTER_BOUND('',#1463,.T.);
#679=FACE_OUTER_BOUND('',#1464,.T.);
#680=FACE_OUTER_BOUND('',#1465,.T.);
#681=FACE_OUTER_BOUND('',#1466,.T.);
#682=FACE_OUTER_BOUND('',#1467,.T.);
#683=FACE_OUTER_BOUND('',#1468,.T.);
#684=FACE_OUTER_BOUND('',#1469,.T.);
#685=FACE_OUTER_BOUND('',#1470,.T.);
#686=FACE_OUTER_BOUND('',#1471,.T.);
#687=FACE_OUTER_BOUND('',#1472,.T.);
#688=FACE_OUTER_BOUND('',#1473,.T.);
#689=FACE_OUTER_BOUND('',#1474,.T.);
#690=FACE_OUTER_BOUND('',#1475,.T.);
#691=FACE_OUTER_BOUND('',#1476,.T.);
#692=FACE_OUTER_BOUND('',#1477,.T.);
#693=FACE_OUTER_BOUND('',#1478,.T.);
#694=FACE_OUTER_BOUND('',#1479,.T.);
#695=FACE_OUTER_BOUND('',#1480,.T.);
#696=FACE_OUTER_BOUND('',#1481,.T.);
#697=FACE_OUTER_BOUND('',#1482,.T.);
#698=FACE_OUTER_BOUND('',#1483,.T.);
#699=FACE_OUTER_BOUND('',#1484,.T.);
#700=FACE_OUTER_BOUND('',#1485,.T.);
#701=FACE_OUTER_BOUND('',#1486,.T.);
#702=FACE_OUTER_BOUND('',#1487,.T.);
#703=FACE_OUTER_BOUND('',#1488,.T.);
#704=FACE_OUTER_BOUND('',#1489,.T.);
#705=FACE_OUTER_BOUND('',#1490,.T.);
#706=FACE_OUTER_BOUND('',#1491,.T.);
#707=FACE_OUTER_BOUND('',#1492,.T.);
#708=FACE_OUTER_BOUND('',#1493,.T.);
#709=FACE_OUTER_BOUND('',#1494,.T.);
#710=FACE_OUTER_BOUND('',#1495,.T.);
#711=FACE_OUTER_BOUND('',#1496,.T.);
#712=FACE_OUTER_BOUND('',#1497,.T.);
#713=FACE_OUTER_BOUND('',#1498,.T.);
#714=FACE_OUTER_BOUND('',#1499,.T.);
#715=FACE_OUTER_BOUND('',#1500,.T.);
#716=FACE_OUTER_BOUND('',#1501,.T.);
#717=FACE_OUTER_BOUND('',#1502,.T.);
#718=FACE_OUTER_BOUND('',#1503,.T.);
#719=FACE_OUTER_BOUND('',#1504,.T.);
#720=FACE_OUTER_BOUND('',#1505,.T.);
#721=FACE_OUTER_BOUND('',#1506,.T.);
#722=FACE_OUTER_BOUND('',#1509,.T.);
#723=FACE_OUTER_BOUND('',#1510,.T.);
#724=FACE_OUTER_BOUND('',#1511,.T.);
#725=FACE_OUTER_BOUND('',#1512,.T.);
#726=FACE_OUTER_BOUND('',#1515,.T.);
#727=FACE_OUTER_BOUND('',#1516,.T.);
#728=FACE_OUTER_BOUND('',#1517,.T.);
#729=FACE_OUTER_BOUND('',#1519,.T.);
#730=FACE_OUTER_BOUND('',#1521,.T.);
#731=FACE_OUTER_BOUND('',#1522,.T.);
#732=FACE_OUTER_BOUND('',#1523,.T.);
#733=FACE_OUTER_BOUND('',#1524,.T.);
#734=FACE_OUTER_BOUND('',#1525,.T.);
#735=FACE_OUTER_BOUND('',#1526,.T.);
#736=FACE_OUTER_BOUND('',#1527,.T.);
#737=FACE_OUTER_BOUND('',#1529,.T.);
#738=FACE_OUTER_BOUND('',#1530,.T.);
#739=FACE_OUTER_BOUND('',#1531,.T.);
#740=FACE_OUTER_BOUND('',#1532,.T.);
#741=FACE_OUTER_BOUND('',#1533,.T.);
#742=FACE_OUTER_BOUND('',#1534,.T.);
#743=FACE_OUTER_BOUND('',#1535,.T.);
#744=FACE_OUTER_BOUND('',#1536,.T.);
#745=FACE_OUTER_BOUND('',#1537,.T.);
#746=FACE_OUTER_BOUND('',#1538,.T.);
#747=FACE_OUTER_BOUND('',#1539,.T.);
#748=FACE_OUTER_BOUND('',#1540,.T.);
#749=FACE_OUTER_BOUND('',#1541,.T.);
#750=FACE_OUTER_BOUND('',#1544,.T.);
#751=FACE_OUTER_BOUND('',#1545,.T.);
#752=FACE_OUTER_BOUND('',#1546,.T.);
#753=FACE_OUTER_BOUND('',#1547,.T.);
#754=FACE_OUTER_BOUND('',#1548,.T.);
#755=FACE_OUTER_BOUND('',#1549,.T.);
#756=FACE_OUTER_BOUND('',#1552,.T.);
#757=FACE_OUTER_BOUND('',#1553,.T.);
#758=FACE_OUTER_BOUND('',#1554,.T.);
#759=FACE_OUTER_BOUND('',#1555,.T.);
#760=FACE_OUTER_BOUND('',#1556,.T.);
#761=FACE_OUTER_BOUND('',#1557,.T.);
#762=FACE_OUTER_BOUND('',#1558,.T.);
#763=FACE_OUTER_BOUND('',#1560,.T.);
#764=FACE_OUTER_BOUND('',#1561,.T.);
#765=FACE_OUTER_BOUND('',#1562,.T.);
#766=FACE_OUTER_BOUND('',#1563,.T.);
#767=FACE_OUTER_BOUND('',#1564,.T.);
#768=FACE_OUTER_BOUND('',#1565,.T.);
#769=FACE_OUTER_BOUND('',#1566,.T.);
#770=FACE_OUTER_BOUND('',#1567,.T.);
#771=FACE_OUTER_BOUND('',#1568,.T.);
#772=FACE_OUTER_BOUND('',#1569,.T.);
#773=FACE_OUTER_BOUND('',#1570,.T.);
#774=FACE_OUTER_BOUND('',#1571,.T.);
#775=FACE_OUTER_BOUND('',#1572,.T.);
#776=FACE_OUTER_BOUND('',#1573,.T.);
#777=FACE_OUTER_BOUND('',#1574,.T.);
#778=FACE_OUTER_BOUND('',#1576,.T.);
#779=FACE_OUTER_BOUND('',#1590,.T.);
#780=FACE_OUTER_BOUND('',#1591,.T.);
#781=FACE_OUTER_BOUND('',#1592,.T.);
#782=FACE_OUTER_BOUND('',#1593,.T.);
#783=FACE_OUTER_BOUND('',#1594,.T.);
#784=FACE_OUTER_BOUND('',#1595,.T.);
#785=FACE_OUTER_BOUND('',#1596,.T.);
#786=FACE_OUTER_BOUND('',#1597,.T.);
#787=FACE_OUTER_BOUND('',#1598,.T.);
#788=FACE_OUTER_BOUND('',#1599,.T.);
#789=FACE_OUTER_BOUND('',#1600,.T.);
#790=FACE_OUTER_BOUND('',#1601,.T.);
#791=FACE_OUTER_BOUND('',#1602,.T.);
#792=FACE_OUTER_BOUND('',#1603,.T.);
#793=FACE_OUTER_BOUND('',#1604,.T.);
#794=FACE_OUTER_BOUND('',#1605,.T.);
#795=FACE_OUTER_BOUND('',#1606,.T.);
#796=FACE_OUTER_BOUND('',#1607,.T.);
#797=FACE_OUTER_BOUND('',#1608,.T.);
#798=FACE_OUTER_BOUND('',#1609,.T.);
#799=FACE_OUTER_BOUND('',#1610,.T.);
#800=FACE_OUTER_BOUND('',#1611,.T.);
#801=FACE_OUTER_BOUND('',#1612,.T.);
#802=FACE_OUTER_BOUND('',#1613,.T.);
#803=FACE_OUTER_BOUND('',#1614,.T.);
#804=FACE_OUTER_BOUND('',#1615,.T.);
#805=FACE_OUTER_BOUND('',#1616,.T.);
#806=FACE_OUTER_BOUND('',#1617,.T.);
#807=FACE_OUTER_BOUND('',#1618,.T.);
#808=FACE_OUTER_BOUND('',#1619,.T.);
#809=FACE_OUTER_BOUND('',#1620,.T.);
#810=FACE_OUTER_BOUND('',#1621,.T.);
#811=FACE_OUTER_BOUND('',#1622,.T.);
#812=FACE_OUTER_BOUND('',#1623,.T.);
#813=FACE_OUTER_BOUND('',#1624,.T.);
#814=FACE_OUTER_BOUND('',#1625,.T.);
#815=FACE_OUTER_BOUND('',#1626,.T.);
#816=FACE_OUTER_BOUND('',#1627,.T.);
#817=FACE_OUTER_BOUND('',#1628,.T.);
#818=FACE_OUTER_BOUND('',#1629,.T.);
#819=FACE_OUTER_BOUND('',#1630,.T.);
#820=FACE_OUTER_BOUND('',#1631,.T.);
#821=FACE_OUTER_BOUND('',#1632,.T.);
#822=FACE_OUTER_BOUND('',#1633,.T.);
#823=FACE_OUTER_BOUND('',#1634,.T.);
#824=FACE_OUTER_BOUND('',#1635,.T.);
#825=FACE_OUTER_BOUND('',#1636,.T.);
#826=FACE_OUTER_BOUND('',#1637,.T.);
#827=FACE_OUTER_BOUND('',#1638,.T.);
#828=FACE_OUTER_BOUND('',#1639,.T.);
#829=FACE_OUTER_BOUND('',#1640,.T.);
#830=FACE_OUTER_BOUND('',#1641,.T.);
#831=FACE_OUTER_BOUND('',#1642,.T.);
#832=FACE_OUTER_BOUND('',#1643,.T.);
#833=FACE_OUTER_BOUND('',#1644,.T.);
#834=FACE_OUTER_BOUND('',#1645,.T.);
#835=FACE_OUTER_BOUND('',#1646,.T.);
#836=FACE_OUTER_BOUND('',#1647,.T.);
#837=FACE_OUTER_BOUND('',#1648,.T.);
#838=FACE_OUTER_BOUND('',#1649,.T.);
#839=FACE_OUTER_BOUND('',#1650,.T.);
#840=FACE_OUTER_BOUND('',#1651,.T.);
#841=FACE_OUTER_BOUND('',#1652,.T.);
#842=FACE_OUTER_BOUND('',#1653,.T.);
#843=FACE_OUTER_BOUND('',#1654,.T.);
#844=FACE_OUTER_BOUND('',#1655,.T.);
#845=FACE_OUTER_BOUND('',#1656,.T.);
#846=FACE_OUTER_BOUND('',#1657,.T.);
#847=FACE_OUTER_BOUND('',#1658,.T.);
#848=FACE_OUTER_BOUND('',#1659,.T.);
#849=FACE_OUTER_BOUND('',#1660,.T.);
#850=FACE_OUTER_BOUND('',#1661,.T.);
#851=FACE_OUTER_BOUND('',#1662,.T.);
#852=FACE_OUTER_BOUND('',#1663,.T.);
#853=FACE_OUTER_BOUND('',#1664,.T.);
#854=FACE_OUTER_BOUND('',#1665,.T.);
#855=FACE_OUTER_BOUND('',#1666,.T.);
#856=FACE_OUTER_BOUND('',#1667,.T.);
#857=FACE_OUTER_BOUND('',#1668,.T.);
#858=FACE_OUTER_BOUND('',#1669,.T.);
#859=FACE_OUTER_BOUND('',#1670,.T.);
#860=FACE_OUTER_BOUND('',#1671,.T.);
#861=FACE_OUTER_BOUND('',#1672,.T.);
#862=FACE_OUTER_BOUND('',#1673,.T.);
#863=FACE_OUTER_BOUND('',#1674,.T.);
#864=FACE_OUTER_BOUND('',#1675,.T.);
#865=FACE_OUTER_BOUND('',#1676,.T.);
#866=FACE_OUTER_BOUND('',#1677,.T.);
#867=FACE_OUTER_BOUND('',#1678,.T.);
#868=FACE_OUTER_BOUND('',#1679,.T.);
#869=FACE_OUTER_BOUND('',#1680,.T.);
#870=FACE_OUTER_BOUND('',#1681,.T.);
#871=FACE_OUTER_BOUND('',#1682,.T.);
#872=FACE_OUTER_BOUND('',#1683,.T.);
#873=FACE_OUTER_BOUND('',#1684,.T.);
#874=FACE_OUTER_BOUND('',#1685,.T.);
#875=FACE_OUTER_BOUND('',#1686,.T.);
#876=FACE_OUTER_BOUND('',#1687,.T.);
#877=FACE_OUTER_BOUND('',#1688,.T.);
#878=FACE_OUTER_BOUND('',#1689,.T.);
#879=FACE_OUTER_BOUND('',#1690,.T.);
#880=FACE_OUTER_BOUND('',#1691,.T.);
#881=FACE_OUTER_BOUND('',#1692,.T.);
#882=FACE_OUTER_BOUND('',#1693,.T.);
#883=FACE_OUTER_BOUND('',#1694,.T.);
#884=FACE_OUTER_BOUND('',#1695,.T.);
#885=FACE_OUTER_BOUND('',#1696,.T.);
#886=FACE_OUTER_BOUND('',#1697,.T.);
#887=FACE_OUTER_BOUND('',#1698,.T.);
#888=FACE_OUTER_BOUND('',#1699,.T.);
#889=FACE_OUTER_BOUND('',#1700,.T.);
#890=FACE_OUTER_BOUND('',#1701,.T.);
#891=FACE_OUTER_BOUND('',#1702,.T.);
#892=FACE_OUTER_BOUND('',#1703,.T.);
#893=FACE_OUTER_BOUND('',#1704,.T.);
#894=FACE_OUTER_BOUND('',#1705,.T.);
#895=FACE_OUTER_BOUND('',#1706,.T.);
#896=FACE_OUTER_BOUND('',#1707,.T.);
#897=FACE_OUTER_BOUND('',#1708,.T.);
#898=FACE_OUTER_BOUND('',#1709,.T.);
#899=FACE_OUTER_BOUND('',#1710,.T.);
#900=FACE_OUTER_BOUND('',#1711,.T.);
#901=FACE_OUTER_BOUND('',#1712,.T.);
#902=FACE_OUTER_BOUND('',#1713,.T.);
#903=FACE_OUTER_BOUND('',#1714,.T.);
#904=FACE_OUTER_BOUND('',#1715,.T.);
#905=FACE_OUTER_BOUND('',#1716,.T.);
#906=FACE_OUTER_BOUND('',#1717,.T.);
#907=FACE_OUTER_BOUND('',#1718,.T.);
#908=FACE_OUTER_BOUND('',#1719,.T.);
#909=FACE_OUTER_BOUND('',#1720,.T.);
#910=FACE_OUTER_BOUND('',#1721,.T.);
#911=FACE_OUTER_BOUND('',#1722,.T.);
#912=FACE_OUTER_BOUND('',#1723,.T.);
#913=FACE_OUTER_BOUND('',#1724,.T.);
#914=FACE_OUTER_BOUND('',#1725,.T.);
#915=FACE_OUTER_BOUND('',#1726,.T.);
#916=FACE_OUTER_BOUND('',#1727,.T.);
#917=FACE_OUTER_BOUND('',#1729,.T.);
#918=FACE_OUTER_BOUND('',#1730,.T.);
#919=FACE_OUTER_BOUND('',#1731,.T.);
#920=FACE_OUTER_BOUND('',#1737,.T.);
#921=FACE_OUTER_BOUND('',#1747,.T.);
#922=FACE_OUTER_BOUND('',#1748,.T.);
#923=FACE_OUTER_BOUND('',#1749,.T.);
#924=FACE_OUTER_BOUND('',#1750,.T.);
#925=FACE_OUTER_BOUND('',#1751,.T.);
#926=FACE_OUTER_BOUND('',#1752,.T.);
#927=FACE_OUTER_BOUND('',#1753,.T.);
#928=FACE_OUTER_BOUND('',#1754,.T.);
#929=FACE_OUTER_BOUND('',#1755,.T.);
#930=FACE_OUTER_BOUND('',#1756,.T.);
#931=FACE_OUTER_BOUND('',#1757,.T.);
#932=FACE_OUTER_BOUND('',#1758,.T.);
#933=FACE_OUTER_BOUND('',#1759,.T.);
#934=FACE_OUTER_BOUND('',#1760,.T.);
#935=FACE_OUTER_BOUND('',#1761,.T.);
#936=FACE_OUTER_BOUND('',#1762,.T.);
#937=FACE_OUTER_BOUND('',#1763,.T.);
#938=FACE_OUTER_BOUND('',#1764,.T.);
#939=FACE_OUTER_BOUND('',#1765,.T.);
#940=FACE_OUTER_BOUND('',#1766,.T.);
#941=FACE_OUTER_BOUND('',#1767,.T.);
#942=FACE_OUTER_BOUND('',#1768,.T.);
#943=FACE_OUTER_BOUND('',#1769,.T.);
#944=FACE_OUTER_BOUND('',#1770,.T.);
#945=FACE_OUTER_BOUND('',#1771,.T.);
#946=FACE_OUTER_BOUND('',#1772,.T.);
#947=FACE_OUTER_BOUND('',#1773,.T.);
#948=FACE_OUTER_BOUND('',#1774,.T.);
#949=FACE_OUTER_BOUND('',#1775,.T.);
#950=FACE_OUTER_BOUND('',#1776,.T.);
#951=FACE_OUTER_BOUND('',#1777,.T.);
#952=FACE_OUTER_BOUND('',#1778,.T.);
#953=FACE_OUTER_BOUND('',#1779,.T.);
#954=FACE_OUTER_BOUND('',#1780,.T.);
#955=FACE_OUTER_BOUND('',#1781,.T.);
#956=FACE_OUTER_BOUND('',#1782,.T.);
#957=FACE_OUTER_BOUND('',#1783,.T.);
#958=FACE_OUTER_BOUND('',#1784,.T.);
#959=FACE_OUTER_BOUND('',#1785,.T.);
#960=FACE_OUTER_BOUND('',#1786,.T.);
#961=FACE_OUTER_BOUND('',#1787,.T.);
#962=FACE_OUTER_BOUND('',#1788,.T.);
#963=FACE_OUTER_BOUND('',#1789,.T.);
#964=FACE_OUTER_BOUND('',#1790,.T.);
#965=FACE_OUTER_BOUND('',#1791,.T.);
#966=FACE_OUTER_BOUND('',#1792,.T.);
#967=FACE_OUTER_BOUND('',#1793,.T.);
#968=FACE_OUTER_BOUND('',#1794,.T.);
#969=FACE_OUTER_BOUND('',#1795,.T.);
#970=FACE_OUTER_BOUND('',#1796,.T.);
#971=FACE_OUTER_BOUND('',#1797,.T.);
#972=FACE_OUTER_BOUND('',#1798,.T.);
#973=FACE_OUTER_BOUND('',#1799,.T.);
#974=FACE_OUTER_BOUND('',#1800,.T.);
#975=FACE_OUTER_BOUND('',#1801,.T.);
#976=FACE_OUTER_BOUND('',#1802,.T.);
#977=FACE_OUTER_BOUND('',#1803,.T.);
#978=FACE_OUTER_BOUND('',#1804,.T.);
#979=FACE_OUTER_BOUND('',#1805,.T.);
#980=FACE_OUTER_BOUND('',#1806,.T.);
#981=FACE_OUTER_BOUND('',#1807,.T.);
#982=FACE_OUTER_BOUND('',#1809,.T.);
#983=FACE_OUTER_BOUND('',#1810,.T.);
#984=FACE_OUTER_BOUND('',#1811,.T.);
#985=FACE_OUTER_BOUND('',#1812,.T.);
#986=FACE_OUTER_BOUND('',#1813,.T.);
#987=FACE_OUTER_BOUND('',#1814,.T.);
#988=FACE_OUTER_BOUND('',#1815,.T.);
#989=FACE_OUTER_BOUND('',#1816,.T.);
#990=FACE_OUTER_BOUND('',#1817,.T.);
#991=FACE_OUTER_BOUND('',#1818,.T.);
#992=FACE_OUTER_BOUND('',#1819,.T.);
#993=FACE_OUTER_BOUND('',#1821,.T.);
#994=FACE_OUTER_BOUND('',#1822,.T.);
#995=FACE_OUTER_BOUND('',#1823,.T.);
#996=FACE_OUTER_BOUND('',#1824,.T.);
#997=FACE_OUTER_BOUND('',#1825,.T.);
#998=FACE_OUTER_BOUND('',#1826,.T.);
#999=FACE_OUTER_BOUND('',#1828,.T.);
#1000=FACE_OUTER_BOUND('',#1829,.T.);
#1001=FACE_OUTER_BOUND('',#1830,.T.);
#1002=FACE_OUTER_BOUND('',#1831,.T.);
#1003=FACE_OUTER_BOUND('',#1833,.T.);
#1004=FACE_OUTER_BOUND('',#1834,.T.);
#1005=FACE_OUTER_BOUND('',#1837,.T.);
#1006=FACE_OUTER_BOUND('',#1838,.T.);
#1007=FACE_OUTER_BOUND('',#1839,.T.);
#1008=FACE_OUTER_BOUND('',#1840,.T.);
#1009=FACE_OUTER_BOUND('',#1841,.T.);
#1010=FACE_OUTER_BOUND('',#1842,.T.);
#1011=FACE_OUTER_BOUND('',#1843,.T.);
#1012=FACE_OUTER_BOUND('',#1844,.T.);
#1013=FACE_OUTER_BOUND('',#1845,.T.);
#1014=FACE_OUTER_BOUND('',#1846,.T.);
#1015=FACE_OUTER_BOUND('',#1847,.T.);
#1016=FACE_OUTER_BOUND('',#1848,.T.);
#1017=FACE_OUTER_BOUND('',#1851,.T.);
#1018=FACE_OUTER_BOUND('',#1852,.T.);
#1019=FACE_OUTER_BOUND('',#1853,.T.);
#1020=FACE_OUTER_BOUND('',#1854,.T.);
#1021=FACE_OUTER_BOUND('',#1855,.T.);
#1022=FACE_OUTER_BOUND('',#1856,.T.);
#1023=FACE_OUTER_BOUND('',#1857,.T.);
#1024=FACE_OUTER_BOUND('',#1858,.T.);
#1025=FACE_OUTER_BOUND('',#1859,.T.);
#1026=FACE_OUTER_BOUND('',#1860,.T.);
#1027=FACE_OUTER_BOUND('',#1861,.T.);
#1028=FACE_OUTER_BOUND('',#1862,.T.);
#1029=FACE_OUTER_BOUND('',#1863,.T.);
#1030=FACE_OUTER_BOUND('',#1864,.T.);
#1031=FACE_OUTER_BOUND('',#1865,.T.);
#1032=FACE_OUTER_BOUND('',#1866,.T.);
#1033=FACE_OUTER_BOUND('',#1867,.T.);
#1034=FACE_OUTER_BOUND('',#1868,.T.);
#1035=FACE_OUTER_BOUND('',#1869,.T.);
#1036=FACE_OUTER_BOUND('',#1870,.T.);
#1037=FACE_OUTER_BOUND('',#1871,.T.);
#1038=FACE_OUTER_BOUND('',#1872,.T.);
#1039=FACE_OUTER_BOUND('',#1873,.T.);
#1040=FACE_OUTER_BOUND('',#1874,.T.);
#1041=FACE_OUTER_BOUND('',#1875,.T.);
#1042=FACE_OUTER_BOUND('',#1876,.T.);
#1043=FACE_OUTER_BOUND('',#1877,.T.);
#1044=FACE_OUTER_BOUND('',#1878,.T.);
#1045=FACE_OUTER_BOUND('',#1879,.T.);
#1046=FACE_OUTER_BOUND('',#1880,.T.);
#1047=FACE_OUTER_BOUND('',#1881,.T.);
#1048=FACE_OUTER_BOUND('',#1882,.T.);
#1049=FACE_OUTER_BOUND('',#1883,.T.);
#1050=FACE_OUTER_BOUND('',#1884,.T.);
#1051=FACE_OUTER_BOUND('',#1885,.T.);
#1052=FACE_OUTER_BOUND('',#1886,.T.);
#1053=FACE_OUTER_BOUND('',#1887,.T.);
#1054=FACE_OUTER_BOUND('',#1888,.T.);
#1055=FACE_OUTER_BOUND('',#1889,.T.);
#1056=FACE_OUTER_BOUND('',#1890,.T.);
#1057=FACE_OUTER_BOUND('',#1891,.T.);
#1058=FACE_OUTER_BOUND('',#1892,.T.);
#1059=FACE_OUTER_BOUND('',#1893,.T.);
#1060=FACE_OUTER_BOUND('',#1894,.T.);
#1061=FACE_OUTER_BOUND('',#1895,.T.);
#1062=FACE_OUTER_BOUND('',#1896,.T.);
#1063=FACE_OUTER_BOUND('',#1897,.T.);
#1064=FACE_OUTER_BOUND('',#1898,.T.);
#1065=FACE_OUTER_BOUND('',#1899,.T.);
#1066=FACE_OUTER_BOUND('',#1900,.T.);
#1067=FACE_OUTER_BOUND('',#1901,.T.);
#1068=FACE_OUTER_BOUND('',#1902,.T.);
#1069=FACE_OUTER_BOUND('',#1903,.T.);
#1070=FACE_OUTER_BOUND('',#1904,.T.);
#1071=FACE_OUTER_BOUND('',#1905,.T.);
#1072=FACE_OUTER_BOUND('',#1906,.T.);
#1073=FACE_OUTER_BOUND('',#1907,.T.);
#1074=FACE_OUTER_BOUND('',#1908,.T.);
#1075=FACE_OUTER_BOUND('',#1909,.T.);
#1076=FACE_OUTER_BOUND('',#1910,.T.);
#1077=FACE_OUTER_BOUND('',#1911,.T.);
#1078=FACE_OUTER_BOUND('',#1912,.T.);
#1079=FACE_OUTER_BOUND('',#1913,.T.);
#1080=FACE_OUTER_BOUND('',#1914,.T.);
#1081=FACE_OUTER_BOUND('',#1915,.T.);
#1082=FACE_OUTER_BOUND('',#1916,.T.);
#1083=FACE_OUTER_BOUND('',#1917,.T.);
#1084=FACE_OUTER_BOUND('',#1918,.T.);
#1085=FACE_OUTER_BOUND('',#1919,.T.);
#1086=FACE_OUTER_BOUND('',#1920,.T.);
#1087=FACE_OUTER_BOUND('',#1921,.T.);
#1088=FACE_OUTER_BOUND('',#1922,.T.);
#1089=FACE_OUTER_BOUND('',#1923,.T.);
#1090=FACE_OUTER_BOUND('',#1924,.T.);
#1091=FACE_OUTER_BOUND('',#1925,.T.);
#1092=FACE_OUTER_BOUND('',#1926,.T.);
#1093=FACE_OUTER_BOUND('',#1927,.T.);
#1094=FACE_OUTER_BOUND('',#1928,.T.);
#1095=FACE_OUTER_BOUND('',#1929,.T.);
#1096=FACE_OUTER_BOUND('',#1930,.T.);
#1097=FACE_OUTER_BOUND('',#1931,.T.);
#1098=FACE_OUTER_BOUND('',#1932,.T.);
#1099=FACE_OUTER_BOUND('',#1934,.T.);
#1100=FACE_OUTER_BOUND('',#1936,.T.);
#1101=FACE_OUTER_BOUND('',#1937,.T.);
#1102=FACE_OUTER_BOUND('',#1938,.T.);
#1103=FACE_OUTER_BOUND('',#1939,.T.);
#1104=FACE_OUTER_BOUND('',#1940,.T.);
#1105=FACE_OUTER_BOUND('',#1941,.T.);
#1106=FACE_OUTER_BOUND('',#1942,.T.);
#1107=FACE_OUTER_BOUND('',#1944,.T.);
#1108=FACE_OUTER_BOUND('',#1945,.T.);
#1109=FACE_OUTER_BOUND('',#1947,.T.);
#1110=FACE_OUTER_BOUND('',#1948,.T.);
#1111=FACE_OUTER_BOUND('',#1949,.T.);
#1112=FACE_OUTER_BOUND('',#1950,.T.);
#1113=FACE_OUTER_BOUND('',#1951,.T.);
#1114=FACE_OUTER_BOUND('',#1952,.T.);
#1115=FACE_OUTER_BOUND('',#1953,.T.);
#1116=FACE_OUTER_BOUND('',#1954,.T.);
#1117=FACE_OUTER_BOUND('',#1955,.T.);
#1118=FACE_OUTER_BOUND('',#1956,.T.);
#1119=FACE_OUTER_BOUND('',#1958,.T.);
#1120=FACE_OUTER_BOUND('',#1960,.T.);
#1121=FACE_OUTER_BOUND('',#1961,.T.);
#1122=FACE_OUTER_BOUND('',#1962,.T.);
#1123=FACE_OUTER_BOUND('',#1964,.T.);
#1124=FACE_OUTER_BOUND('',#1966,.T.);
#1125=FACE_OUTER_BOUND('',#1967,.T.);
#1126=FACE_OUTER_BOUND('',#1968,.T.);
#1127=FACE_OUTER_BOUND('',#1969,.T.);
#1128=FACE_OUTER_BOUND('',#1970,.T.);
#1129=FACE_OUTER_BOUND('',#1971,.T.);
#1130=FACE_OUTER_BOUND('',#1972,.T.);
#1131=FACE_OUTER_BOUND('',#1973,.T.);
#1132=FACE_OUTER_BOUND('',#1974,.T.);
#1133=FACE_OUTER_BOUND('',#1975,.T.);
#1134=FACE_OUTER_BOUND('',#1976,.T.);
#1135=FACE_OUTER_BOUND('',#1977,.T.);
#1136=FACE_OUTER_BOUND('',#1978,.T.);
#1137=FACE_OUTER_BOUND('',#1979,.T.);
#1138=FACE_OUTER_BOUND('',#1980,.T.);
#1139=FACE_OUTER_BOUND('',#1981,.T.);
#1140=FACE_OUTER_BOUND('',#1982,.T.);
#1141=FACE_OUTER_BOUND('',#1983,.T.);
#1142=FACE_OUTER_BOUND('',#1984,.T.);
#1143=FACE_OUTER_BOUND('',#1985,.T.);
#1144=FACE_OUTER_BOUND('',#1986,.T.);
#1145=FACE_OUTER_BOUND('',#1987,.T.);
#1146=FACE_OUTER_BOUND('',#1988,.T.);
#1147=FACE_OUTER_BOUND('',#1989,.T.);
#1148=FACE_OUTER_BOUND('',#1990,.T.);
#1149=FACE_OUTER_BOUND('',#1991,.T.);
#1150=FACE_OUTER_BOUND('',#1992,.T.);
#1151=FACE_OUTER_BOUND('',#1993,.T.);
#1152=FACE_OUTER_BOUND('',#1994,.T.);
#1153=FACE_OUTER_BOUND('',#1995,.T.);
#1154=FACE_OUTER_BOUND('',#1996,.T.);
#1155=FACE_OUTER_BOUND('',#1997,.T.);
#1156=FACE_OUTER_BOUND('',#1998,.T.);
#1157=FACE_OUTER_BOUND('',#1999,.T.);
#1158=FACE_OUTER_BOUND('',#2000,.T.);
#1159=FACE_OUTER_BOUND('',#2001,.T.);
#1160=FACE_OUTER_BOUND('',#2002,.T.);
#1161=FACE_OUTER_BOUND('',#2003,.T.);
#1162=FACE_OUTER_BOUND('',#2004,.T.);
#1163=FACE_OUTER_BOUND('',#2005,.T.);
#1164=FACE_OUTER_BOUND('',#2006,.T.);
#1165=FACE_OUTER_BOUND('',#2007,.T.);
#1166=FACE_OUTER_BOUND('',#2008,.T.);
#1167=FACE_OUTER_BOUND('',#2009,.T.);
#1168=FACE_OUTER_BOUND('',#2010,.T.);
#1169=FACE_OUTER_BOUND('',#2011,.T.);
#1170=FACE_OUTER_BOUND('',#2012,.T.);
#1171=FACE_OUTER_BOUND('',#2013,.T.);
#1172=FACE_OUTER_BOUND('',#2014,.T.);
#1173=FACE_OUTER_BOUND('',#2015,.T.);
#1174=FACE_OUTER_BOUND('',#2016,.T.);
#1175=FACE_OUTER_BOUND('',#2017,.T.);
#1176=FACE_OUTER_BOUND('',#2018,.T.);
#1177=FACE_OUTER_BOUND('',#2019,.T.);
#1178=FACE_OUTER_BOUND('',#2020,.T.);
#1179=FACE_OUTER_BOUND('',#2021,.T.);
#1180=FACE_OUTER_BOUND('',#2022,.T.);
#1181=FACE_OUTER_BOUND('',#2023,.T.);
#1182=FACE_OUTER_BOUND('',#2024,.T.);
#1183=FACE_OUTER_BOUND('',#2025,.T.);
#1184=FACE_OUTER_BOUND('',#2026,.T.);
#1185=FACE_OUTER_BOUND('',#2027,.T.);
#1186=FACE_OUTER_BOUND('',#2028,.T.);
#1187=FACE_OUTER_BOUND('',#2029,.T.);
#1188=FACE_OUTER_BOUND('',#2030,.T.);
#1189=FACE_OUTER_BOUND('',#2031,.T.);
#1190=FACE_OUTER_BOUND('',#2032,.T.);
#1191=FACE_OUTER_BOUND('',#2033,.T.);
#1192=FACE_OUTER_BOUND('',#2034,.T.);
#1193=FACE_OUTER_BOUND('',#2035,.T.);
#1194=FACE_OUTER_BOUND('',#2036,.T.);
#1195=FACE_OUTER_BOUND('',#2037,.T.);
#1196=FACE_OUTER_BOUND('',#2038,.T.);
#1197=FACE_OUTER_BOUND('',#2039,.T.);
#1198=FACE_OUTER_BOUND('',#2040,.T.);
#1199=FACE_OUTER_BOUND('',#2041,.T.);
#1200=FACE_OUTER_BOUND('',#2042,.T.);
#1201=FACE_OUTER_BOUND('',#2043,.T.);
#1202=FACE_OUTER_BOUND('',#2044,.T.);
#1203=FACE_OUTER_BOUND('',#2045,.T.);
#1204=FACE_OUTER_BOUND('',#2046,.T.);
#1205=FACE_OUTER_BOUND('',#2047,.T.);
#1206=FACE_OUTER_BOUND('',#2048,.T.);
#1207=FACE_OUTER_BOUND('',#2049,.T.);
#1208=FACE_OUTER_BOUND('',#2050,.T.);
#1209=FACE_OUTER_BOUND('',#2051,.T.);
#1210=FACE_OUTER_BOUND('',#2052,.T.);
#1211=FACE_OUTER_BOUND('',#2053,.T.);
#1212=FACE_OUTER_BOUND('',#2054,.T.);
#1213=FACE_OUTER_BOUND('',#2055,.T.);
#1214=FACE_OUTER_BOUND('',#2056,.T.);
#1215=FACE_OUTER_BOUND('',#2058,.T.);
#1216=FACE_OUTER_BOUND('',#2059,.T.);
#1217=FACE_OUTER_BOUND('',#2061,.T.);
#1218=FACE_OUTER_BOUND('',#2062,.T.);
#1219=FACE_OUTER_BOUND('',#2063,.T.);
#1220=FACE_OUTER_BOUND('',#2064,.T.);
#1221=FACE_OUTER_BOUND('',#2066,.T.);
#1222=FACE_OUTER_BOUND('',#2068,.T.);
#1223=FACE_OUTER_BOUND('',#2069,.T.);
#1224=FACE_OUTER_BOUND('',#2070,.T.);
#1225=FACE_OUTER_BOUND('',#2071,.T.);
#1226=FACE_OUTER_BOUND('',#2072,.T.);
#1227=FACE_OUTER_BOUND('',#2073,.T.);
#1228=FACE_OUTER_BOUND('',#2074,.T.);
#1229=FACE_OUTER_BOUND('',#2075,.T.);
#1230=FACE_OUTER_BOUND('',#2076,.T.);
#1231=FACE_OUTER_BOUND('',#2077,.T.);
#1232=FACE_OUTER_BOUND('',#2078,.T.);
#1233=FACE_OUTER_BOUND('',#2079,.T.);
#1234=FACE_OUTER_BOUND('',#2080,.T.);
#1235=FACE_OUTER_BOUND('',#2081,.T.);
#1236=FACE_OUTER_BOUND('',#2082,.T.);
#1237=FACE_OUTER_BOUND('',#2083,.T.);
#1238=FACE_OUTER_BOUND('',#2084,.T.);
#1239=FACE_OUTER_BOUND('',#2085,.T.);
#1240=FACE_OUTER_BOUND('',#2086,.T.);
#1241=FACE_OUTER_BOUND('',#2087,.T.);
#1242=FACE_OUTER_BOUND('',#2088,.T.);
#1243=FACE_OUTER_BOUND('',#2089,.T.);
#1244=FACE_OUTER_BOUND('',#2090,.T.);
#1245=FACE_OUTER_BOUND('',#2091,.T.);
#1246=FACE_OUTER_BOUND('',#2092,.T.);
#1247=FACE_OUTER_BOUND('',#2093,.T.);
#1248=FACE_OUTER_BOUND('',#2094,.T.);
#1249=FACE_OUTER_BOUND('',#2095,.T.);
#1250=FACE_OUTER_BOUND('',#2096,.T.);
#1251=FACE_OUTER_BOUND('',#2097,.T.);
#1252=FACE_OUTER_BOUND('',#2098,.T.);
#1253=FACE_OUTER_BOUND('',#2099,.T.);
#1254=FACE_OUTER_BOUND('',#2100,.T.);
#1255=FACE_OUTER_BOUND('',#2101,.T.);
#1256=FACE_OUTER_BOUND('',#2102,.T.);
#1257=FACE_OUTER_BOUND('',#2103,.T.);
#1258=FACE_OUTER_BOUND('',#2104,.T.);
#1259=FACE_OUTER_BOUND('',#2105,.T.);
#1260=FACE_OUTER_BOUND('',#2106,.T.);
#1261=FACE_OUTER_BOUND('',#2107,.T.);
#1262=FACE_OUTER_BOUND('',#2108,.T.);
#1263=FACE_OUTER_BOUND('',#2109,.T.);
#1264=FACE_OUTER_BOUND('',#2110,.T.);
#1265=FACE_OUTER_BOUND('',#2111,.T.);
#1266=FACE_OUTER_BOUND('',#2112,.T.);
#1267=FACE_OUTER_BOUND('',#2113,.T.);
#1268=FACE_OUTER_BOUND('',#2114,.T.);
#1269=FACE_OUTER_BOUND('',#2115,.T.);
#1270=FACE_OUTER_BOUND('',#2116,.T.);
#1271=FACE_OUTER_BOUND('',#2117,.T.);
#1272=FACE_OUTER_BOUND('',#2118,.T.);
#1273=FACE_OUTER_BOUND('',#2119,.T.);
#1274=FACE_OUTER_BOUND('',#2120,.T.);
#1275=FACE_OUTER_BOUND('',#2121,.T.);
#1276=FACE_OUTER_BOUND('',#2122,.T.);
#1277=FACE_OUTER_BOUND('',#2123,.T.);
#1278=FACE_OUTER_BOUND('',#2124,.T.);
#1279=FACE_OUTER_BOUND('',#2125,.T.);
#1280=FACE_OUTER_BOUND('',#2126,.T.);
#1281=FACE_OUTER_BOUND('',#2127,.T.);
#1282=FACE_OUTER_BOUND('',#2128,.T.);
#1283=FACE_OUTER_BOUND('',#2129,.T.);
#1284=FACE_OUTER_BOUND('',#2130,.T.);
#1285=FACE_OUTER_BOUND('',#2131,.T.);
#1286=FACE_OUTER_BOUND('',#2132,.T.);
#1287=FACE_OUTER_BOUND('',#2133,.T.);
#1288=FACE_OUTER_BOUND('',#2134,.T.);
#1289=FACE_OUTER_BOUND('',#2135,.T.);
#1290=FACE_OUTER_BOUND('',#2136,.T.);
#1291=FACE_OUTER_BOUND('',#2137,.T.);
#1292=FACE_OUTER_BOUND('',#2138,.T.);
#1293=FACE_OUTER_BOUND('',#2139,.T.);
#1294=FACE_OUTER_BOUND('',#2140,.T.);
#1295=FACE_OUTER_BOUND('',#2141,.T.);
#1296=FACE_OUTER_BOUND('',#2142,.T.);
#1297=FACE_OUTER_BOUND('',#2143,.T.);
#1298=FACE_OUTER_BOUND('',#2144,.T.);
#1299=FACE_OUTER_BOUND('',#2145,.T.);
#1300=FACE_OUTER_BOUND('',#2147,.T.);
#1301=FACE_OUTER_BOUND('',#2148,.T.);
#1302=FACE_OUTER_BOUND('',#2150,.T.);
#1303=EDGE_LOOP('',(#8921,#8922,#8923,#8924,#8925,#8926,#8927,#8928));
#1304=EDGE_LOOP('',(#8929,#8930,#8931,#8932));
#1305=EDGE_LOOP('',(#8933,#8934,#8935,#8936));
#1306=EDGE_LOOP('',(#8937,#8938,#8939,#8940));
#1307=EDGE_LOOP('',(#8941,#8942,#8943,#8944));
#1308=EDGE_LOOP('',(#8945,#8946,#8947,#8948));
#1309=EDGE_LOOP('',(#8949,#8950,#8951,#8952));
#1310=EDGE_LOOP('',(#8953,#8954,#8955,#8956));
#1311=EDGE_LOOP('',(#8957,#8958,#8959,#8960));
#1312=EDGE_LOOP('',(#8961,#8962,#8963,#8964));
#1313=EDGE_LOOP('',(#8965,#8966,#8967,#8968));
#1314=EDGE_LOOP('',(#8969,#8970,#8971,#8972));
#1315=EDGE_LOOP('',(#8973,#8974,#8975,#8976));
#1316=EDGE_LOOP('',(#8977,#8978,#8979,#8980));
#1317=EDGE_LOOP('',(#8981,#8982,#8983,#8984));
#1318=EDGE_LOOP('',(#8985,#8986,#8987,#8988));
#1319=EDGE_LOOP('',(#8989,#8990,#8991,#8992));
#1320=EDGE_LOOP('',(#8993,#8994,#8995,#8996));
#1321=EDGE_LOOP('',(#8997,#8998,#8999,#9000,#9001,#9002,#9003,#9004));
#1322=EDGE_LOOP('',(#9005,#9006,#9007,#9008));
#1323=EDGE_LOOP('',(#9009,#9010,#9011,#9012));
#1324=EDGE_LOOP('',(#9013,#9014,#9015,#9016));
#1325=EDGE_LOOP('',(#9017,#9018,#9019,#9020));
#1326=EDGE_LOOP('',(#9021,#9022,#9023,#9024));
#1327=EDGE_LOOP('',(#9025,#9026,#9027,#9028));
#1328=EDGE_LOOP('',(#9029,#9030,#9031,#9032));
#1329=EDGE_LOOP('',(#9033,#9034,#9035,#9036));
#1330=EDGE_LOOP('',(#9037,#9038,#9039,#9040));
#1331=EDGE_LOOP('',(#9041,#9042,#9043,#9044));
#1332=EDGE_LOOP('',(#9045,#9046,#9047,#9048));
#1333=EDGE_LOOP('',(#9049,#9050,#9051,#9052));
#1334=EDGE_LOOP('',(#9053,#9054,#9055,#9056));
#1335=EDGE_LOOP('',(#9057,#9058,#9059,#9060));
#1336=EDGE_LOOP('',(#9061,#9062,#9063,#9064));
#1337=EDGE_LOOP('',(#9065,#9066,#9067,#9068));
#1338=EDGE_LOOP('',(#9069,#9070,#9071,#9072));
#1339=EDGE_LOOP('',(#9073,#9074,#9075,#9076,#9077,#9078,#9079,#9080));
#1340=EDGE_LOOP('',(#9081,#9082,#9083,#9084));
#1341=EDGE_LOOP('',(#9085,#9086,#9087,#9088));
#1342=EDGE_LOOP('',(#9089,#9090,#9091,#9092));
#1343=EDGE_LOOP('',(#9093,#9094,#9095,#9096));
#1344=EDGE_LOOP('',(#9097,#9098,#9099,#9100));
#1345=EDGE_LOOP('',(#9101,#9102,#9103,#9104));
#1346=EDGE_LOOP('',(#9105,#9106,#9107,#9108));
#1347=EDGE_LOOP('',(#9109,#9110,#9111,#9112));
#1348=EDGE_LOOP('',(#9113,#9114,#9115,#9116));
#1349=EDGE_LOOP('',(#9117,#9118,#9119,#9120));
#1350=EDGE_LOOP('',(#9121,#9122,#9123,#9124));
#1351=EDGE_LOOP('',(#9125,#9126,#9127,#9128));
#1352=EDGE_LOOP('',(#9129,#9130,#9131,#9132));
#1353=EDGE_LOOP('',(#9133,#9134,#9135,#9136));
#1354=EDGE_LOOP('',(#9137,#9138,#9139,#9140));
#1355=EDGE_LOOP('',(#9141,#9142,#9143,#9144));
#1356=EDGE_LOOP('',(#9145,#9146,#9147,#9148));
#1357=EDGE_LOOP('',(#9149,#9150,#9151,#9152,#9153,#9154,#9155,#9156));
#1358=EDGE_LOOP('',(#9157,#9158,#9159,#9160));
#1359=EDGE_LOOP('',(#9161,#9162,#9163,#9164));
#1360=EDGE_LOOP('',(#9165,#9166,#9167,#9168));
#1361=EDGE_LOOP('',(#9169,#9170,#9171,#9172));
#1362=EDGE_LOOP('',(#9173,#9174,#9175,#9176));
#1363=EDGE_LOOP('',(#9177,#9178,#9179,#9180));
#1364=EDGE_LOOP('',(#9181,#9182,#9183,#9184));
#1365=EDGE_LOOP('',(#9185,#9186,#9187,#9188));
#1366=EDGE_LOOP('',(#9189,#9190,#9191,#9192));
#1367=EDGE_LOOP('',(#9193,#9194,#9195,#9196));
#1368=EDGE_LOOP('',(#9197,#9198,#9199,#9200));
#1369=EDGE_LOOP('',(#9201,#9202,#9203,#9204));
#1370=EDGE_LOOP('',(#9205,#9206,#9207,#9208));
#1371=EDGE_LOOP('',(#9209,#9210,#9211,#9212));
#1372=EDGE_LOOP('',(#9213,#9214,#9215,#9216));
#1373=EDGE_LOOP('',(#9217,#9218,#9219,#9220));
#1374=EDGE_LOOP('',(#9221,#9222,#9223,#9224));
#1375=EDGE_LOOP('',(#9225,#9226,#9227,#9228,#9229,#9230,#9231,#9232));
#1376=EDGE_LOOP('',(#9233,#9234,#9235,#9236));
#1377=EDGE_LOOP('',(#9237,#9238,#9239,#9240));
#1378=EDGE_LOOP('',(#9241,#9242,#9243,#9244));
#1379=EDGE_LOOP('',(#9245,#9246,#9247,#9248));
#1380=EDGE_LOOP('',(#9249,#9250,#9251,#9252));
#1381=EDGE_LOOP('',(#9253,#9254,#9255,#9256));
#1382=EDGE_LOOP('',(#9257,#9258,#9259,#9260));
#1383=EDGE_LOOP('',(#9261,#9262,#9263,#9264));
#1384=EDGE_LOOP('',(#9265,#9266,#9267,#9268));
#1385=EDGE_LOOP('',(#9269,#9270,#9271,#9272));
#1386=EDGE_LOOP('',(#9273,#9274,#9275,#9276));
#1387=EDGE_LOOP('',(#9277,#9278,#9279,#9280));
#1388=EDGE_LOOP('',(#9281,#9282,#9283,#9284));
#1389=EDGE_LOOP('',(#9285,#9286,#9287,#9288));
#1390=EDGE_LOOP('',(#9289,#9290,#9291,#9292));
#1391=EDGE_LOOP('',(#9293,#9294,#9295,#9296));
#1392=EDGE_LOOP('',(#9297,#9298,#9299,#9300));
#1393=EDGE_LOOP('',(#9301,#9302,#9303,#9304,#9305,#9306,#9307,#9308));
#1394=EDGE_LOOP('',(#9309,#9310,#9311,#9312));
#1395=EDGE_LOOP('',(#9313,#9314,#9315,#9316));
#1396=EDGE_LOOP('',(#9317,#9318,#9319,#9320));
#1397=EDGE_LOOP('',(#9321,#9322,#9323,#9324));
#1398=EDGE_LOOP('',(#9325,#9326,#9327,#9328));
#1399=EDGE_LOOP('',(#9329,#9330,#9331,#9332));
#1400=EDGE_LOOP('',(#9333,#9334,#9335,#9336));
#1401=EDGE_LOOP('',(#9337,#9338,#9339,#9340));
#1402=EDGE_LOOP('',(#9341,#9342,#9343,#9344));
#1403=EDGE_LOOP('',(#9345,#9346,#9347,#9348));
#1404=EDGE_LOOP('',(#9349,#9350,#9351,#9352));
#1405=EDGE_LOOP('',(#9353,#9354,#9355,#9356));
#1406=EDGE_LOOP('',(#9357,#9358,#9359,#9360));
#1407=EDGE_LOOP('',(#9361,#9362,#9363,#9364));
#1408=EDGE_LOOP('',(#9365,#9366,#9367,#9368));
#1409=EDGE_LOOP('',(#9369,#9370,#9371,#9372));
#1410=EDGE_LOOP('',(#9373,#9374,#9375,#9376));
#1411=EDGE_LOOP('',(#9377,#9378,#9379,#9380,#9381,#9382,#9383,#9384));
#1412=EDGE_LOOP('',(#9385,#9386,#9387,#9388));
#1413=EDGE_LOOP('',(#9389,#9390,#9391,#9392));
#1414=EDGE_LOOP('',(#9393,#9394,#9395,#9396));
#1415=EDGE_LOOP('',(#9397,#9398,#9399,#9400));
#1416=EDGE_LOOP('',(#9401,#9402,#9403,#9404));
#1417=EDGE_LOOP('',(#9405,#9406,#9407,#9408));
#1418=EDGE_LOOP('',(#9409,#9410,#9411,#9412));
#1419=EDGE_LOOP('',(#9413,#9414,#9415,#9416));
#1420=EDGE_LOOP('',(#9417,#9418,#9419,#9420));
#1421=EDGE_LOOP('',(#9421,#9422,#9423,#9424));
#1422=EDGE_LOOP('',(#9425,#9426,#9427,#9428));
#1423=EDGE_LOOP('',(#9429,#9430,#9431,#9432));
#1424=EDGE_LOOP('',(#9433,#9434,#9435,#9436));
#1425=EDGE_LOOP('',(#9437,#9438,#9439,#9440));
#1426=EDGE_LOOP('',(#9441,#9442,#9443,#9444));
#1427=EDGE_LOOP('',(#9445,#9446,#9447,#9448));
#1428=EDGE_LOOP('',(#9449,#9450,#9451,#9452));
#1429=EDGE_LOOP('',(#9453,#9454,#9455,#9456,#9457,#9458,#9459,#9460));
#1430=EDGE_LOOP('',(#9461,#9462,#9463,#9464));
#1431=EDGE_LOOP('',(#9465,#9466,#9467,#9468));
#1432=EDGE_LOOP('',(#9469,#9470,#9471,#9472));
#1433=EDGE_LOOP('',(#9473,#9474,#9475,#9476));
#1434=EDGE_LOOP('',(#9477,#9478,#9479,#9480));
#1435=EDGE_LOOP('',(#9481,#9482,#9483,#9484));
#1436=EDGE_LOOP('',(#9485,#9486,#9487,#9488));
#1437=EDGE_LOOP('',(#9489,#9490,#9491,#9492));
#1438=EDGE_LOOP('',(#9493,#9494,#9495,#9496));
#1439=EDGE_LOOP('',(#9497,#9498,#9499,#9500));
#1440=EDGE_LOOP('',(#9501,#9502,#9503,#9504));
#1441=EDGE_LOOP('',(#9505,#9506,#9507,#9508));
#1442=EDGE_LOOP('',(#9509,#9510,#9511,#9512));
#1443=EDGE_LOOP('',(#9513,#9514,#9515,#9516));
#1444=EDGE_LOOP('',(#9517,#9518,#9519,#9520));
#1445=EDGE_LOOP('',(#9521,#9522,#9523,#9524));
#1446=EDGE_LOOP('',(#9525,#9526,#9527,#9528));
#1447=EDGE_LOOP('',(#9529,#9530,#9531,#9532));
#1448=EDGE_LOOP('',(#9533));
#1449=EDGE_LOOP('',(#9534));
#1450=EDGE_LOOP('',(#9535,#9536,#9537,#9538));
#1451=EDGE_LOOP('',(#9539));
#1452=EDGE_LOOP('',(#9540));
#1453=EDGE_LOOP('',(#9541,#9542,#9543,#9544));
#1454=EDGE_LOOP('',(#9545));
#1455=EDGE_LOOP('',(#9546));
#1456=EDGE_LOOP('',(#9547,#9548,#9549,#9550));
#1457=EDGE_LOOP('',(#9551));
#1458=EDGE_LOOP('',(#9552));
#1459=EDGE_LOOP('',(#9553,#9554,#9555,#9556));
#1460=EDGE_LOOP('',(#9557,#9558,#9559,#9560));
#1461=EDGE_LOOP('',(#9561,#9562,#9563,#9564));
#1462=EDGE_LOOP('',(#9565,#9566,#9567,#9568));
#1463=EDGE_LOOP('',(#9569,#9570,#9571,#9572,#9573));
#1464=EDGE_LOOP('',(#9574,#9575,#9576,#9577));
#1465=EDGE_LOOP('',(#9578,#9579,#9580,#9581,#9582,#9583,#9584,#9585,#9586,
#9587,#9588,#9589,#9590,#9591,#9592,#9593,#9594,#9595,#9596,#9597,#9598,
#9599));
#1466=EDGE_LOOP('',(#9600,#9601,#9602,#9603,#9604,#9605,#9606,#9607,#9608,
#9609,#9610,#9611,#9612,#9613,#9614,#9615,#9616,#9617,#9618,#9619,#9620,
#9621));
#1467=EDGE_LOOP('',(#9622,#9623,#9624,#9625));
#1468=EDGE_LOOP('',(#9626,#9627,#9628,#9629,#9630));
#1469=EDGE_LOOP('',(#9631,#9632,#9633,#9634));
#1470=EDGE_LOOP('',(#9635,#9636,#9637,#9638,#9639,#9640,#9641,#9642,#9643,
#9644,#9645,#9646,#9647,#9648,#9649,#9650,#9651,#9652,#9653,#9654,#9655,
#9656));
#1471=EDGE_LOOP('',(#9657,#9658,#9659,#9660,#9661,#9662,#9663,#9664,#9665,
#9666,#9667,#9668,#9669,#9670,#9671,#9672,#9673,#9674,#9675,#9676,#9677,
#9678));
#1472=EDGE_LOOP('',(#9679,#9680,#9681,#9682));
#1473=EDGE_LOOP('',(#9683,#9684,#9685,#9686,#9687));
#1474=EDGE_LOOP('',(#9688,#9689,#9690,#9691));
#1475=EDGE_LOOP('',(#9692,#9693,#9694,#9695,#9696,#9697,#9698,#9699,#9700,
#9701,#9702,#9703,#9704,#9705,#9706,#9707,#9708,#9709,#9710,#9711,#9712,
#9713));
#1476=EDGE_LOOP('',(#9714,#9715,#9716,#9717,#9718,#9719,#9720,#9721,#9722,
#9723,#9724,#9725,#9726,#9727,#9728,#9729,#9730,#9731,#9732,#9733,#9734,
#9735));
#1477=EDGE_LOOP('',(#9736,#9737,#9738,#9739));
#1478=EDGE_LOOP('',(#9740,#9741,#9742,#9743,#9744));
#1479=EDGE_LOOP('',(#9745,#9746,#9747,#9748));
#1480=EDGE_LOOP('',(#9749,#9750,#9751,#9752,#9753,#9754,#9755,#9756,#9757,
#9758,#9759,#9760,#9761,#9762,#9763,#9764,#9765,#9766,#9767,#9768,#9769,
#9770));
#1481=EDGE_LOOP('',(#9771,#9772,#9773,#9774,#9775,#9776,#9777,#9778,#9779,
#9780,#9781,#9782,#9783,#9784,#9785,#9786,#9787,#9788,#9789,#9790,#9791,
#9792));
#1482=EDGE_LOOP('',(#9793,#9794,#9795,#9796));
#1483=EDGE_LOOP('',(#9797,#9798,#9799,#9800,#9801));
#1484=EDGE_LOOP('',(#9802,#9803,#9804,#9805));
#1485=EDGE_LOOP('',(#9806,#9807,#9808,#9809,#9810,#9811,#9812,#9813,#9814,
#9815,#9816,#9817,#9818,#9819,#9820,#9821,#9822,#9823,#9824,#9825,#9826,
#9827));
#1486=EDGE_LOOP('',(#9828,#9829,#9830,#9831,#9832,#9833,#9834,#9835,#9836,
#9837,#9838,#9839,#9840,#9841,#9842,#9843,#9844,#9845,#9846,#9847,#9848,
#9849));
#1487=EDGE_LOOP('',(#9850,#9851,#9852,#9853));
#1488=EDGE_LOOP('',(#9854,#9855,#9856,#9857,#9858));
#1489=EDGE_LOOP('',(#9859,#9860,#9861,#9862));
#1490=EDGE_LOOP('',(#9863,#9864,#9865,#9866,#9867,#9868,#9869,#9870,#9871,
#9872,#9873,#9874,#9875,#9876,#9877,#9878,#9879,#9880,#9881,#9882,#9883,
#9884));
#1491=EDGE_LOOP('',(#9885,#9886,#9887,#9888,#9889,#9890,#9891,#9892,#9893,
#9894,#9895,#9896,#9897,#9898,#9899,#9900,#9901,#9902,#9903,#9904,#9905,
#9906));
#1492=EDGE_LOOP('',(#9907,#9908,#9909,#9910));
#1493=EDGE_LOOP('',(#9911,#9912,#9913,#9914,#9915));
#1494=EDGE_LOOP('',(#9916,#9917,#9918,#9919));
#1495=EDGE_LOOP('',(#9920,#9921,#9922,#9923,#9924,#9925,#9926,#9927,#9928,
#9929,#9930,#9931,#9932,#9933,#9934,#9935,#9936,#9937,#9938,#9939,#9940,
#9941));
#1496=EDGE_LOOP('',(#9942,#9943,#9944,#9945,#9946,#9947,#9948,#9949,#9950,
#9951,#9952,#9953,#9954,#9955,#9956,#9957,#9958,#9959,#9960,#9961,#9962,
#9963));
#1497=EDGE_LOOP('',(#9964,#9965,#9966,#9967));
#1498=EDGE_LOOP('',(#9968,#9969,#9970,#9971,#9972));
#1499=EDGE_LOOP('',(#9973,#9974,#9975,#9976));
#1500=EDGE_LOOP('',(#9977,#9978,#9979,#9980,#9981,#9982,#9983,#9984,#9985,
#9986,#9987,#9988,#9989,#9990,#9991,#9992,#9993,#9994,#9995,#9996,#9997,
#9998));
#1501=EDGE_LOOP('',(#9999,#10000,#10001,#10002,#10003,#10004,#10005,#10006,
#10007,#10008,#10009,#10010,#10011,#10012,#10013,#10014,#10015,#10016,#10017,
#10018,#10019,#10020));
#1502=EDGE_LOOP('',(#10021,#10022,#10023,#10024));
#1503=EDGE_LOOP('',(#10025,#10026,#10027,#10028));
#1504=EDGE_LOOP('',(#10029,#10030,#10031,#10032,#10033,#10034,#10035,#10036,
#10037,#10038,#10039,#10040));
#1505=EDGE_LOOP('',(#10041,#10042,#10043,#10044));
#1506=EDGE_LOOP('',(#10045,#10046,#10047,#10048));
#1507=EDGE_LOOP('',(#10049,#10050,#10051,#10052));
#1508=EDGE_LOOP('',(#10053,#10054,#10055,#10056));
#1509=EDGE_LOOP('',(#10057,#10058,#10059,#10060,#10061,#10062,#10063,#10064,
#10065,#10066,#10067,#10068));
#1510=EDGE_LOOP('',(#10069,#10070,#10071,#10072));
#1511=EDGE_LOOP('',(#10073,#10074,#10075,#10076));
#1512=EDGE_LOOP('',(#10077,#10078,#10079,#10080));
#1513=EDGE_LOOP('',(#10081,#10082,#10083,#10084));
#1514=EDGE_LOOP('',(#10085,#10086,#10087,#10088));
#1515=EDGE_LOOP('',(#10089,#10090,#10091,#10092,#10093,#10094));
#1516=EDGE_LOOP('',(#10095,#10096,#10097,#10098));
#1517=EDGE_LOOP('',(#10099,#10100,#10101,#10102,#10103,#10104,#10105,#10106,
#10107,#10108));
#1518=EDGE_LOOP('',(#10109));
#1519=EDGE_LOOP('',(#10110,#10111,#10112,#10113,#10114,#10115,#10116,#10117,
#10118,#10119));
#1520=EDGE_LOOP('',(#10120));
#1521=EDGE_LOOP('',(#10121,#10122,#10123,#10124));
#1522=EDGE_LOOP('',(#10125,#10126,#10127,#10128));
#1523=EDGE_LOOP('',(#10129,#10130,#10131,#10132,#10133,#10134));
#1524=EDGE_LOOP('',(#10135,#10136,#10137,#10138));
#1525=EDGE_LOOP('',(#10139,#10140,#10141,#10142));
#1526=EDGE_LOOP('',(#10143,#10144,#10145,#10146));
#1527=EDGE_LOOP('',(#10147,#10148,#10149,#10150,#10151,#10152,#10153,#10154,
#10155,#10156));
#1528=EDGE_LOOP('',(#10157));
#1529=EDGE_LOOP('',(#10158,#10159,#10160,#10161));
#1530=EDGE_LOOP('',(#10162,#10163,#10164,#10165));
#1531=EDGE_LOOP('',(#10166,#10167,#10168,#10169));
#1532=EDGE_LOOP('',(#10170,#10171,#10172,#10173));
#1533=EDGE_LOOP('',(#10174,#10175,#10176,#10177,#10178,#10179,#10180,#10181,
#10182,#10183,#10184,#10185,#10186,#10187,#10188,#10189,#10190,#10191,#10192,
#10193));
#1534=EDGE_LOOP('',(#10194,#10195,#10196,#10197,#10198,#10199));
#1535=EDGE_LOOP('',(#10200,#10201,#10202,#10203,#10204,#10205));
#1536=EDGE_LOOP('',(#10206,#10207,#10208,#10209));
#1537=EDGE_LOOP('',(#10210,#10211,#10212,#10213,#10214,#10215));
#1538=EDGE_LOOP('',(#10216,#10217,#10218,#10219,#10220,#10221));
#1539=EDGE_LOOP('',(#10222,#10223,#10224,#10225));
#1540=EDGE_LOOP('',(#10226,#10227,#10228,#10229));
#1541=EDGE_LOOP('',(#10230,#10231,#10232,#10233,#10234));
#1542=EDGE_LOOP('',(#10235,#10236,#10237,#10238));
#1543=EDGE_LOOP('',(#10239,#10240,#10241,#10242));
#1544=EDGE_LOOP('',(#10243,#10244,#10245,#10246,#10247,#10248,#10249,#10250,
#10251,#10252,#10253,#10254));
#1545=EDGE_LOOP('',(#10255,#10256,#10257,#10258));
#1546=EDGE_LOOP('',(#10259,#10260,#10261,#10262));
#1547=EDGE_LOOP('',(#10263,#10264,#10265,#10266,#10267,#10268,#10269,#10270,
#10271,#10272,#10273,#10274));
#1548=EDGE_LOOP('',(#10275,#10276,#10277,#10278));
#1549=EDGE_LOOP('',(#10279,#10280,#10281,#10282));
#1550=EDGE_LOOP('',(#10283,#10284,#10285,#10286));
#1551=EDGE_LOOP('',(#10287,#10288,#10289,#10290));
#1552=EDGE_LOOP('',(#10291,#10292,#10293,#10294));
#1553=EDGE_LOOP('',(#10295,#10296,#10297,#10298));
#1554=EDGE_LOOP('',(#10299,#10300,#10301,#10302));
#1555=EDGE_LOOP('',(#10303,#10304,#10305,#10306,#10307,#10308,#10309,#10310,
#10311,#10312,#10313,#10314,#10315,#10316,#10317,#10318,#10319,#10320,#10321,
#10322));
#1556=EDGE_LOOP('',(#10323,#10324,#10325,#10326));
#1557=EDGE_LOOP('',(#10327,#10328,#10329,#10330));
#1558=EDGE_LOOP('',(#10331,#10332,#10333,#10334,#10335,#10336,#10337,#10338,
#10339,#10340));
#1559=EDGE_LOOP('',(#10341));
#1560=EDGE_LOOP('',(#10342,#10343,#10344,#10345));
#1561=EDGE_LOOP('',(#10346,#10347,#10348,#10349,#10350,#10351));
#1562=EDGE_LOOP('',(#10352,#10353,#10354,#10355));
#1563=EDGE_LOOP('',(#10356,#10357,#10358,#10359,#10360,#10361,#10362));
#1564=EDGE_LOOP('',(#10363,#10364,#10365,#10366));
#1565=EDGE_LOOP('',(#10367,#10368,#10369,#10370));
#1566=EDGE_LOOP('',(#10371,#10372,#10373,#10374));
#1567=EDGE_LOOP('',(#10375,#10376,#10377,#10378,#10379,#10380));
#1568=EDGE_LOOP('',(#10381,#10382,#10383,#10384,#10385,#10386));
#1569=EDGE_LOOP('',(#10387,#10388,#10389,#10390));
#1570=EDGE_LOOP('',(#10391,#10392,#10393,#10394,#10395,#10396));
#1571=EDGE_LOOP('',(#10397,#10398,#10399,#10400));
#1572=EDGE_LOOP('',(#10401,#10402,#10403,#10404,#10405,#10406));
#1573=EDGE_LOOP('',(#10407,#10408,#10409,#10410));
#1574=EDGE_LOOP('',(#10411));
#1575=EDGE_LOOP('',(#10412));
#1576=EDGE_LOOP('',(#10413));
#1577=EDGE_LOOP('',(#10414));
#1578=EDGE_LOOP('',(#10415));
#1579=EDGE_LOOP('',(#10416));
#1580=EDGE_LOOP('',(#10417));
#1581=EDGE_LOOP('',(#10418));
#1582=EDGE_LOOP('',(#10419));
#1583=EDGE_LOOP('',(#10420));
#1584=EDGE_LOOP('',(#10421));
#1585=EDGE_LOOP('',(#10422));
#1586=EDGE_LOOP('',(#10423));
#1587=EDGE_LOOP('',(#10424));
#1588=EDGE_LOOP('',(#10425));
#1589=EDGE_LOOP('',(#10426));
#1590=EDGE_LOOP('',(#10427,#10428,#10429,#10430,#10431,#10432,#10433,#10434));
#1591=EDGE_LOOP('',(#10435,#10436,#10437,#10438));
#1592=EDGE_LOOP('',(#10439,#10440,#10441,#10442));
#1593=EDGE_LOOP('',(#10443,#10444,#10445,#10446));
#1594=EDGE_LOOP('',(#10447,#10448,#10449,#10450));
#1595=EDGE_LOOP('',(#10451,#10452,#10453,#10454));
#1596=EDGE_LOOP('',(#10455,#10456,#10457,#10458));
#1597=EDGE_LOOP('',(#10459,#10460,#10461,#10462));
#1598=EDGE_LOOP('',(#10463,#10464,#10465,#10466));
#1599=EDGE_LOOP('',(#10467,#10468,#10469,#10470));
#1600=EDGE_LOOP('',(#10471,#10472,#10473,#10474));
#1601=EDGE_LOOP('',(#10475,#10476,#10477,#10478));
#1602=EDGE_LOOP('',(#10479,#10480,#10481,#10482));
#1603=EDGE_LOOP('',(#10483,#10484,#10485,#10486));
#1604=EDGE_LOOP('',(#10487,#10488,#10489,#10490,#10491,#10492,#10493,#10494));
#1605=EDGE_LOOP('',(#10495,#10496,#10497,#10498));
#1606=EDGE_LOOP('',(#10499,#10500,#10501,#10502));
#1607=EDGE_LOOP('',(#10503,#10504,#10505,#10506));
#1608=EDGE_LOOP('',(#10507,#10508,#10509,#10510));
#1609=EDGE_LOOP('',(#10511,#10512,#10513,#10514));
#1610=EDGE_LOOP('',(#10515,#10516,#10517,#10518));
#1611=EDGE_LOOP('',(#10519,#10520,#10521,#10522));
#1612=EDGE_LOOP('',(#10523,#10524,#10525,#10526));
#1613=EDGE_LOOP('',(#10527,#10528,#10529,#10530));
#1614=EDGE_LOOP('',(#10531,#10532,#10533,#10534));
#1615=EDGE_LOOP('',(#10535,#10536,#10537,#10538));
#1616=EDGE_LOOP('',(#10539,#10540,#10541,#10542));
#1617=EDGE_LOOP('',(#10543,#10544,#10545,#10546));
#1618=EDGE_LOOP('',(#10547,#10548,#10549,#10550,#10551,#10552,#10553,#10554));
#1619=EDGE_LOOP('',(#10555,#10556,#10557,#10558));
#1620=EDGE_LOOP('',(#10559,#10560,#10561,#10562));
#1621=EDGE_LOOP('',(#10563,#10564,#10565,#10566));
#1622=EDGE_LOOP('',(#10567,#10568,#10569,#10570));
#1623=EDGE_LOOP('',(#10571,#10572,#10573,#10574));
#1624=EDGE_LOOP('',(#10575,#10576,#10577,#10578));
#1625=EDGE_LOOP('',(#10579,#10580,#10581,#10582));
#1626=EDGE_LOOP('',(#10583,#10584,#10585,#10586));
#1627=EDGE_LOOP('',(#10587,#10588,#10589,#10590));
#1628=EDGE_LOOP('',(#10591,#10592,#10593,#10594));
#1629=EDGE_LOOP('',(#10595,#10596,#10597,#10598));
#1630=EDGE_LOOP('',(#10599,#10600,#10601,#10602));
#1631=EDGE_LOOP('',(#10603,#10604,#10605,#10606));
#1632=EDGE_LOOP('',(#10607,#10608,#10609,#10610,#10611,#10612,#10613,#10614));
#1633=EDGE_LOOP('',(#10615,#10616,#10617,#10618));
#1634=EDGE_LOOP('',(#10619,#10620,#10621,#10622));
#1635=EDGE_LOOP('',(#10623,#10624,#10625,#10626));
#1636=EDGE_LOOP('',(#10627,#10628,#10629,#10630));
#1637=EDGE_LOOP('',(#10631,#10632,#10633,#10634));
#1638=EDGE_LOOP('',(#10635,#10636,#10637,#10638));
#1639=EDGE_LOOP('',(#10639,#10640,#10641,#10642));
#1640=EDGE_LOOP('',(#10643,#10644,#10645,#10646));
#1641=EDGE_LOOP('',(#10647,#10648,#10649,#10650));
#1642=EDGE_LOOP('',(#10651,#10652,#10653,#10654));
#1643=EDGE_LOOP('',(#10655,#10656,#10657,#10658));
#1644=EDGE_LOOP('',(#10659,#10660,#10661,#10662));
#1645=EDGE_LOOP('',(#10663,#10664,#10665,#10666));
#1646=EDGE_LOOP('',(#10667,#10668,#10669,#10670,#10671,#10672,#10673,#10674));
#1647=EDGE_LOOP('',(#10675,#10676,#10677,#10678));
#1648=EDGE_LOOP('',(#10679,#10680,#10681,#10682));
#1649=EDGE_LOOP('',(#10683,#10684,#10685,#10686));
#1650=EDGE_LOOP('',(#10687,#10688,#10689,#10690));
#1651=EDGE_LOOP('',(#10691,#10692,#10693,#10694));
#1652=EDGE_LOOP('',(#10695,#10696,#10697,#10698));
#1653=EDGE_LOOP('',(#10699,#10700,#10701,#10702));
#1654=EDGE_LOOP('',(#10703,#10704,#10705,#10706));
#1655=EDGE_LOOP('',(#10707,#10708,#10709,#10710,#10711,#10712,#10713,#10714));
#1656=EDGE_LOOP('',(#10715,#10716,#10717,#10718));
#1657=EDGE_LOOP('',(#10719,#10720,#10721,#10722));
#1658=EDGE_LOOP('',(#10723,#10724,#10725,#10726));
#1659=EDGE_LOOP('',(#10727,#10728,#10729,#10730));
#1660=EDGE_LOOP('',(#10731,#10732,#10733,#10734));
#1661=EDGE_LOOP('',(#10735,#10736,#10737,#10738));
#1662=EDGE_LOOP('',(#10739,#10740,#10741,#10742));
#1663=EDGE_LOOP('',(#10743,#10744,#10745,#10746));
#1664=EDGE_LOOP('',(#10747,#10748,#10749,#10750,#10751,#10752,#10753,#10754));
#1665=EDGE_LOOP('',(#10755,#10756,#10757,#10758));
#1666=EDGE_LOOP('',(#10759,#10760,#10761,#10762));
#1667=EDGE_LOOP('',(#10763,#10764,#10765,#10766));
#1668=EDGE_LOOP('',(#10767,#10768,#10769,#10770));
#1669=EDGE_LOOP('',(#10771,#10772,#10773,#10774));
#1670=EDGE_LOOP('',(#10775,#10776,#10777,#10778));
#1671=EDGE_LOOP('',(#10779,#10780,#10781,#10782));
#1672=EDGE_LOOP('',(#10783,#10784,#10785,#10786));
#1673=EDGE_LOOP('',(#10787,#10788,#10789,#10790,#10791,#10792,#10793,#10794));
#1674=EDGE_LOOP('',(#10795,#10796,#10797,#10798));
#1675=EDGE_LOOP('',(#10799,#10800,#10801,#10802));
#1676=EDGE_LOOP('',(#10803,#10804,#10805,#10806));
#1677=EDGE_LOOP('',(#10807,#10808,#10809,#10810));
#1678=EDGE_LOOP('',(#10811,#10812,#10813,#10814));
#1679=EDGE_LOOP('',(#10815,#10816,#10817,#10818));
#1680=EDGE_LOOP('',(#10819,#10820,#10821,#10822));
#1681=EDGE_LOOP('',(#10823,#10824,#10825,#10826));
#1682=EDGE_LOOP('',(#10827,#10828,#10829,#10830));
#1683=EDGE_LOOP('',(#10831,#10832,#10833,#10834));
#1684=EDGE_LOOP('',(#10835,#10836,#10837,#10838,#10839,#10840,#10841,#10842,
#10843,#10844,#10845,#10846,#10847,#10848));
#1685=EDGE_LOOP('',(#10849,#10850,#10851,#10852,#10853,#10854,#10855,#10856,
#10857,#10858,#10859,#10860,#10861));
#1686=EDGE_LOOP('',(#10862,#10863,#10864,#10865));
#1687=EDGE_LOOP('',(#10866,#10867,#10868,#10869));
#1688=EDGE_LOOP('',(#10870,#10871,#10872,#10873));
#1689=EDGE_LOOP('',(#10874,#10875,#10876,#10877,#10878,#10879,#10880,#10881,
#10882,#10883,#10884,#10885,#10886,#10887));
#1690=EDGE_LOOP('',(#10888,#10889,#10890,#10891,#10892,#10893,#10894,#10895,
#10896,#10897,#10898,#10899,#10900));
#1691=EDGE_LOOP('',(#10901,#10902,#10903,#10904));
#1692=EDGE_LOOP('',(#10905,#10906,#10907,#10908));
#1693=EDGE_LOOP('',(#10909,#10910,#10911,#10912));
#1694=EDGE_LOOP('',(#10913,#10914,#10915,#10916,#10917,#10918,#10919,#10920,
#10921,#10922,#10923,#10924,#10925,#10926));
#1695=EDGE_LOOP('',(#10927,#10928,#10929,#10930,#10931,#10932,#10933,#10934,
#10935,#10936,#10937,#10938,#10939));
#1696=EDGE_LOOP('',(#10940,#10941,#10942,#10943));
#1697=EDGE_LOOP('',(#10944,#10945,#10946,#10947));
#1698=EDGE_LOOP('',(#10948,#10949,#10950,#10951));
#1699=EDGE_LOOP('',(#10952,#10953,#10954,#10955,#10956,#10957,#10958,#10959,
#10960,#10961,#10962,#10963,#10964,#10965));
#1700=EDGE_LOOP('',(#10966,#10967,#10968,#10969,#10970,#10971,#10972,#10973,
#10974,#10975,#10976,#10977,#10978));
#1701=EDGE_LOOP('',(#10979,#10980,#10981,#10982));
#1702=EDGE_LOOP('',(#10983));
#1703=EDGE_LOOP('',(#10984));
#1704=EDGE_LOOP('',(#10985));
#1705=EDGE_LOOP('',(#10986));
#1706=EDGE_LOOP('',(#10987,#10988,#10989,#10990,#10991));
#1707=EDGE_LOOP('',(#10992,#10993,#10994,#10995));
#1708=EDGE_LOOP('',(#10996,#10997,#10998,#10999,#11000,#11001,#11002,#11003,
#11004,#11005,#11006,#11007,#11008,#11009,#11010,#11011,#11012,#11013));
#1709=EDGE_LOOP('',(#11014,#11015,#11016,#11017,#11018,#11019,#11020,#11021,
#11022,#11023,#11024,#11025,#11026,#11027,#11028,#11029,#11030,#11031));
#1710=EDGE_LOOP('',(#11032,#11033,#11034,#11035));
#1711=EDGE_LOOP('',(#11036,#11037,#11038,#11039,#11040));
#1712=EDGE_LOOP('',(#11041,#11042,#11043,#11044));
#1713=EDGE_LOOP('',(#11045,#11046,#11047,#11048,#11049,#11050,#11051,#11052,
#11053,#11054,#11055,#11056,#11057,#11058,#11059,#11060,#11061,#11062));
#1714=EDGE_LOOP('',(#11063,#11064,#11065,#11066,#11067,#11068,#11069,#11070,
#11071,#11072,#11073,#11074,#11075,#11076,#11077,#11078,#11079,#11080));
#1715=EDGE_LOOP('',(#11081,#11082,#11083,#11084));
#1716=EDGE_LOOP('',(#11085,#11086,#11087,#11088,#11089));
#1717=EDGE_LOOP('',(#11090,#11091,#11092,#11093));
#1718=EDGE_LOOP('',(#11094,#11095,#11096,#11097,#11098,#11099,#11100,#11101,
#11102,#11103,#11104,#11105,#11106,#11107,#11108,#11109,#11110,#11111));
#1719=EDGE_LOOP('',(#11112,#11113,#11114,#11115,#11116,#11117,#11118,#11119,
#11120,#11121,#11122,#11123,#11124,#11125,#11126,#11127,#11128,#11129));
#1720=EDGE_LOOP('',(#11130,#11131,#11132,#11133));
#1721=EDGE_LOOP('',(#11134,#11135,#11136,#11137,#11138));
#1722=EDGE_LOOP('',(#11139,#11140,#11141,#11142));
#1723=EDGE_LOOP('',(#11143,#11144,#11145,#11146,#11147,#11148,#11149,#11150,
#11151,#11152,#11153,#11154,#11155,#11156,#11157,#11158,#11159,#11160));
#1724=EDGE_LOOP('',(#11161,#11162,#11163,#11164,#11165,#11166,#11167,#11168,
#11169,#11170,#11171,#11172,#11173,#11174,#11175,#11176,#11177,#11178));
#1725=EDGE_LOOP('',(#11179,#11180,#11181,#11182));
#1726=EDGE_LOOP('',(#11183,#11184,#11185,#11186));
#1727=EDGE_LOOP('',(#11187));
#1728=EDGE_LOOP('',(#11188));
#1729=EDGE_LOOP('',(#11189,#11190,#11191,#11192));
#1730=EDGE_LOOP('',(#11193,#11194,#11195,#11196));
#1731=EDGE_LOOP('',(#11197));
#1732=EDGE_LOOP('',(#11198,#11199,#11200,#11201));
#1733=EDGE_LOOP('',(#11202,#11203,#11204,#11205));
#1734=EDGE_LOOP('',(#11206,#11207,#11208,#11209));
#1735=EDGE_LOOP('',(#11210,#11211,#11212,#11213));
#1736=EDGE_LOOP('',(#11214));
#1737=EDGE_LOOP('',(#11215));
#1738=EDGE_LOOP('',(#11216,#11217,#11218,#11219));
#1739=EDGE_LOOP('',(#11220,#11221,#11222,#11223));
#1740=EDGE_LOOP('',(#11224));
#1741=EDGE_LOOP('',(#11225));
#1742=EDGE_LOOP('',(#11226));
#1743=EDGE_LOOP('',(#11227));
#1744=EDGE_LOOP('',(#11228));
#1745=EDGE_LOOP('',(#11229,#11230,#11231,#11232));
#1746=EDGE_LOOP('',(#11233,#11234,#11235,#11236));
#1747=EDGE_LOOP('',(#11237,#11238,#11239,#11240));
#1748=EDGE_LOOP('',(#11241,#11242,#11243,#11244));
#1749=EDGE_LOOP('',(#11245,#11246,#11247,#11248));
#1750=EDGE_LOOP('',(#11249,#11250,#11251,#11252));
#1751=EDGE_LOOP('',(#11253,#11254,#11255,#11256));
#1752=EDGE_LOOP('',(#11257,#11258,#11259,#11260));
#1753=EDGE_LOOP('',(#11261,#11262,#11263,#11264));
#1754=EDGE_LOOP('',(#11265,#11266,#11267,#11268));
#1755=EDGE_LOOP('',(#11269,#11270,#11271,#11272));
#1756=EDGE_LOOP('',(#11273,#11274,#11275,#11276));
#1757=EDGE_LOOP('',(#11277,#11278,#11279,#11280));
#1758=EDGE_LOOP('',(#11281,#11282,#11283,#11284));
#1759=EDGE_LOOP('',(#11285,#11286,#11287,#11288));
#1760=EDGE_LOOP('',(#11289,#11290,#11291,#11292));
#1761=EDGE_LOOP('',(#11293,#11294,#11295,#11296));
#1762=EDGE_LOOP('',(#11297,#11298,#11299,#11300));
#1763=EDGE_LOOP('',(#11301,#11302,#11303,#11304));
#1764=EDGE_LOOP('',(#11305,#11306,#11307,#11308));
#1765=EDGE_LOOP('',(#11309,#11310,#11311,#11312));
#1766=EDGE_LOOP('',(#11313,#11314,#11315,#11316));
#1767=EDGE_LOOP('',(#11317,#11318,#11319,#11320));
#1768=EDGE_LOOP('',(#11321,#11322,#11323,#11324));
#1769=EDGE_LOOP('',(#11325,#11326,#11327,#11328));
#1770=EDGE_LOOP('',(#11329,#11330,#11331,#11332));
#1771=EDGE_LOOP('',(#11333,#11334,#11335,#11336));
#1772=EDGE_LOOP('',(#11337,#11338,#11339,#11340));
#1773=EDGE_LOOP('',(#11341,#11342,#11343,#11344));
#1774=EDGE_LOOP('',(#11345,#11346,#11347,#11348));
#1775=EDGE_LOOP('',(#11349,#11350,#11351,#11352));
#1776=EDGE_LOOP('',(#11353,#11354,#11355,#11356));
#1777=EDGE_LOOP('',(#11357,#11358,#11359,#11360));
#1778=EDGE_LOOP('',(#11361,#11362,#11363,#11364));
#1779=EDGE_LOOP('',(#11365,#11366,#11367,#11368));
#1780=EDGE_LOOP('',(#11369,#11370,#11371,#11372));
#1781=EDGE_LOOP('',(#11373,#11374,#11375,#11376));
#1782=EDGE_LOOP('',(#11377,#11378,#11379,#11380));
#1783=EDGE_LOOP('',(#11381,#11382,#11383,#11384));
#1784=EDGE_LOOP('',(#11385,#11386,#11387,#11388));
#1785=EDGE_LOOP('',(#11389,#11390,#11391,#11392));
#1786=EDGE_LOOP('',(#11393,#11394,#11395,#11396));
#1787=EDGE_LOOP('',(#11397,#11398,#11399,#11400));
#1788=EDGE_LOOP('',(#11401,#11402,#11403,#11404));
#1789=EDGE_LOOP('',(#11405,#11406,#11407,#11408));
#1790=EDGE_LOOP('',(#11409,#11410,#11411,#11412));
#1791=EDGE_LOOP('',(#11413,#11414,#11415,#11416));
#1792=EDGE_LOOP('',(#11417,#11418,#11419,#11420));
#1793=EDGE_LOOP('',(#11421,#11422,#11423,#11424));
#1794=EDGE_LOOP('',(#11425,#11426,#11427,#11428));
#1795=EDGE_LOOP('',(#11429,#11430,#11431,#11432));
#1796=EDGE_LOOP('',(#11433,#11434,#11435,#11436));
#1797=EDGE_LOOP('',(#11437,#11438,#11439,#11440));
#1798=EDGE_LOOP('',(#11441,#11442,#11443,#11444));
#1799=EDGE_LOOP('',(#11445,#11446,#11447,#11448));
#1800=EDGE_LOOP('',(#11449,#11450,#11451,#11452));
#1801=EDGE_LOOP('',(#11453,#11454,#11455,#11456));
#1802=EDGE_LOOP('',(#11457,#11458,#11459,#11460));
#1803=EDGE_LOOP('',(#11461,#11462,#11463,#11464));
#1804=EDGE_LOOP('',(#11465,#11466,#11467,#11468));
#1805=EDGE_LOOP('',(#11469,#11470,#11471,#11472,#11473,#11474,#11475,#11476,
#11477,#11478,#11479,#11480,#11481,#11482,#11483,#11484,#11485,#11486,#11487,
#11488,#11489,#11490,#11491,#11492,#11493,#11494,#11495,#11496,#11497,#11498,
#11499,#11500,#11501,#11502,#11503,#11504,#11505,#11506,#11507,#11508,#11509,
#11510,#11511,#11512,#11513,#11514,#11515,#11516,#11517,#11518,#11519,#11520,
#11521,#11522,#11523,#11524,#11525,#11526,#11527,#11528,#11529));
#1806=EDGE_LOOP('',(#11530,#11531,#11532,#11533,#11534,#11535,#11536,#11537,
#11538,#11539,#11540,#11541,#11542,#11543,#11544,#11545,#11546,#11547,#11548,
#11549,#11550,#11551,#11552,#11553,#11554,#11555,#11556,#11557,#11558,#11559,
#11560,#11561,#11562,#11563,#11564,#11565,#11566,#11567,#11568,#11569,#11570,
#11571,#11572,#11573,#11574,#11575,#11576,#11577,#11578,#11579,#11580,#11581,
#11582,#11583,#11584,#11585,#11586,#11587,#11588,#11589,#11590));
#1807=EDGE_LOOP('',(#11591,#11592,#11593,#11594,#11595,#11596,#11597,#11598));
#1808=EDGE_LOOP('',(#11599,#11600,#11601,#11602));
#1809=EDGE_LOOP('',(#11603,#11604,#11605,#11606));
#1810=EDGE_LOOP('',(#11607,#11608,#11609,#11610));
#1811=EDGE_LOOP('',(#11611,#11612,#11613,#11614));
#1812=EDGE_LOOP('',(#11615,#11616,#11617,#11618));
#1813=EDGE_LOOP('',(#11619,#11620,#11621,#11622,#11623,#11624));
#1814=EDGE_LOOP('',(#11625,#11626,#11627,#11628,#11629,#11630));
#1815=EDGE_LOOP('',(#11631,#11632,#11633,#11634));
#1816=EDGE_LOOP('',(#11635,#11636,#11637,#11638));
#1817=EDGE_LOOP('',(#11639,#11640,#11641,#11642));
#1818=EDGE_LOOP('',(#11643,#11644,#11645,#11646));
#1819=EDGE_LOOP('',(#11647,#11648,#11649,#11650,#11651,#11652,#11653,#11654));
#1820=EDGE_LOOP('',(#11655,#11656,#11657,#11658));
#1821=EDGE_LOOP('',(#11659,#11660,#11661,#11662));
#1822=EDGE_LOOP('',(#11663,#11664,#11665,#11666));
#1823=EDGE_LOOP('',(#11667,#11668,#11669,#11670));
#1824=EDGE_LOOP('',(#11671,#11672,#11673,#11674));
#1825=EDGE_LOOP('',(#11675,#11676,#11677,#11678));
#1826=EDGE_LOOP('',(#11679,#11680,#11681,#11682,#11683,#11684,#11685,#11686,
#11687,#11688,#11689,#11690));
#1827=EDGE_LOOP('',(#11691));
#1828=EDGE_LOOP('',(#11692,#11693,#11694,#11695,#11696,#11697,#11698,#11699));
#1829=EDGE_LOOP('',(#11700,#11701,#11702,#11703,#11704,#11705,#11706,#11707));
#1830=EDGE_LOOP('',(#11708,#11709,#11710,#11711));
#1831=EDGE_LOOP('',(#11712,#11713));
#1832=EDGE_LOOP('',(#11714));
#1833=EDGE_LOOP('',(#11715,#11716,#11717,#11718));
#1834=EDGE_LOOP('',(#11719,#11720,#11721,#11722,#11723,#11724,#11725,#11726,
#11727,#11728,#11729,#11730));
#1835=EDGE_LOOP('',(#11731));
#1836=EDGE_LOOP('',(#11732));
#1837=EDGE_LOOP('',(#11733,#11734,#11735,#11736));
#1838=EDGE_LOOP('',(#11737,#11738,#11739,#11740));
#1839=EDGE_LOOP('',(#11741,#11742,#11743,#11744));
#1840=EDGE_LOOP('',(#11745,#11746,#11747,#11748));
#1841=EDGE_LOOP('',(#11749,#11750,#11751,#11752));
#1842=EDGE_LOOP('',(#11753,#11754,#11755,#11756));
#1843=EDGE_LOOP('',(#11757,#11758,#11759,#11760));
#1844=EDGE_LOOP('',(#11761,#11762,#11763,#11764));
#1845=EDGE_LOOP('',(#11765,#11766,#11767,#11768));
#1846=EDGE_LOOP('',(#11769,#11770,#11771,#11772,#11773,#11774));
#1847=EDGE_LOOP('',(#11775,#11776,#11777,#11778));
#1848=EDGE_LOOP('',(#11779,#11780,#11781,#11782,#11783,#11784,#11785,#11786));
#1849=EDGE_LOOP('',(#11787));
#1850=EDGE_LOOP('',(#11788));
#1851=EDGE_LOOP('',(#11789,#11790,#11791,#11792));
#1852=EDGE_LOOP('',(#11793,#11794,#11795,#11796));
#1853=EDGE_LOOP('',(#11797,#11798,#11799,#11800));
#1854=EDGE_LOOP('',(#11801,#11802,#11803,#11804));
#1855=EDGE_LOOP('',(#11805,#11806,#11807,#11808));
#1856=EDGE_LOOP('',(#11809,#11810,#11811,#11812));
#1857=EDGE_LOOP('',(#11813,#11814,#11815,#11816));
#1858=EDGE_LOOP('',(#11817,#11818,#11819,#11820));
#1859=EDGE_LOOP('',(#11821,#11822,#11823,#11824));
#1860=EDGE_LOOP('',(#11825,#11826,#11827,#11828));
#1861=EDGE_LOOP('',(#11829,#11830,#11831,#11832));
#1862=EDGE_LOOP('',(#11833,#11834,#11835,#11836));
#1863=EDGE_LOOP('',(#11837,#11838,#11839,#11840));
#1864=EDGE_LOOP('',(#11841,#11842,#11843,#11844));
#1865=EDGE_LOOP('',(#11845,#11846,#11847,#11848));
#1866=EDGE_LOOP('',(#11849,#11850,#11851,#11852));
#1867=EDGE_LOOP('',(#11853,#11854,#11855,#11856));
#1868=EDGE_LOOP('',(#11857,#11858,#11859,#11860));
#1869=EDGE_LOOP('',(#11861,#11862,#11863,#11864));
#1870=EDGE_LOOP('',(#11865,#11866,#11867,#11868));
#1871=EDGE_LOOP('',(#11869,#11870,#11871,#11872));
#1872=EDGE_LOOP('',(#11873,#11874,#11875,#11876));
#1873=EDGE_LOOP('',(#11877,#11878,#11879,#11880));
#1874=EDGE_LOOP('',(#11881,#11882,#11883,#11884));
#1875=EDGE_LOOP('',(#11885,#11886,#11887,#11888));
#1876=EDGE_LOOP('',(#11889,#11890,#11891,#11892));
#1877=EDGE_LOOP('',(#11893,#11894,#11895,#11896));
#1878=EDGE_LOOP('',(#11897,#11898,#11899,#11900));
#1879=EDGE_LOOP('',(#11901,#11902,#11903,#11904));
#1880=EDGE_LOOP('',(#11905,#11906,#11907,#11908));
#1881=EDGE_LOOP('',(#11909,#11910,#11911,#11912));
#1882=EDGE_LOOP('',(#11913,#11914,#11915,#11916));
#1883=EDGE_LOOP('',(#11917,#11918,#11919,#11920));
#1884=EDGE_LOOP('',(#11921,#11922,#11923,#11924));
#1885=EDGE_LOOP('',(#11925,#11926,#11927,#11928));
#1886=EDGE_LOOP('',(#11929,#11930,#11931,#11932));
#1887=EDGE_LOOP('',(#11933,#11934,#11935,#11936,#11937,#11938,#11939,#11940));
#1888=EDGE_LOOP('',(#11941,#11942,#11943,#11944));
#1889=EDGE_LOOP('',(#11945,#11946,#11947,#11948));
#1890=EDGE_LOOP('',(#11949,#11950,#11951,#11952));
#1891=EDGE_LOOP('',(#11953,#11954,#11955,#11956));
#1892=EDGE_LOOP('',(#11957,#11958,#11959,#11960));
#1893=EDGE_LOOP('',(#11961,#11962,#11963,#11964));
#1894=EDGE_LOOP('',(#11965,#11966,#11967,#11968));
#1895=EDGE_LOOP('',(#11969,#11970,#11971,#11972));
#1896=EDGE_LOOP('',(#11973,#11974,#11975,#11976));
#1897=EDGE_LOOP('',(#11977,#11978,#11979,#11980));
#1898=EDGE_LOOP('',(#11981,#11982,#11983,#11984));
#1899=EDGE_LOOP('',(#11985,#11986,#11987,#11988));
#1900=EDGE_LOOP('',(#11989,#11990,#11991,#11992));
#1901=EDGE_LOOP('',(#11993,#11994,#11995,#11996));
#1902=EDGE_LOOP('',(#11997,#11998,#11999,#12000));
#1903=EDGE_LOOP('',(#12001,#12002,#12003,#12004));
#1904=EDGE_LOOP('',(#12005,#12006,#12007,#12008));
#1905=EDGE_LOOP('',(#12009,#12010,#12011,#12012));
#1906=EDGE_LOOP('',(#12013,#12014,#12015,#12016));
#1907=EDGE_LOOP('',(#12017,#12018,#12019,#12020));
#1908=EDGE_LOOP('',(#12021,#12022,#12023,#12024));
#1909=EDGE_LOOP('',(#12025,#12026,#12027,#12028));
#1910=EDGE_LOOP('',(#12029,#12030,#12031,#12032));
#1911=EDGE_LOOP('',(#12033,#12034,#12035,#12036));
#1912=EDGE_LOOP('',(#12037,#12038,#12039,#12040));
#1913=EDGE_LOOP('',(#12041,#12042,#12043,#12044));
#1914=EDGE_LOOP('',(#12045,#12046,#12047,#12048));
#1915=EDGE_LOOP('',(#12049,#12050,#12051,#12052));
#1916=EDGE_LOOP('',(#12053,#12054,#12055,#12056));
#1917=EDGE_LOOP('',(#12057,#12058,#12059,#12060));
#1918=EDGE_LOOP('',(#12061,#12062,#12063,#12064));
#1919=EDGE_LOOP('',(#12065,#12066,#12067,#12068));
#1920=EDGE_LOOP('',(#12069,#12070,#12071,#12072));
#1921=EDGE_LOOP('',(#12073,#12074,#12075,#12076));
#1922=EDGE_LOOP('',(#12077,#12078,#12079,#12080));
#1923=EDGE_LOOP('',(#12081,#12082,#12083,#12084));
#1924=EDGE_LOOP('',(#12085,#12086,#12087,#12088));
#1925=EDGE_LOOP('',(#12089,#12090,#12091,#12092));
#1926=EDGE_LOOP('',(#12093,#12094,#12095,#12096));
#1927=EDGE_LOOP('',(#12097,#12098,#12099,#12100));
#1928=EDGE_LOOP('',(#12101,#12102,#12103,#12104));
#1929=EDGE_LOOP('',(#12105,#12106,#12107,#12108));
#1930=EDGE_LOOP('',(#12109,#12110,#12111,#12112,#12113,#12114));
#1931=EDGE_LOOP('',(#12115,#12116,#12117,#12118));
#1932=EDGE_LOOP('',(#12119));
#1933=EDGE_LOOP('',(#12120));
#1934=EDGE_LOOP('',(#12121));
#1935=EDGE_LOOP('',(#12122));
#1936=EDGE_LOOP('',(#12123,#12124,#12125,#12126));
#1937=EDGE_LOOP('',(#12127,#12128,#12129,#12130,#12131));
#1938=EDGE_LOOP('',(#12132,#12133,#12134,#12135,#12136,#12137,#12138,#12139,
#12140,#12141,#12142,#12143,#12144,#12145,#12146,#12147,#12148,#12149,#12150,
#12151,#12152,#12153,#12154,#12155,#12156,#12157,#12158,#12159,#12160,#12161,
#12162,#12163,#12164,#12165,#12166,#12167,#12168,#12169,#12170,#12171,#12172,
#12173,#12174,#12175,#12176,#12177,#12178,#12179,#12180,#12181,#12182,#12183,
#12184,#12185,#12186,#12187,#12188,#12189,#12190,#12191,#12192,#12193,#12194,
#12195,#12196,#12197,#12198,#12199,#12200,#12201,#12202,#12203,#12204,#12205,
#12206,#12207,#12208));
#1939=EDGE_LOOP('',(#12209,#12210,#12211,#12212));
#1940=EDGE_LOOP('',(#12213,#12214,#12215,#12216,#12217,#12218,#12219,#12220,
#12221,#12222,#12223,#12224,#12225,#12226,#12227,#12228,#12229,#12230,#12231,
#12232,#12233,#12234,#12235,#12236,#12237,#12238,#12239,#12240,#12241,#12242,
#12243,#12244,#12245,#12246,#12247,#12248,#12249,#12250,#12251,#12252,#12253,
#12254,#12255,#12256,#12257,#12258,#12259,#12260,#12261,#12262,#12263,#12264,
#12265,#12266,#12267,#12268,#12269,#12270,#12271,#12272,#12273,#12274,#12275,
#12276,#12277,#12278,#12279,#12280,#12281,#12282,#12283,#12284,#12285,#12286,
#12287,#12288,#12289));
#1941=EDGE_LOOP('',(#12290,#12291,#12292,#12293));
#1942=EDGE_LOOP('',(#12294));
#1943=EDGE_LOOP('',(#12295));
#1944=EDGE_LOOP('',(#12296,#12297,#12298,#12299));
#1945=EDGE_LOOP('',(#12300));
#1946=EDGE_LOOP('',(#12301,#12302,#12303,#12304,#12305,#12306));
#1947=EDGE_LOOP('',(#12307,#12308,#12309,#12310));
#1948=EDGE_LOOP('',(#12311,#12312,#12313,#12314));
#1949=EDGE_LOOP('',(#12315,#12316,#12317,#12318));
#1950=EDGE_LOOP('',(#12319,#12320,#12321,#12322));
#1951=EDGE_LOOP('',(#12323,#12324,#12325,#12326));
#1952=EDGE_LOOP('',(#12327,#12328,#12329,#12330));
#1953=EDGE_LOOP('',(#12331,#12332,#12333,#12334));
#1954=EDGE_LOOP('',(#12335,#12336,#12337,#12338));
#1955=EDGE_LOOP('',(#12339,#12340,#12341,#12342));
#1956=EDGE_LOOP('',(#12343));
#1957=EDGE_LOOP('',(#12344));
#1958=EDGE_LOOP('',(#12345));
#1959=EDGE_LOOP('',(#12346));
#1960=EDGE_LOOP('',(#12347,#12348,#12349,#12350));
#1961=EDGE_LOOP('',(#12351,#12352,#12353,#12354));
#1962=EDGE_LOOP('',(#12355));
#1963=EDGE_LOOP('',(#12356));
#1964=EDGE_LOOP('',(#12357));
#1965=EDGE_LOOP('',(#12358));
#1966=EDGE_LOOP('',(#12359,#12360,#12361,#12362));
#1967=EDGE_LOOP('',(#12363,#12364,#12365,#12366));
#1968=EDGE_LOOP('',(#12367,#12368,#12369,#12370));
#1969=EDGE_LOOP('',(#12371,#12372,#12373,#12374));
#1970=EDGE_LOOP('',(#12375,#12376,#12377,#12378));
#1971=EDGE_LOOP('',(#12379,#12380,#12381,#12382));
#1972=EDGE_LOOP('',(#12383,#12384,#12385,#12386));
#1973=EDGE_LOOP('',(#12387,#12388,#12389,#12390));
#1974=EDGE_LOOP('',(#12391,#12392,#12393,#12394));
#1975=EDGE_LOOP('',(#12395,#12396,#12397,#12398));
#1976=EDGE_LOOP('',(#12399,#12400,#12401,#12402));
#1977=EDGE_LOOP('',(#12403,#12404,#12405,#12406));
#1978=EDGE_LOOP('',(#12407,#12408,#12409,#12410));
#1979=EDGE_LOOP('',(#12411,#12412,#12413,#12414));
#1980=EDGE_LOOP('',(#12415,#12416,#12417,#12418));
#1981=EDGE_LOOP('',(#12419,#12420,#12421,#12422));
#1982=EDGE_LOOP('',(#12423,#12424,#12425,#12426));
#1983=EDGE_LOOP('',(#12427,#12428,#12429,#12430));
#1984=EDGE_LOOP('',(#12431,#12432,#12433,#12434));
#1985=EDGE_LOOP('',(#12435,#12436,#12437,#12438));
#1986=EDGE_LOOP('',(#12439,#12440,#12441,#12442));
#1987=EDGE_LOOP('',(#12443,#12444,#12445,#12446));
#1988=EDGE_LOOP('',(#12447,#12448,#12449,#12450));
#1989=EDGE_LOOP('',(#12451,#12452,#12453,#12454));
#1990=EDGE_LOOP('',(#12455,#12456,#12457,#12458));
#1991=EDGE_LOOP('',(#12459,#12460,#12461,#12462));
#1992=EDGE_LOOP('',(#12463,#12464,#12465,#12466));
#1993=EDGE_LOOP('',(#12467,#12468,#12469,#12470));
#1994=EDGE_LOOP('',(#12471,#12472,#12473,#12474));
#1995=EDGE_LOOP('',(#12475,#12476,#12477,#12478));
#1996=EDGE_LOOP('',(#12479,#12480,#12481,#12482));
#1997=EDGE_LOOP('',(#12483,#12484,#12485,#12486));
#1998=EDGE_LOOP('',(#12487,#12488,#12489,#12490));
#1999=EDGE_LOOP('',(#12491,#12492,#12493,#12494));
#2000=EDGE_LOOP('',(#12495,#12496,#12497,#12498));
#2001=EDGE_LOOP('',(#12499,#12500,#12501,#12502));
#2002=EDGE_LOOP('',(#12503,#12504,#12505,#12506));
#2003=EDGE_LOOP('',(#12507,#12508,#12509,#12510));
#2004=EDGE_LOOP('',(#12511,#12512,#12513,#12514));
#2005=EDGE_LOOP('',(#12515,#12516,#12517,#12518));
#2006=EDGE_LOOP('',(#12519,#12520,#12521,#12522));
#2007=EDGE_LOOP('',(#12523,#12524,#12525,#12526));
#2008=EDGE_LOOP('',(#12527,#12528,#12529,#12530));
#2009=EDGE_LOOP('',(#12531,#12532,#12533,#12534));
#2010=EDGE_LOOP('',(#12535,#12536,#12537,#12538));
#2011=EDGE_LOOP('',(#12539,#12540,#12541,#12542));
#2012=EDGE_LOOP('',(#12543,#12544,#12545,#12546));
#2013=EDGE_LOOP('',(#12547,#12548,#12549,#12550));
#2014=EDGE_LOOP('',(#12551,#12552,#12553,#12554));
#2015=EDGE_LOOP('',(#12555,#12556,#12557,#12558));
#2016=EDGE_LOOP('',(#12559,#12560,#12561,#12562));
#2017=EDGE_LOOP('',(#12563,#12564,#12565,#12566));
#2018=EDGE_LOOP('',(#12567,#12568,#12569,#12570));
#2019=EDGE_LOOP('',(#12571,#12572,#12573,#12574));
#2020=EDGE_LOOP('',(#12575,#12576,#12577,#12578));
#2021=EDGE_LOOP('',(#12579,#12580,#12581,#12582));
#2022=EDGE_LOOP('',(#12583,#12584,#12585,#12586));
#2023=EDGE_LOOP('',(#12587,#12588,#12589,#12590));
#2024=EDGE_LOOP('',(#12591,#12592,#12593,#12594));
#2025=EDGE_LOOP('',(#12595,#12596,#12597,#12598));
#2026=EDGE_LOOP('',(#12599,#12600,#12601,#12602));
#2027=EDGE_LOOP('',(#12603,#12604,#12605,#12606));
#2028=EDGE_LOOP('',(#12607,#12608,#12609,#12610));
#2029=EDGE_LOOP('',(#12611,#12612,#12613,#12614));
#2030=EDGE_LOOP('',(#12615,#12616,#12617,#12618));
#2031=EDGE_LOOP('',(#12619,#12620,#12621,#12622));
#2032=EDGE_LOOP('',(#12623,#12624,#12625,#12626));
#2033=EDGE_LOOP('',(#12627,#12628,#12629,#12630));
#2034=EDGE_LOOP('',(#12631,#12632,#12633,#12634));
#2035=EDGE_LOOP('',(#12635,#12636,#12637,#12638));
#2036=EDGE_LOOP('',(#12639,#12640,#12641,#12642));
#2037=EDGE_LOOP('',(#12643,#12644,#12645,#12646));
#2038=EDGE_LOOP('',(#12647,#12648,#12649,#12650));
#2039=EDGE_LOOP('',(#12651,#12652,#12653,#12654));
#2040=EDGE_LOOP('',(#12655,#12656,#12657,#12658));
#2041=EDGE_LOOP('',(#12659,#12660,#12661,#12662));
#2042=EDGE_LOOP('',(#12663,#12664,#12665,#12666));
#2043=EDGE_LOOP('',(#12667,#12668,#12669,#12670));
#2044=EDGE_LOOP('',(#12671,#12672,#12673,#12674,#12675,#12676,#12677,#12678));
#2045=EDGE_LOOP('',(#12679,#12680,#12681,#12682,#12683,#12684,#12685,#12686,
#12687,#12688,#12689,#12690,#12691,#12692,#12693,#12694,#12695,#12696,#12697,
#12698,#12699,#12700,#12701,#12702,#12703,#12704,#12705,#12706,#12707,#12708,
#12709,#12710,#12711,#12712,#12713,#12714,#12715,#12716,#12717,#12718,#12719,
#12720,#12721,#12722,#12723,#12724,#12725,#12726,#12727,#12728,#12729,#12730,
#12731,#12732,#12733,#12734,#12735,#12736,#12737,#12738,#12739,#12740,#12741,
#12742,#12743,#12744,#12745,#12746,#12747,#12748,#12749,#12750,#12751,#12752,
#12753,#12754,#12755,#12756,#12757,#12758,#12759,#12760));
#2046=EDGE_LOOP('',(#12761,#12762,#12763,#12764));
#2047=EDGE_LOOP('',(#12765,#12766,#12767,#12768,#12769,#12770,#12771,#12772,
#12773,#12774,#12775,#12776,#12777,#12778,#12779,#12780,#12781,#12782,#12783,
#12784,#12785,#12786,#12787,#12788,#12789,#12790,#12791,#12792,#12793,#12794,
#12795,#12796,#12797,#12798,#12799,#12800,#12801,#12802,#12803,#12804,#12805,
#12806,#12807,#12808,#12809,#12810,#12811,#12812,#12813,#12814,#12815,#12816,
#12817,#12818,#12819,#12820,#12821,#12822,#12823,#12824,#12825,#12826,#12827,
#12828,#12829,#12830,#12831,#12832,#12833,#12834,#12835,#12836,#12837,#12838,
#12839,#12840,#12841,#12842,#12843,#12844,#12845,#12846,#12847));
#2048=EDGE_LOOP('',(#12848,#12849,#12850,#12851));
#2049=EDGE_LOOP('',(#12852,#12853,#12854,#12855));
#2050=EDGE_LOOP('',(#12856,#12857,#12858,#12859));
#2051=EDGE_LOOP('',(#12860,#12861,#12862,#12863));
#2052=EDGE_LOOP('',(#12864,#12865,#12866,#12867));
#2053=EDGE_LOOP('',(#12868,#12869,#12870,#12871));
#2054=EDGE_LOOP('',(#12872,#12873,#12874,#12875));
#2055=EDGE_LOOP('',(#12876,#12877,#12878,#12879,#12880,#12881));
#2056=EDGE_LOOP('',(#12882));
#2057=EDGE_LOOP('',(#12883,#12884,#12885,#12886));
#2058=EDGE_LOOP('',(#12887,#12888,#12889,#12890));
#2059=EDGE_LOOP('',(#12891));
#2060=EDGE_LOOP('',(#12892,#12893,#12894,#12895,#12896,#12897));
#2061=EDGE_LOOP('',(#12898));
#2062=EDGE_LOOP('',(#12899,#12900,#12901,#12902));
#2063=EDGE_LOOP('',(#12903,#12904,#12905,#12906));
#2064=EDGE_LOOP('',(#12907));
#2065=EDGE_LOOP('',(#12908));
#2066=EDGE_LOOP('',(#12909));
#2067=EDGE_LOOP('',(#12910));
#2068=EDGE_LOOP('',(#12911,#12912,#12913,#12914));
#2069=EDGE_LOOP('',(#12915,#12916,#12917,#12918));
#2070=EDGE_LOOP('',(#12919,#12920,#12921,#12922));
#2071=EDGE_LOOP('',(#12923,#12924,#12925,#12926));
#2072=EDGE_LOOP('',(#12927,#12928,#12929,#12930));
#2073=EDGE_LOOP('',(#12931,#12932,#12933,#12934));
#2074=EDGE_LOOP('',(#12935,#12936,#12937,#12938));
#2075=EDGE_LOOP('',(#12939,#12940,#12941,#12942));
#2076=EDGE_LOOP('',(#12943,#12944,#12945,#12946));
#2077=EDGE_LOOP('',(#12947,#12948,#12949,#12950));
#2078=EDGE_LOOP('',(#12951,#12952,#12953,#12954));
#2079=EDGE_LOOP('',(#12955,#12956,#12957,#12958));
#2080=EDGE_LOOP('',(#12959,#12960,#12961,#12962));
#2081=EDGE_LOOP('',(#12963,#12964,#12965,#12966));
#2082=EDGE_LOOP('',(#12967,#12968,#12969,#12970));
#2083=EDGE_LOOP('',(#12971,#12972,#12973,#12974));
#2084=EDGE_LOOP('',(#12975,#12976,#12977,#12978));
#2085=EDGE_LOOP('',(#12979,#12980,#12981,#12982));
#2086=EDGE_LOOP('',(#12983,#12984,#12985,#12986));
#2087=EDGE_LOOP('',(#12987,#12988,#12989,#12990));
#2088=EDGE_LOOP('',(#12991,#12992,#12993,#12994));
#2089=EDGE_LOOP('',(#12995,#12996,#12997,#12998));
#2090=EDGE_LOOP('',(#12999,#13000,#13001,#13002));
#2091=EDGE_LOOP('',(#13003,#13004,#13005,#13006));
#2092=EDGE_LOOP('',(#13007,#13008,#13009,#13010));
#2093=EDGE_LOOP('',(#13011,#13012,#13013,#13014));
#2094=EDGE_LOOP('',(#13015,#13016,#13017,#13018));
#2095=EDGE_LOOP('',(#13019,#13020,#13021,#13022));
#2096=EDGE_LOOP('',(#13023,#13024,#13025,#13026));
#2097=EDGE_LOOP('',(#13027,#13028,#13029,#13030));
#2098=EDGE_LOOP('',(#13031,#13032,#13033,#13034));
#2099=EDGE_LOOP('',(#13035,#13036,#13037,#13038,#13039));
#2100=EDGE_LOOP('',(#13040,#13041,#13042));
#2101=EDGE_LOOP('',(#13043,#13044,#13045,#13046,#13047));
#2102=EDGE_LOOP('',(#13048,#13049,#13050,#13051));
#2103=EDGE_LOOP('',(#13052,#13053,#13054,#13055));
#2104=EDGE_LOOP('',(#13056,#13057,#13058,#13059));
#2105=EDGE_LOOP('',(#13060,#13061,#13062,#13063));
#2106=EDGE_LOOP('',(#13064,#13065,#13066,#13067));
#2107=EDGE_LOOP('',(#13068,#13069,#13070,#13071));
#2108=EDGE_LOOP('',(#13072,#13073,#13074,#13075));
#2109=EDGE_LOOP('',(#13076,#13077,#13078,#13079));
#2110=EDGE_LOOP('',(#13080,#13081,#13082,#13083));
#2111=EDGE_LOOP('',(#13084,#13085,#13086,#13087));
#2112=EDGE_LOOP('',(#13088,#13089,#13090,#13091));
#2113=EDGE_LOOP('',(#13092,#13093,#13094,#13095));
#2114=EDGE_LOOP('',(#13096,#13097,#13098,#13099));
#2115=EDGE_LOOP('',(#13100,#13101,#13102,#13103));
#2116=EDGE_LOOP('',(#13104,#13105,#13106,#13107));
#2117=EDGE_LOOP('',(#13108,#13109,#13110,#13111));
#2118=EDGE_LOOP('',(#13112,#13113,#13114,#13115));
#2119=EDGE_LOOP('',(#13116,#13117,#13118,#13119));
#2120=EDGE_LOOP('',(#13120,#13121,#13122,#13123));
#2121=EDGE_LOOP('',(#13124,#13125,#13126,#13127));
#2122=EDGE_LOOP('',(#13128,#13129,#13130,#13131));
#2123=EDGE_LOOP('',(#13132,#13133,#13134,#13135));
#2124=EDGE_LOOP('',(#13136,#13137,#13138,#13139));
#2125=EDGE_LOOP('',(#13140,#13141,#13142,#13143));
#2126=EDGE_LOOP('',(#13144,#13145,#13146,#13147));
#2127=EDGE_LOOP('',(#13148,#13149,#13150,#13151));
#2128=EDGE_LOOP('',(#13152,#13153,#13154,#13155));
#2129=EDGE_LOOP('',(#13156,#13157,#13158,#13159));
#2130=EDGE_LOOP('',(#13160,#13161,#13162,#13163));
#2131=EDGE_LOOP('',(#13164,#13165,#13166,#13167));
#2132=EDGE_LOOP('',(#13168,#13169,#13170,#13171,#13172,#13173,#13174,#13175,
#13176));
#2133=EDGE_LOOP('',(#13177,#13178,#13179));
#2134=EDGE_LOOP('',(#13180,#13181,#13182,#13183,#13184,#13185,#13186,#13187,
#13188,#13189,#13190,#13191,#13192,#13193,#13194,#13195,#13196,#13197,#13198,
#13199,#13200,#13201,#13202,#13203,#13204,#13205,#13206,#13207,#13208,#13209,
#13210,#13211,#13212,#13213,#13214,#13215,#13216,#13217,#13218,#13219,#13220,
#13221,#13222,#13223,#13224,#13225,#13226,#13227,#13228,#13229,#13230,#13231,
#13232,#13233,#13234,#13235,#13236,#13237,#13238,#13239,#13240,#13241,#13242,
#13243,#13244,#13245,#13246,#13247));
#2135=EDGE_LOOP('',(#13248,#13249,#13250,#13251));
#2136=EDGE_LOOP('',(#13252,#13253,#13254,#13255,#13256,#13257,#13258,#13259,
#13260,#13261,#13262,#13263,#13264,#13265,#13266,#13267,#13268,#13269,#13270,
#13271,#13272,#13273,#13274,#13275,#13276,#13277,#13278,#13279,#13280,#13281,
#13282,#13283,#13284,#13285,#13286,#13287,#13288,#13289,#13290,#13291,#13292,
#13293,#13294,#13295,#13296,#13297,#13298,#13299,#13300,#13301,#13302,#13303,
#13304,#13305,#13306,#13307,#13308,#13309,#13310,#13311,#13312,#13313,#13314,
#13315,#13316,#13317,#13318));
#2137=EDGE_LOOP('',(#13319,#13320,#13321));
#2138=EDGE_LOOP('',(#13322,#13323,#13324,#13325));
#2139=EDGE_LOOP('',(#13326,#13327,#13328,#13329));
#2140=EDGE_LOOP('',(#13330,#13331,#13332,#13333));
#2141=EDGE_LOOP('',(#13334,#13335,#13336,#13337));
#2142=EDGE_LOOP('',(#13338,#13339,#13340,#13341));
#2143=EDGE_LOOP('',(#13342,#13343,#13344,#13345));
#2144=EDGE_LOOP('',(#13346,#13347,#13348,#13349,#13350,#13351));
#2145=EDGE_LOOP('',(#13352));
#2146=EDGE_LOOP('',(#13353,#13354,#13355,#13356));
#2147=EDGE_LOOP('',(#13357,#13358,#13359,#13360));
#2148=EDGE_LOOP('',(#13361));
#2149=EDGE_LOOP('',(#13362,#13363,#13364,#13365,#13366,#13367));
#2150=EDGE_LOOP('',(#13368));
#2151=CIRCLE('',#14867,2.5175);
#2152=CIRCLE('',#14868,2.5175);
#2153=CIRCLE('',#14869,2.5175);
#2154=CIRCLE('',#14878,2.5175);
#2155=CIRCLE('',#14880,3.07349999999999);
#2156=CIRCLE('',#14889,3.0735);
#2157=CIRCLE('',#14891,2.5175);
#2158=CIRCLE('',#14892,2.5175);
#2159=CIRCLE('',#14893,2.5175);
#2160=CIRCLE('',#14902,2.5175);
#2161=CIRCLE('',#14904,3.07349999999999);
#2162=CIRCLE('',#14913,3.0735);
#2163=CIRCLE('',#14915,2.5175);
#2164=CIRCLE('',#14916,2.5175);
#2165=CIRCLE('',#14917,2.5175);
#2166=CIRCLE('',#14926,2.5175);
#2167=CIRCLE('',#14928,3.0735);
#2168=CIRCLE('',#14937,3.0735);
#2169=CIRCLE('',#14939,2.5175);
#2170=CIRCLE('',#14940,2.5175);
#2171=CIRCLE('',#14941,2.5175);
#2172=CIRCLE('',#14950,2.5175);
#2173=CIRCLE('',#14952,3.0735);
#2174=CIRCLE('',#14961,3.0735);
#2175=CIRCLE('',#14963,2.5175);
#2176=CIRCLE('',#14964,2.5175);
#2177=CIRCLE('',#14965,2.5175);
#2178=CIRCLE('',#14974,2.5175);
#2179=CIRCLE('',#14976,3.07349999999999);
#2180=CIRCLE('',#14985,3.0735);
#2181=CIRCLE('',#14987,2.5175);
#2182=CIRCLE('',#14988,2.5175);
#2183=CIRCLE('',#14989,2.5175);
#2184=CIRCLE('',#14998,2.5175);
#2185=CIRCLE('',#15000,3.0735);
#2186=CIRCLE('',#15009,3.0735);
#2187=CIRCLE('',#15011,2.5175);
#2188=CIRCLE('',#15012,2.5175);
#2189=CIRCLE('',#15013,2.5175);
#2190=CIRCLE('',#15022,2.5175);
#2191=CIRCLE('',#15024,3.0735);
#2192=CIRCLE('',#15033,3.0735);
#2193=CIRCLE('',#15035,2.5175);
#2194=CIRCLE('',#15036,2.5175);
#2195=CIRCLE('',#15037,2.5175);
#2196=CIRCLE('',#15046,2.5175);
#2197=CIRCLE('',#15048,3.07349999999999);
#2198=CIRCLE('',#15057,3.0735);
#2199=CIRCLE('',#15059,7.);
#2200=CIRCLE('',#15060,7.);
#2201=CIRCLE('',#15062,4.5);
#2202=CIRCLE('',#15064,7.);
#2203=CIRCLE('',#15065,7.);
#2204=CIRCLE('',#15067,4.5);
#2205=CIRCLE('',#15069,7.);
#2206=CIRCLE('',#15070,7.);
#2207=CIRCLE('',#15072,4.5);
#2208=CIRCLE('',#15074,7.);
#2209=CIRCLE('',#15075,7.);
#2210=CIRCLE('',#15077,4.5);
#2211=CIRCLE('',#15079,4.5);
#2212=CIRCLE('',#15081,4.5);
#2213=CIRCLE('',#15083,4.5);
#2214=CIRCLE('',#15085,4.5);
#2215=CIRCLE('',#15114,100.);
#2216=CIRCLE('',#15119,100.);
#2217=CIRCLE('',#15121,20.);
#2218=CIRCLE('',#15124,100.);
#2219=CIRCLE('',#15125,20.);
#2220=CIRCLE('',#15127,20.);
#2221=CIRCLE('',#15128,100.);
#2222=CIRCLE('',#15132,20.);
#2223=CIRCLE('',#15137,100.);
#2224=CIRCLE('',#15138,20.);
#2225=CIRCLE('',#15144,20.);
#2226=CIRCLE('',#15145,20.);
#2227=CIRCLE('',#15146,20.);
#2228=CIRCLE('',#15147,20.);
#2229=CIRCLE('',#15148,20.);
#2230=CIRCLE('',#15157,100.);
#2231=CIRCLE('',#15158,100.);
#2232=CIRCLE('',#15165,100.);
#2233=CIRCLE('',#15170,100.);
#2234=CIRCLE('',#15171,100.);
#2235=CIRCLE('',#15189,40.);
#2236=CIRCLE('',#15190,40.);
#2237=CIRCLE('',#15195,3.38975);
#2238=CIRCLE('',#15196,3.38975);
#2239=CIRCLE('',#15197,3.38975);
#2240=CIRCLE('',#15204,3.38975);
#2241=CIRCLE('',#15206,4.085);
#2242=CIRCLE('',#15213,4.085);
#2243=CIRCLE('',#15215,3.38975);
#2244=CIRCLE('',#15216,3.38975);
#2245=CIRCLE('',#15217,3.38975);
#2246=CIRCLE('',#15224,3.38975);
#2247=CIRCLE('',#15226,4.085);
#2248=CIRCLE('',#15233,4.085);
#2249=CIRCLE('',#15235,3.38975);
#2250=CIRCLE('',#15236,3.38975);
#2251=CIRCLE('',#15237,3.38975);
#2252=CIRCLE('',#15244,3.38975);
#2253=CIRCLE('',#15246,4.085);
#2254=CIRCLE('',#15253,4.085);
#2255=CIRCLE('',#15255,3.38975);
#2256=CIRCLE('',#15256,3.38975);
#2257=CIRCLE('',#15257,3.38975);
#2258=CIRCLE('',#15264,3.38975);
#2259=CIRCLE('',#15266,4.085);
#2260=CIRCLE('',#15273,4.085);
#2261=CIRCLE('',#15275,4.263);
#2262=CIRCLE('',#15276,4.263);
#2263=CIRCLE('',#15280,4.263);
#2264=CIRCLE('',#15282,5.099);
#2265=CIRCLE('',#15287,5.099);
#2266=CIRCLE('',#15289,4.263);
#2267=CIRCLE('',#15290,4.263);
#2268=CIRCLE('',#15294,4.263);
#2269=CIRCLE('',#15296,5.099);
#2270=CIRCLE('',#15301,5.099);
#2271=CIRCLE('',#15303,4.263);
#2272=CIRCLE('',#15304,4.263);
#2273=CIRCLE('',#15308,4.263);
#2274=CIRCLE('',#15310,5.099);
#2275=CIRCLE('',#15315,5.099);
#2276=CIRCLE('',#15317,4.263);
#2277=CIRCLE('',#15318,4.263);
#2278=CIRCLE('',#15322,4.263);
#2279=CIRCLE('',#15324,5.099);
#2280=CIRCLE('',#15329,5.099);
#2281=CIRCLE('',#15359,40.);
#2282=CIRCLE('',#15360,40.);
#2283=CIRCLE('',#15362,20.);
#2284=CIRCLE('',#15364,20.);
#2285=CIRCLE('',#15366,110.);
#2286=CIRCLE('',#15367,110.);
#2287=CIRCLE('',#15372,5.13675);
#2288=CIRCLE('',#15400,5.13675);
#2289=CIRCLE('',#15402,6.11324999999999);
#2290=CIRCLE('',#15431,6.11325);
#2291=CIRCLE('',#15448,3.5);
#2292=CIRCLE('',#15449,3.5);
#2293=CIRCLE('',#15451,3.5);
#2294=CIRCLE('',#15452,3.5);
#2295=CIRCLE('',#15454,11.);
#2296=CIRCLE('',#15455,11.);
#2297=CIRCLE('',#15457,11.);
#2298=CIRCLE('',#15458,11.);
#2299=CIRCLE('',#15460,7.);
#2300=CIRCLE('',#15465,11.);
#2301=CIRCLE('',#15466,7.);
#2302=CIRCLE('',#15468,11.);
#2303=CIRCLE('',#15484,5.91675);
#2304=CIRCLE('',#15521,5.91675);
#2305=CIRCLE('',#15522,5.91675);
#2306=CIRCLE('',#15523,5.91675);
#2307=CIRCLE('',#15525,4.91825);
#2308=CIRCLE('',#15569,5.);
#2309=CIRCLE('',#15570,5.);
#2310=CIRCLE('',#15573,5.91675);
#2311=CIRCLE('',#15575,5.91675);
#2312=CIRCLE('',#15578,4.91825);
#2313=CIRCLE('',#15581,10.);
#2314=CIRCLE('',#15583,10.);
#2315=CIRCLE('',#15590,9.);
#2316=CIRCLE('',#15591,5.);
#2317=CIRCLE('',#15593,5.);
#2318=CIRCLE('',#15595,9.);
#2319=CIRCLE('',#15599,6.);
#2320=CIRCLE('',#15600,6.);
#2321=CIRCLE('',#15602,7.);
#2322=CIRCLE('',#15603,7.);
#2323=CIRCLE('',#15608,6.);
#2324=CIRCLE('',#15609,6.);
#2325=CIRCLE('',#15611,10.);
#2326=CIRCLE('',#15612,10.);
#2327=CIRCLE('',#15617,2.942);
#2328=CIRCLE('',#15657,2.37175);
#2329=CIRCLE('',#15697,2.942);
#2330=CIRCLE('',#15698,2.);
#2331=CIRCLE('',#15700,2.37175);
#2332=CIRCLE('',#15710,5.);
#2333=CIRCLE('',#15712,5.);
#2334=CIRCLE('',#15717,3.5);
#2335=CIRCLE('',#15718,3.5);
#2336=CIRCLE('',#15720,7.);
#2337=CIRCLE('',#15721,7.);
#2338=CIRCLE('',#15726,3.933);
#2339=CIRCLE('',#15758,3.933);
#2340=CIRCLE('',#15760,3.22275);
#2341=CIRCLE('',#15762,3.22275);
#2342=CIRCLE('',#15794,3.933);
#2343=CIRCLE('',#15795,3.);
#2344=CIRCLE('',#15798,3.22275);
#2345=CIRCLE('',#15808,6.5);
#2346=CIRCLE('',#15810,6.5);
#2347=B_SPLINE_CURVE_WITH_KNOTS('',3,(#18716,#18717,#18718,#18719),
 .UNSPECIFIED.,.F.,.F.,(4,4),(57.8582309055934,58.5656126576447),
 .UNSPECIFIED.);
#2348=B_SPLINE_CURVE_WITH_KNOTS('',3,(#18727,#18728,#18729,#18730,#18731,
#18732,#18733,#18734,#18735,#18736),.UNSPECIFIED.,.F.,.F.,(4,3,3,4),(-56.5486677646163,
-55.5877001496289,-54.595062646957,-54.1144568630778),.UNSPECIFIED.);
#2349=B_SPLINE_CURVE_WITH_KNOTS('',3,(#18741,#18742,#18743,#18744,#18745,
#18746,#18747,#18748,#18749,#18750,#18751,#18752,#18753,#18754,#18755,#18756,
#18757,#18758,#18759,#18760,#18761,#18762,#18763,#18764,#18765),
 .UNSPECIFIED.,.F.,.F.,(4,3,3,3,3,3,3,3,4),(51.5750455984138,51.6171501389411,
52.6097876416131,53.602425144285,54.595062646957,55.5877001496289,56.5803376523009,
57.5729751549728,57.8582309055934),.UNSPECIFIED.);
#2350=B_SPLINE_CURVE_WITH_KNOTS('',3,(#18766,#18767,#18768,#18769,#18770,
#18771,#18772,#18773,#18774,#18775,#18776,#18777,#18778,#18779,#18780,#18781,
#18782,#18783,#18784,#18785,#18786,#18787),.UNSPECIFIED.,.F.,.F.,(4,3,3,
3,3,3,3,4),(-54.1144568630778,-53.602425144285,-52.6097876416131,-51.6171501389411,
-50.6245126362692,-49.6318751335972,-48.6392376309253,-47.8312715558982),
 .UNSPECIFIED.);
#2351=B_SPLINE_CURVE_WITH_KNOTS('',3,(#18792,#18793,#18794,#18795,#18796,
#18797,#18798,#18799,#18800,#18801,#18802,#18803,#18804,#18805,#18806,#18807,
#18808,#18809,#18810,#18811,#18812,#18813),.UNSPECIFIED.,.F.,.F.,(4,3,3,
3,3,3,3,4),(45.2918602912342,45.6613251229095,46.6539626255814,47.6466001282533,
48.6392376309253,49.6318751335972,50.6245126362692,51.5750455984138),
 .UNSPECIFIED.);
#2352=B_SPLINE_CURVE_WITH_KNOTS('',3,(#18814,#18815,#18816,#18817,#18818,
#18819,#18820,#18821,#18822,#18823,#18824,#18825,#18826,#18827,#18828,#18829,
#18830,#18831,#18832,#18833,#18834,#18835,#18836,#18837,#18838),
 .UNSPECIFIED.,.F.,.F.,(4,3,3,3,3,3,3,3,4),(-47.8312715558982,-47.6466001282533,
-46.6539626255814,-45.6613251229095,-44.6686876202375,-43.6760501175656,
-42.6834126148936,-41.6907751122217,-41.5480862487187),.UNSPECIFIED.);
#2353=B_SPLINE_CURVE_WITH_KNOTS('',3,(#18843,#18844,#18845,#18846,#18847,
#18848,#18849,#18850,#18851,#18852,#18853,#18854,#18855,#18856,#18857,#18858,
#18859,#18860,#18861,#18862,#18863,#18864),.UNSPECIFIED.,.F.,.F.,(4,3,3,
3,3,3,3,4),(39.0086749840546,39.7055001068778,40.6981376095497,41.6907751122217,
42.6834126148936,43.6760501175656,44.6686876202375,45.2918602912342),
 .UNSPECIFIED.);
#2354=B_SPLINE_CURVE_WITH_KNOTS('',3,(#18865,#18866,#18867,#18868,#18869,
#18870,#18871,#18872,#18873,#18874,#18875,#18876,#18877,#18878,#18879,#18880,
#18881,#18882,#18883,#18884,#18885,#18886),.UNSPECIFIED.,.F.,.F.,(4,3,3,
3,3,3,3,4),(-41.5480862487187,-40.6981376095497,-39.7055001068778,-38.7128626042058,
-37.7202251015339,-36.727587598862,-35.73495009619,-35.2649009415391),
 .UNSPECIFIED.);
#2355=B_SPLINE_CURVE_WITH_KNOTS('',3,(#18891,#18892,#18893,#18894,#18895,
#18896,#18897,#18898,#18899,#18900,#18901,#18902,#18903,#18904,#18905,#18906,
#18907,#18908,#18909,#18910,#18911,#18912,#18913,#18914,#18915),
 .UNSPECIFIED.,.F.,.F.,(4,3,3,3,3,3,3,3,4),(32.725489676875,32.7570375881742,
33.7496750908461,34.7423125935181,35.73495009619,36.727587598862,37.7202251015339,
38.7128626042058,39.0086749840546),.UNSPECIFIED.);
#2356=B_SPLINE_CURVE_WITH_KNOTS('',3,(#18916,#18917,#18918,#18919,#18920,
#18921,#18922,#18923,#18924,#18925,#18926,#18927,#18928,#18929,#18930,#18931,
#18932,#18933,#18934,#18935,#18936,#18937),.UNSPECIFIED.,.F.,.F.,(4,3,3,
3,3,3,3,4),(-35.2649009415391,-34.7423125935181,-33.7496750908461,-32.7570375881742,
-31.7644000855022,-30.7717625828303,-29.7791250801584,-28.9817156343595),
 .UNSPECIFIED.);
#2357=B_SPLINE_CURVE_WITH_KNOTS('',3,(#18942,#18943,#18944,#18945,#18946,
#18947,#18948,#18949,#18950,#18951,#18952,#18953,#18954,#18955,#18956,#18957,
#18958,#18959,#18960,#18961,#18962,#18963),.UNSPECIFIED.,.F.,.F.,(4,3,3,
3,3,3,3,4),(26.4423043696954,26.8012125721425,27.7938500748145,28.7864875774864,
29.7791250801583,30.7717625828303,31.7644000855022,32.725489676875),
 .UNSPECIFIED.);
#2358=B_SPLINE_CURVE_WITH_KNOTS('',3,(#18964,#18965,#18966,#18967,#18968,
#18969,#18970,#18971,#18972,#18973,#18974,#18975,#18976,#18977,#18978,#18979,
#18980,#18981,#18982,#18983,#18984,#18985,#18986,#18987,#18988),
 .UNSPECIFIED.,.F.,.F.,(4,3,3,3,3,3,3,3,4),(-28.9817156343595,-28.7864875774864,
-27.7938500748145,-26.8012125721425,-25.8085750694706,-24.8159375667986,
-23.8233000641267,-22.8306625614547,-22.6985303271799),.UNSPECIFIED.);
#2359=B_SPLINE_CURVE_WITH_KNOTS('',3,(#18993,#18994,#18995,#18996,#18997,
#18998,#18999,#19000,#19001,#19002,#19003,#19004,#19005,#19006,#19007,#19008,
#19009,#19010,#19011,#19012,#19013,#19014),.UNSPECIFIED.,.F.,.F.,(4,3,3,
3,3,3,3,4),(20.1591190625158,20.8453875561108,21.8380250587828,22.8306625614547,
23.8233000641267,24.8159375667986,25.8085750694706,26.4423043696954),
 .UNSPECIFIED.);
#2360=B_SPLINE_CURVE_WITH_KNOTS('',3,(#19015,#19016,#19017,#19018,#19019,
#19020,#19021,#19022,#19023,#19024,#19025,#19026,#19027,#19028,#19029,#19030,
#19031,#19032,#19033,#19034,#19035,#19036),.UNSPECIFIED.,.F.,.F.,(4,3,3,
3,3,3,3,4),(-22.6985303271799,-21.8380250587828,-20.8453875561108,-19.8527500534389,
-18.8601125507669,-17.867475048095,-16.8748375454231,-16.4153450200003),
 .UNSPECIFIED.);
#2361=B_SPLINE_CURVE_WITH_KNOTS('',3,(#19041,#19042,#19043,#19044,#19045,
#19046,#19047,#19048,#19049,#19050,#19051,#19052,#19053,#19054,#19055,#19056,
#19057,#19058,#19059,#19060,#19061,#19062,#19063,#19064,#19065),
 .UNSPECIFIED.,.F.,.F.,(4,3,3,3,3,3,3,3,4),(13.8759337553362,13.8969250374072,
14.8895625400792,15.8822000427511,16.8748375454231,17.867475048095,18.860112550767,
19.8527500534389,20.1591190625158),.UNSPECIFIED.);
#2362=B_SPLINE_CURVE_WITH_KNOTS('',3,(#19066,#19067,#19068,#19069,#19070,
#19071,#19072,#19073,#19074,#19075,#19076,#19077,#19078,#19079,#19080,#19081,
#19082,#19083,#19084,#19085,#19086,#19087),.UNSPECIFIED.,.F.,.F.,(4,3,3,
3,3,3,3,4),(-16.4153450200003,-15.8822000427511,-14.8895625400792,-13.8969250374072,
-12.9042875347353,-11.9116500320633,-10.9190125293914,-10.1321597128207),
 .UNSPECIFIED.);
#2363=B_SPLINE_CURVE_WITH_KNOTS('',3,(#19093,#19094,#19095,#19096,#19097,
#19098,#19099,#19100,#19101,#19102,#19103,#19104,#19105),.UNSPECIFIED.,
 .F.,.F.,(4,3,3,3,4),(-3.84897440564114,-2.97791250801584,-1.98527500534389,
-0.992637502671947,0.),.UNSPECIFIED.);
#2364=B_SPLINE_CURVE_WITH_KNOTS('',3,(#19108,#19109,#19110,#19111,#19112,
#19113,#19114,#19115,#19116,#19117,#19118,#19119,#19120,#19121,#19122,#19123,
#19124,#19125,#19126),.UNSPECIFIED.,.F.,.F.,(4,3,3,3,3,3,4),(2.01694489302841,
2.97791250801583,3.97055001068778,4.96318751335972,5.95582501603167,6.94846251870361,
7.59274844815666),.UNSPECIFIED.);
#2365=B_SPLINE_CURVE_WITH_KNOTS('',3,(#19132,#19133,#19134,#19135,#19136,
#19137,#19138,#19139),.UNSPECIFIED.,.F.,.F.,(4,1,1,1,1,4),(65.9734457253856,
66.4540515092647,67.4466890119367,68.4393265146086,69.4319640172806,70.4246015199525),
 .UNSPECIFIED.);
#2366=B_SPLINE_CURVE_WITH_KNOTS('',3,(#19142,#19143,#19144,#19145,#19146,
#19147,#19148,#19149,#19150),.UNSPECIFIED.,.F.,.F.,(4,1,1,1,1,1,4),(65.9734457253856,
66.015550265913,67.0081877685849,68.0008252712568,68.9934627739288,69.9861002766007,
70.9470678915881),.UNSPECIFIED.);
#2367=B_SPLINE_CURVE_WITH_KNOTS('',3,(#19155,#19156,#19157,#19158,#19159,
#19160,#19161,#19162,#19163,#19164),.UNSPECIFIED.,.F.,.F.,(4,1,1,1,1,1,
1,4),(59.6902604182061,60.4982264932331,61.490863995905,62.483501498577,
63.4761390012489,64.4687765039209,65.4614140065928,65.9734457253856),
 .UNSPECIFIED.);
#2368=B_SPLINE_CURVE_WITH_KNOTS('',3,(#19165,#19166,#19167,#19168,#19169,
#19170,#19171,#19172,#19173,#19174),.UNSPECIFIED.,.F.,.F.,(4,1,1,1,1,1,
1,4),(59.6902604182061,60.0597252498813,61.0523627525532,62.0450002552252,
63.0376377578971,64.0302752605691,65.022912763241,65.9734457253856),
 .UNSPECIFIED.);
#2369=B_SPLINE_CURVE_WITH_KNOTS('',3,(#19179,#19180,#19181,#19182,#19183,
#19184,#19185,#19186,#19187,#19188,#19189),.UNSPECIFIED.,.F.,.F.,(4,1,1,
1,1,1,1,1,4),(53.4070751110265,53.5497639745295,54.5424014772014,55.5350389798734,
56.5276764825453,57.5203139852172,58.5129514878892,59.5055889905611,59.6902604182061),
 .UNSPECIFIED.);
#2370=B_SPLINE_CURVE_WITH_KNOTS('',3,(#19190,#19191,#19192,#19193,#19194,
#19195,#19196,#19197,#19198,#19199),.UNSPECIFIED.,.F.,.F.,(4,1,1,1,1,1,
1,4),(53.4070751110265,54.1039002338496,55.0965377365216,56.0891752391935,
57.0818127418655,58.0744502445374,59.0670877472093,59.6902604182061),
 .UNSPECIFIED.);
#2371=B_SPLINE_CURVE_WITH_KNOTS('',3,(#19204,#19205,#19206,#19207,#19208,
#19209,#19210,#19211,#19212,#19213),.UNSPECIFIED.,.F.,.F.,(4,1,1,1,1,1,
1,4),(47.1238898038469,47.5939389584978,48.5865764611697,49.5792139638417,
50.5718514665136,51.5644889691856,52.5571264718575,53.4070751110265),
 .UNSPECIFIED.);
#2372=B_SPLINE_CURVE_WITH_KNOTS('',3,(#19214,#19215,#19216,#19217,#19218,
#19219,#19220,#19221,#19222,#19223,#19224),.UNSPECIFIED.,.F.,.F.,(4,1,1,
1,1,1,1,1,4),(47.1238898038469,47.155437715146,48.1480752178179,49.1407127204899,
50.1333502231618,51.1259877258338,52.1186252285057,53.1112627311777,53.4070751110265),
 .UNSPECIFIED.);
#2373=B_SPLINE_CURVE_WITH_KNOTS('',3,(#19229,#19230,#19231,#19232,#19233,
#19234,#19235,#19236,#19237,#19238),.UNSPECIFIED.,.F.,.F.,(4,1,1,1,1,1,
1,4),(40.8407044966673,41.6381139424661,42.6307514451381,43.62338894781,
44.616026450482,45.6086639531539,46.6013014558259,47.1238898038469),
 .UNSPECIFIED.);
#2374=B_SPLINE_CURVE_WITH_KNOTS('',3,(#19239,#19240,#19241,#19242,#19243,
#19244,#19245,#19246,#19247,#19248),.UNSPECIFIED.,.F.,.F.,(4,1,1,1,1,1,
1,4),(40.8407044966673,41.1996126991143,42.1922502017863,43.1848877044582,
44.1775252071302,45.1701627098021,46.1628002124741,47.1238898038469),
 .UNSPECIFIED.);
#2375=B_SPLINE_CURVE_WITH_KNOTS('',3,(#19253,#19254,#19255,#19256,#19257,
#19258,#19259,#19260,#19261,#19262,#19263),.UNSPECIFIED.,.F.,.F.,(4,1,1,
1,1,1,1,1,4),(34.5575191894877,34.6896514237625,35.6822889264345,36.6749264291064,
37.6675639317784,38.6602014344503,39.6528389371222,40.6454764397942,40.8407044966673),
 .UNSPECIFIED.);
#2376=B_SPLINE_CURVE_WITH_KNOTS('',3,(#19264,#19265,#19266,#19267,#19268,
#19269,#19270,#19271,#19272,#19273),.UNSPECIFIED.,.F.,.F.,(4,1,1,1,1,1,
1,4),(34.5575191894877,35.2437876830827,36.2364251857546,37.2290626884266,
38.2217001910985,39.2143376937704,40.2069751964424,40.8407044966673),
 .UNSPECIFIED.);
#2377=B_SPLINE_CURVE_WITH_KNOTS('',3,(#19278,#19279,#19280,#19281,#19282,
#19283,#19284,#19285,#19286,#19287),.UNSPECIFIED.,.F.,.F.,(4,1,1,1,1,1,
1,4),(28.2743338823081,28.7338264077309,29.7264639104028,30.7191014130747,
31.7117389157467,32.7043764184186,33.6970139210906,34.5575191894877),
 .UNSPECIFIED.);
#2378=B_SPLINE_CURVE_WITH_KNOTS('',3,(#19288,#19289,#19290,#19291,#19292,
#19293,#19294,#19295,#19296,#19297,#19298),.UNSPECIFIED.,.F.,.F.,(4,1,1,
1,1,1,1,1,4),(28.2743338823081,28.2953251643791,29.287962667051,30.2806001697229,
31.2732376723949,32.2658751750668,33.2585126777388,34.2511501804107,34.5575191894877),
 .UNSPECIFIED.);
#2379=B_SPLINE_CURVE_WITH_KNOTS('',3,(#19303,#19304,#19305,#19306,#19307,
#19308,#19309,#19310,#19311,#19312),.UNSPECIFIED.,.F.,.F.,(4,1,1,1,1,1,
1,4),(21.9911485751285,22.7780013916992,23.7706388943711,24.7632763970431,
25.755913899715,26.748551402387,27.7411889050589,28.2743338823081),
 .UNSPECIFIED.);
#2380=B_SPLINE_CURVE_WITH_KNOTS('',3,(#19313,#19314,#19315,#19316,#19317,
#19318,#19319,#19320,#19321,#19322),.UNSPECIFIED.,.F.,.F.,(4,1,1,1,1,1,
1,4),(21.9911485751285,22.3395001483474,23.3321376510193,24.3247751536913,
25.3174126563632,26.3100501590352,27.3026876617071,28.2743338823081),
 .UNSPECIFIED.);
#2381=B_SPLINE_CURVE_WITH_KNOTS('',3,(#19328,#19329,#19330,#19331,#19332),
 .UNSPECIFIED.,.F.,.F.,(4,1,4),(14.3984001269718,15.3910376296438,15.7079632679489),
 .UNSPECIFIED.);
#2382=B_SPLINE_CURVE_WITH_KNOTS('',3,(#19335,#19336,#19337,#19338,#19339),
 .UNSPECIFIED.,.F.,.F.,(4,1,4),(13.8759337553362,14.8369013703236,15.7079632679489),
 .UNSPECIFIED.);
#2383=B_SPLINE_CURVE_WITH_KNOTS('',3,(#19345,#19346,#19347,#19348),
 .UNSPECIFIED.,.F.,.F.,(4,4),(57.8582309055934,58.5656126576447),
 .UNSPECIFIED.);
#2384=B_SPLINE_CURVE_WITH_KNOTS('',3,(#19356,#19357,#19358,#19359,#19360,
#19361,#19362,#19363,#19364,#19365),.UNSPECIFIED.,.F.,.F.,(4,3,3,4),(-56.5486677646163,
-55.5877001496289,-54.595062646957,-54.1144568630778),.UNSPECIFIED.);
#2385=B_SPLINE_CURVE_WITH_KNOTS('',3,(#19370,#19371,#19372,#19373,#19374,
#19375,#19376,#19377,#19378,#19379,#19380,#19381,#19382,#19383,#19384,#19385,
#19386,#19387,#19388,#19389,#19390,#19391,#19392,#19393,#19394),
 .UNSPECIFIED.,.F.,.F.,(4,3,3,3,3,3,3,3,4),(51.5750455984138,51.6171501389411,
52.6097876416131,53.602425144285,54.5950626469569,55.5877001496289,56.5803376523008,
57.5729751549728,57.8582309055934),.UNSPECIFIED.);
#2386=B_SPLINE_CURVE_WITH_KNOTS('',3,(#19395,#19396,#19397,#19398,#19399,
#19400,#19401,#19402,#19403,#19404,#19405,#19406,#19407,#19408,#19409,#19410,
#19411,#19412,#19413,#19414,#19415,#19416),.UNSPECIFIED.,.F.,.F.,(4,3,3,
3,3,3,3,4),(-54.1144568630778,-53.602425144285,-52.6097876416131,-51.6171501389411,
-50.6245126362692,-49.6318751335972,-48.6392376309253,-47.8312715558982),
 .UNSPECIFIED.);
#2387=B_SPLINE_CURVE_WITH_KNOTS('',3,(#19421,#19422,#19423,#19424,#19425,
#19426,#19427,#19428,#19429,#19430,#19431,#19432,#19433,#19434,#19435,#19436,
#19437,#19438,#19439,#19440,#19441,#19442),.UNSPECIFIED.,.F.,.F.,(4,3,3,
3,3,3,3,4),(45.2918602912342,45.6613251229094,46.6539626255814,47.6466001282533,
48.6392376309253,49.6318751335972,50.6245126362692,51.5750455984138),
 .UNSPECIFIED.);
#2388=B_SPLINE_CURVE_WITH_KNOTS('',3,(#19443,#19444,#19445,#19446,#19447,
#19448,#19449,#19450,#19451,#19452,#19453,#19454,#19455,#19456,#19457,#19458,
#19459,#19460,#19461,#19462,#19463,#19464,#19465,#19466,#19467),
 .UNSPECIFIED.,.F.,.F.,(4,3,3,3,3,3,3,3,4),(-47.8312715558982,-47.6466001282533,
-46.6539626255814,-45.6613251229095,-44.6686876202375,-43.6760501175656,
-42.6834126148936,-41.6907751122217,-41.5480862487187),.UNSPECIFIED.);
#2389=B_SPLINE_CURVE_WITH_KNOTS('',3,(#19472,#19473,#19474,#19475,#19476,
#19477,#19478,#19479,#19480,#19481,#19482,#19483,#19484,#19485,#19486,#19487,
#19488,#19489,#19490,#19491,#19492,#19493),.UNSPECIFIED.,.F.,.F.,(4,3,3,
3,3,3,3,4),(39.0086749840546,39.7055001068778,40.6981376095497,41.6907751122217,
42.6834126148936,43.6760501175656,44.6686876202375,45.2918602912342),
 .UNSPECIFIED.);
#2390=B_SPLINE_CURVE_WITH_KNOTS('',3,(#19494,#19495,#19496,#19497,#19498,
#19499,#19500,#19501,#19502,#19503,#19504,#19505,#19506,#19507,#19508,#19509,
#19510,#19511,#19512,#19513,#19514,#19515),.UNSPECIFIED.,.F.,.F.,(4,3,3,
3,3,3,3,4),(-41.5480862487187,-40.6981376095497,-39.7055001068778,-38.7128626042058,
-37.7202251015339,-36.727587598862,-35.73495009619,-35.2649009415391),
 .UNSPECIFIED.);
#2391=B_SPLINE_CURVE_WITH_KNOTS('',3,(#19520,#19521,#19522,#19523,#19524,
#19525,#19526,#19527,#19528,#19529,#19530,#19531,#19532,#19533,#19534,#19535,
#19536,#19537,#19538,#19539,#19540,#19541,#19542,#19543,#19544),
 .UNSPECIFIED.,.F.,.F.,(4,3,3,3,3,3,3,3,4),(32.725489676875,32.7570375881742,
33.7496750908461,34.7423125935181,35.73495009619,36.727587598862,37.7202251015339,
38.7128626042058,39.0086749840546),.UNSPECIFIED.);
#2392=B_SPLINE_CURVE_WITH_KNOTS('',3,(#19545,#19546,#19547,#19548,#19549,
#19550,#19551,#19552,#19553,#19554,#19555,#19556,#19557,#19558,#19559,#19560,
#19561,#19562,#19563,#19564,#19565,#19566),.UNSPECIFIED.,.F.,.F.,(4,3,3,
3,3,3,3,4),(-35.2649009415391,-34.7423125935181,-33.7496750908461,-32.7570375881742,
-31.7644000855022,-30.7717625828303,-29.7791250801584,-28.9817156343595),
 .UNSPECIFIED.);
#2393=B_SPLINE_CURVE_WITH_KNOTS('',3,(#19571,#19572,#19573,#19574,#19575,
#19576,#19577,#19578,#19579,#19580,#19581,#19582,#19583,#19584,#19585,#19586,
#19587,#19588,#19589,#19590,#19591,#19592),.UNSPECIFIED.,.F.,.F.,(4,3,3,
3,3,3,3,4),(26.4423043696954,26.8012125721425,27.7938500748145,28.7864875774864,
29.7791250801583,30.7717625828303,31.7644000855022,32.725489676875),
 .UNSPECIFIED.);
#2394=B_SPLINE_CURVE_WITH_KNOTS('',3,(#19593,#19594,#19595,#19596,#19597,
#19598,#19599,#19600,#19601,#19602,#19603,#19604,#19605,#19606,#19607,#19608,
#19609,#19610,#19611,#19612,#19613,#19614,#19615,#19616,#19617),
 .UNSPECIFIED.,.F.,.F.,(4,3,3,3,3,3,3,3,4),(-28.9817156343595,-28.7864875774864,
-27.7938500748145,-26.8012125721425,-25.8085750694706,-24.8159375667986,
-23.8233000641267,-22.8306625614547,-22.6985303271799),.UNSPECIFIED.);
#2395=B_SPLINE_CURVE_WITH_KNOTS('',3,(#19622,#19623,#19624,#19625,#19626,
#19627,#19628,#19629,#19630,#19631,#19632,#19633,#19634,#19635,#19636,#19637,
#19638,#19639,#19640,#19641,#19642,#19643),.UNSPECIFIED.,.F.,.F.,(4,3,3,
3,3,3,3,4),(20.1591190625158,20.8453875561108,21.8380250587828,22.8306625614547,
23.8233000641267,24.8159375667986,25.8085750694706,26.4423043696954),
 .UNSPECIFIED.);
#2396=B_SPLINE_CURVE_WITH_KNOTS('',3,(#19644,#19645,#19646,#19647,#19648,
#19649,#19650,#19651,#19652,#19653,#19654,#19655,#19656,#19657,#19658,#19659,
#19660,#19661,#19662,#19663,#19664,#19665),.UNSPECIFIED.,.F.,.F.,(4,3,3,
3,3,3,3,4),(-22.6985303271799,-21.8380250587828,-20.8453875561108,-19.8527500534389,
-18.8601125507669,-17.867475048095,-16.8748375454231,-16.4153450200003),
 .UNSPECIFIED.);
#2397=B_SPLINE_CURVE_WITH_KNOTS('',3,(#19670,#19671,#19672,#19673,#19674,
#19675,#19676,#19677,#19678,#19679,#19680,#19681,#19682,#19683,#19684,#19685,
#19686,#19687,#19688,#19689,#19690,#19691,#19692,#19693,#19694),
 .UNSPECIFIED.,.F.,.F.,(4,3,3,3,3,3,3,3,4),(13.8759337553362,13.8969250374072,
14.8895625400792,15.8822000427511,16.8748375454231,17.867475048095,18.8601125507669,
19.8527500534389,20.1591190625158),.UNSPECIFIED.);
#2398=B_SPLINE_CURVE_WITH_KNOTS('',3,(#19695,#19696,#19697,#19698,#19699,
#19700,#19701,#19702,#19703,#19704,#19705,#19706,#19707,#19708,#19709,#19710,
#19711,#19712,#19713,#19714,#19715,#19716),.UNSPECIFIED.,.F.,.F.,(4,3,3,
3,3,3,3,4),(-16.4153450200003,-15.8822000427511,-14.8895625400792,-13.8969250374072,
-12.9042875347353,-11.9116500320633,-10.9190125293914,-10.1321597128207),
 .UNSPECIFIED.);
#2399=B_SPLINE_CURVE_WITH_KNOTS('',3,(#19722,#19723,#19724,#19725,#19726,
#19727,#19728,#19729,#19730,#19731,#19732,#19733,#19734),.UNSPECIFIED.,
 .F.,.F.,(4,3,3,3,4),(-3.84897440564114,-2.97791250801584,-1.98527500534389,
-0.992637502671947,0.),.UNSPECIFIED.);
#2400=B_SPLINE_CURVE_WITH_KNOTS('',3,(#19737,#19738,#19739,#19740,#19741,
#19742,#19743,#19744,#19745,#19746,#19747,#19748,#19749,#19750,#19751,#19752,
#19753,#19754,#19755),.UNSPECIFIED.,.F.,.F.,(4,3,3,3,3,3,4),(2.01694489302844,
2.97791250801583,3.97055001068778,4.96318751335972,5.95582501603167,6.94846251870362,
7.59274844815666),.UNSPECIFIED.);
#2401=B_SPLINE_CURVE_WITH_KNOTS('',3,(#19761,#19762,#19763,#19764,#19765,
#19766,#19767,#19768),.UNSPECIFIED.,.F.,.F.,(4,1,1,1,1,4),(65.9734457253856,
66.4540515092647,67.4466890119367,68.4393265146086,69.4319640172806,70.4246015199525),
 .UNSPECIFIED.);
#2402=B_SPLINE_CURVE_WITH_KNOTS('',3,(#19771,#19772,#19773,#19774,#19775,
#19776,#19777,#19778,#19779),.UNSPECIFIED.,.F.,.F.,(4,1,1,1,1,1,4),(65.9734457253856,
66.0155502659129,67.0081877685849,68.0008252712568,68.9934627739288,69.9861002766007,
70.9470678915881),.UNSPECIFIED.);
#2403=B_SPLINE_CURVE_WITH_KNOTS('',3,(#19784,#19785,#19786,#19787,#19788,
#19789,#19790,#19791,#19792,#19793),.UNSPECIFIED.,.F.,.F.,(4,1,1,1,1,1,
1,4),(59.6902604182061,60.4982264932331,61.490863995905,62.483501498577,
63.4761390012489,64.4687765039209,65.4614140065928,65.9734457253856),
 .UNSPECIFIED.);
#2404=B_SPLINE_CURVE_WITH_KNOTS('',3,(#19794,#19795,#19796,#19797,#19798,
#19799,#19800,#19801,#19802,#19803),.UNSPECIFIED.,.F.,.F.,(4,1,1,1,1,1,
1,4),(59.6902604182061,60.0597252498813,61.0523627525532,62.0450002552252,
63.0376377578971,64.0302752605691,65.022912763241,65.9734457253856),
 .UNSPECIFIED.);
#2405=B_SPLINE_CURVE_WITH_KNOTS('',3,(#19808,#19809,#19810,#19811,#19812,
#19813,#19814,#19815,#19816,#19817,#19818),.UNSPECIFIED.,.F.,.F.,(4,1,1,
1,1,1,1,1,4),(53.4070751110265,53.5497639745295,54.5424014772014,55.5350389798734,
56.5276764825453,57.5203139852172,58.5129514878892,59.5055889905611,59.6902604182061),
 .UNSPECIFIED.);
#2406=B_SPLINE_CURVE_WITH_KNOTS('',3,(#19819,#19820,#19821,#19822,#19823,
#19824,#19825,#19826,#19827,#19828),.UNSPECIFIED.,.F.,.F.,(4,1,1,1,1,1,
1,4),(53.4070751110265,54.1039002338496,55.0965377365216,56.0891752391935,
57.0818127418654,58.0744502445374,59.0670877472093,59.6902604182061),
 .UNSPECIFIED.);
#2407=B_SPLINE_CURVE_WITH_KNOTS('',3,(#19833,#19834,#19835,#19836,#19837,
#19838,#19839,#19840,#19841,#19842),.UNSPECIFIED.,.F.,.F.,(4,1,1,1,1,1,
1,4),(47.1238898038469,47.5939389584978,48.5865764611697,49.5792139638417,
50.5718514665136,51.5644889691856,52.5571264718575,53.4070751110265),
 .UNSPECIFIED.);
#2408=B_SPLINE_CURVE_WITH_KNOTS('',3,(#19843,#19844,#19845,#19846,#19847,
#19848,#19849,#19850,#19851,#19852,#19853),.UNSPECIFIED.,.F.,.F.,(4,1,1,
1,1,1,1,1,4),(47.1238898038469,47.155437715146,48.1480752178179,49.1407127204899,
50.1333502231618,51.1259877258338,52.1186252285057,53.1112627311777,53.4070751110265),
 .UNSPECIFIED.);
#2409=B_SPLINE_CURVE_WITH_KNOTS('',3,(#19858,#19859,#19860,#19861,#19862,
#19863,#19864,#19865,#19866,#19867),.UNSPECIFIED.,.F.,.F.,(4,1,1,1,1,1,
1,4),(40.8407044966673,41.6381139424661,42.6307514451381,43.62338894781,
44.616026450482,45.6086639531539,46.6013014558259,47.1238898038469),
 .UNSPECIFIED.);
#2410=B_SPLINE_CURVE_WITH_KNOTS('',3,(#19868,#19869,#19870,#19871,#19872,
#19873,#19874,#19875,#19876,#19877),.UNSPECIFIED.,.F.,.F.,(4,1,1,1,1,1,
1,4),(40.8407044966673,41.1996126991143,42.1922502017863,43.1848877044582,
44.1775252071302,45.1701627098021,46.1628002124741,47.1238898038469),
 .UNSPECIFIED.);
#2411=B_SPLINE_CURVE_WITH_KNOTS('',3,(#19882,#19883,#19884,#19885,#19886,
#19887,#19888,#19889,#19890,#19891,#19892),.UNSPECIFIED.,.F.,.F.,(4,1,1,
1,1,1,1,1,4),(34.5575191894877,34.6896514237625,35.6822889264345,36.6749264291064,
37.6675639317784,38.6602014344503,39.6528389371222,40.6454764397942,40.8407044966673),
 .UNSPECIFIED.);
#2412=B_SPLINE_CURVE_WITH_KNOTS('',3,(#19893,#19894,#19895,#19896,#19897,
#19898,#19899,#19900,#19901,#19902),.UNSPECIFIED.,.F.,.F.,(4,1,1,1,1,1,
1,4),(34.5575191894877,35.2437876830827,36.2364251857546,37.2290626884266,
38.2217001910985,39.2143376937704,40.2069751964424,40.8407044966673),
 .UNSPECIFIED.);
#2413=B_SPLINE_CURVE_WITH_KNOTS('',3,(#19907,#19908,#19909,#19910,#19911,
#19912,#19913,#19914,#19915,#19916),.UNSPECIFIED.,.F.,.F.,(4,1,1,1,1,1,
1,4),(28.2743338823081,28.7338264077309,29.7264639104028,30.7191014130747,
31.7117389157467,32.7043764184186,33.6970139210906,34.5575191894877),
 .UNSPECIFIED.);
#2414=B_SPLINE_CURVE_WITH_KNOTS('',3,(#19917,#19918,#19919,#19920,#19921,
#19922,#19923,#19924,#19925,#19926,#19927),.UNSPECIFIED.,.F.,.F.,(4,1,1,
1,1,1,1,1,4),(28.2743338823081,28.2953251643791,29.287962667051,30.2806001697229,
31.2732376723949,32.2658751750668,33.2585126777388,34.2511501804107,34.5575191894877),
 .UNSPECIFIED.);
#2415=B_SPLINE_CURVE_WITH_KNOTS('',3,(#19932,#19933,#19934,#19935,#19936,
#19937,#19938,#19939,#19940,#19941),.UNSPECIFIED.,.F.,.F.,(4,1,1,1,1,1,
1,4),(21.9911485751285,22.7780013916992,23.7706388943711,24.7632763970431,
25.755913899715,26.748551402387,27.7411889050589,28.2743338823081),
 .UNSPECIFIED.);
#2416=B_SPLINE_CURVE_WITH_KNOTS('',3,(#19942,#19943,#19944,#19945,#19946,
#19947,#19948,#19949,#19950,#19951),.UNSPECIFIED.,.F.,.F.,(4,1,1,1,1,1,
1,4),(21.9911485751285,22.3395001483474,23.3321376510193,24.3247751536913,
25.3174126563632,26.3100501590352,27.3026876617071,28.2743338823081),
 .UNSPECIFIED.);
#2417=B_SPLINE_CURVE_WITH_KNOTS('',3,(#19957,#19958,#19959,#19960,#19961),
 .UNSPECIFIED.,.F.,.F.,(4,1,4),(14.3984001269718,15.3910376296438,15.7079632679489),
 .UNSPECIFIED.);
#2418=B_SPLINE_CURVE_WITH_KNOTS('',3,(#19964,#19965,#19966,#19967,#19968),
 .UNSPECIFIED.,.F.,.F.,(4,1,4),(13.8759337553362,14.8369013703236,15.7079632679489),
 .UNSPECIFIED.);
#2419=B_SPLINE_CURVE_WITH_KNOTS('',3,(#19974,#19975,#19976,#19977),
 .UNSPECIFIED.,.F.,.F.,(4,4),(57.8582309055934,58.5656126576448),
 .UNSPECIFIED.);
#2420=B_SPLINE_CURVE_WITH_KNOTS('',3,(#19985,#19986,#19987,#19988,#19989,
#19990,#19991,#19992,#19993,#19994),.UNSPECIFIED.,.F.,.F.,(4,3,3,4),(-56.5486677646163,
-55.5877001496289,-54.595062646957,-54.1144568630778),.UNSPECIFIED.);
#2421=B_SPLINE_CURVE_WITH_KNOTS('',3,(#19999,#20000,#20001,#20002,#20003,
#20004,#20005,#20006,#20007,#20008,#20009,#20010,#20011,#20012,#20013,#20014,
#20015,#20016,#20017,#20018,#20019,#20020,#20021,#20022,#20023),
 .UNSPECIFIED.,.F.,.F.,(4,3,3,3,3,3,3,3,4),(51.5750455984138,51.6171501389411,
52.6097876416131,53.602425144285,54.595062646957,55.5877001496289,56.5803376523009,
57.5729751549728,57.8582309055934),.UNSPECIFIED.);
#2422=B_SPLINE_CURVE_WITH_KNOTS('',3,(#20024,#20025,#20026,#20027,#20028,
#20029,#20030,#20031,#20032,#20033,#20034,#20035,#20036,#20037,#20038,#20039,
#20040,#20041,#20042,#20043,#20044,#20045),.UNSPECIFIED.,.F.,.F.,(4,3,3,
3,3,3,3,4),(-54.1144568630778,-53.602425144285,-52.6097876416131,-51.6171501389411,
-50.6245126362692,-49.6318751335972,-48.6392376309253,-47.8312715558982),
 .UNSPECIFIED.);
#2423=B_SPLINE_CURVE_WITH_KNOTS('',3,(#20050,#20051,#20052,#20053,#20054,
#20055,#20056,#20057,#20058,#20059,#20060,#20061,#20062,#20063,#20064,#20065,
#20066,#20067,#20068,#20069,#20070,#20071),.UNSPECIFIED.,.F.,.F.,(4,3,3,
3,3,3,3,4),(45.2918602912342,45.6613251229095,46.6539626255814,47.6466001282534,
48.6392376309253,49.6318751335973,50.6245126362692,51.5750455984138),
 .UNSPECIFIED.);
#2424=B_SPLINE_CURVE_WITH_KNOTS('',3,(#20072,#20073,#20074,#20075,#20076,
#20077,#20078,#20079,#20080,#20081,#20082,#20083,#20084,#20085,#20086,#20087,
#20088,#20089,#20090,#20091,#20092,#20093,#20094,#20095,#20096),
 .UNSPECIFIED.,.F.,.F.,(4,3,3,3,3,3,3,3,4),(-47.8312715558982,-47.6466001282533,
-46.6539626255814,-45.6613251229095,-44.6686876202375,-43.6760501175656,
-42.6834126148936,-41.6907751122217,-41.5480862487187),.UNSPECIFIED.);
#2425=B_SPLINE_CURVE_WITH_KNOTS('',3,(#20101,#20102,#20103,#20104,#20105,
#20106,#20107,#20108,#20109,#20110,#20111,#20112,#20113,#20114,#20115,#20116,
#20117,#20118,#20119,#20120,#20121,#20122),.UNSPECIFIED.,.F.,.F.,(4,3,3,
3,3,3,3,4),(39.0086749840546,39.7055001068778,40.6981376095497,41.6907751122217,
42.6834126148936,43.6760501175656,44.6686876202375,45.2918602912342),
 .UNSPECIFIED.);
#2426=B_SPLINE_CURVE_WITH_KNOTS('',3,(#20123,#20124,#20125,#20126,#20127,
#20128,#20129,#20130,#20131,#20132,#20133,#20134,#20135,#20136,#20137,#20138,
#20139,#20140,#20141,#20142,#20143,#20144),.UNSPECIFIED.,.F.,.F.,(4,3,3,
3,3,3,3,4),(-41.5480862487187,-40.6981376095497,-39.7055001068778,-38.7128626042058,
-37.7202251015339,-36.727587598862,-35.73495009619,-35.2649009415391),
 .UNSPECIFIED.);
#2427=B_SPLINE_CURVE_WITH_KNOTS('',3,(#20149,#20150,#20151,#20152,#20153,
#20154,#20155,#20156,#20157,#20158,#20159,#20160,#20161,#20162,#20163,#20164,
#20165,#20166,#20167,#20168,#20169,#20170,#20171,#20172,#20173),
 .UNSPECIFIED.,.F.,.F.,(4,3,3,3,3,3,3,3,4),(32.725489676875,32.7570375881742,
33.7496750908461,34.7423125935181,35.73495009619,36.727587598862,37.7202251015339,
38.7128626042059,39.0086749840546),.UNSPECIFIED.);
#2428=B_SPLINE_CURVE_WITH_KNOTS('',3,(#20174,#20175,#20176,#20177,#20178,
#20179,#20180,#20181,#20182,#20183,#20184,#20185,#20186,#20187,#20188,#20189,
#20190,#20191,#20192,#20193,#20194,#20195),.UNSPECIFIED.,.F.,.F.,(4,3,3,
3,3,3,3,4),(-35.2649009415391,-34.7423125935181,-33.7496750908461,-32.7570375881742,
-31.7644000855022,-30.7717625828303,-29.7791250801584,-28.9817156343595),
 .UNSPECIFIED.);
#2429=B_SPLINE_CURVE_WITH_KNOTS('',3,(#20200,#20201,#20202,#20203,#20204,
#20205,#20206,#20207,#20208,#20209,#20210,#20211,#20212,#20213,#20214,#20215,
#20216,#20217,#20218,#20219,#20220,#20221),.UNSPECIFIED.,.F.,.F.,(4,3,3,
3,3,3,3,4),(26.4423043696954,26.8012125721425,27.7938500748145,28.7864875774864,
29.7791250801583,30.7717625828303,31.7644000855022,32.725489676875),
 .UNSPECIFIED.);
#2430=B_SPLINE_CURVE_WITH_KNOTS('',3,(#20222,#20223,#20224,#20225,#20226,
#20227,#20228,#20229,#20230,#20231,#20232,#20233,#20234,#20235,#20236,#20237,
#20238,#20239,#20240,#20241,#20242,#20243,#20244,#20245,#20246),
 .UNSPECIFIED.,.F.,.F.,(4,3,3,3,3,3,3,3,4),(-28.9817156343595,-28.7864875774864,
-27.7938500748145,-26.8012125721425,-25.8085750694706,-24.8159375667986,
-23.8233000641267,-22.8306625614547,-22.6985303271799),.UNSPECIFIED.);
#2431=B_SPLINE_CURVE_WITH_KNOTS('',3,(#20251,#20252,#20253,#20254,#20255,
#20256,#20257,#20258,#20259,#20260,#20261,#20262,#20263,#20264,#20265,#20266,
#20267,#20268,#20269,#20270,#20271,#20272),.UNSPECIFIED.,.F.,.F.,(4,3,3,
3,3,3,3,4),(20.1591190625158,20.8453875561108,21.8380250587828,22.8306625614547,
23.8233000641267,24.8159375667986,25.8085750694706,26.4423043696954),
 .UNSPECIFIED.);
#2432=B_SPLINE_CURVE_WITH_KNOTS('',3,(#20273,#20274,#20275,#20276,#20277,
#20278,#20279,#20280,#20281,#20282,#20283,#20284,#20285,#20286,#20287,#20288,
#20289,#20290,#20291,#20292,#20293,#20294),.UNSPECIFIED.,.F.,.F.,(4,3,3,
3,3,3,3,4),(-22.6985303271799,-21.8380250587828,-20.8453875561108,-19.8527500534389,
-18.860112550767,-17.867475048095,-16.8748375454231,-16.4153450200003),
 .UNSPECIFIED.);
#2433=B_SPLINE_CURVE_WITH_KNOTS('',3,(#20299,#20300,#20301,#20302,#20303,
#20304,#20305,#20306,#20307,#20308,#20309,#20310,#20311,#20312,#20313,#20314,
#20315,#20316,#20317,#20318,#20319,#20320,#20321,#20322,#20323),
 .UNSPECIFIED.,.F.,.F.,(4,3,3,3,3,3,3,3,4),(13.8759337553362,13.8969250374072,
14.8895625400792,15.8822000427511,16.8748375454231,17.867475048095,18.860112550767,
19.8527500534389,20.1591190625158),.UNSPECIFIED.);
#2434=B_SPLINE_CURVE_WITH_KNOTS('',3,(#20324,#20325,#20326,#20327,#20328,
#20329,#20330,#20331,#20332,#20333,#20334,#20335,#20336,#20337,#20338,#20339,
#20340,#20341,#20342,#20343,#20344,#20345),.UNSPECIFIED.,.F.,.F.,(4,3,3,
3,3,3,3,4),(-16.4153450200003,-15.8822000427511,-14.8895625400792,-13.8969250374072,
-12.9042875347353,-11.9116500320633,-10.9190125293914,-10.1321597128207),
 .UNSPECIFIED.);
#2435=B_SPLINE_CURVE_WITH_KNOTS('',3,(#20351,#20352,#20353,#20354,#20355,
#20356,#20357,#20358,#20359,#20360,#20361,#20362,#20363),.UNSPECIFIED.,
 .F.,.F.,(4,3,3,3,4),(-3.84897440564114,-2.97791250801583,-1.98527500534389,
-0.992637502671945,0.),.UNSPECIFIED.);
#2436=B_SPLINE_CURVE_WITH_KNOTS('',3,(#20366,#20367,#20368,#20369,#20370,
#20371,#20372,#20373,#20374,#20375,#20376,#20377,#20378,#20379,#20380,#20381,
#20382,#20383,#20384),.UNSPECIFIED.,.F.,.F.,(4,3,3,3,3,3,4),(2.01694489302845,
2.97791250801584,3.97055001068779,4.96318751335973,5.95582501603167,6.94846251870361,
7.59274844815666),.UNSPECIFIED.);
#2437=B_SPLINE_CURVE_WITH_KNOTS('',3,(#20390,#20391,#20392,#20393,#20394,
#20395,#20396,#20397),.UNSPECIFIED.,.F.,.F.,(4,1,1,1,1,4),(65.9734457253856,
66.4540515092647,67.4466890119367,68.4393265146086,69.4319640172806,70.4246015199525),
 .UNSPECIFIED.);
#2438=B_SPLINE_CURVE_WITH_KNOTS('',3,(#20400,#20401,#20402,#20403,#20404,
#20405,#20406,#20407,#20408),.UNSPECIFIED.,.F.,.F.,(4,1,1,1,1,1,4),(65.9734457253856,
66.015550265913,67.0081877685849,68.0008252712569,68.9934627739288,69.9861002766008,
70.9470678915881),.UNSPECIFIED.);
#2439=B_SPLINE_CURVE_WITH_KNOTS('',3,(#20413,#20414,#20415,#20416,#20417,
#20418,#20419,#20420,#20421,#20422),.UNSPECIFIED.,.F.,.F.,(4,1,1,1,1,1,
1,4),(59.6902604182061,60.4982264932331,61.490863995905,62.483501498577,
63.4761390012489,64.4687765039209,65.4614140065928,65.9734457253856),
 .UNSPECIFIED.);
#2440=B_SPLINE_CURVE_WITH_KNOTS('',3,(#20423,#20424,#20425,#20426,#20427,
#20428,#20429,#20430,#20431,#20432),.UNSPECIFIED.,.F.,.F.,(4,1,1,1,1,1,
1,4),(59.6902604182061,60.0597252498813,61.0523627525533,62.0450002552252,
63.0376377578971,64.0302752605691,65.022912763241,65.9734457253856),
 .UNSPECIFIED.);
#2441=B_SPLINE_CURVE_WITH_KNOTS('',3,(#20437,#20438,#20439,#20440,#20441,
#20442,#20443,#20444,#20445,#20446,#20447),.UNSPECIFIED.,.F.,.F.,(4,1,1,
1,1,1,1,1,4),(53.4070751110265,53.5497639745295,54.5424014772014,55.5350389798734,
56.5276764825453,57.5203139852172,58.5129514878892,59.5055889905611,59.6902604182061),
 .UNSPECIFIED.);
#2442=B_SPLINE_CURVE_WITH_KNOTS('',3,(#20448,#20449,#20450,#20451,#20452,
#20453,#20454,#20455,#20456,#20457),.UNSPECIFIED.,.F.,.F.,(4,1,1,1,1,1,
1,4),(53.4070751110265,54.1039002338496,55.0965377365216,56.0891752391935,
57.0818127418655,58.0744502445374,59.0670877472094,59.6902604182061),
 .UNSPECIFIED.);
#2443=B_SPLINE_CURVE_WITH_KNOTS('',3,(#20462,#20463,#20464,#20465,#20466,
#20467,#20468,#20469,#20470,#20471),.UNSPECIFIED.,.F.,.F.,(4,1,1,1,1,1,
1,4),(47.1238898038469,47.5939389584978,48.5865764611697,49.5792139638417,
50.5718514665136,51.5644889691856,52.5571264718575,53.4070751110265),
 .UNSPECIFIED.);
#2444=B_SPLINE_CURVE_WITH_KNOTS('',3,(#20472,#20473,#20474,#20475,#20476,
#20477,#20478,#20479,#20480,#20481,#20482),.UNSPECIFIED.,.F.,.F.,(4,1,1,
1,1,1,1,1,4),(47.1238898038469,47.155437715146,48.148075217818,49.1407127204899,
50.1333502231619,51.1259877258338,52.1186252285057,53.1112627311777,53.4070751110265),
 .UNSPECIFIED.);
#2445=B_SPLINE_CURVE_WITH_KNOTS('',3,(#20487,#20488,#20489,#20490,#20491,
#20492,#20493,#20494,#20495,#20496),.UNSPECIFIED.,.F.,.F.,(4,1,1,1,1,1,
1,4),(40.8407044966673,41.6381139424661,42.6307514451381,43.62338894781,
44.616026450482,45.6086639531539,46.6013014558259,47.1238898038469),
 .UNSPECIFIED.);
#2446=B_SPLINE_CURVE_WITH_KNOTS('',3,(#20497,#20498,#20499,#20500,#20501,
#20502,#20503,#20504,#20505,#20506),.UNSPECIFIED.,.F.,.F.,(4,1,1,1,1,1,
1,4),(40.8407044966673,41.1996126991143,42.1922502017863,43.1848877044582,
44.1775252071302,45.1701627098021,46.1628002124741,47.1238898038469),
 .UNSPECIFIED.);
#2447=B_SPLINE_CURVE_WITH_KNOTS('',3,(#20511,#20512,#20513,#20514,#20515,
#20516,#20517,#20518,#20519,#20520,#20521),.UNSPECIFIED.,.F.,.F.,(4,1,1,
1,1,1,1,1,4),(34.5575191894877,34.6896514237625,35.6822889264345,36.6749264291064,
37.6675639317784,38.6602014344503,39.6528389371222,40.6454764397942,40.8407044966673),
 .UNSPECIFIED.);
#2448=B_SPLINE_CURVE_WITH_KNOTS('',3,(#20522,#20523,#20524,#20525,#20526,
#20527,#20528,#20529,#20530,#20531),.UNSPECIFIED.,.F.,.F.,(4,1,1,1,1,1,
1,4),(34.5575191894877,35.2437876830827,36.2364251857546,37.2290626884266,
38.2217001910985,39.2143376937705,40.2069751964424,40.8407044966673),
 .UNSPECIFIED.);
#2449=B_SPLINE_CURVE_WITH_KNOTS('',3,(#20536,#20537,#20538,#20539,#20540,
#20541,#20542,#20543,#20544,#20545),.UNSPECIFIED.,.F.,.F.,(4,1,1,1,1,1,
1,4),(28.2743338823081,28.7338264077309,29.7264639104028,30.7191014130747,
31.7117389157467,32.7043764184186,33.6970139210906,34.5575191894877),
 .UNSPECIFIED.);
#2450=B_SPLINE_CURVE_WITH_KNOTS('',3,(#20546,#20547,#20548,#20549,#20550,
#20551,#20552,#20553,#20554,#20555,#20556),.UNSPECIFIED.,.F.,.F.,(4,1,1,
1,1,1,1,1,4),(28.2743338823081,28.2953251643791,29.287962667051,30.280600169723,
31.2732376723949,32.2658751750668,33.2585126777388,34.2511501804107,34.5575191894877),
 .UNSPECIFIED.);
#2451=B_SPLINE_CURVE_WITH_KNOTS('',3,(#20561,#20562,#20563,#20564,#20565,
#20566,#20567,#20568,#20569,#20570),.UNSPECIFIED.,.F.,.F.,(4,1,1,1,1,1,
1,4),(21.9911485751285,22.7780013916992,23.7706388943711,24.7632763970431,
25.755913899715,26.748551402387,27.7411889050589,28.2743338823081),
 .UNSPECIFIED.);
#2452=B_SPLINE_CURVE_WITH_KNOTS('',3,(#20571,#20572,#20573,#20574,#20575,
#20576,#20577,#20578,#20579,#20580),.UNSPECIFIED.,.F.,.F.,(4,1,1,1,1,1,
1,4),(21.9911485751285,22.3395001483474,23.3321376510193,24.3247751536913,
25.3174126563632,26.3100501590352,27.3026876617071,28.2743338823081),
 .UNSPECIFIED.);
#2453=B_SPLINE_CURVE_WITH_KNOTS('',3,(#20586,#20587,#20588,#20589,#20590),
 .UNSPECIFIED.,.F.,.F.,(4,1,4),(14.3984001269718,15.3910376296438,15.7079632679489),
 .UNSPECIFIED.);
#2454=B_SPLINE_CURVE_WITH_KNOTS('',3,(#20593,#20594,#20595,#20596,#20597),
 .UNSPECIFIED.,.F.,.F.,(4,1,4),(13.8759337553362,14.8369013703236,15.7079632679489),
 .UNSPECIFIED.);
#2455=B_SPLINE_CURVE_WITH_KNOTS('',3,(#20603,#20604,#20605,#20606),
 .UNSPECIFIED.,.F.,.F.,(4,4),(57.8582309055934,58.5656126576448),
 .UNSPECIFIED.);
#2456=B_SPLINE_CURVE_WITH_KNOTS('',3,(#20614,#20615,#20616,#20617,#20618,
#20619,#20620,#20621,#20622,#20623),.UNSPECIFIED.,.F.,.F.,(4,3,3,4),(-56.5486677646163,
-55.5877001496289,-54.595062646957,-54.1144568630778),.UNSPECIFIED.);
#2457=B_SPLINE_CURVE_WITH_KNOTS('',3,(#20628,#20629,#20630,#20631,#20632,
#20633,#20634,#20635,#20636,#20637,#20638,#20639,#20640,#20641,#20642,#20643,
#20644,#20645,#20646,#20647,#20648,#20649,#20650,#20651,#20652),
 .UNSPECIFIED.,.F.,.F.,(4,3,3,3,3,3,3,3,4),(51.5750455984138,51.6171501389411,
52.6097876416131,53.602425144285,54.595062646957,55.5877001496289,56.5803376523009,
57.5729751549728,57.8582309055934),.UNSPECIFIED.);
#2458=B_SPLINE_CURVE_WITH_KNOTS('',3,(#20653,#20654,#20655,#20656,#20657,
#20658,#20659,#20660,#20661,#20662,#20663,#20664,#20665,#20666,#20667,#20668,
#20669,#20670,#20671,#20672,#20673,#20674),.UNSPECIFIED.,.F.,.F.,(4,3,3,
3,3,3,3,4),(-54.1144568630778,-53.602425144285,-52.6097876416131,-51.6171501389411,
-50.6245126362692,-49.6318751335972,-48.6392376309253,-47.8312715558982),
 .UNSPECIFIED.);
#2459=B_SPLINE_CURVE_WITH_KNOTS('',3,(#20679,#20680,#20681,#20682,#20683,
#20684,#20685,#20686,#20687,#20688,#20689,#20690,#20691,#20692,#20693,#20694,
#20695,#20696,#20697,#20698,#20699,#20700),.UNSPECIFIED.,.F.,.F.,(4,3,3,
3,3,3,3,4),(45.2918602912342,45.6613251229095,46.6539626255814,47.6466001282534,
48.6392376309253,49.6318751335973,50.6245126362692,51.5750455984138),
 .UNSPECIFIED.);
#2460=B_SPLINE_CURVE_WITH_KNOTS('',3,(#20701,#20702,#20703,#20704,#20705,
#20706,#20707,#20708,#20709,#20710,#20711,#20712,#20713,#20714,#20715,#20716,
#20717,#20718,#20719,#20720,#20721,#20722,#20723,#20724,#20725),
 .UNSPECIFIED.,.F.,.F.,(4,3,3,3,3,3,3,3,4),(-47.8312715558982,-47.6466001282533,
-46.6539626255814,-45.6613251229095,-44.6686876202375,-43.6760501175656,
-42.6834126148936,-41.6907751122217,-41.5480862487187),.UNSPECIFIED.);
#2461=B_SPLINE_CURVE_WITH_KNOTS('',3,(#20730,#20731,#20732,#20733,#20734,
#20735,#20736,#20737,#20738,#20739,#20740,#20741,#20742,#20743,#20744,#20745,
#20746,#20747,#20748,#20749,#20750,#20751),.UNSPECIFIED.,.F.,.F.,(4,3,3,
3,3,3,3,4),(39.0086749840546,39.7055001068778,40.6981376095497,41.6907751122217,
42.6834126148936,43.6760501175656,44.6686876202375,45.2918602912342),
 .UNSPECIFIED.);
#2462=B_SPLINE_CURVE_WITH_KNOTS('',3,(#20752,#20753,#20754,#20755,#20756,
#20757,#20758,#20759,#20760,#20761,#20762,#20763,#20764,#20765,#20766,#20767,
#20768,#20769,#20770,#20771,#20772,#20773),.UNSPECIFIED.,.F.,.F.,(4,3,3,
3,3,3,3,4),(-41.5480862487187,-40.6981376095497,-39.7055001068778,-38.7128626042058,
-37.7202251015339,-36.727587598862,-35.73495009619,-35.2649009415391),
 .UNSPECIFIED.);
#2463=B_SPLINE_CURVE_WITH_KNOTS('',3,(#20778,#20779,#20780,#20781,#20782,
#20783,#20784,#20785,#20786,#20787,#20788,#20789,#20790,#20791,#20792,#20793,
#20794,#20795,#20796,#20797,#20798,#20799,#20800,#20801,#20802),
 .UNSPECIFIED.,.F.,.F.,(4,3,3,3,3,3,3,3,4),(32.725489676875,32.7570375881742,
33.7496750908461,34.7423125935181,35.73495009619,36.727587598862,37.7202251015339,
38.7128626042059,39.0086749840546),.UNSPECIFIED.);
#2464=B_SPLINE_CURVE_WITH_KNOTS('',3,(#20803,#20804,#20805,#20806,#20807,
#20808,#20809,#20810,#20811,#20812,#20813,#20814,#20815,#20816,#20817,#20818,
#20819,#20820,#20821,#20822,#20823,#20824),.UNSPECIFIED.,.F.,.F.,(4,3,3,
3,3,3,3,4),(-35.2649009415391,-34.7423125935181,-33.7496750908461,-32.7570375881742,
-31.7644000855022,-30.7717625828303,-29.7791250801584,-28.9817156343595),
 .UNSPECIFIED.);
#2465=B_SPLINE_CURVE_WITH_KNOTS('',3,(#20829,#20830,#20831,#20832,#20833,
#20834,#20835,#20836,#20837,#20838,#20839,#20840,#20841,#20842,#20843,#20844,
#20845,#20846,#20847,#20848,#20849,#20850),.UNSPECIFIED.,.F.,.F.,(4,3,3,
3,3,3,3,4),(26.4423043696954,26.8012125721425,27.7938500748145,28.7864875774864,
29.7791250801583,30.7717625828303,31.7644000855022,32.725489676875),
 .UNSPECIFIED.);
#2466=B_SPLINE_CURVE_WITH_KNOTS('',3,(#20851,#20852,#20853,#20854,#20855,
#20856,#20857,#20858,#20859,#20860,#20861,#20862,#20863,#20864,#20865,#20866,
#20867,#20868,#20869,#20870,#20871,#20872,#20873,#20874,#20875),
 .UNSPECIFIED.,.F.,.F.,(4,3,3,3,3,3,3,3,4),(-28.9817156343595,-28.7864875774864,
-27.7938500748145,-26.8012125721425,-25.8085750694706,-24.8159375667986,
-23.8233000641267,-22.8306625614547,-22.6985303271799),.UNSPECIFIED.);
#2467=B_SPLINE_CURVE_WITH_KNOTS('',3,(#20880,#20881,#20882,#20883,#20884,
#20885,#20886,#20887,#20888,#20889,#20890,#20891,#20892,#20893,#20894,#20895,
#20896,#20897,#20898,#20899,#20900,#20901),.UNSPECIFIED.,.F.,.F.,(4,3,3,
3,3,3,3,4),(20.1591190625158,20.8453875561108,21.8380250587828,22.8306625614547,
23.8233000641267,24.8159375667986,25.8085750694706,26.4423043696954),
 .UNSPECIFIED.);
#2468=B_SPLINE_CURVE_WITH_KNOTS('',3,(#20902,#20903,#20904,#20905,#20906,
#20907,#20908,#20909,#20910,#20911,#20912,#20913,#20914,#20915,#20916,#20917,
#20918,#20919,#20920,#20921,#20922,#20923),.UNSPECIFIED.,.F.,.F.,(4,3,3,
3,3,3,3,4),(-22.6985303271799,-21.8380250587828,-20.8453875561108,-19.8527500534389,
-18.860112550767,-17.867475048095,-16.8748375454231,-16.4153450200003),
 .UNSPECIFIED.);
#2469=B_SPLINE_CURVE_WITH_KNOTS('',3,(#20928,#20929,#20930,#20931,#20932,
#20933,#20934,#20935,#20936,#20937,#20938,#20939,#20940,#20941,#20942,#20943,
#20944,#20945,#20946,#20947,#20948,#20949,#20950,#20951,#20952),
 .UNSPECIFIED.,.F.,.F.,(4,3,3,3,3,3,3,3,4),(13.8759337553362,13.8969250374072,
14.8895625400792,15.8822000427511,16.8748375454231,17.867475048095,18.860112550767,
19.8527500534389,20.1591190625158),.UNSPECIFIED.);
#2470=B_SPLINE_CURVE_WITH_KNOTS('',3,(#20953,#20954,#20955,#20956,#20957,
#20958,#20959,#20960,#20961,#20962,#20963,#20964,#20965,#20966,#20967,#20968,
#20969,#20970,#20971,#20972,#20973,#20974),.UNSPECIFIED.,.F.,.F.,(4,3,3,
3,3,3,3,4),(-16.4153450200003,-15.8822000427511,-14.8895625400792,-13.8969250374072,
-12.9042875347353,-11.9116500320633,-10.9190125293914,-10.1321597128207),
 .UNSPECIFIED.);
#2471=B_SPLINE_CURVE_WITH_KNOTS('',3,(#20980,#20981,#20982,#20983,#20984,
#20985,#20986,#20987,#20988,#20989,#20990,#20991,#20992),.UNSPECIFIED.,
 .F.,.F.,(4,3,3,3,4),(-3.84897440564114,-2.97791250801583,-1.98527500534389,
-0.992637502671945,0.),.UNSPECIFIED.);
#2472=B_SPLINE_CURVE_WITH_KNOTS('',3,(#20995,#20996,#20997,#20998,#20999,
#21000,#21001,#21002,#21003,#21004,#21005,#21006,#21007,#21008,#21009,#21010,
#21011,#21012,#21013),.UNSPECIFIED.,.F.,.F.,(4,3,3,3,3,3,4),(2.01694489302845,
2.97791250801584,3.97055001068779,4.96318751335973,5.95582501603167,6.94846251870361,
7.59274844815666),.UNSPECIFIED.);
#2473=B_SPLINE_CURVE_WITH_KNOTS('',3,(#21019,#21020,#21021,#21022,#21023,
#21024,#21025,#21026),.UNSPECIFIED.,.F.,.F.,(4,1,1,1,1,4),(65.9734457253856,
66.4540515092647,67.4466890119367,68.4393265146086,69.4319640172806,70.4246015199525),
 .UNSPECIFIED.);
#2474=B_SPLINE_CURVE_WITH_KNOTS('',3,(#21029,#21030,#21031,#21032,#21033,
#21034,#21035,#21036,#21037),.UNSPECIFIED.,.F.,.F.,(4,1,1,1,1,1,4),(65.9734457253856,
66.015550265913,67.0081877685849,68.0008252712569,68.9934627739288,69.9861002766008,
70.9470678915881),.UNSPECIFIED.);
#2475=B_SPLINE_CURVE_WITH_KNOTS('',3,(#21042,#21043,#21044,#21045,#21046,
#21047,#21048,#21049,#21050,#21051),.UNSPECIFIED.,.F.,.F.,(4,1,1,1,1,1,
1,4),(59.6902604182061,60.4982264932331,61.490863995905,62.483501498577,
63.4761390012489,64.4687765039209,65.4614140065928,65.9734457253856),
 .UNSPECIFIED.);
#2476=B_SPLINE_CURVE_WITH_KNOTS('',3,(#21052,#21053,#21054,#21055,#21056,
#21057,#21058,#21059,#21060,#21061),.UNSPECIFIED.,.F.,.F.,(4,1,1,1,1,1,
1,4),(59.6902604182061,60.0597252498813,61.0523627525533,62.0450002552252,
63.0376377578971,64.0302752605691,65.022912763241,65.9734457253856),
 .UNSPECIFIED.);
#2477=B_SPLINE_CURVE_WITH_KNOTS('',3,(#21066,#21067,#21068,#21069,#21070,
#21071,#21072,#21073,#21074,#21075,#21076),.UNSPECIFIED.,.F.,.F.,(4,1,1,
1,1,1,1,1,4),(53.4070751110265,53.5497639745295,54.5424014772014,55.5350389798734,
56.5276764825453,57.5203139852172,58.5129514878892,59.5055889905611,59.6902604182061),
 .UNSPECIFIED.);
#2478=B_SPLINE_CURVE_WITH_KNOTS('',3,(#21077,#21078,#21079,#21080,#21081,
#21082,#21083,#21084,#21085,#21086),.UNSPECIFIED.,.F.,.F.,(4,1,1,1,1,1,
1,4),(53.4070751110265,54.1039002338496,55.0965377365216,56.0891752391935,
57.0818127418655,58.0744502445374,59.0670877472094,59.6902604182061),
 .UNSPECIFIED.);
#2479=B_SPLINE_CURVE_WITH_KNOTS('',3,(#21091,#21092,#21093,#21094,#21095,
#21096,#21097,#21098,#21099,#21100),.UNSPECIFIED.,.F.,.F.,(4,1,1,1,1,1,
1,4),(47.1238898038469,47.5939389584978,48.5865764611697,49.5792139638417,
50.5718514665136,51.5644889691856,52.5571264718575,53.4070751110265),
 .UNSPECIFIED.);
#2480=B_SPLINE_CURVE_WITH_KNOTS('',3,(#21101,#21102,#21103,#21104,#21105,
#21106,#21107,#21108,#21109,#21110,#21111),.UNSPECIFIED.,.F.,.F.,(4,1,1,
1,1,1,1,1,4),(47.1238898038469,47.155437715146,48.148075217818,49.1407127204899,
50.1333502231619,51.1259877258338,52.1186252285057,53.1112627311777,53.4070751110265),
 .UNSPECIFIED.);
#2481=B_SPLINE_CURVE_WITH_KNOTS('',3,(#21116,#21117,#21118,#21119,#21120,
#21121,#21122,#21123,#21124,#21125),.UNSPECIFIED.,.F.,.F.,(4,1,1,1,1,1,
1,4),(40.8407044966673,41.6381139424661,42.6307514451381,43.62338894781,
44.616026450482,45.6086639531539,46.6013014558259,47.1238898038469),
 .UNSPECIFIED.);
#2482=B_SPLINE_CURVE_WITH_KNOTS('',3,(#21126,#21127,#21128,#21129,#21130,
#21131,#21132,#21133,#21134,#21135),.UNSPECIFIED.,.F.,.F.,(4,1,1,1,1,1,
1,4),(40.8407044966673,41.1996126991143,42.1922502017863,43.1848877044582,
44.1775252071302,45.1701627098021,46.1628002124741,47.1238898038469),
 .UNSPECIFIED.);
#2483=B_SPLINE_CURVE_WITH_KNOTS('',3,(#21140,#21141,#21142,#21143,#21144,
#21145,#21146,#21147,#21148,#21149,#21150),.UNSPECIFIED.,.F.,.F.,(4,1,1,
1,1,1,1,1,4),(34.5575191894877,34.6896514237625,35.6822889264345,36.6749264291064,
37.6675639317784,38.6602014344503,39.6528389371222,40.6454764397942,40.8407044966673),
 .UNSPECIFIED.);
#2484=B_SPLINE_CURVE_WITH_KNOTS('',3,(#21151,#21152,#21153,#21154,#21155,
#21156,#21157,#21158,#21159,#21160),.UNSPECIFIED.,.F.,.F.,(4,1,1,1,1,1,
1,4),(34.5575191894877,35.2437876830827,36.2364251857546,37.2290626884266,
38.2217001910985,39.2143376937705,40.2069751964424,40.8407044966673),
 .UNSPECIFIED.);
#2485=B_SPLINE_CURVE_WITH_KNOTS('',3,(#21165,#21166,#21167,#21168,#21169,
#21170,#21171,#21172,#21173,#21174),.UNSPECIFIED.,.F.,.F.,(4,1,1,1,1,1,
1,4),(28.2743338823081,28.7338264077309,29.7264639104028,30.7191014130747,
31.7117389157467,32.7043764184186,33.6970139210906,34.5575191894877),
 .UNSPECIFIED.);
#2486=B_SPLINE_CURVE_WITH_KNOTS('',3,(#21175,#21176,#21177,#21178,#21179,
#21180,#21181,#21182,#21183,#21184,#21185),.UNSPECIFIED.,.F.,.F.,(4,1,1,
1,1,1,1,1,4),(28.2743338823081,28.2953251643791,29.287962667051,30.280600169723,
31.2732376723949,32.2658751750668,33.2585126777388,34.2511501804107,34.5575191894877),
 .UNSPECIFIED.);
#2487=B_SPLINE_CURVE_WITH_KNOTS('',3,(#21190,#21191,#21192,#21193,#21194,
#21195,#21196,#21197,#21198,#21199),.UNSPECIFIED.,.F.,.F.,(4,1,1,1,1,1,
1,4),(21.9911485751285,22.7780013916992,23.7706388943711,24.7632763970431,
25.755913899715,26.748551402387,27.7411889050589,28.2743338823081),
 .UNSPECIFIED.);
#2488=B_SPLINE_CURVE_WITH_KNOTS('',3,(#21200,#21201,#21202,#21203,#21204,
#21205,#21206,#21207,#21208,#21209),.UNSPECIFIED.,.F.,.F.,(4,1,1,1,1,1,
1,4),(21.9911485751285,22.3395001483474,23.3321376510193,24.3247751536913,
25.3174126563632,26.3100501590352,27.3026876617071,28.2743338823081),
 .UNSPECIFIED.);
#2489=B_SPLINE_CURVE_WITH_KNOTS('',3,(#21215,#21216,#21217,#21218,#21219),
 .UNSPECIFIED.,.F.,.F.,(4,1,4),(14.3984001269718,15.3910376296438,15.7079632679489),
 .UNSPECIFIED.);
#2490=B_SPLINE_CURVE_WITH_KNOTS('',3,(#21222,#21223,#21224,#21225,#21226),
 .UNSPECIFIED.,.F.,.F.,(4,1,4),(13.8759337553362,14.8369013703236,15.7079632679489),
 .UNSPECIFIED.);
#2491=B_SPLINE_CURVE_WITH_KNOTS('',3,(#21232,#21233,#21234,#21235),
 .UNSPECIFIED.,.F.,.F.,(4,4),(57.8582309055934,58.5656126576447),
 .UNSPECIFIED.);
#2492=B_SPLINE_CURVE_WITH_KNOTS('',3,(#21243,#21244,#21245,#21246,#21247,
#21248,#21249,#21250,#21251,#21252),.UNSPECIFIED.,.F.,.F.,(4,3,3,4),(-56.5486677646163,
-55.5877001496289,-54.595062646957,-54.1144568630778),.UNSPECIFIED.);
#2493=B_SPLINE_CURVE_WITH_KNOTS('',3,(#21257,#21258,#21259,#21260,#21261,
#21262,#21263,#21264,#21265,#21266,#21267,#21268,#21269,#21270,#21271,#21272,
#21273,#21274,#21275,#21276,#21277,#21278,#21279,#21280,#21281),
 .UNSPECIFIED.,.F.,.F.,(4,3,3,3,3,3,3,3,4),(51.5750455984138,51.6171501389411,
52.6097876416131,53.602425144285,54.5950626469569,55.5877001496289,56.5803376523008,
57.5729751549728,57.8582309055934),.UNSPECIFIED.);
#2494=B_SPLINE_CURVE_WITH_KNOTS('',3,(#21282,#21283,#21284,#21285,#21286,
#21287,#21288,#21289,#21290,#21291,#21292,#21293,#21294,#21295,#21296,#21297,
#21298,#21299,#21300,#21301,#21302,#21303),.UNSPECIFIED.,.F.,.F.,(4,3,3,
3,3,3,3,4),(-54.1144568630778,-53.602425144285,-52.6097876416131,-51.6171501389411,
-50.6245126362692,-49.6318751335972,-48.6392376309253,-47.8312715558982),
 .UNSPECIFIED.);
#2495=B_SPLINE_CURVE_WITH_KNOTS('',3,(#21308,#21309,#21310,#21311,#21312,
#21313,#21314,#21315,#21316,#21317,#21318,#21319,#21320,#21321,#21322,#21323,
#21324,#21325,#21326,#21327,#21328,#21329),.UNSPECIFIED.,.F.,.F.,(4,3,3,
3,3,3,3,4),(45.2918602912342,45.6613251229094,46.6539626255814,47.6466001282533,
48.6392376309253,49.6318751335972,50.6245126362692,51.5750455984138),
 .UNSPECIFIED.);
#2496=B_SPLINE_CURVE_WITH_KNOTS('',3,(#21330,#21331,#21332,#21333,#21334,
#21335,#21336,#21337,#21338,#21339,#21340,#21341,#21342,#21343,#21344,#21345,
#21346,#21347,#21348,#21349,#21350,#21351,#21352,#21353,#21354),
 .UNSPECIFIED.,.F.,.F.,(4,3,3,3,3,3,3,3,4),(-47.8312715558982,-47.6466001282533,
-46.6539626255814,-45.6613251229095,-44.6686876202375,-43.6760501175656,
-42.6834126148936,-41.6907751122217,-41.5480862487187),.UNSPECIFIED.);
#2497=B_SPLINE_CURVE_WITH_KNOTS('',3,(#21359,#21360,#21361,#21362,#21363,
#21364,#21365,#21366,#21367,#21368,#21369,#21370,#21371,#21372,#21373,#21374,
#21375,#21376,#21377,#21378,#21379,#21380),.UNSPECIFIED.,.F.,.F.,(4,3,3,
3,3,3,3,4),(39.0086749840546,39.7055001068778,40.6981376095497,41.6907751122217,
42.6834126148936,43.6760501175656,44.6686876202375,45.2918602912342),
 .UNSPECIFIED.);
#2498=B_SPLINE_CURVE_WITH_KNOTS('',3,(#21381,#21382,#21383,#21384,#21385,
#21386,#21387,#21388,#21389,#21390,#21391,#21392,#21393,#21394,#21395,#21396,
#21397,#21398,#21399,#21400,#21401,#21402),.UNSPECIFIED.,.F.,.F.,(4,3,3,
3,3,3,3,4),(-41.5480862487187,-40.6981376095497,-39.7055001068778,-38.7128626042058,
-37.7202251015339,-36.727587598862,-35.73495009619,-35.2649009415391),
 .UNSPECIFIED.);
#2499=B_SPLINE_CURVE_WITH_KNOTS('',3,(#21407,#21408,#21409,#21410,#21411,
#21412,#21413,#21414,#21415,#21416,#21417,#21418,#21419,#21420,#21421,#21422,
#21423,#21424,#21425,#21426,#21427,#21428,#21429,#21430,#21431),
 .UNSPECIFIED.,.F.,.F.,(4,3,3,3,3,3,3,3,4),(32.725489676875,32.7570375881742,
33.7496750908461,34.7423125935181,35.73495009619,36.727587598862,37.7202251015339,
38.7128626042058,39.0086749840546),.UNSPECIFIED.);
#2500=B_SPLINE_CURVE_WITH_KNOTS('',3,(#21432,#21433,#21434,#21435,#21436,
#21437,#21438,#21439,#21440,#21441,#21442,#21443,#21444,#21445,#21446,#21447,
#21448,#21449,#21450,#21451,#21452,#21453),.UNSPECIFIED.,.F.,.F.,(4,3,3,
3,3,3,3,4),(-35.2649009415391,-34.7423125935181,-33.7496750908461,-32.7570375881742,
-31.7644000855022,-30.7717625828303,-29.7791250801584,-28.9817156343595),
 .UNSPECIFIED.);
#2501=B_SPLINE_CURVE_WITH_KNOTS('',3,(#21458,#21459,#21460,#21461,#21462,
#21463,#21464,#21465,#21466,#21467,#21468,#21469,#21470,#21471,#21472,#21473,
#21474,#21475,#21476,#21477,#21478,#21479),.UNSPECIFIED.,.F.,.F.,(4,3,3,
3,3,3,3,4),(26.4423043696954,26.8012125721425,27.7938500748145,28.7864875774864,
29.7791250801583,30.7717625828303,31.7644000855022,32.725489676875),
 .UNSPECIFIED.);
#2502=B_SPLINE_CURVE_WITH_KNOTS('',3,(#21480,#21481,#21482,#21483,#21484,
#21485,#21486,#21487,#21488,#21489,#21490,#21491,#21492,#21493,#21494,#21495,
#21496,#21497,#21498,#21499,#21500,#21501,#21502,#21503,#21504),
 .UNSPECIFIED.,.F.,.F.,(4,3,3,3,3,3,3,3,4),(-28.9817156343595,-28.7864875774864,
-27.7938500748145,-26.8012125721425,-25.8085750694706,-24.8159375667986,
-23.8233000641267,-22.8306625614547,-22.6985303271799),.UNSPECIFIED.);
#2503=B_SPLINE_CURVE_WITH_KNOTS('',3,(#21509,#21510,#21511,#21512,#21513,
#21514,#21515,#21516,#21517,#21518,#21519,#21520,#21521,#21522,#21523,#21524,
#21525,#21526,#21527,#21528,#21529,#21530),.UNSPECIFIED.,.F.,.F.,(4,3,3,
3,3,3,3,4),(20.1591190625158,20.8453875561108,21.8380250587828,22.8306625614547,
23.8233000641267,24.8159375667986,25.8085750694706,26.4423043696954),
 .UNSPECIFIED.);
#2504=B_SPLINE_CURVE_WITH_KNOTS('',3,(#21531,#21532,#21533,#21534,#21535,
#21536,#21537,#21538,#21539,#21540,#21541,#21542,#21543,#21544,#21545,#21546,
#21547,#21548,#21549,#21550,#21551,#21552),.UNSPECIFIED.,.F.,.F.,(4,3,3,
3,3,3,3,4),(-22.6985303271799,-21.8380250587828,-20.8453875561108,-19.8527500534389,
-18.8601125507669,-17.867475048095,-16.8748375454231,-16.4153450200003),
 .UNSPECIFIED.);
#2505=B_SPLINE_CURVE_WITH_KNOTS('',3,(#21557,#21558,#21559,#21560,#21561,
#21562,#21563,#21564,#21565,#21566,#21567,#21568,#21569,#21570,#21571,#21572,
#21573,#21574,#21575,#21576,#21577,#21578,#21579,#21580,#21581),
 .UNSPECIFIED.,.F.,.F.,(4,3,3,3,3,3,3,3,4),(13.8759337553362,13.8969250374072,
14.8895625400792,15.8822000427511,16.8748375454231,17.867475048095,18.8601125507669,
19.8527500534389,20.1591190625158),.UNSPECIFIED.);
#2506=B_SPLINE_CURVE_WITH_KNOTS('',3,(#21582,#21583,#21584,#21585,#21586,
#21587,#21588,#21589,#21590,#21591,#21592,#21593,#21594,#21595,#21596,#21597,
#21598,#21599,#21600,#21601,#21602,#21603),.UNSPECIFIED.,.F.,.F.,(4,3,3,
3,3,3,3,4),(-16.4153450200003,-15.8822000427511,-14.8895625400792,-13.8969250374072,
-12.9042875347353,-11.9116500320633,-10.9190125293914,-10.1321597128207),
 .UNSPECIFIED.);
#2507=B_SPLINE_CURVE_WITH_KNOTS('',3,(#21609,#21610,#21611,#21612,#21613,
#21614,#21615,#21616,#21617,#21618,#21619,#21620,#21621),.UNSPECIFIED.,
 .F.,.F.,(4,3,3,3,4),(-3.84897440564114,-2.97791250801584,-1.98527500534389,
-0.992637502671947,0.),.UNSPECIFIED.);
#2508=B_SPLINE_CURVE_WITH_KNOTS('',3,(#21624,#21625,#21626,#21627,#21628,
#21629,#21630,#21631,#21632,#21633,#21634,#21635,#21636,#21637,#21638,#21639,
#21640,#21641,#21642),.UNSPECIFIED.,.F.,.F.,(4,3,3,3,3,3,4),(2.01694489302844,
2.97791250801583,3.97055001068778,4.96318751335972,5.95582501603167,6.94846251870362,
7.59274844815666),.UNSPECIFIED.);
#2509=B_SPLINE_CURVE_WITH_KNOTS('',3,(#21648,#21649,#21650,#21651,#21652,
#21653,#21654,#21655),.UNSPECIFIED.,.F.,.F.,(4,1,1,1,1,4),(65.9734457253856,
66.4540515092647,67.4466890119367,68.4393265146086,69.4319640172806,70.4246015199525),
 .UNSPECIFIED.);
#2510=B_SPLINE_CURVE_WITH_KNOTS('',3,(#21658,#21659,#21660,#21661,#21662,
#21663,#21664,#21665,#21666),.UNSPECIFIED.,.F.,.F.,(4,1,1,1,1,1,4),(65.9734457253856,
66.0155502659129,67.0081877685849,68.0008252712568,68.9934627739288,69.9861002766007,
70.9470678915881),.UNSPECIFIED.);
#2511=B_SPLINE_CURVE_WITH_KNOTS('',3,(#21671,#21672,#21673,#21674,#21675,
#21676,#21677,#21678,#21679,#21680),.UNSPECIFIED.,.F.,.F.,(4,1,1,1,1,1,
1,4),(59.6902604182061,60.4982264932331,61.490863995905,62.483501498577,
63.4761390012489,64.4687765039209,65.4614140065928,65.9734457253856),
 .UNSPECIFIED.);
#2512=B_SPLINE_CURVE_WITH_KNOTS('',3,(#21681,#21682,#21683,#21684,#21685,
#21686,#21687,#21688,#21689,#21690),.UNSPECIFIED.,.F.,.F.,(4,1,1,1,1,1,
1,4),(59.6902604182061,60.0597252498813,61.0523627525532,62.0450002552252,
63.0376377578971,64.0302752605691,65.022912763241,65.9734457253856),
 .UNSPECIFIED.);
#2513=B_SPLINE_CURVE_WITH_KNOTS('',3,(#21695,#21696,#21697,#21698,#21699,
#21700,#21701,#21702,#21703,#21704,#21705),.UNSPECIFIED.,.F.,.F.,(4,1,1,
1,1,1,1,1,4),(53.4070751110265,53.5497639745295,54.5424014772014,55.5350389798734,
56.5276764825453,57.5203139852172,58.5129514878892,59.5055889905611,59.6902604182061),
 .UNSPECIFIED.);
#2514=B_SPLINE_CURVE_WITH_KNOTS('',3,(#21706,#21707,#21708,#21709,#21710,
#21711,#21712,#21713,#21714,#21715),.UNSPECIFIED.,.F.,.F.,(4,1,1,1,1,1,
1,4),(53.4070751110265,54.1039002338496,55.0965377365216,56.0891752391935,
57.0818127418654,58.0744502445374,59.0670877472093,59.6902604182061),
 .UNSPECIFIED.);
#2515=B_SPLINE_CURVE_WITH_KNOTS('',3,(#21720,#21721,#21722,#21723,#21724,
#21725,#21726,#21727,#21728,#21729),.UNSPECIFIED.,.F.,.F.,(4,1,1,1,1,1,
1,4),(47.1238898038469,47.5939389584978,48.5865764611697,49.5792139638417,
50.5718514665136,51.5644889691856,52.5571264718575,53.4070751110265),
 .UNSPECIFIED.);
#2516=B_SPLINE_CURVE_WITH_KNOTS('',3,(#21730,#21731,#21732,#21733,#21734,
#21735,#21736,#21737,#21738,#21739,#21740),.UNSPECIFIED.,.F.,.F.,(4,1,1,
1,1,1,1,1,4),(47.1238898038469,47.155437715146,48.1480752178179,49.1407127204899,
50.1333502231618,51.1259877258338,52.1186252285057,53.1112627311777,53.4070751110265),
 .UNSPECIFIED.);
#2517=B_SPLINE_CURVE_WITH_KNOTS('',3,(#21745,#21746,#21747,#21748,#21749,
#21750,#21751,#21752,#21753,#21754),.UNSPECIFIED.,.F.,.F.,(4,1,1,1,1,1,
1,4),(40.8407044966673,41.6381139424661,42.6307514451381,43.62338894781,
44.616026450482,45.6086639531539,46.6013014558259,47.1238898038469),
 .UNSPECIFIED.);
#2518=B_SPLINE_CURVE_WITH_KNOTS('',3,(#21755,#21756,#21757,#21758,#21759,
#21760,#21761,#21762,#21763,#21764),.UNSPECIFIED.,.F.,.F.,(4,1,1,1,1,1,
1,4),(40.8407044966673,41.1996126991143,42.1922502017863,43.1848877044582,
44.1775252071302,45.1701627098021,46.1628002124741,47.1238898038469),
 .UNSPECIFIED.);
#2519=B_SPLINE_CURVE_WITH_KNOTS('',3,(#21769,#21770,#21771,#21772,#21773,
#21774,#21775,#21776,#21777,#21778,#21779),.UNSPECIFIED.,.F.,.F.,(4,1,1,
1,1,1,1,1,4),(34.5575191894877,34.6896514237625,35.6822889264345,36.6749264291064,
37.6675639317784,38.6602014344503,39.6528389371222,40.6454764397942,40.8407044966673),
 .UNSPECIFIED.);
#2520=B_SPLINE_CURVE_WITH_KNOTS('',3,(#21780,#21781,#21782,#21783,#21784,
#21785,#21786,#21787,#21788,#21789),.UNSPECIFIED.,.F.,.F.,(4,1,1,1,1,1,
1,4),(34.5575191894877,35.2437876830827,36.2364251857546,37.2290626884266,
38.2217001910985,39.2143376937704,40.2069751964424,40.8407044966673),
 .UNSPECIFIED.);
#2521=B_SPLINE_CURVE_WITH_KNOTS('',3,(#21794,#21795,#21796,#21797,#21798,
#21799,#21800,#21801,#21802,#21803),.UNSPECIFIED.,.F.,.F.,(4,1,1,1,1,1,
1,4),(28.2743338823081,28.7338264077309,29.7264639104028,30.7191014130747,
31.7117389157467,32.7043764184186,33.6970139210906,34.5575191894877),
 .UNSPECIFIED.);
#2522=B_SPLINE_CURVE_WITH_KNOTS('',3,(#21804,#21805,#21806,#21807,#21808,
#21809,#21810,#21811,#21812,#21813,#21814),.UNSPECIFIED.,.F.,.F.,(4,1,1,
1,1,1,1,1,4),(28.2743338823081,28.2953251643791,29.287962667051,30.2806001697229,
31.2732376723949,32.2658751750668,33.2585126777388,34.2511501804107,34.5575191894877),
 .UNSPECIFIED.);
#2523=B_SPLINE_CURVE_WITH_KNOTS('',3,(#21819,#21820,#21821,#21822,#21823,
#21824,#21825,#21826,#21827,#21828),.UNSPECIFIED.,.F.,.F.,(4,1,1,1,1,1,
1,4),(21.9911485751285,22.7780013916992,23.7706388943711,24.7632763970431,
25.755913899715,26.748551402387,27.7411889050589,28.2743338823081),
 .UNSPECIFIED.);
#2524=B_SPLINE_CURVE_WITH_KNOTS('',3,(#21829,#21830,#21831,#21832,#21833,
#21834,#21835,#21836,#21837,#21838),.UNSPECIFIED.,.F.,.F.,(4,1,1,1,1,1,
1,4),(21.9911485751285,22.3395001483474,23.3321376510193,24.3247751536913,
25.3174126563632,26.3100501590352,27.3026876617071,28.2743338823081),
 .UNSPECIFIED.);
#2525=B_SPLINE_CURVE_WITH_KNOTS('',3,(#21844,#21845,#21846,#21847,#21848),
 .UNSPECIFIED.,.F.,.F.,(4,1,4),(14.3984001269718,15.3910376296438,15.7079632679489),
 .UNSPECIFIED.);
#2526=B_SPLINE_CURVE_WITH_KNOTS('',3,(#21851,#21852,#21853,#21854,#21855),
 .UNSPECIFIED.,.F.,.F.,(4,1,4),(13.8759337553362,14.8369013703236,15.7079632679489),
 .UNSPECIFIED.);
#2527=B_SPLINE_CURVE_WITH_KNOTS('',3,(#21861,#21862,#21863,#21864),
 .UNSPECIFIED.,.F.,.F.,(4,4),(57.8582309055934,58.5656126576448),
 .UNSPECIFIED.);
#2528=B_SPLINE_CURVE_WITH_KNOTS('',3,(#21872,#21873,#21874,#21875,#21876,
#21877,#21878,#21879,#21880,#21881),.UNSPECIFIED.,.F.,.F.,(4,3,3,4),(-56.5486677646163,
-55.5877001496289,-54.595062646957,-54.1144568630778),.UNSPECIFIED.);
#2529=B_SPLINE_CURVE_WITH_KNOTS('',3,(#21886,#21887,#21888,#21889,#21890,
#21891,#21892,#21893,#21894,#21895,#21896,#21897,#21898,#21899,#21900,#21901,
#21902,#21903,#21904,#21905,#21906,#21907,#21908,#21909,#21910),
 .UNSPECIFIED.,.F.,.F.,(4,3,3,3,3,3,3,3,4),(51.5750455984138,51.6171501389411,
52.6097876416131,53.602425144285,54.595062646957,55.5877001496289,56.5803376523009,
57.5729751549728,57.8582309055934),.UNSPECIFIED.);
#2530=B_SPLINE_CURVE_WITH_KNOTS('',3,(#21911,#21912,#21913,#21914,#21915,
#21916,#21917,#21918,#21919,#21920,#21921,#21922,#21923,#21924,#21925,#21926,
#21927,#21928,#21929,#21930,#21931,#21932),.UNSPECIFIED.,.F.,.F.,(4,3,3,
3,3,3,3,4),(-54.1144568630778,-53.602425144285,-52.6097876416131,-51.6171501389411,
-50.6245126362692,-49.6318751335972,-48.6392376309253,-47.8312715558982),
 .UNSPECIFIED.);
#2531=B_SPLINE_CURVE_WITH_KNOTS('',3,(#21937,#21938,#21939,#21940,#21941,
#21942,#21943,#21944,#21945,#21946,#21947,#21948,#21949,#21950,#21951,#21952,
#21953,#21954,#21955,#21956,#21957,#21958),.UNSPECIFIED.,.F.,.F.,(4,3,3,
3,3,3,3,4),(45.2918602912342,45.6613251229095,46.6539626255814,47.6466001282534,
48.6392376309253,49.6318751335972,50.6245126362692,51.5750455984138),
 .UNSPECIFIED.);
#2532=B_SPLINE_CURVE_WITH_KNOTS('',3,(#21959,#21960,#21961,#21962,#21963,
#21964,#21965,#21966,#21967,#21968,#21969,#21970,#21971,#21972,#21973,#21974,
#21975,#21976,#21977,#21978,#21979,#21980,#21981,#21982,#21983),
 .UNSPECIFIED.,.F.,.F.,(4,3,3,3,3,3,3,3,4),(-47.8312715558982,-47.6466001282533,
-46.6539626255814,-45.6613251229094,-44.6686876202375,-43.6760501175656,
-42.6834126148936,-41.6907751122217,-41.5480862487187),.UNSPECIFIED.);
#2533=B_SPLINE_CURVE_WITH_KNOTS('',3,(#21988,#21989,#21990,#21991,#21992,
#21993,#21994,#21995,#21996,#21997,#21998,#21999,#22000,#22001,#22002,#22003,
#22004,#22005,#22006,#22007,#22008,#22009),.UNSPECIFIED.,.F.,.F.,(4,3,3,
3,3,3,3,4),(39.0086749840546,39.7055001068778,40.6981376095497,41.6907751122217,
42.6834126148936,43.6760501175656,44.6686876202375,45.2918602912342),
 .UNSPECIFIED.);
#2534=B_SPLINE_CURVE_WITH_KNOTS('',3,(#22010,#22011,#22012,#22013,#22014,
#22015,#22016,#22017,#22018,#22019,#22020,#22021,#22022,#22023,#22024,#22025,
#22026,#22027,#22028,#22029,#22030,#22031),.UNSPECIFIED.,.F.,.F.,(4,3,3,
3,3,3,3,4),(-41.5480862487187,-40.6981376095497,-39.7055001068778,-38.7128626042058,
-37.7202251015339,-36.7275875988619,-35.73495009619,-35.2649009415391),
 .UNSPECIFIED.);
#2535=B_SPLINE_CURVE_WITH_KNOTS('',3,(#22036,#22037,#22038,#22039,#22040,
#22041,#22042,#22043,#22044,#22045,#22046,#22047,#22048,#22049,#22050,#22051,
#22052,#22053,#22054,#22055,#22056,#22057,#22058,#22059,#22060),
 .UNSPECIFIED.,.F.,.F.,(4,3,3,3,3,3,3,3,4),(32.725489676875,32.7570375881742,
33.7496750908461,34.7423125935181,35.73495009619,36.727587598862,37.7202251015339,
38.7128626042059,39.0086749840546),.UNSPECIFIED.);
#2536=B_SPLINE_CURVE_WITH_KNOTS('',3,(#22061,#22062,#22063,#22064,#22065,
#22066,#22067,#22068,#22069,#22070,#22071,#22072,#22073,#22074,#22075,#22076,
#22077,#22078,#22079,#22080,#22081,#22082),.UNSPECIFIED.,.F.,.F.,(4,3,3,
3,3,3,3,4),(-35.2649009415391,-34.7423125935181,-33.7496750908461,-32.7570375881742,
-31.7644000855022,-30.7717625828303,-29.7791250801583,-28.9817156343595),
 .UNSPECIFIED.);
#2537=B_SPLINE_CURVE_WITH_KNOTS('',3,(#22087,#22088,#22089,#22090,#22091,
#22092,#22093,#22094,#22095,#22096,#22097,#22098,#22099,#22100,#22101,#22102,
#22103,#22104,#22105,#22106,#22107,#22108),.UNSPECIFIED.,.F.,.F.,(4,3,3,
3,3,3,3,4),(26.4423043696954,26.8012125721425,27.7938500748145,28.7864875774864,
29.7791250801583,30.7717625828303,31.7644000855022,32.725489676875),
 .UNSPECIFIED.);
#2538=B_SPLINE_CURVE_WITH_KNOTS('',3,(#22109,#22110,#22111,#22112,#22113,
#22114,#22115,#22116,#22117,#22118,#22119,#22120,#22121,#22122,#22123,#22124,
#22125,#22126,#22127,#22128,#22129,#22130,#22131,#22132,#22133),
 .UNSPECIFIED.,.F.,.F.,(4,3,3,3,3,3,3,3,4),(-28.9817156343595,-28.7864875774864,
-27.7938500748144,-26.8012125721425,-25.8085750694706,-24.8159375667986,
-23.8233000641267,-22.8306625614547,-22.6985303271799),.UNSPECIFIED.);
#2539=B_SPLINE_CURVE_WITH_KNOTS('',3,(#22138,#22139,#22140,#22141,#22142,
#22143,#22144,#22145,#22146,#22147,#22148,#22149,#22150,#22151,#22152,#22153,
#22154,#22155,#22156,#22157,#22158,#22159),.UNSPECIFIED.,.F.,.F.,(4,3,3,
3,3,3,3,4),(20.1591190625158,20.8453875561108,21.8380250587828,22.8306625614547,
23.8233000641267,24.8159375667986,25.8085750694706,26.4423043696954),
 .UNSPECIFIED.);
#2540=B_SPLINE_CURVE_WITH_KNOTS('',3,(#22160,#22161,#22162,#22163,#22164,
#22165,#22166,#22167,#22168,#22169,#22170,#22171,#22172,#22173,#22174,#22175,
#22176,#22177,#22178,#22179,#22180,#22181),.UNSPECIFIED.,.F.,.F.,(4,3,3,
3,3,3,3,4),(-22.6985303271799,-21.8380250587828,-20.8453875561108,-19.8527500534389,
-18.8601125507669,-17.867475048095,-16.8748375454231,-16.4153450200003),
 .UNSPECIFIED.);
#2541=B_SPLINE_CURVE_WITH_KNOTS('',3,(#22186,#22187,#22188,#22189,#22190,
#22191,#22192,#22193,#22194,#22195,#22196,#22197,#22198,#22199,#22200,#22201,
#22202,#22203,#22204,#22205,#22206,#22207,#22208,#22209,#22210),
 .UNSPECIFIED.,.F.,.F.,(4,3,3,3,3,3,3,3,4),(13.8759337553362,13.8969250374072,
14.8895625400792,15.8822000427511,16.8748375454231,17.867475048095,18.860112550767,
19.8527500534389,20.1591190625158),.UNSPECIFIED.);
#2542=B_SPLINE_CURVE_WITH_KNOTS('',3,(#22211,#22212,#22213,#22214,#22215,
#22216,#22217,#22218,#22219,#22220,#22221,#22222,#22223,#22224,#22225,#22226,
#22227,#22228,#22229,#22230,#22231,#22232),.UNSPECIFIED.,.F.,.F.,(4,3,3,
3,3,3,3,4),(-16.4153450200003,-15.8822000427511,-14.8895625400792,-13.8969250374072,
-12.9042875347353,-11.9116500320633,-10.9190125293914,-10.1321597128207),
 .UNSPECIFIED.);
#2543=B_SPLINE_CURVE_WITH_KNOTS('',3,(#22238,#22239,#22240,#22241,#22242,
#22243,#22244,#22245,#22246,#22247,#22248,#22249,#22250),.UNSPECIFIED.,
 .F.,.F.,(4,3,3,3,4),(-3.84897440564113,-2.97791250801583,-1.98527500534389,
-0.992637502671945,0.),.UNSPECIFIED.);
#2544=B_SPLINE_CURVE_WITH_KNOTS('',3,(#22253,#22254,#22255,#22256,#22257,
#22258,#22259,#22260,#22261,#22262,#22263,#22264,#22265,#22266,#22267,#22268,
#22269,#22270,#22271),.UNSPECIFIED.,.F.,.F.,(4,3,3,3,3,3,4),(2.0169448930284,
2.97791250801584,3.97055001068778,4.96318751335973,5.95582501603167,6.94846251870361,
7.59274844815666),.UNSPECIFIED.);
#2545=B_SPLINE_CURVE_WITH_KNOTS('',3,(#22277,#22278,#22279,#22280,#22281,
#22282,#22283,#22284),.UNSPECIFIED.,.F.,.F.,(4,1,1,1,1,4),(65.9734457253856,
66.4540515092647,67.4466890119367,68.4393265146086,69.4319640172806,70.4246015199525),
 .UNSPECIFIED.);
#2546=B_SPLINE_CURVE_WITH_KNOTS('',3,(#22287,#22288,#22289,#22290,#22291,
#22292,#22293,#22294,#22295),.UNSPECIFIED.,.F.,.F.,(4,1,1,1,1,1,4),(65.9734457253857,
66.015550265913,67.0081877685849,68.0008252712569,68.9934627739288,69.9861002766008,
70.9470678915881),.UNSPECIFIED.);
#2547=B_SPLINE_CURVE_WITH_KNOTS('',3,(#22300,#22301,#22302,#22303,#22304,
#22305,#22306,#22307,#22308,#22309),.UNSPECIFIED.,.F.,.F.,(4,1,1,1,1,1,
1,4),(59.6902604182061,60.4982264932331,61.490863995905,62.483501498577,
63.4761390012489,64.4687765039209,65.4614140065928,65.9734457253856),
 .UNSPECIFIED.);
#2548=B_SPLINE_CURVE_WITH_KNOTS('',3,(#22310,#22311,#22312,#22313,#22314,
#22315,#22316,#22317,#22318,#22319),.UNSPECIFIED.,.F.,.F.,(4,1,1,1,1,1,
1,4),(59.6902604182061,60.0597252498813,61.0523627525533,62.0450002552252,
63.0376377578971,64.0302752605691,65.022912763241,65.9734457253857),
 .UNSPECIFIED.);
#2549=B_SPLINE_CURVE_WITH_KNOTS('',3,(#22324,#22325,#22326,#22327,#22328,
#22329,#22330,#22331,#22332,#22333,#22334),.UNSPECIFIED.,.F.,.F.,(4,1,1,
1,1,1,1,1,4),(53.4070751110265,53.5497639745295,54.5424014772014,55.5350389798734,
56.5276764825453,57.5203139852172,58.5129514878892,59.5055889905611,59.6902604182061),
 .UNSPECIFIED.);
#2550=B_SPLINE_CURVE_WITH_KNOTS('',3,(#22335,#22336,#22337,#22338,#22339,
#22340,#22341,#22342,#22343,#22344),.UNSPECIFIED.,.F.,.F.,(4,1,1,1,1,1,
1,4),(53.4070751110265,54.1039002338496,55.0965377365216,56.0891752391935,
57.0818127418655,58.0744502445374,59.0670877472094,59.6902604182061),
 .UNSPECIFIED.);
#2551=B_SPLINE_CURVE_WITH_KNOTS('',3,(#22349,#22350,#22351,#22352,#22353,
#22354,#22355,#22356,#22357,#22358),.UNSPECIFIED.,.F.,.F.,(4,1,1,1,1,1,
1,4),(47.1238898038469,47.5939389584978,48.5865764611697,49.5792139638417,
50.5718514665136,51.5644889691856,52.5571264718575,53.4070751110265),
 .UNSPECIFIED.);
#2552=B_SPLINE_CURVE_WITH_KNOTS('',3,(#22359,#22360,#22361,#22362,#22363,
#22364,#22365,#22366,#22367,#22368,#22369),.UNSPECIFIED.,.F.,.F.,(4,1,1,
1,1,1,1,1,4),(47.1238898038469,47.155437715146,48.148075217818,49.1407127204899,
50.1333502231619,51.1259877258338,52.1186252285057,53.1112627311777,53.4070751110265),
 .UNSPECIFIED.);
#2553=B_SPLINE_CURVE_WITH_KNOTS('',3,(#22374,#22375,#22376,#22377,#22378,
#22379,#22380,#22381,#22382,#22383),.UNSPECIFIED.,.F.,.F.,(4,1,1,1,1,1,
1,4),(40.8407044966673,41.6381139424661,42.6307514451381,43.62338894781,
44.616026450482,45.6086639531539,46.6013014558259,47.1238898038469),
 .UNSPECIFIED.);
#2554=B_SPLINE_CURVE_WITH_KNOTS('',3,(#22384,#22385,#22386,#22387,#22388,
#22389,#22390,#22391,#22392,#22393),.UNSPECIFIED.,.F.,.F.,(4,1,1,1,1,1,
1,4),(40.8407044966673,41.1996126991143,42.1922502017863,43.1848877044582,
44.1775252071302,45.1701627098021,46.1628002124741,47.1238898038469),
 .UNSPECIFIED.);
#2555=B_SPLINE_CURVE_WITH_KNOTS('',3,(#22398,#22399,#22400,#22401,#22402,
#22403,#22404,#22405,#22406,#22407,#22408),.UNSPECIFIED.,.F.,.F.,(4,1,1,
1,1,1,1,1,4),(34.5575191894877,34.6896514237625,35.6822889264345,36.6749264291064,
37.6675639317784,38.6602014344503,39.6528389371222,40.6454764397942,40.8407044966673),
 .UNSPECIFIED.);
#2556=B_SPLINE_CURVE_WITH_KNOTS('',3,(#22409,#22410,#22411,#22412,#22413,
#22414,#22415,#22416,#22417,#22418),.UNSPECIFIED.,.F.,.F.,(4,1,1,1,1,1,
1,4),(34.5575191894877,35.2437876830827,36.2364251857546,37.2290626884266,
38.2217001910985,39.2143376937705,40.2069751964424,40.8407044966673),
 .UNSPECIFIED.);
#2557=B_SPLINE_CURVE_WITH_KNOTS('',3,(#22423,#22424,#22425,#22426,#22427,
#22428,#22429,#22430,#22431,#22432),.UNSPECIFIED.,.F.,.F.,(4,1,1,1,1,1,
1,4),(28.2743338823081,28.7338264077309,29.7264639104028,30.7191014130747,
31.7117389157467,32.7043764184186,33.6970139210906,34.5575191894877),
 .UNSPECIFIED.);
#2558=B_SPLINE_CURVE_WITH_KNOTS('',3,(#22433,#22434,#22435,#22436,#22437,
#22438,#22439,#22440,#22441,#22442,#22443),.UNSPECIFIED.,.F.,.F.,(4,1,1,
1,1,1,1,1,4),(28.2743338823081,28.2953251643791,29.287962667051,30.280600169723,
31.2732376723949,32.2658751750668,33.2585126777388,34.2511501804107,34.5575191894877),
 .UNSPECIFIED.);
#2559=B_SPLINE_CURVE_WITH_KNOTS('',3,(#22448,#22449,#22450,#22451,#22452,
#22453,#22454,#22455,#22456,#22457),.UNSPECIFIED.,.F.,.F.,(4,1,1,1,1,1,
1,4),(21.9911485751285,22.7780013916992,23.7706388943711,24.7632763970431,
25.755913899715,26.748551402387,27.7411889050589,28.2743338823081),
 .UNSPECIFIED.);
#2560=B_SPLINE_CURVE_WITH_KNOTS('',3,(#22458,#22459,#22460,#22461,#22462,
#22463,#22464,#22465,#22466,#22467),.UNSPECIFIED.,.F.,.F.,(4,1,1,1,1,1,
1,4),(21.9911485751285,22.3395001483474,23.3321376510193,24.3247751536913,
25.3174126563632,26.3100501590352,27.3026876617071,28.2743338823081),
 .UNSPECIFIED.);
#2561=B_SPLINE_CURVE_WITH_KNOTS('',3,(#22473,#22474,#22475,#22476,#22477),
 .UNSPECIFIED.,.F.,.F.,(4,1,4),(14.3984001269718,15.3910376296438,15.7079632679489),
 .UNSPECIFIED.);
#2562=B_SPLINE_CURVE_WITH_KNOTS('',3,(#22480,#22481,#22482,#22483,#22484),
 .UNSPECIFIED.,.F.,.F.,(4,1,4),(13.8759337553362,14.8369013703236,15.7079632679489),
 .UNSPECIFIED.);
#2563=B_SPLINE_CURVE_WITH_KNOTS('',3,(#22490,#22491,#22492,#22493),
 .UNSPECIFIED.,.F.,.F.,(4,4),(57.8582309055934,58.5656126576448),
 .UNSPECIFIED.);
#2564=B_SPLINE_CURVE_WITH_KNOTS('',3,(#22501,#22502,#22503,#22504,#22505,
#22506,#22507,#22508,#22509,#22510),.UNSPECIFIED.,.F.,.F.,(4,3,3,4),(-56.5486677646163,
-55.5877001496289,-54.595062646957,-54.1144568630779),.UNSPECIFIED.);
#2565=B_SPLINE_CURVE_WITH_KNOTS('',3,(#22515,#22516,#22517,#22518,#22519,
#22520,#22521,#22522,#22523,#22524,#22525,#22526,#22527,#22528,#22529,#22530,
#22531,#22532,#22533,#22534,#22535,#22536,#22537,#22538,#22539),
 .UNSPECIFIED.,.F.,.F.,(4,3,3,3,3,3,3,3,4),(51.5750455984138,51.6171501389411,
52.6097876416131,53.602425144285,54.595062646957,55.5877001496289,56.5803376523009,
57.5729751549728,57.8582309055934),.UNSPECIFIED.);
#2566=B_SPLINE_CURVE_WITH_KNOTS('',3,(#22540,#22541,#22542,#22543,#22544,
#22545,#22546,#22547,#22548,#22549,#22550,#22551,#22552,#22553,#22554,#22555,
#22556,#22557,#22558,#22559,#22560,#22561),.UNSPECIFIED.,.F.,.F.,(4,3,3,
3,3,3,3,4),(-54.1144568630779,-53.602425144285,-52.6097876416131,-51.6171501389411,
-50.6245126362692,-49.6318751335972,-48.6392376309253,-47.8312715558983),
 .UNSPECIFIED.);
#2567=B_SPLINE_CURVE_WITH_KNOTS('',3,(#22566,#22567,#22568,#22569,#22570,
#22571,#22572,#22573,#22574,#22575,#22576,#22577,#22578,#22579,#22580,#22581,
#22582,#22583,#22584,#22585,#22586,#22587),.UNSPECIFIED.,.F.,.F.,(4,3,3,
3,3,3,3,4),(45.2918602912342,45.6613251229095,46.6539626255814,47.6466001282534,
48.6392376309253,49.6318751335972,50.6245126362692,51.5750455984138),
 .UNSPECIFIED.);
#2568=B_SPLINE_CURVE_WITH_KNOTS('',3,(#22588,#22589,#22590,#22591,#22592,
#22593,#22594,#22595,#22596,#22597,#22598,#22599,#22600,#22601,#22602,#22603,
#22604,#22605,#22606,#22607,#22608,#22609,#22610,#22611,#22612),
 .UNSPECIFIED.,.F.,.F.,(4,3,3,3,3,3,3,3,4),(-47.8312715558983,-47.6466001282533,
-46.6539626255814,-45.6613251229095,-44.6686876202375,-43.6760501175656,
-42.6834126148936,-41.6907751122217,-41.5480862487187),.UNSPECIFIED.);
#2569=B_SPLINE_CURVE_WITH_KNOTS('',3,(#22617,#22618,#22619,#22620,#22621,
#22622,#22623,#22624,#22625,#22626,#22627,#22628,#22629,#22630,#22631,#22632,
#22633,#22634,#22635,#22636,#22637,#22638),.UNSPECIFIED.,.F.,.F.,(4,3,3,
3,3,3,3,4),(39.0086749840546,39.7055001068778,40.6981376095497,41.6907751122217,
42.6834126148936,43.6760501175656,44.6686876202375,45.2918602912342),
 .UNSPECIFIED.);
#2570=B_SPLINE_CURVE_WITH_KNOTS('',3,(#22639,#22640,#22641,#22642,#22643,
#22644,#22645,#22646,#22647,#22648,#22649,#22650,#22651,#22652,#22653,#22654,
#22655,#22656,#22657,#22658,#22659,#22660),.UNSPECIFIED.,.F.,.F.,(4,3,3,
3,3,3,3,4),(-41.5480862487187,-40.6981376095497,-39.7055001068778,-38.7128626042058,
-37.7202251015339,-36.727587598862,-35.73495009619,-35.2649009415391),
 .UNSPECIFIED.);
#2571=B_SPLINE_CURVE_WITH_KNOTS('',3,(#22665,#22666,#22667,#22668,#22669,
#22670,#22671,#22672,#22673,#22674,#22675,#22676,#22677,#22678,#22679,#22680,
#22681,#22682,#22683,#22684,#22685,#22686,#22687,#22688,#22689),
 .UNSPECIFIED.,.F.,.F.,(4,3,3,3,3,3,3,3,4),(32.725489676875,32.7570375881742,
33.7496750908461,34.7423125935181,35.73495009619,36.727587598862,37.7202251015339,
38.7128626042059,39.0086749840546),.UNSPECIFIED.);
#2572=B_SPLINE_CURVE_WITH_KNOTS('',3,(#22690,#22691,#22692,#22693,#22694,
#22695,#22696,#22697,#22698,#22699,#22700,#22701,#22702,#22703,#22704,#22705,
#22706,#22707,#22708,#22709,#22710,#22711),.UNSPECIFIED.,.F.,.F.,(4,3,3,
3,3,3,3,4),(-35.2649009415391,-34.7423125935181,-33.7496750908461,-32.7570375881742,
-31.7644000855022,-30.7717625828303,-29.7791250801583,-28.9817156343595),
 .UNSPECIFIED.);
#2573=B_SPLINE_CURVE_WITH_KNOTS('',3,(#22716,#22717,#22718,#22719,#22720,
#22721,#22722,#22723,#22724,#22725,#22726,#22727,#22728,#22729,#22730,#22731,
#22732,#22733,#22734,#22735,#22736,#22737),.UNSPECIFIED.,.F.,.F.,(4,3,3,
3,3,3,3,4),(26.4423043696954,26.8012125721425,27.7938500748145,28.7864875774864,
29.7791250801583,30.7717625828303,31.7644000855022,32.725489676875),
 .UNSPECIFIED.);
#2574=B_SPLINE_CURVE_WITH_KNOTS('',3,(#22738,#22739,#22740,#22741,#22742,
#22743,#22744,#22745,#22746,#22747,#22748,#22749,#22750,#22751,#22752,#22753,
#22754,#22755,#22756,#22757,#22758,#22759,#22760,#22761,#22762),
 .UNSPECIFIED.,.F.,.F.,(4,3,3,3,3,3,3,3,4),(-28.9817156343595,-28.7864875774864,
-27.7938500748144,-26.8012125721425,-25.8085750694706,-24.8159375667986,
-23.8233000641267,-22.8306625614547,-22.6985303271799),.UNSPECIFIED.);
#2575=B_SPLINE_CURVE_WITH_KNOTS('',3,(#22767,#22768,#22769,#22770,#22771,
#22772,#22773,#22774,#22775,#22776,#22777,#22778,#22779,#22780,#22781,#22782,
#22783,#22784,#22785,#22786,#22787,#22788),.UNSPECIFIED.,.F.,.F.,(4,3,3,
3,3,3,3,4),(20.1591190625158,20.8453875561108,21.8380250587828,22.8306625614547,
23.8233000641267,24.8159375667986,25.8085750694706,26.4423043696954),
 .UNSPECIFIED.);
#2576=B_SPLINE_CURVE_WITH_KNOTS('',3,(#22789,#22790,#22791,#22792,#22793,
#22794,#22795,#22796,#22797,#22798,#22799,#22800,#22801,#22802,#22803,#22804,
#22805,#22806,#22807,#22808,#22809,#22810),.UNSPECIFIED.,.F.,.F.,(4,3,3,
3,3,3,3,4),(-22.6985303271799,-21.8380250587828,-20.8453875561108,-19.8527500534389,
-18.860112550767,-17.867475048095,-16.8748375454231,-16.4153450200003),
 .UNSPECIFIED.);
#2577=B_SPLINE_CURVE_WITH_KNOTS('',3,(#22815,#22816,#22817,#22818,#22819,
#22820,#22821,#22822,#22823,#22824,#22825,#22826,#22827,#22828,#22829,#22830,
#22831,#22832,#22833,#22834,#22835,#22836,#22837,#22838,#22839),
 .UNSPECIFIED.,.F.,.F.,(4,3,3,3,3,3,3,3,4),(13.8759337553363,13.8969250374072,
14.8895625400792,15.8822000427511,16.8748375454231,17.867475048095,18.860112550767,
19.8527500534389,20.1591190625158),.UNSPECIFIED.);
#2578=B_SPLINE_CURVE_WITH_KNOTS('',3,(#22840,#22841,#22842,#22843,#22844,
#22845,#22846,#22847,#22848,#22849,#22850,#22851,#22852,#22853,#22854,#22855,
#22856,#22857,#22858,#22859,#22860,#22861),.UNSPECIFIED.,.F.,.F.,(4,3,3,
3,3,3,3,4),(-16.4153450200003,-15.8822000427511,-14.8895625400792,-13.8969250374072,
-12.9042875347353,-11.9116500320633,-10.9190125293914,-10.1321597128207),
 .UNSPECIFIED.);
#2579=B_SPLINE_CURVE_WITH_KNOTS('',3,(#22867,#22868,#22869,#22870,#22871,
#22872,#22873,#22874,#22875,#22876,#22877,#22878,#22879),.UNSPECIFIED.,
 .F.,.F.,(4,3,3,3,4),(-3.84897440564114,-2.97791250801584,-1.98527500534389,
-0.992637502671945,0.),.UNSPECIFIED.);
#2580=B_SPLINE_CURVE_WITH_KNOTS('',3,(#22882,#22883,#22884,#22885,#22886,
#22887,#22888,#22889,#22890,#22891,#22892,#22893,#22894,#22895,#22896,#22897,
#22898,#22899,#22900),.UNSPECIFIED.,.F.,.F.,(4,3,3,3,3,3,4),(2.01694489302845,
2.97791250801584,3.97055001068778,4.96318751335972,5.95582501603167,6.94846251870361,
7.59274844815667),.UNSPECIFIED.);
#2581=B_SPLINE_CURVE_WITH_KNOTS('',3,(#22906,#22907,#22908,#22909,#22910,
#22911,#22912,#22913),.UNSPECIFIED.,.F.,.F.,(4,1,1,1,1,4),(65.9734457253856,
66.4540515092647,67.4466890119367,68.4393265146086,69.4319640172806,70.4246015199525),
 .UNSPECIFIED.);
#2582=B_SPLINE_CURVE_WITH_KNOTS('',3,(#22916,#22917,#22918,#22919,#22920,
#22921,#22922,#22923,#22924),.UNSPECIFIED.,.F.,.F.,(4,1,1,1,1,1,4),(65.9734457253856,
66.015550265913,67.0081877685849,68.0008252712569,68.9934627739288,69.9861002766008,
70.9470678915881),.UNSPECIFIED.);
#2583=B_SPLINE_CURVE_WITH_KNOTS('',3,(#22929,#22930,#22931,#22932,#22933,
#22934,#22935,#22936,#22937,#22938),.UNSPECIFIED.,.F.,.F.,(4,1,1,1,1,1,
1,4),(59.690260418206,60.4982264932331,61.490863995905,62.483501498577,
63.4761390012489,64.4687765039209,65.4614140065928,65.9734457253856),
 .UNSPECIFIED.);
#2584=B_SPLINE_CURVE_WITH_KNOTS('',3,(#22939,#22940,#22941,#22942,#22943,
#22944,#22945,#22946,#22947,#22948),.UNSPECIFIED.,.F.,.F.,(4,1,1,1,1,1,
1,4),(59.6902604182061,60.0597252498813,61.0523627525533,62.0450002552252,
63.0376377578971,64.0302752605691,65.022912763241,65.9734457253856),
 .UNSPECIFIED.);
#2585=B_SPLINE_CURVE_WITH_KNOTS('',3,(#22953,#22954,#22955,#22956,#22957,
#22958,#22959,#22960,#22961,#22962,#22963),.UNSPECIFIED.,.F.,.F.,(4,1,1,
1,1,1,1,1,4),(53.4070751110265,53.5497639745295,54.5424014772014,55.5350389798734,
56.5276764825453,57.5203139852172,58.5129514878892,59.5055889905611,59.690260418206),
 .UNSPECIFIED.);
#2586=B_SPLINE_CURVE_WITH_KNOTS('',3,(#22964,#22965,#22966,#22967,#22968,
#22969,#22970,#22971,#22972,#22973),.UNSPECIFIED.,.F.,.F.,(4,1,1,1,1,1,
1,4),(53.4070751110265,54.1039002338496,55.0965377365216,56.0891752391935,
57.0818127418655,58.0744502445374,59.0670877472094,59.6902604182061),
 .UNSPECIFIED.);
#2587=B_SPLINE_CURVE_WITH_KNOTS('',3,(#22978,#22979,#22980,#22981,#22982,
#22983,#22984,#22985,#22986,#22987),.UNSPECIFIED.,.F.,.F.,(4,1,1,1,1,1,
1,4),(47.1238898038469,47.5939389584978,48.5865764611697,49.5792139638417,
50.5718514665136,51.5644889691856,52.5571264718575,53.4070751110265),
 .UNSPECIFIED.);
#2588=B_SPLINE_CURVE_WITH_KNOTS('',3,(#22988,#22989,#22990,#22991,#22992,
#22993,#22994,#22995,#22996,#22997,#22998),.UNSPECIFIED.,.F.,.F.,(4,1,1,
1,1,1,1,1,4),(47.1238898038469,47.155437715146,48.148075217818,49.1407127204899,
50.1333502231619,51.1259877258338,52.1186252285057,53.1112627311777,53.4070751110265),
 .UNSPECIFIED.);
#2589=B_SPLINE_CURVE_WITH_KNOTS('',3,(#23003,#23004,#23005,#23006,#23007,
#23008,#23009,#23010,#23011,#23012),.UNSPECIFIED.,.F.,.F.,(4,1,1,1,1,1,
1,4),(40.8407044966673,41.6381139424661,42.6307514451381,43.62338894781,
44.616026450482,45.6086639531539,46.6013014558259,47.1238898038469),
 .UNSPECIFIED.);
#2590=B_SPLINE_CURVE_WITH_KNOTS('',3,(#23013,#23014,#23015,#23016,#23017,
#23018,#23019,#23020,#23021,#23022),.UNSPECIFIED.,.F.,.F.,(4,1,1,1,1,1,
1,4),(40.8407044966673,41.1996126991143,42.1922502017863,43.1848877044582,
44.1775252071302,45.1701627098021,46.1628002124741,47.1238898038469),
 .UNSPECIFIED.);
#2591=B_SPLINE_CURVE_WITH_KNOTS('',3,(#23027,#23028,#23029,#23030,#23031,
#23032,#23033,#23034,#23035,#23036,#23037),.UNSPECIFIED.,.F.,.F.,(4,1,1,
1,1,1,1,1,4),(34.5575191894877,34.6896514237625,35.6822889264345,36.6749264291064,
37.6675639317784,38.6602014344503,39.6528389371222,40.6454764397942,40.8407044966673),
 .UNSPECIFIED.);
#2592=B_SPLINE_CURVE_WITH_KNOTS('',3,(#23038,#23039,#23040,#23041,#23042,
#23043,#23044,#23045,#23046,#23047),.UNSPECIFIED.,.F.,.F.,(4,1,1,1,1,1,
1,4),(34.5575191894877,35.2437876830827,36.2364251857546,37.2290626884266,
38.2217001910985,39.2143376937705,40.2069751964424,40.8407044966673),
 .UNSPECIFIED.);
#2593=B_SPLINE_CURVE_WITH_KNOTS('',3,(#23052,#23053,#23054,#23055,#23056,
#23057,#23058,#23059,#23060,#23061),.UNSPECIFIED.,.F.,.F.,(4,1,1,1,1,1,
1,4),(28.2743338823081,28.7338264077309,29.7264639104028,30.7191014130747,
31.7117389157467,32.7043764184186,33.6970139210906,34.5575191894877),
 .UNSPECIFIED.);
#2594=B_SPLINE_CURVE_WITH_KNOTS('',3,(#23062,#23063,#23064,#23065,#23066,
#23067,#23068,#23069,#23070,#23071,#23072),.UNSPECIFIED.,.F.,.F.,(4,1,1,
1,1,1,1,1,4),(28.2743338823081,28.2953251643791,29.287962667051,30.280600169723,
31.2732376723949,32.2658751750668,33.2585126777388,34.2511501804107,34.5575191894877),
 .UNSPECIFIED.);
#2595=B_SPLINE_CURVE_WITH_KNOTS('',3,(#23077,#23078,#23079,#23080,#23081,
#23082,#23083,#23084,#23085,#23086),.UNSPECIFIED.,.F.,.F.,(4,1,1,1,1,1,
1,4),(21.9911485751285,22.7780013916992,23.7706388943711,24.7632763970431,
25.755913899715,26.748551402387,27.7411889050589,28.2743338823081),
 .UNSPECIFIED.);
#2596=B_SPLINE_CURVE_WITH_KNOTS('',3,(#23087,#23088,#23089,#23090,#23091,
#23092,#23093,#23094,#23095,#23096),.UNSPECIFIED.,.F.,.F.,(4,1,1,1,1,1,
1,4),(21.9911485751285,22.3395001483474,23.3321376510193,24.3247751536913,
25.3174126563632,26.3100501590352,27.3026876617071,28.2743338823081),
 .UNSPECIFIED.);
#2597=B_SPLINE_CURVE_WITH_KNOTS('',3,(#23102,#23103,#23104,#23105,#23106),
 .UNSPECIFIED.,.F.,.F.,(4,1,4),(14.3984001269718,15.3910376296438,15.7079632679489),
 .UNSPECIFIED.);
#2598=B_SPLINE_CURVE_WITH_KNOTS('',3,(#23109,#23110,#23111,#23112,#23113),
 .UNSPECIFIED.,.F.,.F.,(4,1,4),(13.8759337553362,14.8369013703236,15.7079632679489),
 .UNSPECIFIED.);
#2599=B_SPLINE_CURVE_WITH_KNOTS('',3,(#23119,#23120,#23121,#23122),
 .UNSPECIFIED.,.F.,.F.,(4,4),(57.8582309055934,58.5656126576447),
 .UNSPECIFIED.);
#2600=B_SPLINE_CURVE_WITH_KNOTS('',3,(#23130,#23131,#23132,#23133,#23134,
#23135,#23136,#23137,#23138,#23139),.UNSPECIFIED.,.F.,.F.,(4,3,3,4),(-56.5486677646163,
-55.5877001496289,-54.595062646957,-54.1144568630778),.UNSPECIFIED.);
#2601=B_SPLINE_CURVE_WITH_KNOTS('',3,(#23144,#23145,#23146,#23147,#23148,
#23149,#23150,#23151,#23152,#23153,#23154,#23155,#23156,#23157,#23158,#23159,
#23160,#23161,#23162,#23163,#23164,#23165,#23166,#23167,#23168),
 .UNSPECIFIED.,.F.,.F.,(4,3,3,3,3,3,3,3,4),(51.5750455984138,51.6171501389411,
52.6097876416131,53.602425144285,54.595062646957,55.5877001496289,56.5803376523009,
57.5729751549728,57.8582309055934),.UNSPECIFIED.);
#2602=B_SPLINE_CURVE_WITH_KNOTS('',3,(#23169,#23170,#23171,#23172,#23173,
#23174,#23175,#23176,#23177,#23178,#23179,#23180,#23181,#23182,#23183,#23184,
#23185,#23186,#23187,#23188,#23189,#23190),.UNSPECIFIED.,.F.,.F.,(4,3,3,
3,3,3,3,4),(-54.1144568630778,-53.602425144285,-52.6097876416131,-51.6171501389411,
-50.6245126362692,-49.6318751335972,-48.6392376309253,-47.8312715558982),
 .UNSPECIFIED.);
#2603=B_SPLINE_CURVE_WITH_KNOTS('',3,(#23195,#23196,#23197,#23198,#23199,
#23200,#23201,#23202,#23203,#23204,#23205,#23206,#23207,#23208,#23209,#23210,
#23211,#23212,#23213,#23214,#23215,#23216),.UNSPECIFIED.,.F.,.F.,(4,3,3,
3,3,3,3,4),(45.2918602912342,45.6613251229095,46.6539626255814,47.6466001282534,
48.6392376309253,49.6318751335972,50.6245126362692,51.5750455984138),
 .UNSPECIFIED.);
#2604=B_SPLINE_CURVE_WITH_KNOTS('',3,(#23217,#23218,#23219,#23220,#23221,
#23222,#23223,#23224,#23225,#23226,#23227,#23228,#23229,#23230,#23231,#23232,
#23233,#23234,#23235,#23236,#23237,#23238,#23239,#23240,#23241),
 .UNSPECIFIED.,.F.,.F.,(4,3,3,3,3,3,3,3,4),(-47.8312715558982,-47.6466001282533,
-46.6539626255814,-45.6613251229095,-44.6686876202375,-43.6760501175656,
-42.6834126148936,-41.6907751122217,-41.5480862487187),.UNSPECIFIED.);
#2605=B_SPLINE_CURVE_WITH_KNOTS('',3,(#23246,#23247,#23248,#23249,#23250,
#23251,#23252,#23253,#23254,#23255,#23256,#23257,#23258,#23259,#23260,#23261,
#23262,#23263,#23264,#23265,#23266,#23267),.UNSPECIFIED.,.F.,.F.,(4,3,3,
3,3,3,3,4),(39.0086749840546,39.7055001068778,40.6981376095497,41.6907751122217,
42.6834126148936,43.6760501175656,44.6686876202375,45.2918602912342),
 .UNSPECIFIED.);
#2606=B_SPLINE_CURVE_WITH_KNOTS('',3,(#23268,#23269,#23270,#23271,#23272,
#23273,#23274,#23275,#23276,#23277,#23278,#23279,#23280,#23281,#23282,#23283,
#23284,#23285,#23286,#23287,#23288,#23289),.UNSPECIFIED.,.F.,.F.,(4,3,3,
3,3,3,3,4),(-41.5480862487187,-40.6981376095497,-39.7055001068778,-38.7128626042058,
-37.7202251015339,-36.727587598862,-35.73495009619,-35.2649009415391),
 .UNSPECIFIED.);
#2607=B_SPLINE_CURVE_WITH_KNOTS('',3,(#23294,#23295,#23296,#23297,#23298,
#23299,#23300,#23301,#23302,#23303,#23304,#23305,#23306,#23307,#23308,#23309,
#23310,#23311,#23312,#23313,#23314,#23315,#23316,#23317,#23318),
 .UNSPECIFIED.,.F.,.F.,(4,3,3,3,3,3,3,3,4),(32.725489676875,32.7570375881742,
33.7496750908461,34.7423125935181,35.73495009619,36.727587598862,37.7202251015339,
38.7128626042059,39.0086749840546),.UNSPECIFIED.);
#2608=B_SPLINE_CURVE_WITH_KNOTS('',3,(#23319,#23320,#23321,#23322,#23323,
#23324,#23325,#23326,#23327,#23328,#23329,#23330,#23331,#23332,#23333,#23334,
#23335,#23336,#23337,#23338,#23339,#23340),.UNSPECIFIED.,.F.,.F.,(4,3,3,
3,3,3,3,4),(-35.2649009415391,-34.7423125935181,-33.7496750908461,-32.7570375881742,
-31.7644000855022,-30.7717625828303,-29.7791250801584,-28.9817156343595),
 .UNSPECIFIED.);
#2609=B_SPLINE_CURVE_WITH_KNOTS('',3,(#23345,#23346,#23347,#23348,#23349,
#23350,#23351,#23352,#23353,#23354,#23355,#23356,#23357,#23358,#23359,#23360,
#23361,#23362,#23363,#23364,#23365,#23366),.UNSPECIFIED.,.F.,.F.,(4,3,3,
3,3,3,3,4),(26.4423043696954,26.8012125721425,27.7938500748145,28.7864875774864,
29.7791250801584,30.7717625828303,31.7644000855022,32.725489676875),
 .UNSPECIFIED.);
#2610=B_SPLINE_CURVE_WITH_KNOTS('',3,(#23367,#23368,#23369,#23370,#23371,
#23372,#23373,#23374,#23375,#23376,#23377,#23378,#23379,#23380,#23381,#23382,
#23383,#23384,#23385,#23386,#23387,#23388,#23389,#23390,#23391),
 .UNSPECIFIED.,.F.,.F.,(4,3,3,3,3,3,3,3,4),(-28.9817156343595,-28.7864875774864,
-27.7938500748145,-26.8012125721425,-25.8085750694706,-24.8159375667986,
-23.8233000641267,-22.8306625614547,-22.6985303271799),.UNSPECIFIED.);
#2611=B_SPLINE_CURVE_WITH_KNOTS('',3,(#23396,#23397,#23398,#23399,#23400,
#23401,#23402,#23403,#23404,#23405,#23406,#23407,#23408,#23409,#23410,#23411,
#23412,#23413,#23414,#23415,#23416,#23417),.UNSPECIFIED.,.F.,.F.,(4,3,3,
3,3,3,3,4),(20.1591190625158,20.8453875561108,21.8380250587828,22.8306625614547,
23.8233000641267,24.8159375667986,25.8085750694706,26.4423043696954),
 .UNSPECIFIED.);
#2612=B_SPLINE_CURVE_WITH_KNOTS('',3,(#23418,#23419,#23420,#23421,#23422,
#23423,#23424,#23425,#23426,#23427,#23428,#23429,#23430,#23431,#23432,#23433,
#23434,#23435,#23436,#23437,#23438,#23439),.UNSPECIFIED.,.F.,.F.,(4,3,3,
3,3,3,3,4),(-22.6985303271799,-21.8380250587828,-20.8453875561108,-19.8527500534389,
-18.8601125507669,-17.867475048095,-16.8748375454231,-16.4153450200003),
 .UNSPECIFIED.);
#2613=B_SPLINE_CURVE_WITH_KNOTS('',3,(#23444,#23445,#23446,#23447,#23448,
#23449,#23450,#23451,#23452,#23453,#23454,#23455,#23456,#23457,#23458,#23459,
#23460,#23461,#23462,#23463,#23464,#23465,#23466,#23467,#23468),
 .UNSPECIFIED.,.F.,.F.,(4,3,3,3,3,3,3,3,4),(13.8759337553363,13.8969250374072,
14.8895625400792,15.8822000427511,16.8748375454231,17.867475048095,18.860112550767,
19.8527500534389,20.1591190625158),.UNSPECIFIED.);
#2614=B_SPLINE_CURVE_WITH_KNOTS('',3,(#23469,#23470,#23471,#23472,#23473,
#23474,#23475,#23476,#23477,#23478,#23479,#23480,#23481,#23482,#23483,#23484,
#23485,#23486,#23487,#23488,#23489,#23490),.UNSPECIFIED.,.F.,.F.,(4,3,3,
3,3,3,3,4),(-16.4153450200003,-15.8822000427511,-14.8895625400792,-13.8969250374072,
-12.9042875347353,-11.9116500320633,-10.9190125293914,-10.1321597128207),
 .UNSPECIFIED.);
#2615=B_SPLINE_CURVE_WITH_KNOTS('',3,(#23496,#23497,#23498,#23499,#23500,
#23501,#23502,#23503,#23504,#23505,#23506,#23507,#23508),.UNSPECIFIED.,
 .F.,.F.,(4,3,3,3,4),(-3.84897440564114,-2.97791250801583,-1.98527500534389,
-0.992637502671944,0.),.UNSPECIFIED.);
#2616=B_SPLINE_CURVE_WITH_KNOTS('',3,(#23511,#23512,#23513,#23514,#23515,
#23516,#23517,#23518,#23519,#23520,#23521,#23522,#23523,#23524,#23525,#23526,
#23527,#23528,#23529),.UNSPECIFIED.,.F.,.F.,(4,3,3,3,3,3,4),(2.01694489302844,
2.97791250801584,3.97055001068778,4.96318751335973,5.95582501603167,6.94846251870362,
7.59274844815667),.UNSPECIFIED.);
#2617=B_SPLINE_CURVE_WITH_KNOTS('',3,(#23535,#23536,#23537,#23538,#23539,
#23540,#23541,#23542),.UNSPECIFIED.,.F.,.F.,(4,1,1,1,1,4),(65.9734457253856,
66.4540515092648,67.4466890119367,68.4393265146086,69.4319640172806,70.4246015199525),
 .UNSPECIFIED.);
#2618=B_SPLINE_CURVE_WITH_KNOTS('',3,(#23545,#23546,#23547,#23548,#23549,
#23550,#23551,#23552,#23553),.UNSPECIFIED.,.F.,.F.,(4,1,1,1,1,1,4),(65.9734457253856,
66.015550265913,67.0081877685849,68.0008252712568,68.9934627739288,69.9861002766007,
70.9470678915881),.UNSPECIFIED.);
#2619=B_SPLINE_CURVE_WITH_KNOTS('',3,(#23558,#23559,#23560,#23561,#23562,
#23563,#23564,#23565,#23566,#23567),.UNSPECIFIED.,.F.,.F.,(4,1,1,1,1,1,
1,4),(59.6902604182061,60.4982264932331,61.490863995905,62.483501498577,
63.4761390012489,64.4687765039209,65.4614140065928,65.9734457253856),
 .UNSPECIFIED.);
#2620=B_SPLINE_CURVE_WITH_KNOTS('',3,(#23568,#23569,#23570,#23571,#23572,
#23573,#23574,#23575,#23576,#23577),.UNSPECIFIED.,.F.,.F.,(4,1,1,1,1,1,
1,4),(59.6902604182061,60.0597252498813,61.0523627525532,62.0450002552252,
63.0376377578971,64.0302752605691,65.022912763241,65.9734457253856),
 .UNSPECIFIED.);
#2621=B_SPLINE_CURVE_WITH_KNOTS('',3,(#23582,#23583,#23584,#23585,#23586,
#23587,#23588,#23589,#23590,#23591,#23592),.UNSPECIFIED.,.F.,.F.,(4,1,1,
1,1,1,1,1,4),(53.4070751110265,53.5497639745295,54.5424014772014,55.5350389798734,
56.5276764825453,57.5203139852172,58.5129514878892,59.5055889905611,59.6902604182061),
 .UNSPECIFIED.);
#2622=B_SPLINE_CURVE_WITH_KNOTS('',3,(#23593,#23594,#23595,#23596,#23597,
#23598,#23599,#23600,#23601,#23602),.UNSPECIFIED.,.F.,.F.,(4,1,1,1,1,1,
1,4),(53.4070751110265,54.1039002338496,55.0965377365216,56.0891752391935,
57.0818127418655,58.0744502445374,59.0670877472093,59.6902604182061),
 .UNSPECIFIED.);
#2623=B_SPLINE_CURVE_WITH_KNOTS('',3,(#23607,#23608,#23609,#23610,#23611,
#23612,#23613,#23614,#23615,#23616),.UNSPECIFIED.,.F.,.F.,(4,1,1,1,1,1,
1,4),(47.1238898038469,47.5939389584978,48.5865764611697,49.5792139638417,
50.5718514665136,51.5644889691856,52.5571264718575,53.4070751110265),
 .UNSPECIFIED.);
#2624=B_SPLINE_CURVE_WITH_KNOTS('',3,(#23617,#23618,#23619,#23620,#23621,
#23622,#23623,#23624,#23625,#23626,#23627),.UNSPECIFIED.,.F.,.F.,(4,1,1,
1,1,1,1,1,4),(47.1238898038469,47.155437715146,48.1480752178179,49.1407127204899,
50.1333502231618,51.1259877258338,52.1186252285057,53.1112627311777,53.4070751110265),
 .UNSPECIFIED.);
#2625=B_SPLINE_CURVE_WITH_KNOTS('',3,(#23632,#23633,#23634,#23635,#23636,
#23637,#23638,#23639,#23640,#23641),.UNSPECIFIED.,.F.,.F.,(4,1,1,1,1,1,
1,4),(40.8407044966673,41.6381139424661,42.6307514451381,43.62338894781,
44.616026450482,45.6086639531539,46.6013014558259,47.1238898038469),
 .UNSPECIFIED.);
#2626=B_SPLINE_CURVE_WITH_KNOTS('',3,(#23642,#23643,#23644,#23645,#23646,
#23647,#23648,#23649,#23650,#23651),.UNSPECIFIED.,.F.,.F.,(4,1,1,1,1,1,
1,4),(40.8407044966673,41.1996126991143,42.1922502017863,43.1848877044582,
44.1775252071302,45.1701627098021,46.1628002124741,47.1238898038469),
 .UNSPECIFIED.);
#2627=B_SPLINE_CURVE_WITH_KNOTS('',3,(#23656,#23657,#23658,#23659,#23660,
#23661,#23662,#23663,#23664,#23665,#23666),.UNSPECIFIED.,.F.,.F.,(4,1,1,
1,1,1,1,1,4),(34.5575191894877,34.6896514237625,35.6822889264345,36.6749264291064,
37.6675639317784,38.6602014344503,39.6528389371222,40.6454764397942,40.8407044966673),
 .UNSPECIFIED.);
#2628=B_SPLINE_CURVE_WITH_KNOTS('',3,(#23667,#23668,#23669,#23670,#23671,
#23672,#23673,#23674,#23675,#23676),.UNSPECIFIED.,.F.,.F.,(4,1,1,1,1,1,
1,4),(34.5575191894877,35.2437876830827,36.2364251857546,37.2290626884266,
38.2217001910985,39.2143376937704,40.2069751964424,40.8407044966673),
 .UNSPECIFIED.);
#2629=B_SPLINE_CURVE_WITH_KNOTS('',3,(#23681,#23682,#23683,#23684,#23685,
#23686,#23687,#23688,#23689,#23690),.UNSPECIFIED.,.F.,.F.,(4,1,1,1,1,1,
1,4),(28.2743338823081,28.7338264077309,29.7264639104028,30.7191014130747,
31.7117389157467,32.7043764184186,33.6970139210906,34.5575191894877),
 .UNSPECIFIED.);
#2630=B_SPLINE_CURVE_WITH_KNOTS('',3,(#23691,#23692,#23693,#23694,#23695,
#23696,#23697,#23698,#23699,#23700,#23701),.UNSPECIFIED.,.F.,.F.,(4,1,1,
1,1,1,1,1,4),(28.2743338823081,28.2953251643791,29.287962667051,30.2806001697229,
31.2732376723949,32.2658751750668,33.2585126777388,34.2511501804107,34.5575191894877),
 .UNSPECIFIED.);
#2631=B_SPLINE_CURVE_WITH_KNOTS('',3,(#23706,#23707,#23708,#23709,#23710,
#23711,#23712,#23713,#23714,#23715),.UNSPECIFIED.,.F.,.F.,(4,1,1,1,1,1,
1,4),(21.9911485751285,22.7780013916992,23.7706388943711,24.7632763970431,
25.755913899715,26.748551402387,27.7411889050589,28.2743338823081),
 .UNSPECIFIED.);
#2632=B_SPLINE_CURVE_WITH_KNOTS('',3,(#23716,#23717,#23718,#23719,#23720,
#23721,#23722,#23723,#23724,#23725),.UNSPECIFIED.,.F.,.F.,(4,1,1,1,1,1,
1,4),(21.9911485751285,22.3395001483474,23.3321376510193,24.3247751536913,
25.3174126563632,26.3100501590352,27.3026876617071,28.2743338823081),
 .UNSPECIFIED.);
#2633=B_SPLINE_CURVE_WITH_KNOTS('',3,(#23731,#23732,#23733,#23734,#23735),
 .UNSPECIFIED.,.F.,.F.,(4,1,4),(14.3984001269718,15.3910376296438,15.7079632679489),
 .UNSPECIFIED.);
#2634=B_SPLINE_CURVE_WITH_KNOTS('',3,(#23738,#23739,#23740,#23741,#23742),
 .UNSPECIFIED.,.F.,.F.,(4,1,4),(13.8759337553362,14.8369013703236,15.7079632679489),
 .UNSPECIFIED.);
#2635=B_SPLINE_CURVE_WITH_KNOTS('',3,(#23796,#23797,#23798,#23799,#23800,
#23801,#23802,#23803,#23804,#23805,#23806,#23807,#23808,#23809,#23810,#23811,
#23812,#23813,#23814,#23815,#23816,#23817,#23818,#23819,#23820,#23821,#23822,
#23823,#23824,#23825,#23826,#23827,#23828,#23829,#23830,#23831,#23832,#23833,
#23834,#23835,#23836,#23837,#23838,#23839,#23840,#23841,#23842,#23843,#23844,
#23845,#23846,#23847,#23848,#23849,#23850,#23851,#23852,#23853,#23854,#23855,
#23856,#23857,#23858,#23859,#23860,#23861,#23862,#23863,#23864,#23865,#23866,
#23867,#23868,#23869,#23870,#23871,#23872,#23873,#23874,#23875,#23876,#23877,
#23878,#23879,#23880,#23881,#23882,#23883,#23884,#23885,#23886,#23887,#23888,
#23889),.UNSPECIFIED.,.F.,.F.,(4,3,3,3,3,3,3,3,3,3,3,3,3,3,3,3,3,3,3,3,
3,3,3,3,3,3,3,3,3,3,3,4),(-0.569248610399519,-0.543573521275112,-0.517270334894588,
-0.510403597501912,-0.504800301943937,-0.477738562936544,-0.455893959419014,
-0.447075871895859,-0.442407285930102,-0.414674892956538,-0.386513329416069,
-0.358572400845104,-0.344674734332904,-0.340104787267607,-0.311173962811257,
-0.302981734796303,-0.275165122896056,-0.246719621409672,-0.236777833320522,
-0.231757247321404,-0.227578652734185,-0.198579230964211,-0.169010642259111,
-0.139211776300183,-0.123031160575437,-0.117998606549764,-0.113391716242956,
-0.0828441510686728,-0.0522701024998839,-0.0223137899294547,-0.00976685050221584,
0.),.UNSPECIFIED.);
#2636=B_SPLINE_CURVE_WITH_KNOTS('',3,(#23890,#23891,#23892,#23893,#23894,
#23895,#23896,#23897,#23898,#23899,#23900,#23901,#23902,#23903,#23904,#23905,
#23906,#23907,#23908,#23909,#23910,#23911,#23912,#23913,#23914,#23915,#23916,
#23917,#23918,#23919,#23920,#23921,#23922,#23923,#23924,#23925,#23926,#23927,
#23928,#23929,#23930,#23931,#23932,#23933,#23934,#23935,#23936,#23937,#23938,
#23939,#23940,#23941,#23942,#23943,#23944,#23945,#23946,#23947,#23948,#23949,
#23950,#23951,#23952,#23953,#23954,#23955,#23956,#23957,#23958,#23959,#23960,
#23961,#23962,#23963,#23964,#23965,#23966,#23967,#23968,#23969,#23970,#23971,
#23972,#23973,#23974,#23975,#23976,#23977,#23978,#23979,#23980,#23981,#23982,
#23983),.UNSPECIFIED.,.F.,.F.,(4,3,3,3,3,3,3,3,3,3,3,3,3,3,3,3,3,3,3,3,
3,3,3,3,3,3,3,3,3,3,3,4),(-0.566847306048109,-0.536665088445275,-0.506058869929166,
-0.497416819810769,-0.490479649741127,-0.46033271574735,-0.437086681478693,
-0.424703687019547,-0.42046272258324,-0.391037834184797,-0.361869486038122,
-0.333545859254429,-0.318750504840346,-0.313020117693916,-0.30866018151949,
-0.280670752475326,-0.274364441598099,-0.245887082813539,-0.21615615821092,
-0.204673879614289,-0.200549632065964,-0.172713962599083,-0.14494922019829,
-0.117659631761598,-0.103957138540472,-0.0999252379237537,-0.0958138251359032,
-0.0691413140129682,-0.0429166578991969,-0.017493208914001,-0.00803968599259055,
0.),.UNSPECIFIED.);
#2637=B_SPLINE_CURVE_WITH_KNOTS('',3,(#23985,#23986,#23987,#23988,#23989,
#23990,#23991,#23992,#23993,#23994,#23995),.UNSPECIFIED.,.F.,.F.,(4,1,1,
1,1,1,1,1,4),(15.7079632679489,15.8295388729956,16.8221763756675,17.8148138783395,
18.8074513810114,19.8000888836834,20.7927263863553,21.7853638890272,21.9911485751285),
 .UNSPECIFIED.);
#2638=B_SPLINE_CURVE_WITH_KNOTS('',3,(#23996,#23997,#23998,#23999,#24000,
#24001,#24002,#24003,#24004,#24005),.UNSPECIFIED.,.F.,.F.,(4,1,1,1,1,1,
1,4),(15.7079632679489,16.3836751323157,17.3763126349877,18.3689501376596,
19.3615876403316,20.3542251430035,21.3468626456754,21.9911485751285),
 .UNSPECIFIED.);
#2639=B_SPLINE_CURVE_WITH_KNOTS('',3,(#24254,#24255,#24256,#24257,#24258,
#24259,#24260,#24261,#24262,#24263,#24264,#24265,#24266,#24267,#24268,#24269,
#24270,#24271,#24272,#24273,#24274,#24275,#24276,#24277,#24278,#24279,#24280,
#24281,#24282,#24283,#24284,#24285,#24286,#24287,#24288,#24289,#24290,#24291,
#24292,#24293,#24294,#24295,#24296,#24297,#24298,#24299,#24300,#24301,#24302,
#24303,#24304,#24305,#24306,#24307,#24308,#24309,#24310,#24311,#24312,#24313,
#24314,#24315,#24316,#24317,#24318,#24319,#24320,#24321,#24322,#24323,#24324,
#24325,#24326,#24327,#24328,#24329,#24330,#24331,#24332,#24333,#24334,#24335,
#24336,#24337,#24338,#24339,#24340,#24341,#24342,#24343,#24344),
 .UNSPECIFIED.,.F.,.F.,(4,3,3,3,3,3,3,3,3,3,3,3,3,3,3,3,3,3,3,3,3,3,3,3,
3,3,3,3,3,3,4),(0.,0.025364227043299,0.0513999158242781,0.0781558845304562,
0.0899177963079168,0.0966255877899614,0.102679521308728,0.129980995912345,
0.157733300312116,0.184661891602512,0.195928358257316,0.202971023563161,
0.20709884911213,0.236273257292916,0.265447665473703,0.293340547237465,
0.302677560574438,0.308745297675078,0.31452875584614,0.34260671879725,0.371727098701369,
0.401175544565762,0.421351009768009,0.42675374067059,0.456805248025141,
0.481883952215566,0.490048831459895,0.498378778112269,0.528887549635078,
0.557120064786841,0.566847306048159),.UNSPECIFIED.);
#2640=B_SPLINE_CURVE_WITH_KNOTS('',3,(#24345,#24346,#24347,#24348,#24349,
#24350,#24351,#24352,#24353,#24354,#24355,#24356,#24357,#24358,#24359,#24360,
#24361,#24362,#24363,#24364,#24365,#24366,#24367,#24368,#24369),
 .UNSPECIFIED.,.F.,.F.,(4,3,3,3,3,3,3,3,4),(-10.1321597128207,-9.92637502671944,
-8.9337375240475,-7.94110002137556,-6.94846251870361,-5.95582501603167,
-4.96318751335973,-3.97055001068778,-3.84897440564114),.UNSPECIFIED.);
#2641=B_SPLINE_CURVE_WITH_KNOTS('',3,(#24618,#24619,#24620,#24621,#24622,
#24623,#24624,#24625,#24626,#24627,#24628,#24629,#24630,#24631,#24632,#24633,
#24634,#24635,#24636,#24637,#24638,#24639),.UNSPECIFIED.,.F.,.F.,(4,3,3,
3,3,3,3,4),(7.59274844815667,7.94110002137556,8.9337375240475,9.92637502671945,
10.9190125293914,11.9116500320633,12.9042875347353,13.8759337553363),
 .UNSPECIFIED.);
#2642=B_SPLINE_CURVE_WITH_KNOTS('',3,(#24640,#24641,#24642,#24643,#24644,
#24645,#24646,#24647,#24648,#24649,#24650,#24651,#24652,#24653,#24654,#24655,
#24656,#24657,#24658,#24659,#24660,#24661,#24662,#24663,#24664,#24665,#24666,
#24667,#24668,#24669,#24670,#24671,#24672,#24673,#24674,#24675,#24676,#24677,
#24678,#24679,#24680,#24681,#24682,#24683,#24684,#24685,#24686,#24687,#24688,
#24689,#24690,#24691,#24692,#24693,#24694,#24695,#24696,#24697,#24698,#24699,
#24700,#24701,#24702,#24703,#24704,#24705,#24706,#24707,#24708,#24709,#24710,
#24711,#24712,#24713,#24714,#24715,#24716,#24717,#24718,#24719,#24720,#24721,
#24722,#24723,#24724,#24725,#24726,#24727,#24728,#24729,#24730),
 .UNSPECIFIED.,.F.,.F.,(4,3,3,3,3,3,3,3,3,3,3,3,3,3,3,3,3,3,3,3,3,3,3,3,
3,3,3,3,3,3,4),(0.,0.0297250789974743,0.0601087924509222,0.0893485781496982,
0.114933390636127,0.120627516286913,0.150386820364465,0.179982109044272,
0.208493351293487,0.220471801725418,0.228882355327184,0.234177134950228,
0.264102106495679,0.29200679839712,0.29402707804113,0.322973448322085,0.339362620925793,
0.343535829100154,0.371629352207137,0.399767745756159,0.427502104297442,
0.437970824675921,0.445641165257623,0.450375052516567,0.478076743972786,
0.498853012564951,0.508250460865973,0.513369595206828,0.539284549530519,
0.561181818341445,0.569248610399484),.UNSPECIFIED.);
#2643=B_SPLINE_CURVE_WITH_KNOTS('',3,(#24733,#24734,#24735,#24736,#24737,
#24738,#24739,#24740,#24741,#24742,#24743,#24744,#24745,#24746,#24747,#24748,
#24749,#24750,#24751,#24752,#24753,#24754,#24755,#24756,#24757,#24758,#24759,
#24760,#24761,#24762,#24763,#24764,#24765,#24766,#24767,#24768,#24769,#24770,
#24771,#24772,#24773,#24774,#24775,#24776,#24777,#24778,#24779,#24780,#24781,
#24782,#24783,#24784,#24785,#24786,#24787,#24788,#24789,#24790,#24791,#24792,
#24793,#24794,#24795,#24796,#24797,#24798,#24799,#24800,#24801,#24802,#24803,
#24804,#24805,#24806,#24807,#24808,#24809,#24810,#24811,#24812,#24813,#24814,
#24815,#24816,#24817,#24818,#24819,#24820,#24821,#24822,#24823,#24824,#24825,
#24826),.UNSPECIFIED.,.F.,.F.,(4,3,3,3,3,3,3,3,3,3,3,3,3,3,3,3,3,3,3,3,
3,3,3,3,3,3,3,3,3,3,3,4),(-0.569248610399391,-0.543573485199943,-0.517270268565312,
-0.51040343212095,-0.504800294612885,-0.477738530287438,-0.455893930851042,
-0.447075593991324,-0.442407019766337,-0.414674597913133,-0.386513035378128,
-0.358572122738531,-0.344674525752965,-0.340104447556141,-0.311173623171527,
-0.302981734796268,-0.27516514613859,-0.246719659301531,-0.236777951845204,
-0.231757521912826,-0.227579246481702,-0.198579856955019,-0.169011286171866,
-0.139212421577441,-0.12303172519304,-0.118001035990282,-0.113392013031005,
-0.0828444532672019,-0.0522704025528943,-0.0223140889578805,-0.00976685050222891,
0.),.UNSPECIFIED.);
#2644=B_SPLINE_CURVE_WITH_KNOTS('',3,(#24827,#24828,#24829,#24830,#24831,
#24832,#24833,#24834,#24835,#24836,#24837,#24838,#24839,#24840,#24841,#24842,
#24843,#24844,#24845,#24846,#24847,#24848,#24849,#24850,#24851,#24852,#24853,
#24854,#24855,#24856,#24857,#24858,#24859,#24860,#24861,#24862,#24863,#24864,
#24865,#24866,#24867,#24868,#24869,#24870,#24871,#24872,#24873,#24874,#24875,
#24876,#24877,#24878,#24879,#24880,#24881,#24882,#24883,#24884,#24885,#24886,
#24887,#24888,#24889,#24890,#24891,#24892,#24893,#24894,#24895,#24896,#24897,
#24898,#24899,#24900,#24901,#24902,#24903,#24904,#24905,#24906,#24907,#24908,
#24909,#24910,#24911,#24912,#24913,#24914,#24915,#24916,#24917,#24918,#24919,
#24920),.UNSPECIFIED.,.F.,.F.,(4,3,3,3,3,3,3,3,3,3,3,3,3,3,3,3,3,3,3,3,
3,3,3,3,3,3,3,3,3,3,3,4),(-0.566847306048135,-0.536665109075417,-0.506058896071854,
-0.497416851909175,-0.49047965571675,-0.460332721088332,-0.437086686152057,
-0.424703698099728,-0.420462735133408,-0.39103784434011,-0.361869493654616,
-0.33354585979786,-0.318750505247928,-0.313020123387797,-0.308660184852524,
-0.280670747442105,-0.274364441598135,-0.245887082189052,-0.216156157664495,
-0.204673880739737,-0.200549631762214,-0.172713963704145,-0.144949220452659,
-0.117659624553142,-0.103957132233074,-0.0999252283847502,-0.0958138212739285,
-0.0691413054179344,-0.0429166386626297,-0.0174931714382136,-0.00803968599259392,
0.),.UNSPECIFIED.);
#2645=B_SPLINE_CURVE_WITH_KNOTS('',3,(#24922,#24923,#24924,#24925,#24926,
#24927,#24928,#24929,#24930,#24931,#24932),.UNSPECIFIED.,.F.,.F.,(4,1,1,
1,1,1,1,1,4),(15.7079632679489,15.8295388729956,16.8221763756675,17.8148138783395,
18.8074513810114,19.8000888836834,20.7927263863553,21.7853638890272,21.9911485751285),
 .UNSPECIFIED.);
#2646=B_SPLINE_CURVE_WITH_KNOTS('',3,(#24933,#24934,#24935,#24936,#24937,
#24938,#24939,#24940,#24941,#24942),.UNSPECIFIED.,.F.,.F.,(4,1,1,1,1,1,
1,4),(15.7079632679489,16.3836751323157,17.3763126349877,18.3689501376596,
19.3615876403316,20.3542251430035,21.3468626456754,21.9911485751285),
 .UNSPECIFIED.);
#2647=B_SPLINE_CURVE_WITH_KNOTS('',3,(#25191,#25192,#25193,#25194,#25195,
#25196,#25197,#25198,#25199,#25200,#25201,#25202,#25203,#25204,#25205,#25206,
#25207,#25208,#25209,#25210,#25211,#25212,#25213,#25214,#25215,#25216,#25217,
#25218,#25219,#25220,#25221,#25222,#25223,#25224,#25225,#25226,#25227,#25228,
#25229,#25230,#25231,#25232,#25233,#25234,#25235,#25236,#25237,#25238,#25239,
#25240,#25241,#25242,#25243,#25244,#25245,#25246,#25247,#25248,#25249,#25250,
#25251,#25252,#25253,#25254,#25255,#25256,#25257,#25258,#25259,#25260,#25261,
#25262,#25263,#25264,#25265,#25266,#25267,#25268,#25269,#25270,#25271,#25272,
#25273,#25274,#25275,#25276,#25277,#25278,#25279,#25280,#25281),
 .UNSPECIFIED.,.F.,.F.,(4,3,3,3,3,3,3,3,3,3,3,3,3,3,3,3,3,3,3,3,3,3,3,3,
3,3,3,3,3,3,4),(0.,0.0253641940060491,0.0513998528853357,0.0781558294588739,
0.0899177835126812,0.096625586076476,0.102679521314574,0.129980972716582,
0.157733265563707,0.18466186554119,0.195928352608436,0.202971020906728,
0.20709884412475,0.236273254799196,0.265447665473641,0.293340562931045,
0.302677593280724,0.308745430621993,0.314528754610798,0.34260673975117,
0.371727130037291,0.401175578671832,0.421351088041328,0.426753710423992,
0.456805222326454,0.481883932941516,0.490048800165398,0.498378785902177,
0.528887556975208,0.557120064786702,0.566847306048017),.UNSPECIFIED.);
#2648=B_SPLINE_CURVE_WITH_KNOTS('',3,(#25282,#25283,#25284,#25285,#25286,
#25287,#25288,#25289,#25290,#25291,#25292,#25293,#25294,#25295,#25296,#25297,
#25298,#25299,#25300,#25301,#25302,#25303,#25304,#25305,#25306),
 .UNSPECIFIED.,.F.,.F.,(4,3,3,3,3,3,3,3,4),(-10.1321597128207,-9.92637502671944,
-8.9337375240475,-7.94110002137556,-6.94846251870361,-5.95582501603167,
-4.96318751335972,-3.97055001068778,-3.84897440564114),.UNSPECIFIED.);
#2649=B_SPLINE_CURVE_WITH_KNOTS('',3,(#25555,#25556,#25557,#25558,#25559,
#25560,#25561,#25562,#25563,#25564,#25565,#25566,#25567,#25568,#25569,#25570,
#25571,#25572,#25573,#25574,#25575,#25576),.UNSPECIFIED.,.F.,.F.,(4,3,3,
3,3,3,3,4),(7.59274844815667,7.94110002137556,8.9337375240475,9.92637502671945,
10.9190125293914,11.9116500320633,12.9042875347353,13.8759337553363),
 .UNSPECIFIED.);
#2650=B_SPLINE_CURVE_WITH_KNOTS('',3,(#25577,#25578,#25579,#25580,#25581,
#25582,#25583,#25584,#25585,#25586,#25587,#25588,#25589,#25590,#25591,#25592,
#25593,#25594,#25595,#25596,#25597,#25598,#25599,#25600,#25601,#25602,#25603,
#25604,#25605,#25606,#25607,#25608,#25609,#25610,#25611,#25612,#25613,#25614,
#25615,#25616,#25617,#25618,#25619,#25620,#25621,#25622,#25623,#25624,#25625,
#25626,#25627,#25628,#25629,#25630,#25631,#25632,#25633,#25634,#25635,#25636,
#25637,#25638,#25639,#25640,#25641,#25642,#25643,#25644,#25645,#25646,#25647,
#25648,#25649,#25650,#25651,#25652,#25653,#25654,#25655,#25656,#25657,#25658,
#25659,#25660,#25661,#25662,#25663,#25664,#25665,#25666,#25667),
 .UNSPECIFIED.,.F.,.F.,(4,3,3,3,3,3,3,3,3,3,3,3,3,3,3,3,3,3,3,3,3,3,3,3,
3,3,3,3,3,3,4),(0.,0.0297251106276555,0.060108839848521,0.0893486196225938,
0.114933426924907,0.120627518834092,0.150386823450882,0.179982103762232,
0.20849334733195,0.220471792278386,0.22888232925389,0.234177127568146,0.264102102804625,
0.292006786872335,0.294027078041103,0.322973449904451,0.339362616990066,
0.343535824371297,0.371629348477673,0.399767742470069,0.427502094759513,
0.437970801715733,0.445641085172893,0.450375033464681,0.478076729683868,
0.498853001848258,0.508250421438057,0.513369584444669,0.539284522924145,
0.561181818341429,0.569248610399466),.UNSPECIFIED.);
#2651=B_SPLINE_CURVE_WITH_KNOTS('',3,(#25670,#25671,#25672,#25673,#25674,
#25675,#25676,#25677,#25678,#25679,#25680,#25681,#25682,#25683,#25684,#25685,
#25686,#25687,#25688,#25689,#25690,#25691,#25692,#25693,#25694,#25695,#25696,
#25697,#25698,#25699,#25700,#25701,#25702,#25703,#25704,#25705,#25706,#25707,
#25708,#25709,#25710,#25711,#25712,#25713,#25714,#25715,#25716,#25717,#25718,
#25719,#25720,#25721,#25722,#25723,#25724,#25725,#25726,#25727,#25728,#25729,
#25730,#25731,#25732,#25733,#25734,#25735,#25736,#25737,#25738,#25739,#25740,
#25741,#25742,#25743,#25744,#25745,#25746,#25747,#25748,#25749,#25750,#25751,
#25752,#25753,#25754,#25755,#25756,#25757,#25758,#25759,#25760,#25761,#25762,
#25763),.UNSPECIFIED.,.F.,.F.,(4,3,3,3,3,3,3,3,3,3,3,3,3,3,3,3,3,3,3,3,
3,3,3,3,3,3,3,3,3,3,3,4),(-0.569248610399449,-0.543573504102472,-0.517270303312747,
-0.510403518760422,-0.504800298462602,-0.477738547398343,-0.455893945823089,
-0.447075739640472,-0.442407159267797,-0.414674752545088,-0.38651318948242,
-0.358572268495855,-0.344674635070969,-0.340104625623979,-0.311173801204194,
-0.302981734796311,-0.275165133963676,-0.246719639454603,-0.236777889761598,
-0.231757378131509,-0.227578935732346,-0.198579529322731,-0.169010949155984,
-0.139212083849189,-0.12303142968082,-0.117999764723668,-0.113391857955279,
-0.0828442953573812,-0.0522702457649171,-0.022313932701136,-0.00976685050223398,
0.),.UNSPECIFIED.);
#2652=B_SPLINE_CURVE_WITH_KNOTS('',3,(#25764,#25765,#25766,#25767,#25768,
#25769,#25770,#25771,#25772,#25773,#25774,#25775,#25776,#25777,#25778,#25779,
#25780,#25781,#25782,#25783,#25784,#25785,#25786,#25787,#25788,#25789,#25790,
#25791,#25792,#25793,#25794,#25795,#25796,#25797,#25798,#25799,#25800,#25801,
#25802,#25803,#25804,#25805,#25806,#25807,#25808,#25809,#25810,#25811,#25812,
#25813,#25814,#25815,#25816,#25817,#25818,#25819,#25820,#25821,#25822,#25823,
#25824,#25825,#25826,#25827,#25828,#25829,#25830,#25831,#25832,#25833,#25834,
#25835,#25836,#25837,#25838,#25839,#25840,#25841,#25842,#25843,#25844,#25845,
#25846,#25847,#25848,#25849,#25850,#25851,#25852,#25853,#25854,#25855,#25856,
#25857),.UNSPECIFIED.,.F.,.F.,(4,3,3,3,3,3,3,3,3,3,3,3,3,3,3,3,3,3,3,3,
3,3,3,3,3,3,3,3,3,3,3,4),(-0.566847306048014,-0.536665117697509,-0.506058906999567,
-0.497416865326767,-0.490479658240677,-0.460332723347166,-0.437086688128531,
-0.424703702775148,-0.420462740381493,-0.391037848587686,-0.361869496840286,
-0.333545860028828,-0.318750505421142,-0.31302012577693,-0.308660186240849,
-0.28067074533307,-0.274364441598086,-0.245887081933056,-0.216156157440498,
-0.204673881207202,-0.200549631596289,-0.172713964128302,-0.144949220523049,
-0.117659621509534,-0.103957129569916,-0.0999252244321675,-0.095813819666998,
-0.0691413018378718,-0.0429166306421052,-0.0174931558038003,-0.00803968599259028,
0.),.UNSPECIFIED.);
#2653=B_SPLINE_CURVE_WITH_KNOTS('',3,(#25859,#25860,#25861,#25862,#25863,
#25864,#25865,#25866,#25867,#25868,#25869),.UNSPECIFIED.,.F.,.F.,(4,1,1,
1,1,1,1,1,4),(15.7079632679489,15.8295388729956,16.8221763756675,17.8148138783395,
18.8074513810114,19.8000888836834,20.7927263863553,21.7853638890272,21.9911485751285),
 .UNSPECIFIED.);
#2654=B_SPLINE_CURVE_WITH_KNOTS('',3,(#25870,#25871,#25872,#25873,#25874,
#25875,#25876,#25877,#25878,#25879),.UNSPECIFIED.,.F.,.F.,(4,1,1,1,1,1,
1,4),(15.7079632679489,16.3836751323157,17.3763126349877,18.3689501376596,
19.3615876403316,20.3542251430035,21.3468626456755,21.9911485751285),
 .UNSPECIFIED.);
#2655=B_SPLINE_CURVE_WITH_KNOTS('',3,(#26128,#26129,#26130,#26131,#26132,
#26133,#26134,#26135,#26136,#26137,#26138,#26139,#26140,#26141,#26142,#26143,
#26144,#26145,#26146,#26147,#26148,#26149,#26150,#26151,#26152,#26153,#26154,
#26155,#26156,#26157,#26158,#26159,#26160,#26161,#26162,#26163,#26164,#26165,
#26166,#26167,#26168,#26169,#26170,#26171,#26172,#26173,#26174,#26175,#26176,
#26177,#26178,#26179,#26180,#26181,#26182,#26183,#26184,#26185,#26186,#26187,
#26188,#26189,#26190,#26191,#26192,#26193,#26194,#26195,#26196,#26197,#26198,
#26199,#26200,#26201,#26202,#26203,#26204,#26205,#26206,#26207,#26208,#26209,
#26210,#26211,#26212,#26213,#26214,#26215,#26216,#26217,#26218),
 .UNSPECIFIED.,.F.,.F.,(4,3,3,3,3,3,3,3,3,3,3,3,3,3,3,3,3,3,3,3,3,3,3,3,
3,3,3,3,3,3,4),(0.,0.0253641802043484,0.0513998265906757,0.0781558064510469,
0.0899177781668214,0.0966255853603576,0.102679521324914,0.129980963033573,
0.157733251052733,0.184661854657961,0.195928350249662,0.202971019794835,
0.207098842071563,0.236273253772604,0.265447665473645,0.293340569486741,
0.302677606942409,0.308745486155756,0.314528754108539,0.342606748516018,
0.371727143138761,0.401175592930875,0.421351120763801,0.426753697797161,
0.45680521160119,0.481883924897573,0.49004878710534,0.498378789150779,0.528887560035012,
0.557120064786721,0.566847306048034),.UNSPECIFIED.);
#2656=B_SPLINE_CURVE_WITH_KNOTS('',3,(#26219,#26220,#26221,#26222,#26223,
#26224,#26225,#26226,#26227,#26228,#26229,#26230,#26231,#26232,#26233,#26234,
#26235,#26236,#26237,#26238,#26239,#26240,#26241,#26242,#26243),
 .UNSPECIFIED.,.F.,.F.,(4,3,3,3,3,3,3,3,4),(-10.1321597128207,-9.92637502671944,
-8.9337375240475,-7.94110002137556,-6.94846251870361,-5.95582501603167,
-4.96318751335972,-3.97055001068778,-3.84897440564113),.UNSPECIFIED.);
#2657=B_SPLINE_CURVE_WITH_KNOTS('',3,(#26492,#26493,#26494,#26495,#26496,
#26497,#26498,#26499,#26500,#26501,#26502,#26503,#26504,#26505,#26506,#26507,
#26508,#26509,#26510,#26511,#26512,#26513),.UNSPECIFIED.,.F.,.F.,(4,3,3,
3,3,3,3,4),(7.59274844815666,7.94110002137556,8.9337375240475,9.92637502671945,
10.9190125293914,11.9116500320633,12.9042875347353,13.8759337553362),
 .UNSPECIFIED.);
#2658=B_SPLINE_CURVE_WITH_KNOTS('',3,(#26514,#26515,#26516,#26517,#26518,
#26519,#26520,#26521,#26522,#26523,#26524,#26525,#26526,#26527,#26528,#26529,
#26530,#26531,#26532,#26533,#26534,#26535,#26536,#26537,#26538,#26539,#26540,
#26541,#26542,#26543,#26544,#26545,#26546,#26547,#26548,#26549,#26550,#26551,
#26552,#26553,#26554,#26555,#26556,#26557,#26558,#26559,#26560,#26561,#26562,
#26563,#26564,#26565,#26566,#26567,#26568,#26569,#26570,#26571,#26572,#26573,
#26574,#26575,#26576,#26577,#26578,#26579,#26580,#26581,#26582,#26583,#26584,
#26585,#26586,#26587,#26588,#26589,#26590,#26591,#26592,#26593,#26594,#26595,
#26596,#26597,#26598,#26599,#26600,#26601,#26602,#26603,#26604),
 .UNSPECIFIED.,.F.,.F.,(4,3,3,3,3,3,3,3,3,3,3,3,3,3,3,3,3,3,3,3,3,3,3,3,
3,3,3,3,3,3,4),(0.,0.0297250940603701,0.0601088150228865,0.0893485979001609,
0.114933407917776,0.120627517502826,0.150386821838171,0.179982106532903,
0.208493349409947,0.220471797231655,0.228882342926144,0.234177131447686,
0.264102104744384,0.292006792915222,0.294027078041082,0.322973449076703,
0.339362619054412,0.34353582684914,0.371629350432206,0.399767744193081,
0.427502099759356,0.437970813749853,0.445641127145106,0.45037504344892,
0.478076737172018,0.498853007464342,0.508250442098983,0.513369590083379,
0.539284536863559,0.561181818341313,0.56924861039935),.UNSPECIFIED.);
#2659=B_SPLINE_CURVE_WITH_KNOTS('',3,(#26607,#26608,#26609,#26610,#26611,
#26612,#26613,#26614,#26615,#26616,#26617,#26618,#26619,#26620,#26621,#26622,
#26623,#26624,#26625,#26626,#26627,#26628,#26629,#26630,#26631,#26632,#26633,
#26634,#26635,#26636,#26637,#26638,#26639,#26640,#26641,#26642,#26643,#26644,
#26645,#26646,#26647,#26648,#26649,#26650,#26651,#26652,#26653,#26654,#26655,
#26656,#26657,#26658,#26659,#26660,#26661,#26662,#26663,#26664,#26665,#26666,
#26667,#26668,#26669,#26670,#26671,#26672,#26673,#26674,#26675,#26676,#26677,
#26678,#26679,#26680,#26681,#26682,#26683,#26684,#26685,#26686,#26687,#26688,
#26689,#26690,#26691,#26692,#26693,#26694,#26695,#26696,#26697,#26698,#26699,
#26700),.UNSPECIFIED.,.F.,.F.,(4,3,3,3,3,3,3,3,3,3,3,3,3,3,3,3,3,3,3,3,
3,3,3,3,3,3,3,3,3,3,3,4),(-0.569248610399476,-0.543573485205502,-0.517270268573132,
-0.510403432146651,-0.50480029464855,-0.477738530324984,-0.4558939308839,
-0.447075594297702,-0.442407020006122,-0.414674598149304,-0.386513035614215,
-0.358572122969062,-0.344674525925876,-0.340104447830039,-0.3111736234517,
-0.302981734796315,-0.275165146138309,-0.246719659299767,-0.236777951841385,
-0.231757521910833,-0.227579246473126,-0.198579856945078,-0.169011286162167,
-0.139212421569045,-0.123031725185693,-0.118001036018665,-0.113392013034907,
-0.0828444532722089,-0.0522704025570408,-0.0223140889611495,-0.0097668505022249,
0.),.UNSPECIFIED.);
#2660=B_SPLINE_CURVE_WITH_KNOTS('',3,(#26701,#26702,#26703,#26704,#26705,
#26706,#26707,#26708,#26709,#26710,#26711,#26712,#26713,#26714,#26715,#26716,
#26717,#26718,#26719,#26720,#26721,#26722,#26723,#26724,#26725,#26726,#26727,
#26728,#26729,#26730,#26731,#26732,#26733,#26734,#26735,#26736,#26737,#26738,
#26739,#26740,#26741,#26742,#26743,#26744,#26745,#26746,#26747,#26748,#26749,
#26750,#26751,#26752,#26753,#26754,#26755,#26756,#26757,#26758,#26759,#26760,
#26761,#26762,#26763,#26764,#26765,#26766,#26767,#26768,#26769,#26770,#26771,
#26772,#26773,#26774,#26775,#26776,#26777,#26778,#26779,#26780,#26781,#26782,
#26783,#26784,#26785,#26786,#26787,#26788,#26789,#26790,#26791,#26792,#26793,
#26794),.UNSPECIFIED.,.F.,.F.,(4,3,3,3,3,3,3,3,3,3,3,3,3,3,3,3,3,3,3,3,
3,3,3,3,3,3,3,3,3,3,3,4),(-0.5668473060481,-0.536665109079502,-0.506058896073369,
-0.497416851912877,-0.490479655811324,-0.460332721180406,-0.43708668623262,
-0.424703698246803,-0.420462735243598,-0.391037844452743,-0.361869493739087,
-0.333545859882985,-0.318750505311769,-0.313020123569819,-0.308660184935363,
-0.280670747518966,-0.27436444159812,-0.245887082194013,-0.216156157668836,
-0.20467388073518,-0.200549631773281,-0.172713963716999,-0.144949220465045,
-0.117659624577274,-0.103957132254189,-0.0999252285358155,-0.0958138213027416,
-0.0691413054476691,-0.04291663869175,-0.017493171464394,-0.00803968599259441,
0.),.UNSPECIFIED.);
#2661=B_SPLINE_CURVE_WITH_KNOTS('',3,(#26796,#26797,#26798,#26799,#26800,
#26801,#26802,#26803,#26804,#26805,#26806),.UNSPECIFIED.,.F.,.F.,(4,1,1,
1,1,1,1,1,4),(15.7079632679489,15.8295388729956,16.8221763756675,17.8148138783395,
18.8074513810114,19.8000888836834,20.7927263863553,21.7853638890272,21.9911485751285),
 .UNSPECIFIED.);
#2662=B_SPLINE_CURVE_WITH_KNOTS('',3,(#26807,#26808,#26809,#26810,#26811,
#26812,#26813,#26814,#26815,#26816),.UNSPECIFIED.,.F.,.F.,(4,1,1,1,1,1,
1,4),(15.7079632679489,16.3836751323157,17.3763126349877,18.3689501376596,
19.3615876403316,20.3542251430035,21.3468626456754,21.9911485751285),
 .UNSPECIFIED.);
#2663=B_SPLINE_CURVE_WITH_KNOTS('',3,(#27065,#27066,#27067,#27068,#27069,
#27070,#27071,#27072,#27073,#27074,#27075,#27076,#27077,#27078,#27079,#27080,
#27081,#27082,#27083,#27084,#27085,#27086,#27087,#27088,#27089,#27090,#27091,
#27092,#27093,#27094,#27095,#27096,#27097,#27098,#27099,#27100,#27101,#27102,
#27103,#27104,#27105,#27106,#27107,#27108,#27109,#27110,#27111,#27112,#27113,
#27114,#27115,#27116,#27117,#27118,#27119,#27120,#27121,#27122,#27123,#27124,
#27125,#27126,#27127,#27128,#27129,#27130,#27131,#27132,#27133,#27134,#27135,
#27136,#27137,#27138,#27139,#27140,#27141,#27142,#27143,#27144,#27145,#27146,
#27147,#27148,#27149,#27150,#27151,#27152,#27153,#27154,#27155),
 .UNSPECIFIED.,.F.,.F.,(4,3,3,3,3,3,3,3,3,3,3,3,3,3,3,3,3,3,3,3,3,3,3,3,
3,3,3,3,3,3,4),(0.,0.0253641940059154,0.0513998528845501,0.0781558294581879,
0.0899177835124791,0.0966255860763879,0.102679521323728,0.129980972726384,
0.157733265573268,0.184661865548364,0.195928352610419,0.202971020904623,
0.207098844127634,0.236273254800643,0.265447665473653,0.293340562930928,
0.302677593280407,0.30874543062048,0.314528754623958,0.342606739764072,
0.371727130050435,0.401175578685423,0.421351088070314,0.426753710426087,
0.45680522232921,0.4818839329436,0.490048800169418,0.498378785911953,0.52888755698416,
0.557120064786771,0.566847306048087),.UNSPECIFIED.);
#2664=B_SPLINE_CURVE_WITH_KNOTS('',3,(#27156,#27157,#27158,#27159,#27160,
#27161,#27162,#27163,#27164,#27165,#27166,#27167,#27168,#27169,#27170,#27171,
#27172,#27173,#27174,#27175,#27176,#27177,#27178,#27179,#27180),
 .UNSPECIFIED.,.F.,.F.,(4,3,3,3,3,3,3,3,4),(-10.1321597128207,-9.92637502671944,
-8.9337375240475,-7.94110002137556,-6.94846251870361,-5.95582501603167,
-4.96318751335973,-3.97055001068778,-3.84897440564114),.UNSPECIFIED.);
#2665=B_SPLINE_CURVE_WITH_KNOTS('',3,(#27429,#27430,#27431,#27432,#27433,
#27434,#27435,#27436,#27437,#27438,#27439,#27440,#27441,#27442,#27443,#27444,
#27445,#27446,#27447,#27448,#27449,#27450),.UNSPECIFIED.,.F.,.F.,(4,3,3,
3,3,3,3,4),(7.59274844815666,7.94110002137556,8.9337375240475,9.92637502671945,
10.9190125293914,11.9116500320633,12.9042875347353,13.8759337553362),
 .UNSPECIFIED.);
#2666=B_SPLINE_CURVE_WITH_KNOTS('',3,(#27451,#27452,#27453,#27454,#27455,
#27456,#27457,#27458,#27459,#27460,#27461,#27462,#27463,#27464,#27465,#27466,
#27467,#27468,#27469,#27470,#27471,#27472,#27473,#27474,#27475,#27476,#27477,
#27478,#27479,#27480,#27481,#27482,#27483,#27484,#27485,#27486,#27487,#27488,
#27489,#27490,#27491,#27492,#27493,#27494,#27495,#27496,#27497,#27498,#27499,
#27500,#27501,#27502,#27503,#27504,#27505,#27506,#27507,#27508,#27509,#27510,
#27511,#27512,#27513,#27514,#27515,#27516,#27517,#27518,#27519,#27520,#27521,
#27522,#27523,#27524,#27525,#27526,#27527,#27528,#27529,#27530,#27531,#27532,
#27533,#27534,#27535,#27536,#27537,#27538,#27539,#27540,#27541),
 .UNSPECIFIED.,.F.,.F.,(4,3,3,3,3,3,3,3,3,3,3,3,3,3,3,3,3,3,3,3,3,3,3,3,
3,3,3,3,3,3,4),(0.,0.0297251106280497,0.0601088398490155,0.0893486196230253,
0.114933426925284,0.120627518834333,0.150386823451848,0.179982103763167,
0.208493347332649,0.220471792279509,0.228882329257328,0.234177127564844,
0.264102102802969,0.292006786870997,0.294027078041094,0.322973449904779,
0.339362616990787,0.343535824361368,0.371629348467577,0.399767742460233,
0.427502094749591,0.437970801695254,0.445641085107272,0.45037503345148,
0.47807672967396,0.498853001840821,0.508250421414146,0.513369584440127,
0.539284522919995,0.561181818341402,0.569248610399439),.UNSPECIFIED.);
#2667=B_SPLINE_CURVE_WITH_KNOTS('',3,(#27544,#27545,#27546,#27547,#27548,
#27549,#27550,#27551,#27552,#27553,#27554,#27555,#27556,#27557,#27558,#27559,
#27560,#27561,#27562,#27563,#27564,#27565,#27566,#27567,#27568,#27569,#27570,
#27571,#27572,#27573,#27574,#27575,#27576,#27577,#27578,#27579,#27580,#27581,
#27582,#27583,#27584,#27585,#27586,#27587,#27588,#27589,#27590,#27591,#27592,
#27593,#27594,#27595,#27596,#27597,#27598,#27599,#27600,#27601,#27602,#27603,
#27604,#27605,#27606,#27607,#27608,#27609,#27610,#27611,#27612,#27613,#27614,
#27615,#27616,#27617,#27618,#27619,#27620,#27621,#27622,#27623,#27624,#27625,
#27626,#27627,#27628,#27629,#27630,#27631,#27632,#27633,#27634,#27635,#27636,
#27637),.UNSPECIFIED.,.F.,.F.,(4,3,3,3,3,3,3,3,3,3,3,3,3,3,3,3,3,3,3,3,
3,3,3,3,3,3,3,3,3,3,3,4),(-0.569248610399503,-0.543573536725572,-0.517270363300643,
-0.510403668322967,-0.504800305048166,-0.47773857688201,-0.455893971621299,
-0.447075990604545,-0.442407399438625,-0.414675018820766,-0.386513454853249,
-0.35857251946668,-0.34467482329909,-0.340104931946522,-0.311174107463772,
-0.302981734796321,-0.275165112945586,-0.246719605186861,-0.236777782574912,
-0.231757129804548,-0.227578398489937,-0.198578962914807,-0.169010366535306,
-0.139211499993959,-0.123030918807493,-0.117997565283917,-0.113391588480745,
-0.0828440209838422,-0.0522699733385328,-0.0223136612161147,-0.00976685050222925,
0.),.UNSPECIFIED.);
#2668=B_SPLINE_CURVE_WITH_KNOTS('',3,(#27638,#27639,#27640,#27641,#27642,
#27643,#27644,#27645,#27646,#27647,#27648,#27649,#27650,#27651,#27652,#27653,
#27654,#27655,#27656,#27657,#27658,#27659,#27660,#27661,#27662,#27663,#27664,
#27665,#27666,#27667,#27668,#27669,#27670,#27671,#27672,#27673,#27674,#27675,
#27676,#27677,#27678,#27679,#27680,#27681,#27682,#27683,#27684,#27685,#27686,
#27687,#27688,#27689,#27690,#27691,#27692,#27693,#27694,#27695,#27696,#27697,
#27698,#27699,#27700,#27701,#27702,#27703,#27704,#27705,#27706,#27707,#27708,
#27709,#27710,#27711,#27712,#27713,#27714,#27715,#27716,#27717,#27718,#27719,
#27720,#27721,#27722,#27723,#27724,#27725,#27726,#27727,#27728,#27729,#27730,
#27731),.UNSPECIFIED.,.F.,.F.,(4,3,3,3,3,3,3,3,3,3,3,3,3,3,3,3,3,3,3,3,
3,3,3,3,3,3,3,3,3,3,3,4),(-0.566847306048007,-0.536665099326187,-0.50605888371953,
-0.497416836745447,-0.490479652851239,-0.460332718522974,-0.437086683907363,
-0.424703692798494,-0.420462729215447,-0.391037839556167,-0.361869490066648,
-0.333545859553922,-0.318750505064964,-0.31302012072499,-0.308660183331501,
-0.280670749875022,-0.27436444159809,-0.245887082485289,-0.216156157923702,
-0.204673880207543,-0.200549631930185,-0.172713963206743,-0.144949220356295,
-0.117659627980649,-0.103957135232142,-0.099925232967256,-0.0958138231131305,
-0.069141309492666,-0.042916647764108,-0.017493189155658,-0.00803968599259752,
0.),.UNSPECIFIED.);
#2669=B_SPLINE_CURVE_WITH_KNOTS('',3,(#27733,#27734,#27735,#27736,#27737,
#27738,#27739,#27740,#27741,#27742,#27743),.UNSPECIFIED.,.F.,.F.,(4,1,1,
1,1,1,1,1,4),(15.7079632679489,15.8295388729956,16.8221763756675,17.8148138783395,
18.8074513810114,19.8000888836834,20.7927263863553,21.7853638890272,21.9911485751285),
 .UNSPECIFIED.);
#2670=B_SPLINE_CURVE_WITH_KNOTS('',3,(#27744,#27745,#27746,#27747,#27748,
#27749,#27750,#27751,#27752,#27753),.UNSPECIFIED.,.F.,.F.,(4,1,1,1,1,1,
1,4),(15.7079632679489,16.3836751323157,17.3763126349877,18.3689501376596,
19.3615876403316,20.3542251430035,21.3468626456754,21.9911485751285),
 .UNSPECIFIED.);
#2671=B_SPLINE_CURVE_WITH_KNOTS('',3,(#28002,#28003,#28004,#28005,#28006,
#28007,#28008,#28009,#28010,#28011,#28012,#28013,#28014,#28015,#28016,#28017,
#28018,#28019,#28020,#28021,#28022,#28023,#28024,#28025,#28026,#28027,#28028,
#28029,#28030,#28031,#28032,#28033,#28034,#28035,#28036,#28037,#28038,#28039,
#28040,#28041,#28042,#28043,#28044,#28045,#28046,#28047,#28048,#28049,#28050,
#28051,#28052,#28053,#28054,#28055,#28056,#28057,#28058,#28059,#28060,#28061,
#28062,#28063,#28064,#28065,#28066,#28067,#28068,#28069,#28070,#28071,#28072,
#28073,#28074,#28075,#28076,#28077,#28078,#28079,#28080,#28081,#28082,#28083,
#28084,#28085,#28086,#28087,#28088,#28089,#28090,#28091,#28092),
 .UNSPECIFIED.,.F.,.F.,(4,3,3,3,3,3,3,3,3,3,3,3,3,3,3,3,3,3,3,3,3,3,3,3,
3,3,3,3,3,3,4),(0.,0.0253642096190117,0.0513998826294253,0.078155855484953,
0.0899177895597073,0.0966255868864595,0.102679521322493,0.129980983690104,
0.157733281997098,0.184661877866235,0.195928355280655,0.20297102215946,
0.207098846520249,0.236273255996948,0.265447665473647,0.293340555515042,
0.302677577825464,0.308745367797819,0.314528755194195,0.342606729849992,
0.37172711523001,0.401175562555647,0.421351051054358,0.426753724713226,
0.45680523446668,0.481883942046697,0.490048814948903,0.498378782214203,
0.528887553499741,0.557120064786748,0.566847306048067),.UNSPECIFIED.);
#2672=B_SPLINE_CURVE_WITH_KNOTS('',3,(#28093,#28094,#28095,#28096,#28097,
#28098,#28099,#28100,#28101,#28102,#28103,#28104,#28105,#28106,#28107,#28108,
#28109,#28110,#28111,#28112,#28113,#28114,#28115,#28116,#28117),
 .UNSPECIFIED.,.F.,.F.,(4,3,3,3,3,3,3,3,4),(-10.1321597128207,-9.92637502671945,
-8.93373752404751,-7.94110002137556,-6.94846251870361,-5.95582501603167,
-4.96318751335972,-3.97055001068778,-3.84897440564114),.UNSPECIFIED.);
#2673=B_SPLINE_CURVE_WITH_KNOTS('',3,(#28366,#28367,#28368,#28369,#28370,
#28371,#28372,#28373,#28374,#28375,#28376,#28377,#28378,#28379,#28380,#28381,
#28382,#28383,#28384,#28385,#28386,#28387),.UNSPECIFIED.,.F.,.F.,(4,3,3,
3,3,3,3,4),(7.59274844815666,7.94110002137556,8.93373752404751,9.92637502671945,
10.9190125293914,11.9116500320633,12.9042875347353,13.8759337553362),
 .UNSPECIFIED.);
#2674=B_SPLINE_CURVE_WITH_KNOTS('',3,(#28388,#28389,#28390,#28391,#28392,
#28393,#28394,#28395,#28396,#28397,#28398,#28399,#28400,#28401,#28402,#28403,
#28404,#28405,#28406,#28407,#28408,#28409,#28410,#28411,#28412,#28413,#28414,
#28415,#28416,#28417,#28418,#28419,#28420,#28421,#28422,#28423,#28424,#28425,
#28426,#28427,#28428,#28429,#28430,#28431,#28432,#28433,#28434,#28435,#28436,
#28437,#28438,#28439,#28440,#28441,#28442,#28443,#28444,#28445,#28446,#28447,
#28448,#28449,#28450,#28451,#28452,#28453,#28454,#28455,#28456,#28457,#28458,
#28459,#28460,#28461,#28462,#28463,#28464,#28465,#28466,#28467,#28468,#28469,
#28470,#28471,#28472,#28473,#28474,#28475,#28476,#28477,#28478),
 .UNSPECIFIED.,.F.,.F.,(4,3,3,3,3,3,3,3,3,3,3,3,3,3,3,3,3,3,3,3,3,3,3,3,
3,3,3,3,3,3,4),(0.,0.029725065450369,0.060108772149361,0.0893485603858319,
0.114933375092744,0.120627515201239,0.150386819046978,0.179982111308832,
0.208493352991906,0.220471805772867,0.228882366497282,0.234177138099837,
0.264102108070482,0.292006803324548,0.294027078041128,0.322973447643439,
0.339362622606945,0.343535831117231,0.371629353795543,0.399767747153013,
0.427502108367365,0.437970834477791,0.445641199459811,0.450375060656323,
0.478076750077611,0.498853017143577,0.50825047771638,0.513369599808131,
0.539284560911353,0.561181818341475,0.569248610399517),.UNSPECIFIED.);
#2675=B_SPLINE_CURVE_WITH_KNOTS('',3,(#28481,#28482,#28483,#28484,#28485,
#28486,#28487,#28488,#28489,#28490,#28491,#28492,#28493,#28494,#28495,#28496,
#28497,#28498,#28499,#28500,#28501,#28502,#28503,#28504,#28505,#28506,#28507,
#28508,#28509,#28510,#28511,#28512,#28513,#28514,#28515,#28516,#28517,#28518,
#28519,#28520,#28521,#28522,#28523,#28524,#28525,#28526,#28527,#28528,#28529,
#28530,#28531,#28532,#28533,#28534,#28535,#28536,#28537,#28538,#28539,#28540,
#28541,#28542,#28543,#28544,#28545,#28546,#28547,#28548,#28549,#28550,#28551,
#28552,#28553,#28554,#28555,#28556,#28557,#28558,#28559,#28560,#28561,#28562,
#28563,#28564,#28565,#28566,#28567,#28568,#28569,#28570,#28571,#28572,#28573,
#28574),.UNSPECIFIED.,.F.,.F.,(4,3,3,3,3,3,3,3,3,3,3,3,3,3,3,3,3,3,3,3,
3,3,3,3,3,3,3,3,3,3,3,4),(-0.569248610399503,-0.543573521277575,-0.51727033489437,
-0.510403597501007,-0.504800301984927,-0.477738562977673,-0.455893959455004,
-0.447075872238583,-0.442407286260358,-0.414674893289812,-0.386513329748341,
-0.358572401173164,-0.344674734578953,-0.340104787662881,-0.311173963212057,
-0.302981734796321,-0.275165122896258,-0.246719621408367,-0.236777833316757,
-0.231757247392069,-0.22757865289815,-0.198579231130546,-0.169010642427486,
-0.139211776471259,-0.12303116072513,-0.117998607181915,-0.113391716319945,
-0.0828441511418465,-0.0522701025755355,-0.0223137900019766,-0.00976685050222925,
0.),.UNSPECIFIED.);
#2676=B_SPLINE_CURVE_WITH_KNOTS('',3,(#28575,#28576,#28577,#28578,#28579,
#28580,#28581,#28582,#28583,#28584,#28585,#28586,#28587,#28588,#28589,#28590,
#28591,#28592,#28593,#28594,#28595,#28596,#28597,#28598,#28599,#28600,#28601,
#28602,#28603,#28604,#28605,#28606,#28607,#28608,#28609,#28610,#28611,#28612,
#28613,#28614,#28615,#28616,#28617,#28618,#28619,#28620,#28621,#28622,#28623,
#28624,#28625,#28626,#28627,#28628,#28629,#28630,#28631,#28632,#28633,#28634,
#28635,#28636,#28637,#28638,#28639,#28640,#28641,#28642,#28643,#28644,#28645,
#28646,#28647,#28648,#28649,#28650,#28651,#28652,#28653,#28654,#28655,#28656,
#28657,#28658,#28659,#28660,#28661,#28662,#28663,#28664,#28665,#28666,#28667,
#28668),.UNSPECIFIED.,.F.,.F.,(4,3,3,3,3,3,3,3,3,3,3,3,3,3,3,3,3,3,3,3,
3,3,3,3,3,3,3,3,3,3,3,4),(-0.566847306048007,-0.536665088443819,-0.506058869926945,
-0.497416819812331,-0.490479649708581,-0.4603327157151,-0.437086681450474,
-0.424703686967728,-0.420462722527238,-0.391037834128131,-0.36186948599562,
-0.333545859211528,-0.318750504808168,-0.313020117605598,-0.308660181455267,
-0.280670752414333,-0.27436444159809,-0.24588708281337,-0.216156158210774,
-0.204673879612822,-0.200549632067082,-0.172713962600946,-0.144949220202067,
-0.117659631764077,-0.103957138542642,-0.0999252379790372,-0.0958138251467766,
-0.0691413140230926,-0.0429166579078794,-0.0174932089177672,-0.00803968599259752,
0.),.UNSPECIFIED.);
#2677=B_SPLINE_CURVE_WITH_KNOTS('',3,(#28670,#28671,#28672,#28673,#28674,
#28675,#28676,#28677,#28678,#28679,#28680),.UNSPECIFIED.,.F.,.F.,(4,1,1,
1,1,1,1,1,4),(15.7079632679489,15.8295388729956,16.8221763756675,17.8148138783395,
18.8074513810114,19.8000888836834,20.7927263863553,21.7853638890272,21.9911485751285),
 .UNSPECIFIED.);
#2678=B_SPLINE_CURVE_WITH_KNOTS('',3,(#28681,#28682,#28683,#28684,#28685,
#28686,#28687,#28688,#28689,#28690),.UNSPECIFIED.,.F.,.F.,(4,1,1,1,1,1,
1,4),(15.7079632679489,16.3836751323157,17.3763126349877,18.3689501376596,
19.3615876403316,20.3542251430035,21.3468626456754,21.9911485751285),
 .UNSPECIFIED.);
#2679=B_SPLINE_CURVE_WITH_KNOTS('',3,(#28939,#28940,#28941,#28942,#28943,
#28944,#28945,#28946,#28947,#28948,#28949,#28950,#28951,#28952,#28953,#28954,
#28955,#28956,#28957,#28958,#28959,#28960,#28961,#28962,#28963,#28964,#28965,
#28966,#28967,#28968,#28969,#28970,#28971,#28972,#28973,#28974,#28975,#28976,
#28977,#28978,#28979,#28980,#28981,#28982,#28983,#28984,#28985,#28986,#28987,
#28988,#28989,#28990,#28991,#28992,#28993,#28994,#28995,#28996,#28997,#28998,
#28999,#29000,#29001,#29002,#29003,#29004,#29005,#29006,#29007,#29008,#29009,
#29010,#29011,#29012,#29013,#29014,#29015,#29016,#29017,#29018,#29019,#29020,
#29021,#29022,#29023,#29024,#29025,#29026,#29027,#29028,#29029),
 .UNSPECIFIED.,.F.,.F.,(4,3,3,3,3,3,3,3,3,3,3,3,3,3,3,3,3,3,3,3,3,3,3,3,
3,3,3,3,3,3,4),(0.,0.0253642270426691,0.0513999158235613,0.0781558845298221,
0.0899177963077374,0.0966255877901253,0.102679521320011,0.12998099592429,
0.157733300324819,0.184661891612026,0.195928358260196,0.202971023559155,
0.207098849097602,0.236273257285624,0.265447665473647,0.293340547237358,
0.302677560574417,0.30874529767522,0.314528755850086,0.342606718802077,
0.371727098706227,0.401175544570548,0.421351009778467,0.426753740647144,
0.456805248003638,0.481883952199416,0.490048831431489,0.498378778130755,
0.528887549653182,0.557120064786748,0.566847306048067),.UNSPECIFIED.);
#2680=B_SPLINE_CURVE_WITH_KNOTS('',3,(#29030,#29031,#29032,#29033,#29034,
#29035,#29036,#29037,#29038,#29039,#29040,#29041,#29042,#29043,#29044,#29045,
#29046,#29047,#29048,#29049,#29050,#29051,#29052,#29053,#29054),
 .UNSPECIFIED.,.F.,.F.,(4,3,3,3,3,3,3,3,4),(-10.1321597128207,-9.92637502671945,
-8.93373752404751,-7.94110002137556,-6.94846251870361,-5.95582501603167,
-4.96318751335972,-3.97055001068778,-3.84897440564114),.UNSPECIFIED.);
#2681=B_SPLINE_CURVE_WITH_KNOTS('',3,(#29303,#29304,#29305,#29306,#29307,
#29308,#29309,#29310,#29311,#29312,#29313,#29314,#29315,#29316,#29317,#29318,
#29319,#29320,#29321,#29322,#29323,#29324),.UNSPECIFIED.,.F.,.F.,(4,3,3,
3,3,3,3,4),(7.59274844815666,7.94110002137556,8.93373752404751,9.92637502671945,
10.9190125293914,11.9116500320633,12.9042875347353,13.8759337553362),
 .UNSPECIFIED.);
#2682=B_SPLINE_CURVE_WITH_KNOTS('',3,(#29325,#29326,#29327,#29328,#29329,
#29330,#29331,#29332,#29333,#29334,#29335,#29336,#29337,#29338,#29339,#29340,
#29341,#29342,#29343,#29344,#29345,#29346,#29347,#29348,#29349,#29350,#29351,
#29352,#29353,#29354,#29355,#29356,#29357,#29358,#29359,#29360,#29361,#29362,
#29363,#29364,#29365,#29366,#29367,#29368,#29369,#29370,#29371,#29372,#29373,
#29374,#29375,#29376,#29377,#29378,#29379,#29380,#29381,#29382,#29383,#29384,
#29385,#29386,#29387,#29388,#29389,#29390,#29391,#29392,#29393,#29394,#29395,
#29396,#29397,#29398,#29399,#29400,#29401,#29402,#29403,#29404,#29405,#29406,
#29407,#29408,#29409,#29410,#29411,#29412,#29413,#29414,#29415),
 .UNSPECIFIED.,.F.,.F.,(4,3,3,3,3,3,3,3,3,3,3,3,3,3,3,3,3,3,3,3,3,3,3,3,
3,3,3,3,3,3,4),(0.,0.0297250789967798,0.0601087924493119,0.0893485781482889,
0.114933390634894,0.120627516294312,0.150386820372194,0.179982109051852,
0.208493351299171,0.220471801734144,0.228882355353164,0.234177134961176,
0.264102106501152,0.292006798402076,0.294027078041128,0.32297344832203,
0.339362620925334,0.343535829103202,0.371629352210162,0.399767745759375,
0.427502104300572,0.437970824682022,0.445641165284965,0.450375052521985,
0.478076743976858,0.498853012568012,0.508250460876233,0.513369595208601,
0.539284549532082,0.561181818341475,0.569248610399517),.UNSPECIFIED.);
#2683=B_SPLINE_CURVE_WITH_KNOTS('',3,(#29418,#29419,#29420,#29421,#29422,
#29423,#29424,#29425,#29426,#29427,#29428,#29429,#29430,#29431,#29432,#29433,
#29434,#29435,#29436,#29437,#29438,#29439,#29440,#29441,#29442,#29443,#29444,
#29445,#29446,#29447,#29448,#29449,#29450,#29451,#29452,#29453,#29454,#29455,
#29456,#29457,#29458,#29459,#29460,#29461,#29462,#29463,#29464,#29465,#29466,
#29467,#29468,#29469,#29470,#29471,#29472,#29473,#29474,#29475,#29476,#29477,
#29478,#29479,#29480,#29481,#29482,#29483,#29484,#29485,#29486,#29487,#29488,
#29489,#29490,#29491,#29492,#29493,#29494,#29495,#29496,#29497,#29498,#29499,
#29500,#29501,#29502,#29503,#29504,#29505,#29506,#29507,#29508,#29509,#29510,
#29511),.UNSPECIFIED.,.F.,.F.,(4,3,3,3,3,3,3,3,3,3,3,3,3,3,3,3,3,3,3,3,
3,3,3,3,3,3,3,3,3,3,3,4),(-0.569248610399476,-0.543573504098887,-0.517270303307527,
-0.510403518746194,-0.504800298512377,-0.477738547447543,-0.45589394586614,
-0.447075740045164,-0.442407159583378,-0.414674752859423,-0.386513189796536,
-0.358572268806566,-0.344674635304004,-0.340104625965199,-0.3111738015465,
-0.302981734796315,-0.275165133962666,-0.246719639451408,-0.236777889756063,
-0.23175737813359,-0.227578935587986,-0.19857952917295,-0.16901094900184,
-0.139212083695293,-0.12303142954616,-0.117999764265674,-0.113391857900451,
-0.0828442953049202,-0.0522702457140997,-0.0223139326486197,-0.0097668505022249,
0.),.UNSPECIFIED.);
#2684=B_SPLINE_CURVE_WITH_KNOTS('',3,(#29512,#29513,#29514,#29515,#29516,
#29517,#29518,#29519,#29520,#29521,#29522,#29523,#29524,#29525,#29526,#29527,
#29528,#29529,#29530,#29531,#29532,#29533,#29534,#29535,#29536,#29537,#29538,
#29539,#29540,#29541,#29542,#29543,#29544,#29545,#29546,#29547,#29548,#29549,
#29550,#29551,#29552,#29553,#29554,#29555,#29556,#29557,#29558,#29559,#29560,
#29561,#29562,#29563,#29564,#29565,#29566,#29567,#29568,#29569,#29570,#29571,
#29572,#29573,#29574,#29575,#29576,#29577,#29578,#29579,#29580,#29581,#29582,
#29583,#29584,#29585,#29586,#29587,#29588,#29589,#29590,#29591,#29592,#29593,
#29594,#29595,#29596,#29597,#29598,#29599,#29600,#29601,#29602,#29603,#29604,
#29605),.UNSPECIFIED.,.F.,.F.,(4,3,3,3,3,3,3,3,3,3,3,3,3,3,3,3,3,3,3,3,
3,3,3,3,3,3,3,3,3,3,3,4),(-0.5668473060481,-0.536665117700605,-0.506058907018577,
-0.497416865349869,-0.490479658256923,-0.460332723361999,-0.437086688141514,
-0.424703702797736,-0.420462740364944,-0.391037848573074,-0.361869496829336,
-0.333545860020099,-0.318750505414604,-0.313020125757269,-0.308660186231234,
-0.280670745320505,-0.27436444159812,-0.245887081934671,-0.216156157441912,
-0.204673881207046,-0.200549631648242,-0.172713964179309,-0.1449492205742,
-0.117659621562307,-0.103957129616093,-0.099925224573015,-0.0958138196940146,
-0.0691413018599106,-0.0429166306649946,-0.017493155823278,-0.00803968599259441,
0.),.UNSPECIFIED.);
#2685=B_SPLINE_CURVE_WITH_KNOTS('',3,(#29607,#29608,#29609,#29610,#29611,
#29612,#29613,#29614,#29615,#29616,#29617),.UNSPECIFIED.,.F.,.F.,(4,1,1,
1,1,1,1,1,4),(15.7079632679489,15.8295388729956,16.8221763756675,17.8148138783395,
18.8074513810114,19.8000888836834,20.7927263863553,21.7853638890272,21.9911485751285),
 .UNSPECIFIED.);
#2686=B_SPLINE_CURVE_WITH_KNOTS('',3,(#29618,#29619,#29620,#29621,#29622,
#29623,#29624,#29625,#29626,#29627),.UNSPECIFIED.,.F.,.F.,(4,1,1,1,1,1,
1,4),(15.7079632679489,16.3836751323157,17.3763126349877,18.3689501376596,
19.3615876403316,20.3542251430035,21.3468626456754,21.9911485751285),
 .UNSPECIFIED.);
#2687=B_SPLINE_CURVE_WITH_KNOTS('',3,(#29876,#29877,#29878,#29879,#29880,
#29881,#29882,#29883,#29884,#29885,#29886,#29887,#29888,#29889,#29890,#29891,
#29892,#29893,#29894,#29895,#29896,#29897,#29898,#29899,#29900,#29901,#29902,
#29903,#29904,#29905,#29906,#29907,#29908,#29909,#29910,#29911,#29912,#29913,
#29914,#29915,#29916,#29917,#29918,#29919,#29920,#29921,#29922,#29923,#29924,
#29925,#29926,#29927,#29928,#29929,#29930,#29931,#29932,#29933,#29934,#29935,
#29936,#29937,#29938,#29939,#29940,#29941,#29942,#29943,#29944,#29945,#29946,
#29947,#29948,#29949,#29950,#29951,#29952,#29953,#29954,#29955,#29956,#29957,
#29958,#29959,#29960,#29961,#29962,#29963,#29964,#29965,#29966),
 .UNSPECIFIED.,.F.,.F.,(4,3,3,3,3,3,3,3,3,3,3,3,3,3,3,3,3,3,3,3,3,3,3,3,
3,3,3,3,3,3,4),(0.,0.0253641802036794,0.0513998265899383,0.0781558064504026,
0.0899177781666192,0.0966255853603217,0.102679521312511,0.129980963020898,
0.157733251039943,0.18466185464837,0.195928350246773,0.202971019797871,
0.207098842066092,0.236273253769872,0.265447665473653,0.293340569485815,
0.302677606940801,0.308745486149141,0.314528754111136,0.342606748517284,
0.371727143140112,0.401175592932008,0.421351120766356,0.426753697775984,
0.456805211578956,0.48188392488091,0.490048787075816,0.498378789152568,
0.528887560036472,0.557120064786771,0.566847306048087),.UNSPECIFIED.);
#2688=B_SPLINE_CURVE_WITH_KNOTS('',3,(#29967,#29968,#29969,#29970,#29971,
#29972,#29973,#29974,#29975,#29976,#29977,#29978,#29979,#29980,#29981,#29982,
#29983,#29984,#29985,#29986,#29987,#29988,#29989,#29990,#29991),
 .UNSPECIFIED.,.F.,.F.,(4,3,3,3,3,3,3,3,4),(-10.1321597128207,-9.92637502671944,
-8.9337375240475,-7.94110002137556,-6.94846251870361,-5.95582501603167,
-4.96318751335973,-3.97055001068778,-3.84897440564114),.UNSPECIFIED.);
#2689=B_SPLINE_CURVE_WITH_KNOTS('',3,(#30240,#30241,#30242,#30243,#30244,
#30245,#30246,#30247,#30248,#30249,#30250,#30251,#30252,#30253,#30254,#30255,
#30256,#30257,#30258,#30259,#30260,#30261),.UNSPECIFIED.,.F.,.F.,(4,3,3,
3,3,3,3,4),(7.59274844815666,7.94110002137556,8.9337375240475,9.92637502671945,
10.9190125293914,11.9116500320633,12.9042875347353,13.8759337553362),
 .UNSPECIFIED.);
#2690=B_SPLINE_CURVE_WITH_KNOTS('',3,(#30262,#30263,#30264,#30265,#30266,
#30267,#30268,#30269,#30270,#30271,#30272,#30273,#30274,#30275,#30276,#30277,
#30278,#30279,#30280,#30281,#30282,#30283,#30284,#30285,#30286,#30287,#30288,
#30289,#30290,#30291,#30292,#30293,#30294,#30295,#30296,#30297,#30298,#30299,
#30300,#30301,#30302,#30303,#30304,#30305,#30306,#30307,#30308,#30309,#30310,
#30311,#30312,#30313,#30314,#30315,#30316,#30317,#30318,#30319,#30320,#30321,
#30322,#30323,#30324,#30325,#30326,#30327,#30328,#30329,#30330,#30331,#30332,
#30333,#30334,#30335,#30336,#30337,#30338,#30339,#30340,#30341,#30342,#30343,
#30344,#30345,#30346,#30347,#30348,#30349,#30350,#30351,#30352),
 .UNSPECIFIED.,.F.,.F.,(4,3,3,3,3,3,3,3,3,3,3,3,3,3,3,3,3,3,3,3,3,3,3,3,
3,3,3,3,3,3,4),(0.,0.0297250940606226,0.0601088150228004,0.0893485979000871,
0.114933407917713,0.120627517505873,0.150386821840842,0.179982106535776,
0.208493349412105,0.220471797235071,0.228882342936493,0.234177131450068,
0.264102104745581,0.292006792916583,0.294027078041094,0.322973449076029,
0.339362619052793,0.343535826866069,0.371629350449308,0.399767744210079,
0.42750209977512,0.437970813781883,0.445641127259269,0.450375043472223,
0.478076737189517,0.498853007477489,0.508250442141124,0.513369590092699,
0.539284536873453,0.561181818341402,0.569248610399439),.UNSPECIFIED.);
#2691=B_SPLINE_CURVE_WITH_KNOTS('',3,(#30355,#30356,#30357,#30358,#30359,
#30360,#30361,#30362,#30363,#30364,#30365,#30366,#30367,#30368,#30369,#30370,
#30371,#30372,#30373,#30374,#30375,#30376,#30377,#30378,#30379,#30380,#30381,
#30382,#30383,#30384,#30385,#30386,#30387,#30388,#30389,#30390,#30391,#30392,
#30393,#30394,#30395,#30396,#30397,#30398,#30399,#30400,#30401,#30402,#30403,
#30404,#30405,#30406,#30407,#30408,#30409,#30410,#30411,#30412,#30413,#30414,
#30415,#30416,#30417,#30418,#30419,#30420,#30421,#30422,#30423,#30424,#30425,
#30426,#30427,#30428,#30429,#30430,#30431,#30432,#30433,#30434,#30435,#30436,
#30437,#30438,#30439,#30440,#30441,#30442,#30443,#30444,#30445,#30446,#30447,
#30448),.UNSPECIFIED.,.F.,.F.,(4,3,3,3,3,3,3,3,3,3,3,3,3,3,3,3,3,3,3,3,
3,3,3,3,3,3,3,3,3,3,3,4),(-0.569248610399398,-0.543573536722457,-0.517270363294533,
-0.51040366831408,-0.504800304920549,-0.477738576752391,-0.455893971507876,
-0.447075989543432,-0.442407398493899,-0.414675017857191,-0.386513453890818,
-0.358572518516808,-0.344674822586674,-0.340104930814443,-0.311174106326863,
-0.30298173479627,-0.275165112946267,-0.246719605185614,-0.236777782571111,
-0.231757129783002,-0.227578398430794,-0.19857896285462,-0.169010366474117,
-0.13921149993454,-0.1230309187555,-0.11799756500965,-0.1133915884468,-0.0828440209407878,
-0.0522699732955569,-0.0223136611739256,-0.009766850502225,0.),
 .UNSPECIFIED.);
#2692=B_SPLINE_CURVE_WITH_KNOTS('',3,(#30449,#30450,#30451,#30452,#30453,
#30454,#30455,#30456,#30457,#30458,#30459,#30460,#30461,#30462,#30463,#30464,
#30465,#30466,#30467,#30468,#30469,#30470,#30471,#30472,#30473,#30474,#30475,
#30476,#30477,#30478,#30479,#30480,#30481,#30482,#30483,#30484,#30485,#30486,
#30487,#30488,#30489,#30490,#30491,#30492,#30493,#30494,#30495,#30496,#30497,
#30498,#30499,#30500,#30501,#30502,#30503,#30504,#30505,#30506,#30507,#30508,
#30509,#30510,#30511,#30512,#30513,#30514,#30515,#30516,#30517,#30518,#30519,
#30520,#30521,#30522,#30523,#30524,#30525,#30526,#30527,#30528,#30529,#30530,
#30531,#30532,#30533,#30534,#30535,#30536,#30537,#30538,#30539,#30540,#30541,
#30542),.UNSPECIFIED.,.F.,.F.,(4,3,3,3,3,3,3,3,3,3,3,3,3,3,3,3,3,3,3,3,
3,3,3,3,3,3,3,3,3,3,3,4),(-0.566847306048064,-0.53666509932804,-0.506058883722337,
-0.49741683674965,-0.490479652915231,-0.460332718584937,-0.437086683961585,
-0.424703692897771,-0.420462729229891,-0.391037839573047,-0.361869490079316,
-0.333545859563191,-0.318750505071923,-0.313020120746328,-0.308660183205439,
-0.280670749749197,-0.274364441598121,-0.245887082486665,-0.216156157924906,
-0.204673880202647,-0.200549631865089,-0.172713963141432,-0.144949220293018,
-0.117659627928902,-0.103957135186863,-0.0999252328769017,-0.0958138230959625,
-0.0691413094734294,-0.0429166477463372,-0.0174931891367085,-0.00803968599259447,
0.),.UNSPECIFIED.);
#2693=B_SPLINE_CURVE_WITH_KNOTS('',3,(#30544,#30545,#30546,#30547,#30548,
#30549,#30550,#30551,#30552,#30553,#30554),.UNSPECIFIED.,.F.,.F.,(4,1,1,
1,1,1,1,1,4),(15.7079632679489,15.8295388729956,16.8221763756675,17.8148138783395,
18.8074513810114,19.8000888836834,20.7927263863553,21.7853638890272,21.9911485751285),
 .UNSPECIFIED.);
#2694=B_SPLINE_CURVE_WITH_KNOTS('',3,(#30555,#30556,#30557,#30558,#30559,
#30560,#30561,#30562,#30563,#30564),.UNSPECIFIED.,.F.,.F.,(4,1,1,1,1,1,
1,4),(15.7079632679489,16.3836751323157,17.3763126349877,18.3689501376596,
19.3615876403316,20.3542251430035,21.3468626456754,21.9911485751285),
 .UNSPECIFIED.);
#2695=B_SPLINE_CURVE_WITH_KNOTS('',3,(#30813,#30814,#30815,#30816,#30817,
#30818,#30819,#30820,#30821,#30822,#30823,#30824,#30825,#30826,#30827,#30828,
#30829,#30830,#30831,#30832,#30833,#30834,#30835,#30836,#30837,#30838,#30839,
#30840,#30841,#30842,#30843,#30844,#30845,#30846,#30847,#30848,#30849,#30850,
#30851,#30852,#30853,#30854,#30855,#30856,#30857,#30858,#30859,#30860,#30861,
#30862,#30863,#30864,#30865,#30866,#30867,#30868,#30869,#30870,#30871,#30872,
#30873,#30874,#30875,#30876,#30877,#30878,#30879,#30880,#30881,#30882,#30883,
#30884,#30885,#30886,#30887,#30888,#30889,#30890,#30891,#30892,#30893,#30894,
#30895,#30896,#30897,#30898,#30899,#30900,#30901,#30902,#30903),
 .UNSPECIFIED.,.F.,.F.,(4,3,3,3,3,3,3,3,3,3,3,3,3,3,3,3,3,3,3,3,3,3,3,3,
3,3,3,3,3,3,4),(0.,0.0253642096188033,0.0513998826295139,0.0781558554850298,
0.0899177895596805,0.0966255868861821,0.102679521310141,0.129980983678453,
0.157733281985931,0.184661877857859,0.195928355278117,0.202971022163091,
0.207098846486765,0.236273255980203,0.265447665473641,0.293340555515088,
0.302677577825616,0.308745367798475,0.314528755200454,0.342606729855242,
0.371727115235203,0.401175562560648,0.421351051065242,0.426753724704252,
0.456805234460622,0.481883942042153,0.490048814940579,0.498378782229001,
0.528887553514328,0.557120064786745,0.566847306048064),.UNSPECIFIED.);
#2696=B_SPLINE_CURVE_WITH_KNOTS('',3,(#30904,#30905,#30906,#30907,#30908,
#30909,#30910,#30911,#30912,#30913,#30914,#30915,#30916,#30917,#30918,#30919,
#30920,#30921,#30922,#30923,#30924,#30925,#30926,#30927,#30928),
 .UNSPECIFIED.,.F.,.F.,(4,3,3,3,3,3,3,3,4),(-10.1321597128207,-9.92637502671944,
-8.9337375240475,-7.94110002137556,-6.94846251870361,-5.95582501603167,
-4.96318751335973,-3.97055001068778,-3.84897440564114),.UNSPECIFIED.);
#2697=B_SPLINE_CURVE_WITH_KNOTS('',3,(#31177,#31178,#31179,#31180,#31181,
#31182,#31183,#31184,#31185,#31186,#31187,#31188,#31189,#31190,#31191,#31192,
#31193,#31194,#31195,#31196,#31197,#31198),.UNSPECIFIED.,.F.,.F.,(4,3,3,
3,3,3,3,4),(7.59274844815666,7.94110002137555,8.9337375240475,9.92637502671945,
10.9190125293914,11.9116500320633,12.9042875347353,13.8759337553362),
 .UNSPECIFIED.);
#2698=B_SPLINE_CURVE_WITH_KNOTS('',3,(#31199,#31200,#31201,#31202,#31203,
#31204,#31205,#31206,#31207,#31208,#31209,#31210,#31211,#31212,#31213,#31214,
#31215,#31216,#31217,#31218,#31219,#31220,#31221,#31222,#31223,#31224,#31225,
#31226,#31227,#31228,#31229,#31230,#31231,#31232,#31233,#31234,#31235,#31236,
#31237,#31238,#31239,#31240,#31241,#31242,#31243,#31244,#31245,#31246,#31247,
#31248,#31249,#31250,#31251,#31252,#31253,#31254,#31255,#31256,#31257,#31258,
#31259,#31260,#31261,#31262,#31263,#31264,#31265,#31266,#31267,#31268,#31269,
#31270,#31271,#31272,#31273,#31274,#31275,#31276,#31277,#31278,#31279,#31280,
#31281,#31282,#31283,#31284,#31285,#31286,#31287,#31288,#31289),
 .UNSPECIFIED.,.F.,.F.,(4,3,3,3,3,3,3,3,3,3,3,3,3,3,3,3,3,3,3,3,3,3,3,3,
3,3,3,3,3,3,4),(0.,0.0297250654509073,0.0601087721503145,0.0893485603866636,
0.114933375093469,0.120627515201004,0.150386819046398,0.179982111307967,
0.208493352991252,0.220471805771853,0.22888236649448,0.234177138111355,
0.264102108076231,0.292006803331058,0.294027078041107,0.322973447641599,
0.33936262260274,0.34353583112749,0.371629353805975,0.399767747163329,0.427502108378127,
0.43797083449966,0.445641199537009,0.450375060671855,0.478076750089239,
0.498853017152278,0.50825047774578,0.513369599814417,0.539284560918029,
0.561181818341393,0.569248610399432),.UNSPECIFIED.);
#2699=B_SPLINE_CURVE_WITH_KNOTS('',3,(#31645,#31646,#31647,#31648,#31649,
#31650,#31651),.UNSPECIFIED.,.F.,.F.,(4,3,4),(45.2911347714885,46.2720920281241,
47.2566046244672),.UNSPECIFIED.);
#2700=B_SPLINE_CURVE_WITH_KNOTS('',3,(#31659,#31660,#31661,#31662,#31663,
#31664,#31665,#31666,#31667,#31668,#31669,#31670,#31671),.UNSPECIFIED.,
 .F.,.F.,(4,3,3,3,4),(-45.238934211693,-44.303066835438,-43.3185542390949,
-42.3340416427518,-41.5495372882101),.UNSPECIFIED.);
#2701=B_SPLINE_CURVE_WITH_KNOTS('',3,(#31676,#31677,#31678,#31679,#31680,
#31681,#31682,#31683,#31684,#31685,#31686,#31687,#31688,#31689,#31690,#31691,
#31692,#31693,#31694,#31695,#31696,#31697,#31698,#31699,#31700),
 .UNSPECIFIED.,.F.,.F.,(4,3,3,3,3,3,3,3,4),(39.0079494643089,39.3805038537227,
40.3650164500657,41.3495290464088,42.3340416427518,43.3185542390949,44.303066835438,
45.287579431781,45.2911347714885),.UNSPECIFIED.);
#2702=B_SPLINE_CURVE_WITH_KNOTS('',3,(#31701,#31702,#31703,#31704,#31705,
#31706,#31707,#31708,#31709,#31710,#31711,#31712,#31713,#31714,#31715,#31716,
#31717,#31718,#31719,#31720,#31721,#31722,#31723,#31724,#31725),
 .UNSPECIFIED.,.F.,.F.,(4,3,3,3,3,3,3,3,4),(-41.5495372882101,-41.3495290464088,
-40.3650164500657,-39.3805038537227,-38.3959912573796,-37.4114786610365,
-36.4269660646935,-35.4424534683504,-35.2663519810305),.UNSPECIFIED.);
#2703=B_SPLINE_CURVE_WITH_KNOTS('',3,(#31730,#31731,#31732,#31733,#31734,
#31735,#31736,#31737,#31738,#31739,#31740,#31741,#31742,#31743,#31744,#31745,
#31746,#31747,#31748,#31749,#31750,#31751),.UNSPECIFIED.,.F.,.F.,(4,3,3,
3,3,3,3,4),(32.7247641571293,33.4734282756643,34.4579408720073,35.4424534683504,
36.4269660646935,37.4114786610365,38.3959912573796,39.0079494643089),
 .UNSPECIFIED.);
#2704=B_SPLINE_CURVE_WITH_KNOTS('',3,(#31752,#31753,#31754,#31755,#31756,
#31757,#31758,#31759,#31760,#31761,#31762,#31763,#31764,#31765,#31766,#31767,
#31768,#31769,#31770,#31771,#31772,#31773),.UNSPECIFIED.,.F.,.F.,(4,3,3,
3,3,3,3,4),(-35.2663519810305,-34.4579408720073,-33.4734282756643,-32.4889156793212,
-31.5044030829781,-30.5198904866351,-29.535377890292,-28.9831666738509),
 .UNSPECIFIED.);
#2705=B_SPLINE_CURVE_WITH_KNOTS('',3,(#31778,#31779,#31780,#31781,#31782,
#31783,#31784,#31785,#31786,#31787,#31788,#31789,#31790,#31791,#31792,#31793,
#31794,#31795,#31796,#31797,#31798,#31799,#31800,#31801,#31802),
 .UNSPECIFIED.,.F.,.F.,(4,3,3,3,3,3,3,3,4),(26.4415788499498,26.5818401012628,
27.5663526976059,28.5508652939489,29.535377890292,30.5198904866351,31.5044030829781,
32.4889156793212,32.7247641571293),.UNSPECIFIED.);
#2706=B_SPLINE_CURVE_WITH_KNOTS('',3,(#31803,#31804,#31805,#31806,#31807,
#31808,#31809,#31810,#31811,#31812,#31813,#31814,#31815,#31816,#31817,#31818,
#31819,#31820,#31821,#31822,#31823,#31824),.UNSPECIFIED.,.F.,.F.,(4,3,3,
3,3,3,3,4),(-28.9831666738509,-28.5508652939489,-27.5663526976059,-26.5818401012628,
-25.5973275049197,-24.6128149085767,-23.6283023122336,-22.6999813666713),
 .UNSPECIFIED.);
#2707=B_SPLINE_CURVE_WITH_KNOTS('',3,(#31829,#31830,#31831,#31832,#31833,
#31834,#31835,#31836,#31837,#31838,#31839,#31840,#31841,#31842,#31843,#31844,
#31845,#31846,#31847,#31848,#31849,#31850),.UNSPECIFIED.,.F.,.F.,(4,3,3,
3,3,3,3,4),(20.1583935427702,20.6747645232044,21.6592771195475,22.6437897158905,
23.6283023122336,24.6128149085767,25.5973275049197,26.4415788499498),
 .UNSPECIFIED.);
#2708=B_SPLINE_CURVE_WITH_KNOTS('',3,(#31851,#31852,#31853,#31854,#31855,
#31856,#31857,#31858,#31859,#31860,#31861,#31862,#31863,#31864,#31865,#31866,
#31867,#31868,#31869,#31870,#31871,#31872,#31873,#31874,#31875),
 .UNSPECIFIED.,.F.,.F.,(4,3,3,3,3,3,3,3,4),(-22.6999813666713,-22.6437897158905,
-21.6592771195475,-20.6747645232044,-19.6902519268613,-18.7057393305183,
-17.7212267341752,-16.7367141378321,-16.4167960594917),.UNSPECIFIED.);
#2709=B_SPLINE_CURVE_WITH_KNOTS('',3,(#31880,#31881,#31882,#31883,#31884,
#31885,#31886,#31887,#31888,#31889,#31890,#31891,#31892,#31893,#31894,#31895,
#31896,#31897,#31898,#31899,#31900,#31901),.UNSPECIFIED.,.F.,.F.,(4,3,3,
3,3,3,3,4),(13.8752082355906,14.767688945146,15.7522015414891,16.7367141378321,
17.7212267341752,18.7057393305183,19.6902519268613,20.1583935427702),
 .UNSPECIFIED.);
#2710=B_SPLINE_CURVE_WITH_KNOTS('',3,(#31902,#31903,#31904,#31905,#31906,
#31907,#31908,#31909,#31910,#31911,#31912,#31913,#31914,#31915,#31916,#31917,
#31918,#31919,#31920,#31921,#31922,#31923),.UNSPECIFIED.,.F.,.F.,(4,3,3,
3,3,3,3,4),(-16.4167960594917,-15.7522015414891,-14.767688945146,-13.7831763488029,
-12.7986637524599,-11.8141511561168,-10.8296385597737,-10.1336107523121),
 .UNSPECIFIED.);
#2711=B_SPLINE_CURVE_WITH_KNOTS('',3,(#31929,#31930,#31931,#31932,#31933,
#31934,#31935,#31936,#31937,#31938,#31939,#31940,#31941),.UNSPECIFIED.,
 .F.,.F.,(4,3,3,3,4),(-3.85042544513253,-2.9535377890292,-1.96902519268613,
-0.984512596343067,0.),.UNSPECIFIED.);
#2712=B_SPLINE_CURVE_WITH_KNOTS('',3,(#31944,#31945,#31946,#31947,#31948,
#31949,#31950,#31951,#31952,#31953,#31954,#31955,#31956,#31957,#31958,#31959,
#31960,#31961,#31962),.UNSPECIFIED.,.F.,.F.,(4,3,3,3,3,3,4),(2.01767041277416,
2.9535377890292,3.93805038537227,4.92256298171533,5.9070755780584,6.89158817440147,
7.592022928411),.UNSPECIFIED.);
#2713=B_SPLINE_CURVE_WITH_KNOTS('',3,(#31968,#31969,#31970,#31971,#31972,
#31973,#31974,#31975,#31976),.UNSPECIFIED.,.F.,.F.,(4,1,1,1,1,1,4),(53.4070751110265,
54.1915794655683,55.1760920619113,56.1606046582544,57.1451172545975,58.1296298509405,
59.1141424472836),.UNSPECIFIED.);
#2714=B_SPLINE_CURVE_WITH_KNOTS('',3,(#31979,#31980,#31981,#31982,#31983,
#31984,#31985,#31986,#31987,#31988),.UNSPECIFIED.,.F.,.F.,(4,1,1,1,1,1,
1,4),(53.4070751110265,53.7796295004402,54.7641420967832,55.7486546931263,
56.7331672894694,57.7176798858124,58.7021924821555,59.6380598584106),
 .UNSPECIFIED.);
#2715=B_SPLINE_CURVE_WITH_KNOTS('',3,(#31993,#31994,#31995,#31996,#31997,
#31998,#31999,#32000,#32001,#32002,#32003),.UNSPECIFIED.,.F.,.F.,(4,1,1,
1,1,1,1,1,4),(47.1238898038469,47.2999912911668,48.2845038875099,49.2690164838529,
50.253529080196,51.2380416765391,52.2225542728821,53.2070668692252,53.4070751110265),
 .UNSPECIFIED.);
#2716=B_SPLINE_CURVE_WITH_KNOTS('',3,(#32004,#32005,#32006,#32007,#32008,
#32009,#32010,#32011,#32012,#32013),.UNSPECIFIED.,.F.,.F.,(4,1,1,1,1,1,
1,4),(47.1238898038469,47.8725539223818,48.8570665187248,49.8415791150679,
50.826091711411,51.810604307754,52.7951169040971,53.4070751110265),
 .UNSPECIFIED.);
#2717=B_SPLINE_CURVE_WITH_KNOTS('',3,(#32018,#32019,#32020,#32021,#32022,
#32023,#32024,#32025,#32026,#32027),.UNSPECIFIED.,.F.,.F.,(4,1,1,1,1,1,
1,4),(40.8407044966673,41.3929157131084,42.3774283094515,43.3619409057945,
44.3464535021376,45.3309660984807,46.3154786948237,47.1238898038469),
 .UNSPECIFIED.);
#2718=B_SPLINE_CURVE_WITH_KNOTS('',3,(#32028,#32029,#32030,#32031,#32032,
#32033,#32034,#32035,#32036,#32037,#32038),.UNSPECIFIED.,.F.,.F.,(4,1,1,
1,1,1,1,1,4),(40.8407044966673,40.9809657479803,41.9654783443234,42.9499909406665,
43.9345035370095,44.9190161333526,45.9035287296957,46.8880413260387,47.1238898038469),
 .UNSPECIFIED.);
#2719=B_SPLINE_CURVE_WITH_KNOTS('',3,(#32043,#32044,#32045,#32046,#32047,
#32048,#32049,#32050,#32051,#32052),.UNSPECIFIED.,.F.,.F.,(4,1,1,1,1,1,
1,4),(34.5575191894877,35.48584013505,36.4703527313931,37.4548653277361,
38.4393779240792,39.4238905204223,40.4084031167653,40.8407044966673),
 .UNSPECIFIED.);
#2720=B_SPLINE_CURVE_WITH_KNOTS('',3,(#32053,#32054,#32055,#32056,#32057,
#32058,#32059,#32060,#32061,#32062),.UNSPECIFIED.,.F.,.F.,(4,1,1,1,1,1,
1,4),(34.5575191894877,35.0738901699219,36.058402766265,37.0429153626081,
38.0274279589511,39.0119405552942,39.9964531516373,40.8407044966673),
 .UNSPECIFIED.);
#2721=B_SPLINE_CURVE_WITH_KNOTS('',3,(#32067,#32068,#32069,#32070,#32071,
#32072,#32073,#32074,#32075,#32076,#32077),.UNSPECIFIED.,.F.,.F.,(4,1,1,
1,1,1,1,1,4),(28.2743338823081,28.5942519606485,29.5787645569916,30.5632771533347,
31.5477897496777,32.5323023460208,33.5168149423639,34.5013275387069,34.5575191894877),
 .UNSPECIFIED.);
#2722=B_SPLINE_CURVE_WITH_KNOTS('',3,(#32078,#32079,#32080,#32081,#32082,
#32083,#32084,#32085,#32086,#32087),.UNSPECIFIED.,.F.,.F.,(4,1,1,1,1,1,
1,4),(28.2743338823081,29.1668145918635,30.1513271882066,31.1358397845497,
32.1203523808927,33.1048649772358,34.0893775735789,34.5575191894877),
 .UNSPECIFIED.);
#2723=B_SPLINE_CURVE_WITH_KNOTS('',3,(#32092,#32093,#32094,#32095,#32096,
#32097,#32098,#32099,#32100,#32101),.UNSPECIFIED.,.F.,.F.,(4,1,1,1,1,1,
1,4),(21.9911485751285,22.6871763825901,23.6716889789332,24.6562015752763,
25.6407141716193,26.6252267679624,27.6097393643055,28.2743338823081),
 .UNSPECIFIED.);
#2724=B_SPLINE_CURVE_WITH_KNOTS('',3,(#32102,#32103,#32104,#32105,#32106,
#32107,#32108,#32109,#32110,#32111,#32112),.UNSPECIFIED.,.F.,.F.,(4,1,1,
1,1,1,1,1,4),(21.9911485751285,22.2752264174621,23.2597390138051,24.2442516101482,
25.2287642064913,26.2132768028343,27.1977893991774,28.1823019955205,28.2743338823081),
 .UNSPECIFIED.);
#2725=B_SPLINE_CURVE_WITH_KNOTS('',3,(#32118,#32119,#32120,#32121,#32122),
 .UNSPECIFIED.,.F.,.F.,(4,1,4),(14.3991256467175,15.3836382430606,15.7079632679489),
 .UNSPECIFIED.);
#2726=B_SPLINE_CURVE_WITH_KNOTS('',3,(#32125,#32126,#32127,#32128,#32129),
 .UNSPECIFIED.,.F.,.F.,(4,1,4),(13.8752082355906,14.8110756118456,15.7079632679489),
 .UNSPECIFIED.);
#2727=B_SPLINE_CURVE_WITH_KNOTS('',3,(#32135,#32136,#32137,#32138,#32139,
#32140,#32141),.UNSPECIFIED.,.F.,.F.,(4,3,4),(45.2911347714885,46.2720920281241,
47.2566046244672),.UNSPECIFIED.);
#2728=B_SPLINE_CURVE_WITH_KNOTS('',3,(#32149,#32150,#32151,#32152,#32153,
#32154,#32155,#32156,#32157,#32158,#32159,#32160,#32161),.UNSPECIFIED.,
 .F.,.F.,(4,3,3,3,4),(-45.238934211693,-44.303066835438,-43.3185542390949,
-42.3340416427519,-41.54953728821),.UNSPECIFIED.);
#2729=B_SPLINE_CURVE_WITH_KNOTS('',3,(#32166,#32167,#32168,#32169,#32170,
#32171,#32172,#32173,#32174,#32175,#32176,#32177,#32178,#32179,#32180,#32181,
#32182,#32183,#32184,#32185,#32186,#32187,#32188,#32189,#32190),
 .UNSPECIFIED.,.F.,.F.,(4,3,3,3,3,3,3,3,4),(39.0079494643089,39.3805038537226,
40.3650164500657,41.3495290464088,42.3340416427518,43.3185542390949,44.303066835438,
45.287579431781,45.2911347714885),.UNSPECIFIED.);
#2730=B_SPLINE_CURVE_WITH_KNOTS('',3,(#32191,#32192,#32193,#32194,#32195,
#32196,#32197,#32198,#32199,#32200,#32201,#32202,#32203,#32204,#32205,#32206,
#32207,#32208,#32209,#32210,#32211,#32212,#32213,#32214,#32215),
 .UNSPECIFIED.,.F.,.F.,(4,3,3,3,3,3,3,3,4),(-41.54953728821,-41.3495290464088,
-40.3650164500657,-39.3805038537227,-38.3959912573796,-37.4114786610365,
-36.4269660646935,-35.4424534683504,-35.2663519810305),.UNSPECIFIED.);
#2731=B_SPLINE_CURVE_WITH_KNOTS('',3,(#32220,#32221,#32222,#32223,#32224,
#32225,#32226,#32227,#32228,#32229,#32230,#32231,#32232,#32233,#32234,#32235,
#32236,#32237,#32238,#32239,#32240,#32241),.UNSPECIFIED.,.F.,.F.,(4,3,3,
3,3,3,3,4),(32.7247641571293,33.4734282756642,34.4579408720073,35.4424534683504,
36.4269660646934,37.4114786610365,38.3959912573796,39.0079494643089),
 .UNSPECIFIED.);
#2732=B_SPLINE_CURVE_WITH_KNOTS('',3,(#32242,#32243,#32244,#32245,#32246,
#32247,#32248,#32249,#32250,#32251,#32252,#32253,#32254,#32255,#32256,#32257,
#32258,#32259,#32260,#32261,#32262,#32263),.UNSPECIFIED.,.F.,.F.,(4,3,3,
3,3,3,3,4),(-35.2663519810305,-34.4579408720073,-33.4734282756642,-32.4889156793212,
-31.5044030829781,-30.5198904866351,-29.535377890292,-28.9831666738509),
 .UNSPECIFIED.);
#2733=B_SPLINE_CURVE_WITH_KNOTS('',3,(#32268,#32269,#32270,#32271,#32272,
#32273,#32274,#32275,#32276,#32277,#32278,#32279,#32280,#32281,#32282,#32283,
#32284,#32285,#32286,#32287,#32288,#32289,#32290,#32291,#32292),
 .UNSPECIFIED.,.F.,.F.,(4,3,3,3,3,3,3,3,4),(26.4415788499498,26.5818401012628,
27.5663526976058,28.5508652939489,29.535377890292,30.519890486635,31.5044030829781,
32.4889156793212,32.7247641571293),.UNSPECIFIED.);
#2734=B_SPLINE_CURVE_WITH_KNOTS('',3,(#32293,#32294,#32295,#32296,#32297,
#32298,#32299,#32300,#32301,#32302,#32303,#32304,#32305,#32306,#32307,#32308,
#32309,#32310,#32311,#32312,#32313,#32314),.UNSPECIFIED.,.F.,.F.,(4,3,3,
3,3,3,3,4),(-28.9831666738509,-28.5508652939489,-27.5663526976059,-26.5818401012628,
-25.5973275049197,-24.6128149085767,-23.6283023122336,-22.6999813666713),
 .UNSPECIFIED.);
#2735=B_SPLINE_CURVE_WITH_KNOTS('',3,(#32319,#32320,#32321,#32322,#32323,
#32324,#32325,#32326,#32327,#32328,#32329,#32330,#32331,#32332,#32333,#32334,
#32335,#32336,#32337,#32338,#32339,#32340),.UNSPECIFIED.,.F.,.F.,(4,3,3,
3,3,3,3,4),(20.1583935427702,20.6747645232044,21.6592771195474,22.6437897158905,
23.6283023122336,24.6128149085766,25.5973275049197,26.4415788499498),
 .UNSPECIFIED.);
#2736=B_SPLINE_CURVE_WITH_KNOTS('',3,(#32341,#32342,#32343,#32344,#32345,
#32346,#32347,#32348,#32349,#32350,#32351,#32352,#32353,#32354,#32355,#32356,
#32357,#32358,#32359,#32360,#32361,#32362,#32363,#32364,#32365),
 .UNSPECIFIED.,.F.,.F.,(4,3,3,3,3,3,3,3,4),(-22.6999813666713,-22.6437897158905,
-21.6592771195475,-20.6747645232044,-19.6902519268613,-18.7057393305183,
-17.7212267341752,-16.7367141378321,-16.4167960594917),.UNSPECIFIED.);
#2737=B_SPLINE_CURVE_WITH_KNOTS('',3,(#32370,#32371,#32372,#32373,#32374,
#32375,#32376,#32377,#32378,#32379,#32380,#32381,#32382,#32383,#32384,#32385,
#32386,#32387,#32388,#32389,#32390,#32391),.UNSPECIFIED.,.F.,.F.,(4,3,3,
3,3,3,3,4),(13.8752082355906,14.767688945146,15.7522015414891,16.7367141378321,
17.7212267341752,18.7057393305182,19.6902519268613,20.1583935427702),
 .UNSPECIFIED.);
#2738=B_SPLINE_CURVE_WITH_KNOTS('',3,(#32392,#32393,#32394,#32395,#32396,
#32397,#32398,#32399,#32400,#32401,#32402,#32403,#32404,#32405,#32406,#32407,
#32408,#32409,#32410,#32411,#32412,#32413),.UNSPECIFIED.,.F.,.F.,(4,3,3,
3,3,3,3,4),(-16.4167960594917,-15.7522015414891,-14.767688945146,-13.7831763488029,
-12.7986637524599,-11.8141511561168,-10.8296385597737,-10.1336107523121),
 .UNSPECIFIED.);
#2739=B_SPLINE_CURVE_WITH_KNOTS('',3,(#32419,#32420,#32421,#32422,#32423,
#32424,#32425,#32426,#32427,#32428,#32429,#32430,#32431),.UNSPECIFIED.,
 .F.,.F.,(4,3,3,3,4),(-3.85042544513253,-2.9535377890292,-1.96902519268613,
-0.984512596343066,0.),.UNSPECIFIED.);
#2740=B_SPLINE_CURVE_WITH_KNOTS('',3,(#32434,#32435,#32436,#32437,#32438,
#32439,#32440,#32441,#32442,#32443,#32444,#32445,#32446,#32447,#32448,#32449,
#32450,#32451,#32452),.UNSPECIFIED.,.F.,.F.,(4,3,3,3,3,3,4),(2.01767041277416,
2.9535377890292,3.93805038537227,4.92256298171533,5.9070755780584,6.89158817440146,
7.592022928411),.UNSPECIFIED.);
#2741=B_SPLINE_CURVE_WITH_KNOTS('',3,(#32458,#32459,#32460,#32461,#32462,
#32463,#32464,#32465,#32466),.UNSPECIFIED.,.F.,.F.,(4,1,1,1,1,1,4),(53.4070751110265,
54.1915794655683,55.1760920619113,56.1606046582544,57.1451172545975,58.1296298509405,
59.1141424472836),.UNSPECIFIED.);
#2742=B_SPLINE_CURVE_WITH_KNOTS('',3,(#32469,#32470,#32471,#32472,#32473,
#32474,#32475,#32476,#32477,#32478),.UNSPECIFIED.,.F.,.F.,(4,1,1,1,1,1,
1,4),(53.4070751110265,53.7796295004402,54.7641420967832,55.7486546931263,
56.7331672894694,57.7176798858124,58.7021924821555,59.6380598584105),
 .UNSPECIFIED.);
#2743=B_SPLINE_CURVE_WITH_KNOTS('',3,(#32483,#32484,#32485,#32486,#32487,
#32488,#32489,#32490,#32491,#32492,#32493),.UNSPECIFIED.,.F.,.F.,(4,1,1,
1,1,1,1,1,4),(47.1238898038469,47.2999912911668,48.2845038875099,49.2690164838529,
50.253529080196,51.2380416765391,52.2225542728821,53.2070668692252,53.4070751110265),
 .UNSPECIFIED.);
#2744=B_SPLINE_CURVE_WITH_KNOTS('',3,(#32494,#32495,#32496,#32497,#32498,
#32499,#32500,#32501,#32502,#32503),.UNSPECIFIED.,.F.,.F.,(4,1,1,1,1,1,
1,4),(47.1238898038469,47.8725539223818,48.8570665187248,49.8415791150679,
50.826091711411,51.810604307754,52.7951169040971,53.4070751110265),
 .UNSPECIFIED.);
#2745=B_SPLINE_CURVE_WITH_KNOTS('',3,(#32508,#32509,#32510,#32511,#32512,
#32513,#32514,#32515,#32516,#32517),.UNSPECIFIED.,.F.,.F.,(4,1,1,1,1,1,
1,4),(40.8407044966673,41.3929157131084,42.3774283094515,43.3619409057945,
44.3464535021376,45.3309660984807,46.3154786948237,47.1238898038469),
 .UNSPECIFIED.);
#2746=B_SPLINE_CURVE_WITH_KNOTS('',3,(#32518,#32519,#32520,#32521,#32522,
#32523,#32524,#32525,#32526,#32527,#32528),.UNSPECIFIED.,.F.,.F.,(4,1,1,
1,1,1,1,1,4),(40.8407044966673,40.9809657479803,41.9654783443234,42.9499909406664,
43.9345035370095,44.9190161333526,45.9035287296956,46.8880413260387,47.1238898038469),
 .UNSPECIFIED.);
#2747=B_SPLINE_CURVE_WITH_KNOTS('',3,(#32533,#32534,#32535,#32536,#32537,
#32538,#32539,#32540,#32541,#32542),.UNSPECIFIED.,.F.,.F.,(4,1,1,1,1,1,
1,4),(34.5575191894877,35.48584013505,36.4703527313931,37.4548653277361,
38.4393779240792,39.4238905204223,40.4084031167653,40.8407044966673),
 .UNSPECIFIED.);
#2748=B_SPLINE_CURVE_WITH_KNOTS('',3,(#32543,#32544,#32545,#32546,#32547,
#32548,#32549,#32550,#32551,#32552),.UNSPECIFIED.,.F.,.F.,(4,1,1,1,1,1,
1,4),(34.5575191894877,35.0738901699219,36.058402766265,37.042915362608,
38.0274279589511,39.0119405552942,39.9964531516372,40.8407044966673),
 .UNSPECIFIED.);
#2749=B_SPLINE_CURVE_WITH_KNOTS('',3,(#32557,#32558,#32559,#32560,#32561,
#32562,#32563,#32564,#32565,#32566,#32567),.UNSPECIFIED.,.F.,.F.,(4,1,1,
1,1,1,1,1,4),(28.2743338823081,28.5942519606485,29.5787645569916,30.5632771533347,
31.5477897496777,32.5323023460208,33.5168149423639,34.5013275387069,34.5575191894877),
 .UNSPECIFIED.);
#2750=B_SPLINE_CURVE_WITH_KNOTS('',3,(#32568,#32569,#32570,#32571,#32572,
#32573,#32574,#32575,#32576,#32577),.UNSPECIFIED.,.F.,.F.,(4,1,1,1,1,1,
1,4),(28.2743338823081,29.1668145918635,30.1513271882066,31.1358397845496,
32.1203523808927,33.1048649772358,34.0893775735788,34.5575191894877),
 .UNSPECIFIED.);
#2751=B_SPLINE_CURVE_WITH_KNOTS('',3,(#32582,#32583,#32584,#32585,#32586,
#32587,#32588,#32589,#32590,#32591),.UNSPECIFIED.,.F.,.F.,(4,1,1,1,1,1,
1,4),(21.9911485751285,22.6871763825901,23.6716889789332,24.6562015752763,
25.6407141716193,26.6252267679624,27.6097393643055,28.2743338823081),
 .UNSPECIFIED.);
#2752=B_SPLINE_CURVE_WITH_KNOTS('',3,(#32592,#32593,#32594,#32595,#32596,
#32597,#32598,#32599,#32600,#32601,#32602),.UNSPECIFIED.,.F.,.F.,(4,1,1,
1,1,1,1,1,4),(21.9911485751285,22.2752264174621,23.2597390138051,24.2442516101482,
25.2287642064913,26.2132768028343,27.1977893991774,28.1823019955205,28.2743338823081),
 .UNSPECIFIED.);
#2753=B_SPLINE_CURVE_WITH_KNOTS('',3,(#32608,#32609,#32610,#32611,#32612),
 .UNSPECIFIED.,.F.,.F.,(4,1,4),(14.3991256467175,15.3836382430606,15.7079632679489),
 .UNSPECIFIED.);
#2754=B_SPLINE_CURVE_WITH_KNOTS('',3,(#32615,#32616,#32617,#32618,#32619),
 .UNSPECIFIED.,.F.,.F.,(4,1,4),(13.8752082355906,14.8110756118456,15.7079632679489),
 .UNSPECIFIED.);
#2755=B_SPLINE_CURVE_WITH_KNOTS('',3,(#32625,#32626,#32627,#32628,#32629,
#32630,#32631),.UNSPECIFIED.,.F.,.F.,(4,3,4),(45.2911347714885,46.2720920281241,
47.2566046244672),.UNSPECIFIED.);
#2756=B_SPLINE_CURVE_WITH_KNOTS('',3,(#32639,#32640,#32641,#32642,#32643,
#32644,#32645,#32646,#32647,#32648,#32649,#32650,#32651),.UNSPECIFIED.,
 .F.,.F.,(4,3,3,3,4),(-45.238934211693,-44.303066835438,-43.3185542390949,
-42.3340416427518,-41.5495372882101),.UNSPECIFIED.);
#2757=B_SPLINE_CURVE_WITH_KNOTS('',3,(#32656,#32657,#32658,#32659,#32660,
#32661,#32662,#32663,#32664,#32665,#32666,#32667,#32668,#32669,#32670,#32671,
#32672,#32673,#32674,#32675,#32676,#32677,#32678,#32679,#32680),
 .UNSPECIFIED.,.F.,.F.,(4,3,3,3,3,3,3,3,4),(39.0079494643089,39.3805038537227,
40.3650164500657,41.3495290464088,42.3340416427518,43.3185542390949,44.303066835438,
45.287579431781,45.2911347714885),.UNSPECIFIED.);
#2758=B_SPLINE_CURVE_WITH_KNOTS('',3,(#32681,#32682,#32683,#32684,#32685,
#32686,#32687,#32688,#32689,#32690,#32691,#32692,#32693,#32694,#32695,#32696,
#32697,#32698,#32699,#32700,#32701,#32702,#32703,#32704,#32705),
 .UNSPECIFIED.,.F.,.F.,(4,3,3,3,3,3,3,3,4),(-41.5495372882101,-41.3495290464088,
-40.3650164500657,-39.3805038537227,-38.3959912573796,-37.4114786610365,
-36.4269660646935,-35.4424534683504,-35.2663519810305),.UNSPECIFIED.);
#2759=B_SPLINE_CURVE_WITH_KNOTS('',3,(#32710,#32711,#32712,#32713,#32714,
#32715,#32716,#32717,#32718,#32719,#32720,#32721,#32722,#32723,#32724,#32725,
#32726,#32727,#32728,#32729,#32730,#32731),.UNSPECIFIED.,.F.,.F.,(4,3,3,
3,3,3,3,4),(32.7247641571293,33.4734282756643,34.4579408720073,35.4424534683504,
36.4269660646935,37.4114786610365,38.3959912573796,39.0079494643089),
 .UNSPECIFIED.);
#2760=B_SPLINE_CURVE_WITH_KNOTS('',3,(#32732,#32733,#32734,#32735,#32736,
#32737,#32738,#32739,#32740,#32741,#32742,#32743,#32744,#32745,#32746,#32747,
#32748,#32749,#32750,#32751,#32752,#32753),.UNSPECIFIED.,.F.,.F.,(4,3,3,
3,3,3,3,4),(-35.2663519810305,-34.4579408720073,-33.4734282756643,-32.4889156793212,
-31.5044030829781,-30.5198904866351,-29.535377890292,-28.9831666738509),
 .UNSPECIFIED.);
#2761=B_SPLINE_CURVE_WITH_KNOTS('',3,(#32758,#32759,#32760,#32761,#32762,
#32763,#32764,#32765,#32766,#32767,#32768,#32769,#32770,#32771,#32772,#32773,
#32774,#32775,#32776,#32777,#32778,#32779,#32780,#32781,#32782),
 .UNSPECIFIED.,.F.,.F.,(4,3,3,3,3,3,3,3,4),(26.4415788499498,26.5818401012628,
27.5663526976059,28.5508652939489,29.535377890292,30.5198904866351,31.5044030829781,
32.4889156793212,32.7247641571293),.UNSPECIFIED.);
#2762=B_SPLINE_CURVE_WITH_KNOTS('',3,(#32783,#32784,#32785,#32786,#32787,
#32788,#32789,#32790,#32791,#32792,#32793,#32794,#32795,#32796,#32797,#32798,
#32799,#32800,#32801,#32802,#32803,#32804),.UNSPECIFIED.,.F.,.F.,(4,3,3,
3,3,3,3,4),(-28.9831666738509,-28.5508652939489,-27.5663526976059,-26.5818401012628,
-25.5973275049197,-24.6128149085767,-23.6283023122336,-22.6999813666713),
 .UNSPECIFIED.);
#2763=B_SPLINE_CURVE_WITH_KNOTS('',3,(#32809,#32810,#32811,#32812,#32813,
#32814,#32815,#32816,#32817,#32818,#32819,#32820,#32821,#32822,#32823,#32824,
#32825,#32826,#32827,#32828,#32829,#32830),.UNSPECIFIED.,.F.,.F.,(4,3,3,
3,3,3,3,4),(20.1583935427702,20.6747645232044,21.6592771195475,22.6437897158905,
23.6283023122336,24.6128149085767,25.5973275049197,26.4415788499498),
 .UNSPECIFIED.);
#2764=B_SPLINE_CURVE_WITH_KNOTS('',3,(#32831,#32832,#32833,#32834,#32835,
#32836,#32837,#32838,#32839,#32840,#32841,#32842,#32843,#32844,#32845,#32846,
#32847,#32848,#32849,#32850,#32851,#32852,#32853,#32854,#32855),
 .UNSPECIFIED.,.F.,.F.,(4,3,3,3,3,3,3,3,4),(-22.6999813666713,-22.6437897158905,
-21.6592771195475,-20.6747645232044,-19.6902519268613,-18.7057393305183,
-17.7212267341752,-16.7367141378321,-16.4167960594917),.UNSPECIFIED.);
#2765=B_SPLINE_CURVE_WITH_KNOTS('',3,(#32860,#32861,#32862,#32863,#32864,
#32865,#32866,#32867,#32868,#32869,#32870,#32871,#32872,#32873,#32874,#32875,
#32876,#32877,#32878,#32879,#32880,#32881),.UNSPECIFIED.,.F.,.F.,(4,3,3,
3,3,3,3,4),(13.8752082355906,14.767688945146,15.7522015414891,16.7367141378321,
17.7212267341752,18.7057393305183,19.6902519268613,20.1583935427702),
 .UNSPECIFIED.);
#2766=B_SPLINE_CURVE_WITH_KNOTS('',3,(#32882,#32883,#32884,#32885,#32886,
#32887,#32888,#32889,#32890,#32891,#32892,#32893,#32894,#32895,#32896,#32897,
#32898,#32899,#32900,#32901,#32902,#32903),.UNSPECIFIED.,.F.,.F.,(4,3,3,
3,3,3,3,4),(-16.4167960594917,-15.7522015414891,-14.767688945146,-13.7831763488029,
-12.7986637524599,-11.8141511561168,-10.8296385597737,-10.1336107523121),
 .UNSPECIFIED.);
#2767=B_SPLINE_CURVE_WITH_KNOTS('',3,(#32909,#32910,#32911,#32912,#32913,
#32914,#32915,#32916,#32917,#32918,#32919,#32920,#32921),.UNSPECIFIED.,
 .F.,.F.,(4,3,3,3,4),(-3.85042544513253,-2.9535377890292,-1.96902519268613,
-0.984512596343067,0.),.UNSPECIFIED.);
#2768=B_SPLINE_CURVE_WITH_KNOTS('',3,(#32924,#32925,#32926,#32927,#32928,
#32929,#32930,#32931,#32932,#32933,#32934,#32935,#32936,#32937,#32938,#32939,
#32940,#32941,#32942),.UNSPECIFIED.,.F.,.F.,(4,3,3,3,3,3,4),(2.01767041277416,
2.9535377890292,3.93805038537227,4.92256298171533,5.9070755780584,6.89158817440147,
7.592022928411),.UNSPECIFIED.);
#2769=B_SPLINE_CURVE_WITH_KNOTS('',3,(#32948,#32949,#32950,#32951,#32952,
#32953,#32954,#32955,#32956),.UNSPECIFIED.,.F.,.F.,(4,1,1,1,1,1,4),(53.4070751110265,
54.1915794655683,55.1760920619113,56.1606046582544,57.1451172545975,58.1296298509405,
59.1141424472836),.UNSPECIFIED.);
#2770=B_SPLINE_CURVE_WITH_KNOTS('',3,(#32959,#32960,#32961,#32962,#32963,
#32964,#32965,#32966,#32967,#32968),.UNSPECIFIED.,.F.,.F.,(4,1,1,1,1,1,
1,4),(53.4070751110265,53.7796295004402,54.7641420967832,55.7486546931263,
56.7331672894694,57.7176798858124,58.7021924821555,59.6380598584106),
 .UNSPECIFIED.);
#2771=B_SPLINE_CURVE_WITH_KNOTS('',3,(#32973,#32974,#32975,#32976,#32977,
#32978,#32979,#32980,#32981,#32982,#32983),.UNSPECIFIED.,.F.,.F.,(4,1,1,
1,1,1,1,1,4),(47.1238898038469,47.2999912911668,48.2845038875099,49.2690164838529,
50.253529080196,51.2380416765391,52.2225542728821,53.2070668692252,53.4070751110265),
 .UNSPECIFIED.);
#2772=B_SPLINE_CURVE_WITH_KNOTS('',3,(#32984,#32985,#32986,#32987,#32988,
#32989,#32990,#32991,#32992,#32993),.UNSPECIFIED.,.F.,.F.,(4,1,1,1,1,1,
1,4),(47.1238898038469,47.8725539223818,48.8570665187248,49.8415791150679,
50.826091711411,51.810604307754,52.7951169040971,53.4070751110265),
 .UNSPECIFIED.);
#2773=B_SPLINE_CURVE_WITH_KNOTS('',3,(#32998,#32999,#33000,#33001,#33002,
#33003,#33004,#33005,#33006,#33007),.UNSPECIFIED.,.F.,.F.,(4,1,1,1,1,1,
1,4),(40.8407044966673,41.3929157131084,42.3774283094515,43.3619409057945,
44.3464535021376,45.3309660984807,46.3154786948237,47.1238898038469),
 .UNSPECIFIED.);
#2774=B_SPLINE_CURVE_WITH_KNOTS('',3,(#33008,#33009,#33010,#33011,#33012,
#33013,#33014,#33015,#33016,#33017,#33018),.UNSPECIFIED.,.F.,.F.,(4,1,1,
1,1,1,1,1,4),(40.8407044966673,40.9809657479803,41.9654783443234,42.9499909406665,
43.9345035370095,44.9190161333526,45.9035287296957,46.8880413260387,47.1238898038469),
 .UNSPECIFIED.);
#2775=B_SPLINE_CURVE_WITH_KNOTS('',3,(#33023,#33024,#33025,#33026,#33027,
#33028,#33029,#33030,#33031,#33032),.UNSPECIFIED.,.F.,.F.,(4,1,1,1,1,1,
1,4),(34.5575191894877,35.48584013505,36.4703527313931,37.4548653277361,
38.4393779240792,39.4238905204223,40.4084031167653,40.8407044966673),
 .UNSPECIFIED.);
#2776=B_SPLINE_CURVE_WITH_KNOTS('',3,(#33033,#33034,#33035,#33036,#33037,
#33038,#33039,#33040,#33041,#33042),.UNSPECIFIED.,.F.,.F.,(4,1,1,1,1,1,
1,4),(34.5575191894877,35.0738901699219,36.058402766265,37.0429153626081,
38.0274279589511,39.0119405552942,39.9964531516373,40.8407044966673),
 .UNSPECIFIED.);
#2777=B_SPLINE_CURVE_WITH_KNOTS('',3,(#33047,#33048,#33049,#33050,#33051,
#33052,#33053,#33054,#33055,#33056,#33057),.UNSPECIFIED.,.F.,.F.,(4,1,1,
1,1,1,1,1,4),(28.2743338823081,28.5942519606485,29.5787645569916,30.5632771533347,
31.5477897496777,32.5323023460208,33.5168149423639,34.5013275387069,34.5575191894877),
 .UNSPECIFIED.);
#2778=B_SPLINE_CURVE_WITH_KNOTS('',3,(#33058,#33059,#33060,#33061,#33062,
#33063,#33064,#33065,#33066,#33067),.UNSPECIFIED.,.F.,.F.,(4,1,1,1,1,1,
1,4),(28.2743338823081,29.1668145918635,30.1513271882066,31.1358397845497,
32.1203523808927,33.1048649772358,34.0893775735789,34.5575191894877),
 .UNSPECIFIED.);
#2779=B_SPLINE_CURVE_WITH_KNOTS('',3,(#33072,#33073,#33074,#33075,#33076,
#33077,#33078,#33079,#33080,#33081),.UNSPECIFIED.,.F.,.F.,(4,1,1,1,1,1,
1,4),(21.9911485751285,22.6871763825901,23.6716889789332,24.6562015752763,
25.6407141716193,26.6252267679624,27.6097393643055,28.2743338823081),
 .UNSPECIFIED.);
#2780=B_SPLINE_CURVE_WITH_KNOTS('',3,(#33082,#33083,#33084,#33085,#33086,
#33087,#33088,#33089,#33090,#33091,#33092),.UNSPECIFIED.,.F.,.F.,(4,1,1,
1,1,1,1,1,4),(21.9911485751285,22.2752264174621,23.2597390138051,24.2442516101482,
25.2287642064913,26.2132768028343,27.1977893991774,28.1823019955205,28.2743338823081),
 .UNSPECIFIED.);
#2781=B_SPLINE_CURVE_WITH_KNOTS('',3,(#33098,#33099,#33100,#33101,#33102),
 .UNSPECIFIED.,.F.,.F.,(4,1,4),(14.3991256467175,15.3836382430606,15.7079632679489),
 .UNSPECIFIED.);
#2782=B_SPLINE_CURVE_WITH_KNOTS('',3,(#33105,#33106,#33107,#33108,#33109),
 .UNSPECIFIED.,.F.,.F.,(4,1,4),(13.8752082355906,14.8110756118456,15.7079632679489),
 .UNSPECIFIED.);
#2783=B_SPLINE_CURVE_WITH_KNOTS('',3,(#33115,#33116,#33117,#33118,#33119,
#33120,#33121),.UNSPECIFIED.,.F.,.F.,(4,3,4),(45.2911347714885,46.2720920281241,
47.2566046244672),.UNSPECIFIED.);
#2784=B_SPLINE_CURVE_WITH_KNOTS('',3,(#33129,#33130,#33131,#33132,#33133,
#33134,#33135,#33136,#33137,#33138,#33139,#33140,#33141),.UNSPECIFIED.,
 .F.,.F.,(4,3,3,3,4),(-45.238934211693,-44.303066835438,-43.3185542390949,
-42.3340416427518,-41.54953728821),.UNSPECIFIED.);
#2785=B_SPLINE_CURVE_WITH_KNOTS('',3,(#33146,#33147,#33148,#33149,#33150,
#33151,#33152,#33153,#33154,#33155,#33156,#33157,#33158,#33159,#33160,#33161,
#33162,#33163,#33164,#33165,#33166,#33167,#33168,#33169,#33170),
 .UNSPECIFIED.,.F.,.F.,(4,3,3,3,3,3,3,3,4),(39.0079494643089,39.3805038537226,
40.3650164500657,41.3495290464088,42.3340416427518,43.3185542390949,44.303066835438,
45.287579431781,45.2911347714885),.UNSPECIFIED.);
#2786=B_SPLINE_CURVE_WITH_KNOTS('',3,(#33171,#33172,#33173,#33174,#33175,
#33176,#33177,#33178,#33179,#33180,#33181,#33182,#33183,#33184,#33185,#33186,
#33187,#33188,#33189,#33190,#33191,#33192,#33193,#33194,#33195),
 .UNSPECIFIED.,.F.,.F.,(4,3,3,3,3,3,3,3,4),(-41.54953728821,-41.3495290464088,
-40.3650164500657,-39.3805038537226,-38.3959912573796,-37.4114786610365,
-36.4269660646934,-35.4424534683504,-35.2663519810305),.UNSPECIFIED.);
#2787=B_SPLINE_CURVE_WITH_KNOTS('',3,(#33200,#33201,#33202,#33203,#33204,
#33205,#33206,#33207,#33208,#33209,#33210,#33211,#33212,#33213,#33214,#33215,
#33216,#33217,#33218,#33219,#33220,#33221),.UNSPECIFIED.,.F.,.F.,(4,3,3,
3,3,3,3,4),(32.7247641571293,33.4734282756642,34.4579408720073,35.4424534683504,
36.4269660646934,37.4114786610365,38.3959912573796,39.0079494643089),
 .UNSPECIFIED.);
#2788=B_SPLINE_CURVE_WITH_KNOTS('',3,(#33222,#33223,#33224,#33225,#33226,
#33227,#33228,#33229,#33230,#33231,#33232,#33233,#33234,#33235,#33236,#33237,
#33238,#33239,#33240,#33241,#33242,#33243),.UNSPECIFIED.,.F.,.F.,(4,3,3,
3,3,3,3,4),(-35.2663519810305,-34.4579408720073,-33.4734282756642,-32.4889156793212,
-31.5044030829781,-30.519890486635,-29.535377890292,-28.9831666738509),
 .UNSPECIFIED.);
#2789=B_SPLINE_CURVE_WITH_KNOTS('',3,(#33248,#33249,#33250,#33251,#33252,
#33253,#33254,#33255,#33256,#33257,#33258,#33259,#33260,#33261,#33262,#33263,
#33264,#33265,#33266,#33267,#33268,#33269,#33270,#33271,#33272),
 .UNSPECIFIED.,.F.,.F.,(4,3,3,3,3,3,3,3,4),(26.4415788499497,26.5818401012628,
27.5663526976059,28.5508652939489,29.535377890292,30.519890486635,31.5044030829781,
32.4889156793212,32.7247641571293),.UNSPECIFIED.);
#2790=B_SPLINE_CURVE_WITH_KNOTS('',3,(#33273,#33274,#33275,#33276,#33277,
#33278,#33279,#33280,#33281,#33282,#33283,#33284,#33285,#33286,#33287,#33288,
#33289,#33290,#33291,#33292,#33293,#33294),.UNSPECIFIED.,.F.,.F.,(4,3,3,
3,3,3,3,4),(-28.9831666738509,-28.5508652939489,-27.5663526976059,-26.5818401012628,
-25.5973275049197,-24.6128149085767,-23.6283023122336,-22.6999813666713),
 .UNSPECIFIED.);
#2791=B_SPLINE_CURVE_WITH_KNOTS('',3,(#33299,#33300,#33301,#33302,#33303,
#33304,#33305,#33306,#33307,#33308,#33309,#33310,#33311,#33312,#33313,#33314,
#33315,#33316,#33317,#33318,#33319,#33320),.UNSPECIFIED.,.F.,.F.,(4,3,3,
3,3,3,3,4),(20.1583935427702,20.6747645232044,21.6592771195474,22.6437897158905,
23.6283023122336,24.6128149085766,25.5973275049197,26.4415788499497),
 .UNSPECIFIED.);
#2792=B_SPLINE_CURVE_WITH_KNOTS('',3,(#33321,#33322,#33323,#33324,#33325,
#33326,#33327,#33328,#33329,#33330,#33331,#33332,#33333,#33334,#33335,#33336,
#33337,#33338,#33339,#33340,#33341,#33342,#33343,#33344,#33345),
 .UNSPECIFIED.,.F.,.F.,(4,3,3,3,3,3,3,3,4),(-22.6999813666713,-22.6437897158905,
-21.6592771195475,-20.6747645232044,-19.6902519268613,-18.7057393305183,
-17.7212267341752,-16.7367141378321,-16.4167960594917),.UNSPECIFIED.);
#2793=B_SPLINE_CURVE_WITH_KNOTS('',3,(#33350,#33351,#33352,#33353,#33354,
#33355,#33356,#33357,#33358,#33359,#33360,#33361,#33362,#33363,#33364,#33365,
#33366,#33367,#33368,#33369,#33370,#33371),.UNSPECIFIED.,.F.,.F.,(4,3,3,
3,3,3,3,4),(13.8752082355906,14.767688945146,15.7522015414891,16.7367141378321,
17.7212267341752,18.7057393305182,19.6902519268613,20.1583935427702),
 .UNSPECIFIED.);
#2794=B_SPLINE_CURVE_WITH_KNOTS('',3,(#33372,#33373,#33374,#33375,#33376,
#33377,#33378,#33379,#33380,#33381,#33382,#33383,#33384,#33385,#33386,#33387,
#33388,#33389,#33390,#33391,#33392,#33393),.UNSPECIFIED.,.F.,.F.,(4,3,3,
3,3,3,3,4),(-16.4167960594917,-15.7522015414891,-14.767688945146,-13.7831763488029,
-12.7986637524599,-11.8141511561168,-10.8296385597737,-10.1336107523121),
 .UNSPECIFIED.);
#2795=B_SPLINE_CURVE_WITH_KNOTS('',3,(#33399,#33400,#33401,#33402,#33403,
#33404,#33405,#33406,#33407,#33408,#33409,#33410,#33411),.UNSPECIFIED.,
 .F.,.F.,(4,3,3,3,4),(-3.85042544513252,-2.9535377890292,-1.96902519268613,
-0.984512596343066,0.),.UNSPECIFIED.);
#2796=B_SPLINE_CURVE_WITH_KNOTS('',3,(#33414,#33415,#33416,#33417,#33418,
#33419,#33420,#33421,#33422,#33423,#33424,#33425,#33426,#33427,#33428,#33429,
#33430,#33431,#33432),.UNSPECIFIED.,.F.,.F.,(4,3,3,3,3,3,4),(2.01767041277416,
2.9535377890292,3.93805038537226,4.92256298171533,5.90707557805839,6.89158817440146,
7.59202292841098),.UNSPECIFIED.);
#2797=B_SPLINE_CURVE_WITH_KNOTS('',3,(#33438,#33439,#33440,#33441,#33442,
#33443,#33444,#33445,#33446),.UNSPECIFIED.,.F.,.F.,(4,1,1,1,1,1,4),(53.4070751110265,
54.1915794655683,55.1760920619113,56.1606046582544,57.1451172545975,58.1296298509405,
59.1141424472836),.UNSPECIFIED.);
#2798=B_SPLINE_CURVE_WITH_KNOTS('',3,(#33449,#33450,#33451,#33452,#33453,
#33454,#33455,#33456,#33457,#33458),.UNSPECIFIED.,.F.,.F.,(4,1,1,1,1,1,
1,4),(53.4070751110265,53.7796295004402,54.7641420967832,55.7486546931263,
56.7331672894694,57.7176798858124,58.7021924821555,59.6380598584106),
 .UNSPECIFIED.);
#2799=B_SPLINE_CURVE_WITH_KNOTS('',3,(#33463,#33464,#33465,#33466,#33467,
#33468,#33469,#33470,#33471,#33472,#33473),.UNSPECIFIED.,.F.,.F.,(4,1,1,
1,1,1,1,1,4),(47.1238898038469,47.2999912911668,48.2845038875099,49.2690164838529,
50.253529080196,51.2380416765391,52.2225542728821,53.2070668692252,53.4070751110265),
 .UNSPECIFIED.);
#2800=B_SPLINE_CURVE_WITH_KNOTS('',3,(#33474,#33475,#33476,#33477,#33478,
#33479,#33480,#33481,#33482,#33483),.UNSPECIFIED.,.F.,.F.,(4,1,1,1,1,1,
1,4),(47.1238898038469,47.8725539223818,48.8570665187248,49.8415791150679,
50.826091711411,51.810604307754,52.7951169040971,53.4070751110265),
 .UNSPECIFIED.);
#2801=B_SPLINE_CURVE_WITH_KNOTS('',3,(#33488,#33489,#33490,#33491,#33492,
#33493,#33494,#33495,#33496,#33497),.UNSPECIFIED.,.F.,.F.,(4,1,1,1,1,1,
1,4),(40.8407044966673,41.3929157131084,42.3774283094515,43.3619409057945,
44.3464535021376,45.3309660984807,46.3154786948237,47.1238898038469),
 .UNSPECIFIED.);
#2802=B_SPLINE_CURVE_WITH_KNOTS('',3,(#33498,#33499,#33500,#33501,#33502,
#33503,#33504,#33505,#33506,#33507,#33508),.UNSPECIFIED.,.F.,.F.,(4,1,1,
1,1,1,1,1,4),(40.8407044966673,40.9809657479803,41.9654783443234,42.9499909406665,
43.9345035370095,44.9190161333526,45.9035287296957,46.8880413260387,47.1238898038469),
 .UNSPECIFIED.);
#2803=B_SPLINE_CURVE_WITH_KNOTS('',3,(#33513,#33514,#33515,#33516,#33517,
#33518,#33519,#33520,#33521,#33522),.UNSPECIFIED.,.F.,.F.,(4,1,1,1,1,1,
1,4),(34.5575191894877,35.48584013505,36.4703527313931,37.4548653277361,
38.4393779240792,39.4238905204223,40.4084031167653,40.8407044966673),
 .UNSPECIFIED.);
#2804=B_SPLINE_CURVE_WITH_KNOTS('',3,(#33523,#33524,#33525,#33526,#33527,
#33528,#33529,#33530,#33531,#33532),.UNSPECIFIED.,.F.,.F.,(4,1,1,1,1,1,
1,4),(34.5575191894877,35.0738901699219,36.058402766265,37.0429153626081,
38.0274279589511,39.0119405552942,39.9964531516373,40.8407044966673),
 .UNSPECIFIED.);
#2805=B_SPLINE_CURVE_WITH_KNOTS('',3,(#33537,#33538,#33539,#33540,#33541,
#33542,#33543,#33544,#33545,#33546,#33547),.UNSPECIFIED.,.F.,.F.,(4,1,1,
1,1,1,1,1,4),(28.2743338823081,28.5942519606485,29.5787645569916,30.5632771533347,
31.5477897496777,32.5323023460208,33.5168149423639,34.5013275387069,34.5575191894877),
 .UNSPECIFIED.);
#2806=B_SPLINE_CURVE_WITH_KNOTS('',3,(#33548,#33549,#33550,#33551,#33552,
#33553,#33554,#33555,#33556,#33557),.UNSPECIFIED.,.F.,.F.,(4,1,1,1,1,1,
1,4),(28.2743338823081,29.1668145918635,30.1513271882066,31.1358397845497,
32.1203523808927,33.1048649772358,34.0893775735789,34.5575191894877),
 .UNSPECIFIED.);
#2807=B_SPLINE_CURVE_WITH_KNOTS('',3,(#33562,#33563,#33564,#33565,#33566,
#33567,#33568,#33569,#33570,#33571),.UNSPECIFIED.,.F.,.F.,(4,1,1,1,1,1,
1,4),(21.9911485751285,22.6871763825902,23.6716889789332,24.6562015752763,
25.6407141716194,26.6252267679624,27.6097393643055,28.2743338823081),
 .UNSPECIFIED.);
#2808=B_SPLINE_CURVE_WITH_KNOTS('',3,(#33572,#33573,#33574,#33575,#33576,
#33577,#33578,#33579,#33580,#33581,#33582),.UNSPECIFIED.,.F.,.F.,(4,1,1,
1,1,1,1,1,4),(21.9911485751285,22.2752264174621,23.2597390138051,24.2442516101482,
25.2287642064913,26.2132768028343,27.1977893991774,28.1823019955205,28.2743338823081),
 .UNSPECIFIED.);
#2809=B_SPLINE_CURVE_WITH_KNOTS('',3,(#33588,#33589,#33590,#33591,#33592),
 .UNSPECIFIED.,.F.,.F.,(4,1,4),(14.3991256467175,15.3836382430606,15.7079632679489),
 .UNSPECIFIED.);
#2810=B_SPLINE_CURVE_WITH_KNOTS('',3,(#33595,#33596,#33597,#33598,#33599),
 .UNSPECIFIED.,.F.,.F.,(4,1,4),(13.8752082355906,14.8110756118456,15.7079632679489),
 .UNSPECIFIED.);
#2811=B_SPLINE_CURVE_WITH_KNOTS('',3,(#33605,#33606,#33607,#33608,#33609,
#33610,#33611,#33612,#33613,#33614,#33615,#33616,#33617,#33618,#33619,#33620,
#33621,#33622,#33623,#33624,#33625,#33626,#33627,#33628,#33629,#33630,#33631,
#33632,#33633,#33634,#33635,#33636,#33637,#33638),.UNSPECIFIED.,.F.,.F.,
(4,3,3,3,3,3,3,3,3,3,3,4),(26.4410951701193,26.4459204490819,26.9356597166575,
27.4253989842331,27.9151382518087,28.4048775193843,28.8946167869599,29.3843560545355,
29.874095322111,30.3638345896866,30.8535738572622,31.3433131248378),
 .UNSPECIFIED.);
#2812=B_SPLINE_CURVE_WITH_KNOTS('',3,(#33642,#33643,#33644,#33645),
 .UNSPECIFIED.,.F.,.F.,(4,4),(-29.3215314335047,-28.9877616322403),
 .UNSPECIFIED.);
#2813=B_SPLINE_CURVE_WITH_KNOTS('',3,(#33649,#33650,#33651,#33652,#33653,
#33654,#33655,#33656,#33657,#33658,#33659,#33660,#33661,#33662,#33663,#33664,
#33665,#33666,#33667,#33668,#33669,#33670,#33671,#33672,#33673,#33674,#33675,
#33676,#33677,#33678,#33679,#33680,#33681,#33682,#33683,#33684,#33685,#33686,
#33687,#33688,#33689,#33690,#33691),.UNSPECIFIED.,.F.,.F.,(4,3,3,3,3,3,
3,3,3,3,3,3,3,3,4),(-28.9877616322403,-28.8946167869599,-28.4048775193843,
-27.9151382518087,-27.4253989842331,-26.9356597166575,-26.4459204490819,
-25.9561811815063,-25.4664419139307,-24.9767026463552,-24.4869633787796,
-23.997224111204,-23.5074848436284,-23.0177455760528,-22.7045763250607),
 .UNSPECIFIED.);
#2814=B_SPLINE_CURVE_WITH_KNOTS('',3,(#33696,#33697,#33698,#33699,#33700,
#33701,#33702,#33703,#33704,#33705,#33706,#33707,#33708,#33709,#33710,#33711,
#33712,#33713,#33714,#33715,#33716,#33717,#33718,#33719,#33720,#33721,#33722,
#33723,#33724,#33725,#33726,#33727,#33728,#33729,#33730,#33731,#33732,#33733,
#33734,#33735),.UNSPECIFIED.,.F.,.F.,(4,3,3,3,3,3,3,3,3,3,3,3,3,4),(20.1579098629397,
20.5690492381748,21.0587885057504,21.548527773326,22.0382670409016,22.5280063084772,
23.0177455760528,23.5074848436284,23.997224111204,24.4869633787796,24.9767026463551,
25.4664419139307,25.9561811815063,26.4410951701193),.UNSPECIFIED.);
#2815=B_SPLINE_CURVE_WITH_KNOTS('',3,(#33736,#33737,#33738,#33739,#33740,
#33741,#33742,#33743,#33744,#33745,#33746,#33747,#33748,#33749,#33750,#33751,
#33752,#33753,#33754,#33755,#33756,#33757,#33758,#33759,#33760,#33761,#33762,
#33763,#33764,#33765,#33766,#33767,#33768,#33769,#33770,#33771,#33772,#33773,
#33774,#33775),.UNSPECIFIED.,.F.,.F.,(4,3,3,3,3,3,3,3,3,3,3,3,3,4),(-22.7045763250607,
-22.5280063084772,-22.0382670409016,-21.548527773326,-21.0587885057504,
-20.5690492381748,-20.0793099705992,-19.5895707030236,-19.0998314354481,
-18.6100921678725,-18.1203529002969,-17.6306136327213,-16.6511350975701,
-16.4213910178811),.UNSPECIFIED.);
#2816=B_SPLINE_CURVE_WITH_KNOTS('',3,(#33780,#33781,#33782,#33783,#33784,
#33785,#33786,#33787,#33788,#33789,#33790,#33791,#33792,#33793,#33794,#33795,
#33796,#33797,#33798,#33799,#33800,#33801,#33802,#33803,#33804,#33805,#33806,
#33807,#33808,#33809,#33810,#33811,#33812,#33813),.UNSPECIFIED.,.F.,.F.,
(4,3,3,3,3,3,3,3,3,3,3,4),(13.8747245557601,14.2024387596921,14.6921780272677,
15.6716565624189,16.6511350975701,17.6306136327213,18.1203529002969,18.6100921678725,
19.099831435448,19.5895707030236,20.0793099705992,20.1579098629397),
 .UNSPECIFIED.);
#2817=B_SPLINE_CURVE_WITH_KNOTS('',3,(#33814,#33815,#33816,#33817,#33818,
#33819,#33820,#33821,#33822,#33823,#33824,#33825,#33826,#33827,#33828,#33829,
#33830,#33831,#33832,#33833,#33834,#33835,#33836,#33837,#33838,#33839,#33840,
#33841,#33842,#33843,#33844,#33845,#33846,#33847,#33848,#33849,#33850),
 .UNSPECIFIED.,.F.,.F.,(4,3,3,3,3,3,3,3,3,3,3,3,4),(-16.4213910178811,-15.6716565624189,
-14.6921780272677,-14.2024387596921,-13.7126994921166,-13.222960224541,
-12.7332209569654,-12.2434816893898,-11.7537424218142,-11.2640031542386,
-10.774263886663,-10.2845246190874,-10.1382057107015),.UNSPECIFIED.);
#2818=B_SPLINE_CURVE_WITH_KNOTS('',3,(#33856,#33857,#33858,#33859,#33860,
#33861,#33862,#33863,#33864,#33865,#33866,#33867,#33868,#33869,#33870,#33871,
#33872,#33873,#33874,#33875,#33876,#33877,#33878,#33879,#33880),
 .UNSPECIFIED.,.F.,.F.,(4,3,3,3,3,3,3,3,4),(-3.85502040352192,-3.42817487302914,
-2.93843560545355,-2.44869633787796,-1.95895707030237,-1.46921780272678,
-0.979478535151181,-0.489739267575591,0.),.UNSPECIFIED.);
#2819=B_SPLINE_CURVE_WITH_KNOTS('',3,(#33883,#33884,#33885,#33886,#33887,
#33888,#33889,#33890,#33891,#33892,#33893,#33894,#33895,#33896,#33897,#33898,
#33899,#33900,#33901,#33902,#33903,#33904,#33905,#33906,#33907,#33908,#33909,
#33910,#33911,#33912,#33913,#33914,#33915,#33916,#33917,#33918,#33919),
 .UNSPECIFIED.,.F.,.F.,(4,3,3,3,3,3,3,3,3,3,3,3,4),(2.02178169133308,2.44869633787796,
2.93843560545355,3.42817487302914,3.91791414060473,4.40765340818032,4.89739267575591,
5.3871319433315,5.87687121090709,6.36661047848268,6.85634974605827,7.34608901363386,
7.59153924858054),.UNSPECIFIED.);
#2820=B_SPLINE_CURVE_WITH_KNOTS('',3,(#33925,#33926,#33927,#33928,#33929,
#33930,#33931,#33932),.UNSPECIFIED.,.F.,.F.,(4,1,1,1,1,4),(40.8407044966673,
41.2372989189625,41.7270381865381,42.2167774541137,42.7065167216893,43.1962559892649),
 .UNSPECIFIED.);
#2821=B_SPLINE_CURVE_WITH_KNOTS('',3,(#33935,#33936,#33937,#33938,#33939,
#33940,#33941,#33942,#33943,#33944),.UNSPECIFIED.,.F.,.F.,(4,1,1,1,1,1,
1,4),(40.8407044966673,40.8455297756299,41.3352690432055,41.8250083107811,
42.3147475783567,42.8044868459323,43.2942261135079,43.7211407600527),
 .UNSPECIFIED.);
#2822=B_SPLINE_CURVE_WITH_KNOTS('',3,(#33949,#33950,#33951,#33952,#33953,
#33954,#33955,#33956,#33957,#33958,#33959,#33960,#33961,#33962,#33963,#33964,
#33965),.UNSPECIFIED.,.F.,.F.,(4,1,1,1,1,1,1,1,1,1,1,1,1,1,4),(34.5575191894877,
34.8706884404798,35.3604277080554,35.850166975631,36.3399062432066,36.8296455107822,
37.3193847783578,37.8091240459334,38.298863313509,38.7886025810846,39.2783418486602,
39.7680811162357,40.2578203838113,40.7475596513869,40.8407044966673),
 .UNSPECIFIED.);
#2823=B_SPLINE_CURVE_WITH_KNOTS('',3,(#33966,#33967,#33968,#33969,#33970,
#33971,#33972,#33973,#33974,#33975,#33976,#33977,#33978,#33979,#33980,#33981),
 .UNSPECIFIED.,.F.,.F.,(4,1,1,1,1,1,1,1,1,1,1,1,1,4),(34.5575191894877,
34.9686585647228,35.4583978322984,35.948137099874,36.4378763674496,36.9276156350252,
37.4173549026008,37.9070941701764,38.396833437752,38.8865727053276,39.3763119729032,
39.8660512404787,40.3557905080543,40.8407044966673),.UNSPECIFIED.);
#2824=B_SPLINE_CURVE_WITH_KNOTS('',3,(#33986,#33987,#33988,#33989,#33990,
#33991,#33992,#33993,#33994,#33995,#33996,#33997,#33998,#33999,#34000,#34001),
 .UNSPECIFIED.,.F.,.F.,(4,1,1,1,1,1,1,1,1,1,1,1,1,4),(28.2743338823081,
28.5040779619972,29.4835564971483,29.9732957647239,30.4630350322995,30.9527742998751,
31.4425135674507,31.9322528350263,32.4219921026019,32.9117313701775,33.4014706377531,
33.8912099053287,34.3809491729042,34.5575191894877),.UNSPECIFIED.);
#2825=B_SPLINE_CURVE_WITH_KNOTS('',3,(#34002,#34003,#34004,#34005,#34006,
#34007,#34008,#34009,#34010,#34011,#34012,#34013,#34014,#34015),
 .UNSPECIFIED.,.F.,.F.,(4,1,1,1,1,1,1,1,1,1,1,4),(28.2743338823081,28.6020480862402,
29.0917873538157,30.0712658889669,31.0507444241181,32.0302229592693,32.5199622268449,
33.0097014944205,33.4994407619961,33.9891800295717,34.4789192971472,34.5575191894877),
 .UNSPECIFIED.);
#2826=B_SPLINE_CURVE_WITH_KNOTS('',3,(#34020,#34021,#34022,#34023,#34024,
#34025,#34026,#34027,#34028,#34029,#34030,#34031,#34032,#34033,#34034),
 .UNSPECIFIED.,.F.,.F.,(4,1,1,1,1,1,1,1,1,1,1,1,4),(21.9911485751285,22.1374674835145,
22.6272067510901,23.1169460186656,23.6066852862412,24.0964245538168,24.5861638213924,
25.075903088968,25.5656423565436,26.0553816241192,26.5451208916948,27.524599426846,
28.2743338823081),.UNSPECIFIED.);
#2827=B_SPLINE_CURVE_WITH_KNOTS('',3,(#34035,#34036,#34037,#34038,#34039,
#34040,#34041,#34042,#34043,#34044,#34045,#34046,#34047,#34048,#34049,#34050,
#34051),.UNSPECIFIED.,.F.,.F.,(4,1,1,1,1,1,1,1,1,1,1,1,1,1,4),(21.9911485751285,
22.2354376077575,22.7251768753331,23.2149161429087,23.7046554104842,24.1943946780598,
24.6841339456354,25.173873213211,25.6636124807866,26.1533517483622,26.6430910159378,
27.1328302835134,27.622569551089,28.1123088186646,28.2743338823081),
 .UNSPECIFIED.);
#2828=B_SPLINE_CURVE_WITH_KNOTS('',3,(#34057,#34058,#34059,#34060,#34061,
#34062),.UNSPECIFIED.,.F.,.F.,(4,1,1,4),(14.399609326548,14.8893485941236,
15.3790878616992,15.707963267949),.UNSPECIFIED.);
#2829=B_SPLINE_CURVE_WITH_KNOTS('',3,(#34065,#34066,#34067,#34068,#34069,
#34070,#34071),.UNSPECIFIED.,.F.,.F.,(4,1,1,1,4),(13.8747245557601,14.301639202305,
14.7913784698806,15.2811177374562,15.707963267949),.UNSPECIFIED.);
#2830=B_SPLINE_CURVE_WITH_KNOTS('',3,(#34077,#34078,#34079,#34080,#34081,
#34082,#34083,#34084,#34085,#34086,#34087,#34088,#34089,#34090,#34091,#34092,
#34093,#34094,#34095,#34096,#34097,#34098,#34099,#34100,#34101,#34102,#34103,
#34104,#34105,#34106,#34107,#34108,#34109,#34110),.UNSPECIFIED.,.F.,.F.,
(4,3,3,3,3,3,3,3,3,3,3,4),(26.4410951701193,26.4459204490819,26.9356597166575,
27.4253989842331,27.9151382518087,28.4048775193843,28.8946167869599,29.3843560545355,
29.8740953221111,30.3638345896866,30.8535738572622,31.3433131248378),
 .UNSPECIFIED.);
#2831=B_SPLINE_CURVE_WITH_KNOTS('',3,(#34114,#34115,#34116,#34117),
 .UNSPECIFIED.,.F.,.F.,(4,4),(-29.3215314335047,-28.9877616322403),
 .UNSPECIFIED.);
#2832=B_SPLINE_CURVE_WITH_KNOTS('',3,(#34121,#34122,#34123,#34124,#34125,
#34126,#34127,#34128,#34129,#34130,#34131,#34132,#34133,#34134,#34135,#34136,
#34137,#34138,#34139,#34140,#34141,#34142,#34143,#34144,#34145,#34146,#34147,
#34148,#34149,#34150,#34151,#34152,#34153,#34154,#34155,#34156,#34157,#34158,
#34159,#34160,#34161,#34162,#34163),.UNSPECIFIED.,.F.,.F.,(4,3,3,3,3,3,
3,3,3,3,3,3,3,3,4),(-28.9877616322403,-28.8946167869599,-28.4048775193843,
-27.9151382518087,-27.4253989842331,-26.9356597166575,-26.4459204490819,
-25.9561811815063,-25.4664419139307,-24.9767026463551,-24.4869633787795,
-23.997224111204,-23.5074848436284,-23.0177455760528,-22.7045763250607),
 .UNSPECIFIED.);
#2833=B_SPLINE_CURVE_WITH_KNOTS('',3,(#34168,#34169,#34170,#34171,#34172,
#34173,#34174,#34175,#34176,#34177,#34178,#34179,#34180,#34181,#34182,#34183,
#34184,#34185,#34186,#34187,#34188,#34189,#34190,#34191,#34192,#34193,#34194,
#34195,#34196,#34197,#34198,#34199,#34200,#34201,#34202,#34203,#34204,#34205,
#34206,#34207),.UNSPECIFIED.,.F.,.F.,(4,3,3,3,3,3,3,3,3,3,3,3,3,4),(20.1579098629397,
20.5690492381748,21.0587885057504,21.548527773326,22.0382670409016,22.5280063084772,
23.0177455760528,23.5074848436284,23.997224111204,24.4869633787795,24.9767026463551,
25.4664419139307,25.9561811815063,26.4410951701193),.UNSPECIFIED.);
#2834=B_SPLINE_CURVE_WITH_KNOTS('',3,(#34208,#34209,#34210,#34211,#34212,
#34213,#34214,#34215,#34216,#34217,#34218,#34219,#34220,#34221,#34222,#34223,
#34224,#34225,#34226,#34227,#34228,#34229,#34230,#34231,#34232,#34233,#34234,
#34235,#34236,#34237,#34238,#34239,#34240,#34241,#34242,#34243,#34244,#34245,
#34246,#34247),.UNSPECIFIED.,.F.,.F.,(4,3,3,3,3,3,3,3,3,3,3,3,3,4),(-22.7045763250607,
-22.5280063084772,-22.0382670409016,-21.548527773326,-21.0587885057504,
-20.5690492381748,-20.0793099705992,-19.5895707030236,-19.099831435448,
-18.6100921678725,-18.1203529002969,-17.6306136327213,-16.6511350975701,
-16.4213910178811),.UNSPECIFIED.);
#2835=B_SPLINE_CURVE_WITH_KNOTS('',3,(#34252,#34253,#34254,#34255,#34256,
#34257,#34258,#34259,#34260,#34261,#34262,#34263,#34264,#34265,#34266,#34267,
#34268,#34269,#34270,#34271,#34272,#34273,#34274,#34275,#34276,#34277,#34278,
#34279,#34280,#34281,#34282,#34283,#34284,#34285),.UNSPECIFIED.,.F.,.F.,
(4,3,3,3,3,3,3,3,3,3,3,4),(13.8747245557601,14.2024387596921,14.6921780272677,
15.6716565624189,16.6511350975701,17.6306136327213,18.1203529002969,18.6100921678725,
19.099831435448,19.5895707030236,20.0793099705992,20.1579098629397),
 .UNSPECIFIED.);
#2836=B_SPLINE_CURVE_WITH_KNOTS('',3,(#34286,#34287,#34288,#34289,#34290,
#34291,#34292,#34293,#34294,#34295,#34296,#34297,#34298,#34299,#34300,#34301,
#34302,#34303,#34304,#34305,#34306,#34307,#34308,#34309,#34310,#34311,#34312,
#34313,#34314,#34315,#34316,#34317,#34318,#34319,#34320,#34321,#34322),
 .UNSPECIFIED.,.F.,.F.,(4,3,3,3,3,3,3,3,3,3,3,3,4),(-16.4213910178811,-15.6716565624189,
-14.6921780272677,-14.2024387596921,-13.7126994921165,-13.222960224541,
-12.7332209569654,-12.2434816893898,-11.7537424218142,-11.2640031542386,
-10.774263886663,-10.2845246190874,-10.1382057107015),.UNSPECIFIED.);
#2837=B_SPLINE_CURVE_WITH_KNOTS('',3,(#34328,#34329,#34330,#34331,#34332,
#34333,#34334,#34335,#34336,#34337,#34338,#34339,#34340,#34341,#34342,#34343,
#34344,#34345,#34346,#34347,#34348,#34349,#34350,#34351,#34352),
 .UNSPECIFIED.,.F.,.F.,(4,3,3,3,3,3,3,3,4),(-3.85502040352192,-3.42817487302914,
-2.93843560545354,-2.44869633787795,-1.95895707030236,-1.46921780272677,
-0.979478535151182,-0.489739267575592,0.),.UNSPECIFIED.);
#2838=B_SPLINE_CURVE_WITH_KNOTS('',3,(#34355,#34356,#34357,#34358,#34359,
#34360,#34361,#34362,#34363,#34364,#34365,#34366,#34367,#34368,#34369,#34370,
#34371,#34372,#34373,#34374,#34375,#34376,#34377,#34378,#34379,#34380,#34381,
#34382,#34383,#34384,#34385,#34386,#34387,#34388,#34389,#34390,#34391),
 .UNSPECIFIED.,.F.,.F.,(4,3,3,3,3,3,3,3,3,3,3,3,4),(2.02178169133309,2.44869633787795,
2.93843560545354,3.42817487302914,3.91791414060473,4.40765340818032,4.89739267575591,
5.3871319433315,5.87687121090709,6.36661047848268,6.85634974605827,7.34608901363386,
7.59153924858054),.UNSPECIFIED.);
#2839=B_SPLINE_CURVE_WITH_KNOTS('',3,(#34397,#34398,#34399,#34400,#34401,
#34402,#34403,#34404),.UNSPECIFIED.,.F.,.F.,(4,1,1,1,1,4),(40.8407044966673,
41.2372989189625,41.7270381865381,42.2167774541137,42.7065167216893,43.1962559892649),
 .UNSPECIFIED.);
#2840=B_SPLINE_CURVE_WITH_KNOTS('',3,(#34407,#34408,#34409,#34410,#34411,
#34412,#34413,#34414,#34415,#34416),.UNSPECIFIED.,.F.,.F.,(4,1,1,1,1,1,
1,4),(40.8407044966673,40.8455297756299,41.3352690432055,41.8250083107811,
42.3147475783567,42.8044868459323,43.2942261135079,43.7211407600527),
 .UNSPECIFIED.);
#2841=B_SPLINE_CURVE_WITH_KNOTS('',3,(#34421,#34422,#34423,#34424,#34425,
#34426,#34427,#34428,#34429,#34430,#34431,#34432,#34433,#34434,#34435,#34436,
#34437),.UNSPECIFIED.,.F.,.F.,(4,1,1,1,1,1,1,1,1,1,1,1,1,1,4),(34.5575191894877,
34.8706884404798,35.3604277080554,35.850166975631,36.3399062432066,36.8296455107822,
37.3193847783578,37.8091240459334,38.298863313509,38.7886025810846,39.2783418486601,
39.7680811162357,40.2578203838113,40.7475596513869,40.8407044966673),
 .UNSPECIFIED.);
#2842=B_SPLINE_CURVE_WITH_KNOTS('',3,(#34438,#34439,#34440,#34441,#34442,
#34443,#34444,#34445,#34446,#34447,#34448,#34449,#34450,#34451,#34452,#34453),
 .UNSPECIFIED.,.F.,.F.,(4,1,1,1,1,1,1,1,1,1,1,1,1,4),(34.5575191894877,
34.9686585647228,35.4583978322984,35.948137099874,36.4378763674496,36.9276156350252,
37.4173549026008,37.9070941701764,38.396833437752,38.8865727053276,39.3763119729032,
39.8660512404787,40.3557905080543,40.8407044966673),.UNSPECIFIED.);
#2843=B_SPLINE_CURVE_WITH_KNOTS('',3,(#34458,#34459,#34460,#34461,#34462,
#34463,#34464,#34465,#34466,#34467,#34468,#34469,#34470,#34471,#34472,#34473),
 .UNSPECIFIED.,.F.,.F.,(4,1,1,1,1,1,1,1,1,1,1,1,1,4),(28.2743338823081,
28.5040779619971,29.4835564971483,29.9732957647239,30.4630350322995,30.9527742998751,
31.4425135674507,31.9322528350263,32.4219921026019,32.9117313701775,33.4014706377531,
33.8912099053287,34.3809491729042,34.5575191894877),.UNSPECIFIED.);
#2844=B_SPLINE_CURVE_WITH_KNOTS('',3,(#34474,#34475,#34476,#34477,#34478,
#34479,#34480,#34481,#34482,#34483,#34484,#34485,#34486,#34487),
 .UNSPECIFIED.,.F.,.F.,(4,1,1,1,1,1,1,1,1,1,1,4),(28.2743338823081,28.6020480862402,
29.0917873538157,30.0712658889669,31.0507444241181,32.0302229592693,32.5199622268449,
33.0097014944205,33.4994407619961,33.9891800295717,34.4789192971472,34.5575191894877),
 .UNSPECIFIED.);
#2845=B_SPLINE_CURVE_WITH_KNOTS('',3,(#34492,#34493,#34494,#34495,#34496,
#34497,#34498,#34499,#34500,#34501,#34502,#34503,#34504,#34505,#34506),
 .UNSPECIFIED.,.F.,.F.,(4,1,1,1,1,1,1,1,1,1,1,1,4),(21.9911485751285,22.1374674835145,
22.6272067510901,23.1169460186656,23.6066852862412,24.0964245538168,24.5861638213924,
25.075903088968,25.5656423565436,26.0553816241192,26.5451208916948,27.524599426846,
28.2743338823081),.UNSPECIFIED.);
#2846=B_SPLINE_CURVE_WITH_KNOTS('',3,(#34507,#34508,#34509,#34510,#34511,
#34512,#34513,#34514,#34515,#34516,#34517,#34518,#34519,#34520,#34521,#34522,
#34523),.UNSPECIFIED.,.F.,.F.,(4,1,1,1,1,1,1,1,1,1,1,1,1,1,4),(21.9911485751285,
22.2354376077575,22.7251768753331,23.2149161429087,23.7046554104842,24.1943946780598,
24.6841339456354,25.173873213211,25.6636124807866,26.1533517483622,26.6430910159378,
27.1328302835134,27.622569551089,28.1123088186646,28.2743338823081),
 .UNSPECIFIED.);
#2847=B_SPLINE_CURVE_WITH_KNOTS('',3,(#34529,#34530,#34531,#34532,#34533,
#34534),.UNSPECIFIED.,.F.,.F.,(4,1,1,4),(14.399609326548,14.8893485941236,
15.3790878616992,15.707963267949),.UNSPECIFIED.);
#2848=B_SPLINE_CURVE_WITH_KNOTS('',3,(#34537,#34538,#34539,#34540,#34541,
#34542,#34543),.UNSPECIFIED.,.F.,.F.,(4,1,1,1,4),(13.8747245557601,14.301639202305,
14.7913784698806,15.2811177374562,15.707963267949),.UNSPECIFIED.);
#2849=B_SPLINE_CURVE_WITH_KNOTS('',3,(#34549,#34550,#34551,#34552,#34553,
#34554,#34555,#34556,#34557,#34558,#34559,#34560,#34561,#34562,#34563,#34564,
#34565,#34566,#34567,#34568,#34569,#34570,#34571,#34572,#34573,#34574,#34575,
#34576,#34577,#34578,#34579,#34580,#34581,#34582),.UNSPECIFIED.,.F.,.F.,
(4,3,3,3,3,3,3,3,3,3,3,4),(26.4410951701193,26.4459204490819,26.9356597166575,
27.4253989842331,27.9151382518087,28.4048775193843,28.8946167869599,29.3843560545355,
29.874095322111,30.3638345896866,30.8535738572622,31.3433131248378),
 .UNSPECIFIED.);
#2850=B_SPLINE_CURVE_WITH_KNOTS('',3,(#34586,#34587,#34588,#34589),
 .UNSPECIFIED.,.F.,.F.,(4,4),(-29.3215314335047,-28.9877616322403),
 .UNSPECIFIED.);
#2851=B_SPLINE_CURVE_WITH_KNOTS('',3,(#34593,#34594,#34595,#34596,#34597,
#34598,#34599,#34600,#34601,#34602,#34603,#34604,#34605,#34606,#34607,#34608,
#34609,#34610,#34611,#34612,#34613,#34614,#34615,#34616,#34617,#34618,#34619,
#34620,#34621,#34622,#34623,#34624,#34625,#34626,#34627,#34628,#34629,#34630,
#34631,#34632,#34633,#34634,#34635),.UNSPECIFIED.,.F.,.F.,(4,3,3,3,3,3,
3,3,3,3,3,3,3,3,4),(-28.9877616322403,-28.8946167869599,-28.4048775193843,
-27.9151382518087,-27.4253989842331,-26.9356597166575,-26.4459204490819,
-25.9561811815063,-25.4664419139307,-24.9767026463552,-24.4869633787796,
-23.997224111204,-23.5074848436284,-23.0177455760528,-22.7045763250607),
 .UNSPECIFIED.);
#2852=B_SPLINE_CURVE_WITH_KNOTS('',3,(#34640,#34641,#34642,#34643,#34644,
#34645,#34646,#34647,#34648,#34649,#34650,#34651,#34652,#34653,#34654,#34655,
#34656,#34657,#34658,#34659,#34660,#34661,#34662,#34663,#34664,#34665,#34666,
#34667,#34668,#34669,#34670,#34671,#34672,#34673,#34674,#34675,#34676,#34677,
#34678,#34679),.UNSPECIFIED.,.F.,.F.,(4,3,3,3,3,3,3,3,3,3,3,3,3,4),(20.1579098629397,
20.5690492381748,21.0587885057504,21.548527773326,22.0382670409016,22.5280063084772,
23.0177455760528,23.5074848436284,23.997224111204,24.4869633787795,24.9767026463551,
25.4664419139307,25.9561811815063,26.4410951701193),.UNSPECIFIED.);
#2853=B_SPLINE_CURVE_WITH_KNOTS('',3,(#34680,#34681,#34682,#34683,#34684,
#34685,#34686,#34687,#34688,#34689,#34690,#34691,#34692,#34693,#34694,#34695,
#34696,#34697,#34698,#34699,#34700,#34701,#34702,#34703,#34704,#34705,#34706,
#34707,#34708,#34709,#34710,#34711,#34712,#34713,#34714,#34715,#34716,#34717,
#34718,#34719),.UNSPECIFIED.,.F.,.F.,(4,3,3,3,3,3,3,3,3,3,3,3,3,4),(-22.7045763250607,
-22.5280063084772,-22.0382670409016,-21.548527773326,-21.0587885057504,
-20.5690492381748,-20.0793099705992,-19.5895707030236,-19.0998314354481,
-18.6100921678725,-18.1203529002969,-17.6306136327213,-16.6511350975701,
-16.4213910178811),.UNSPECIFIED.);
#2854=B_SPLINE_CURVE_WITH_KNOTS('',3,(#34724,#34725,#34726,#34727,#34728,
#34729,#34730,#34731,#34732,#34733,#34734,#34735,#34736,#34737,#34738,#34739,
#34740,#34741,#34742,#34743,#34744,#34745,#34746,#34747,#34748,#34749,#34750,
#34751,#34752,#34753,#34754,#34755,#34756,#34757),.UNSPECIFIED.,.F.,.F.,
(4,3,3,3,3,3,3,3,3,3,3,4),(13.8747245557601,14.2024387596921,14.6921780272677,
15.6716565624189,16.6511350975701,17.6306136327213,18.1203529002969,18.6100921678725,
19.0998314354481,19.5895707030236,20.0793099705992,20.1579098629397),
 .UNSPECIFIED.);
#2855=B_SPLINE_CURVE_WITH_KNOTS('',3,(#34758,#34759,#34760,#34761,#34762,
#34763,#34764,#34765,#34766,#34767,#34768,#34769,#34770,#34771,#34772,#34773,
#34774,#34775,#34776,#34777,#34778,#34779,#34780,#34781,#34782,#34783,#34784,
#34785,#34786,#34787,#34788,#34789,#34790,#34791,#34792,#34793,#34794),
 .UNSPECIFIED.,.F.,.F.,(4,3,3,3,3,3,3,3,3,3,3,3,4),(-16.4213910178811,-15.6716565624189,
-14.6921780272677,-14.2024387596921,-13.7126994921165,-13.222960224541,
-12.7332209569654,-12.2434816893898,-11.7537424218142,-11.2640031542386,
-10.774263886663,-10.2845246190874,-10.1382057107015),.UNSPECIFIED.);
#2856=B_SPLINE_CURVE_WITH_KNOTS('',3,(#34800,#34801,#34802,#34803,#34804,
#34805,#34806,#34807,#34808,#34809,#34810,#34811,#34812,#34813,#34814,#34815,
#34816,#34817,#34818,#34819,#34820,#34821,#34822,#34823,#34824),
 .UNSPECIFIED.,.F.,.F.,(4,3,3,3,3,3,3,3,4),(-3.85502040352192,-3.42817487302914,
-2.93843560545355,-2.44869633787795,-1.95895707030236,-1.46921780272677,
-0.979478535151183,-0.489739267575592,0.),.UNSPECIFIED.);
#2857=B_SPLINE_CURVE_WITH_KNOTS('',3,(#34827,#34828,#34829,#34830,#34831,
#34832,#34833,#34834,#34835,#34836,#34837,#34838,#34839,#34840,#34841,#34842,
#34843,#34844,#34845,#34846,#34847,#34848,#34849,#34850,#34851,#34852,#34853,
#34854,#34855,#34856,#34857,#34858,#34859,#34860,#34861,#34862,#34863),
 .UNSPECIFIED.,.F.,.F.,(4,3,3,3,3,3,3,3,3,3,3,3,4),(2.02178169133308,2.44869633787795,
2.93843560545355,3.42817487302914,3.91791414060473,4.40765340818032,4.89739267575591,
5.3871319433315,5.87687121090709,6.36661047848268,6.85634974605827,7.34608901363386,
7.59153924858054),.UNSPECIFIED.);
#2858=B_SPLINE_CURVE_WITH_KNOTS('',3,(#34869,#34870,#34871,#34872,#34873,
#34874,#34875,#34876),.UNSPECIFIED.,.F.,.F.,(4,1,1,1,1,4),(40.8407044966673,
41.2372989189625,41.7270381865381,42.2167774541137,42.7065167216893,43.1962559892649),
 .UNSPECIFIED.);
#2859=B_SPLINE_CURVE_WITH_KNOTS('',3,(#34879,#34880,#34881,#34882,#34883,
#34884,#34885,#34886,#34887,#34888),.UNSPECIFIED.,.F.,.F.,(4,1,1,1,1,1,
1,4),(40.8407044966673,40.8455297756299,41.3352690432055,41.8250083107811,
42.3147475783567,42.8044868459323,43.2942261135079,43.7211407600527),
 .UNSPECIFIED.);
#2860=B_SPLINE_CURVE_WITH_KNOTS('',3,(#34893,#34894,#34895,#34896,#34897,
#34898,#34899,#34900,#34901,#34902,#34903,#34904,#34905,#34906,#34907,#34908,
#34909),.UNSPECIFIED.,.F.,.F.,(4,1,1,1,1,1,1,1,1,1,1,1,1,1,4),(34.5575191894877,
34.8706884404798,35.3604277080554,35.850166975631,36.3399062432066,36.8296455107822,
37.3193847783578,37.8091240459334,38.298863313509,38.7886025810846,39.2783418486601,
39.7680811162357,40.2578203838113,40.7475596513869,40.8407044966673),
 .UNSPECIFIED.);
#2861=B_SPLINE_CURVE_WITH_KNOTS('',3,(#34910,#34911,#34912,#34913,#34914,
#34915,#34916,#34917,#34918,#34919,#34920,#34921,#34922,#34923,#34924,#34925),
 .UNSPECIFIED.,.F.,.F.,(4,1,1,1,1,1,1,1,1,1,1,1,1,4),(34.5575191894877,
34.9686585647228,35.4583978322984,35.948137099874,36.4378763674496,36.9276156350252,
37.4173549026008,37.9070941701764,38.396833437752,38.8865727053276,39.3763119729032,
39.8660512404787,40.3557905080543,40.8407044966673),.UNSPECIFIED.);
#2862=B_SPLINE_CURVE_WITH_KNOTS('',3,(#34930,#34931,#34932,#34933,#34934,
#34935,#34936,#34937,#34938,#34939,#34940,#34941,#34942,#34943,#34944,#34945),
 .UNSPECIFIED.,.F.,.F.,(4,1,1,1,1,1,1,1,1,1,1,1,1,4),(28.2743338823081,
28.5040779619971,29.4835564971483,29.9732957647239,30.4630350322995,30.9527742998751,
31.4425135674507,31.9322528350263,32.4219921026019,32.9117313701775,33.4014706377531,
33.8912099053287,34.3809491729042,34.5575191894877),.UNSPECIFIED.);
#2863=B_SPLINE_CURVE_WITH_KNOTS('',3,(#34946,#34947,#34948,#34949,#34950,
#34951,#34952,#34953,#34954,#34955,#34956,#34957,#34958,#34959),
 .UNSPECIFIED.,.F.,.F.,(4,1,1,1,1,1,1,1,1,1,1,4),(28.2743338823081,28.6020480862402,
29.0917873538157,30.0712658889669,31.0507444241181,32.0302229592693,32.5199622268449,
33.0097014944205,33.4994407619961,33.9891800295717,34.4789192971472,34.5575191894877),
 .UNSPECIFIED.);
#2864=B_SPLINE_CURVE_WITH_KNOTS('',3,(#34964,#34965,#34966,#34967,#34968,
#34969,#34970,#34971,#34972,#34973,#34974,#34975,#34976,#34977,#34978),
 .UNSPECIFIED.,.F.,.F.,(4,1,1,1,1,1,1,1,1,1,1,1,4),(21.9911485751285,22.1374674835145,
22.6272067510901,23.1169460186656,23.6066852862412,24.0964245538168,24.5861638213924,
25.075903088968,25.5656423565436,26.0553816241192,26.5451208916948,27.524599426846,
28.2743338823081),.UNSPECIFIED.);
#2865=B_SPLINE_CURVE_WITH_KNOTS('',3,(#34979,#34980,#34981,#34982,#34983,
#34984,#34985,#34986,#34987,#34988,#34989,#34990,#34991,#34992,#34993,#34994,
#34995),.UNSPECIFIED.,.F.,.F.,(4,1,1,1,1,1,1,1,1,1,1,1,1,1,4),(21.9911485751285,
22.2354376077575,22.7251768753331,23.2149161429087,23.7046554104842,24.1943946780598,
24.6841339456354,25.173873213211,25.6636124807866,26.1533517483622,26.6430910159378,
27.1328302835134,27.622569551089,28.1123088186646,28.2743338823081),
 .UNSPECIFIED.);
#2866=B_SPLINE_CURVE_WITH_KNOTS('',3,(#35001,#35002,#35003,#35004,#35005,
#35006),.UNSPECIFIED.,.F.,.F.,(4,1,1,4),(14.399609326548,14.8893485941236,
15.3790878616992,15.707963267949),.UNSPECIFIED.);
#2867=B_SPLINE_CURVE_WITH_KNOTS('',3,(#35009,#35010,#35011,#35012,#35013,
#35014,#35015),.UNSPECIFIED.,.F.,.F.,(4,1,1,1,4),(13.8747245557601,14.301639202305,
14.7913784698806,15.2811177374562,15.707963267949),.UNSPECIFIED.);
#2868=B_SPLINE_CURVE_WITH_KNOTS('',3,(#35021,#35022,#35023,#35024,#35025,
#35026,#35027,#35028,#35029,#35030,#35031,#35032,#35033,#35034,#35035,#35036,
#35037,#35038,#35039,#35040,#35041,#35042,#35043,#35044,#35045,#35046,#35047,
#35048,#35049,#35050,#35051,#35052,#35053,#35054),.UNSPECIFIED.,.F.,.F.,
(4,3,3,3,3,3,3,3,3,3,3,4),(26.4410951701193,26.4459204490819,26.9356597166575,
27.4253989842331,27.9151382518087,28.4048775193843,28.8946167869599,29.3843560545355,
29.874095322111,30.3638345896866,30.8535738572622,31.3433131248378),
 .UNSPECIFIED.);
#2869=B_SPLINE_CURVE_WITH_KNOTS('',3,(#35058,#35059,#35060,#35061),
 .UNSPECIFIED.,.F.,.F.,(4,4),(-29.3215314335047,-28.9877616322403),
 .UNSPECIFIED.);
#2870=B_SPLINE_CURVE_WITH_KNOTS('',3,(#35065,#35066,#35067,#35068,#35069,
#35070,#35071,#35072,#35073,#35074,#35075,#35076,#35077,#35078,#35079,#35080,
#35081,#35082,#35083,#35084,#35085,#35086,#35087,#35088,#35089,#35090,#35091,
#35092,#35093,#35094,#35095,#35096,#35097,#35098,#35099,#35100,#35101,#35102,
#35103,#35104,#35105,#35106,#35107),.UNSPECIFIED.,.F.,.F.,(4,3,3,3,3,3,
3,3,3,3,3,3,3,3,4),(-28.9877616322403,-28.8946167869599,-28.4048775193843,
-27.9151382518087,-27.4253989842331,-26.9356597166575,-26.4459204490819,
-25.9561811815063,-25.4664419139307,-24.9767026463552,-24.4869633787796,
-23.997224111204,-23.5074848436284,-23.0177455760528,-22.7045763250607),
 .UNSPECIFIED.);
#2871=B_SPLINE_CURVE_WITH_KNOTS('',3,(#35112,#35113,#35114,#35115,#35116,
#35117,#35118,#35119,#35120,#35121,#35122,#35123,#35124,#35125,#35126,#35127,
#35128,#35129,#35130,#35131,#35132,#35133,#35134,#35135,#35136,#35137,#35138,
#35139,#35140,#35141,#35142,#35143,#35144,#35145,#35146,#35147,#35148,#35149,
#35150,#35151),.UNSPECIFIED.,.F.,.F.,(4,3,3,3,3,3,3,3,3,3,3,3,3,4),(20.1579098629397,
20.5690492381748,21.0587885057504,21.548527773326,22.0382670409016,22.5280063084772,
23.0177455760528,23.5074848436284,23.997224111204,24.4869633787796,24.9767026463551,
25.4664419139307,25.9561811815063,26.4410951701193),.UNSPECIFIED.);
#2872=B_SPLINE_CURVE_WITH_KNOTS('',3,(#35152,#35153,#35154,#35155,#35156,
#35157,#35158,#35159,#35160,#35161,#35162,#35163,#35164,#35165,#35166,#35167,
#35168,#35169,#35170,#35171,#35172,#35173,#35174,#35175,#35176,#35177,#35178,
#35179,#35180,#35181,#35182,#35183,#35184,#35185,#35186,#35187,#35188,#35189,
#35190,#35191),.UNSPECIFIED.,.F.,.F.,(4,3,3,3,3,3,3,3,3,3,3,3,3,4),(-22.7045763250607,
-22.5280063084772,-22.0382670409016,-21.548527773326,-21.0587885057504,
-20.5690492381748,-20.0793099705992,-19.5895707030236,-19.0998314354481,
-18.6100921678725,-18.1203529002969,-17.6306136327213,-16.6511350975701,
-16.4213910178811),.UNSPECIFIED.);
#2873=B_SPLINE_CURVE_WITH_KNOTS('',3,(#35196,#35197,#35198,#35199,#35200,
#35201,#35202,#35203,#35204,#35205,#35206,#35207,#35208,#35209,#35210,#35211,
#35212,#35213,#35214,#35215,#35216,#35217,#35218,#35219,#35220,#35221,#35222,
#35223,#35224,#35225,#35226,#35227,#35228,#35229),.UNSPECIFIED.,.F.,.F.,
(4,3,3,3,3,3,3,3,3,3,3,4),(13.8747245557601,14.2024387596921,14.6921780272677,
15.6716565624189,16.6511350975701,17.6306136327213,18.1203529002969,18.6100921678725,
19.0998314354481,19.5895707030236,20.0793099705992,20.1579098629397),
 .UNSPECIFIED.);
#2874=B_SPLINE_CURVE_WITH_KNOTS('',3,(#35230,#35231,#35232,#35233,#35234,
#35235,#35236,#35237,#35238,#35239,#35240,#35241,#35242,#35243,#35244,#35245,
#35246,#35247,#35248,#35249,#35250,#35251,#35252,#35253,#35254,#35255,#35256,
#35257,#35258,#35259,#35260,#35261,#35262,#35263,#35264,#35265,#35266),
 .UNSPECIFIED.,.F.,.F.,(4,3,3,3,3,3,3,3,3,3,3,3,4),(-16.4213910178811,-15.6716565624189,
-14.6921780272677,-14.2024387596921,-13.7126994921165,-13.222960224541,
-12.7332209569654,-12.2434816893898,-11.7537424218142,-11.2640031542386,
-10.774263886663,-10.2845246190874,-10.1382057107015),.UNSPECIFIED.);
#2875=B_SPLINE_CURVE_WITH_KNOTS('',3,(#35272,#35273,#35274,#35275,#35276,
#35277,#35278,#35279,#35280,#35281,#35282,#35283,#35284,#35285,#35286,#35287,
#35288,#35289,#35290,#35291,#35292,#35293,#35294,#35295,#35296),
 .UNSPECIFIED.,.F.,.F.,(4,3,3,3,3,3,3,3,4),(-3.85502040352192,-3.42817487302914,
-2.93843560545355,-2.44869633787795,-1.95895707030236,-1.46921780272677,
-0.979478535151183,-0.489739267575592,0.),.UNSPECIFIED.);
#2876=B_SPLINE_CURVE_WITH_KNOTS('',3,(#35299,#35300,#35301,#35302,#35303,
#35304,#35305,#35306,#35307,#35308,#35309,#35310,#35311,#35312,#35313,#35314,
#35315,#35316,#35317,#35318,#35319,#35320,#35321,#35322,#35323,#35324,#35325,
#35326,#35327,#35328,#35329,#35330,#35331,#35332,#35333,#35334,#35335),
 .UNSPECIFIED.,.F.,.F.,(4,3,3,3,3,3,3,3,3,3,3,3,4),(2.02178169133309,2.44869633787795,
2.93843560545355,3.42817487302914,3.91791414060473,4.40765340818032,4.89739267575591,
5.3871319433315,5.87687121090709,6.36661047848268,6.85634974605827,7.34608901363386,
7.59153924858054),.UNSPECIFIED.);
#2877=B_SPLINE_CURVE_WITH_KNOTS('',3,(#35341,#35342,#35343,#35344,#35345,
#35346,#35347,#35348),.UNSPECIFIED.,.F.,.F.,(4,1,1,1,1,4),(40.8407044966673,
41.2372989189625,41.7270381865381,42.2167774541137,42.7065167216893,43.1962559892649),
 .UNSPECIFIED.);
#2878=B_SPLINE_CURVE_WITH_KNOTS('',3,(#35351,#35352,#35353,#35354,#35355,
#35356,#35357,#35358,#35359,#35360),.UNSPECIFIED.,.F.,.F.,(4,1,1,1,1,1,
1,4),(40.8407044966673,40.8455297756299,41.3352690432055,41.8250083107811,
42.3147475783567,42.8044868459323,43.2942261135079,43.7211407600527),
 .UNSPECIFIED.);
#2879=B_SPLINE_CURVE_WITH_KNOTS('',3,(#35365,#35366,#35367,#35368,#35369,
#35370,#35371,#35372,#35373,#35374,#35375,#35376,#35377,#35378,#35379,#35380,
#35381),.UNSPECIFIED.,.F.,.F.,(4,1,1,1,1,1,1,1,1,1,1,1,1,1,4),(34.5575191894877,
34.8706884404798,35.3604277080554,35.850166975631,36.3399062432066,36.8296455107822,
37.3193847783578,37.8091240459334,38.298863313509,38.7886025810846,39.2783418486601,
39.7680811162357,40.2578203838113,40.7475596513869,40.8407044966673),
 .UNSPECIFIED.);
#2880=B_SPLINE_CURVE_WITH_KNOTS('',3,(#35382,#35383,#35384,#35385,#35386,
#35387,#35388,#35389,#35390,#35391,#35392,#35393,#35394,#35395,#35396,#35397),
 .UNSPECIFIED.,.F.,.F.,(4,1,1,1,1,1,1,1,1,1,1,1,1,4),(34.5575191894877,
34.9686585647228,35.4583978322984,35.948137099874,36.4378763674496,36.9276156350252,
37.4173549026008,37.9070941701764,38.396833437752,38.8865727053276,39.3763119729032,
39.8660512404787,40.3557905080543,40.8407044966673),.UNSPECIFIED.);
#2881=B_SPLINE_CURVE_WITH_KNOTS('',3,(#35402,#35403,#35404,#35405,#35406,
#35407,#35408,#35409,#35410,#35411,#35412,#35413,#35414,#35415,#35416,#35417),
 .UNSPECIFIED.,.F.,.F.,(4,1,1,1,1,1,1,1,1,1,1,1,1,4),(28.2743338823081,
28.5040779619971,29.4835564971483,29.9732957647239,30.4630350322995,30.9527742998751,
31.4425135674507,31.9322528350263,32.4219921026019,32.9117313701775,33.4014706377531,
33.8912099053287,34.3809491729042,34.5575191894877),.UNSPECIFIED.);
#2882=B_SPLINE_CURVE_WITH_KNOTS('',3,(#35418,#35419,#35420,#35421,#35422,
#35423,#35424,#35425,#35426,#35427,#35428,#35429,#35430,#35431),
 .UNSPECIFIED.,.F.,.F.,(4,1,1,1,1,1,1,1,1,1,1,4),(28.2743338823081,28.6020480862402,
29.0917873538157,30.0712658889669,31.0507444241181,32.0302229592693,32.5199622268449,
33.0097014944205,33.4994407619961,33.9891800295717,34.4789192971472,34.5575191894877),
 .UNSPECIFIED.);
#2883=B_SPLINE_CURVE_WITH_KNOTS('',3,(#35436,#35437,#35438,#35439,#35440,
#35441,#35442,#35443,#35444,#35445,#35446,#35447,#35448,#35449,#35450),
 .UNSPECIFIED.,.F.,.F.,(4,1,1,1,1,1,1,1,1,1,1,1,4),(21.9911485751285,22.1374674835145,
22.6272067510901,23.1169460186656,23.6066852862412,24.0964245538168,24.5861638213924,
25.075903088968,25.5656423565436,26.0553816241192,26.5451208916948,27.524599426846,
28.2743338823081),.UNSPECIFIED.);
#2884=B_SPLINE_CURVE_WITH_KNOTS('',3,(#35451,#35452,#35453,#35454,#35455,
#35456,#35457,#35458,#35459,#35460,#35461,#35462,#35463,#35464,#35465,#35466,
#35467),.UNSPECIFIED.,.F.,.F.,(4,1,1,1,1,1,1,1,1,1,1,1,1,1,4),(21.9911485751285,
22.2354376077575,22.7251768753331,23.2149161429087,23.7046554104842,24.1943946780598,
24.6841339456354,25.173873213211,25.6636124807866,26.1533517483622,26.6430910159378,
27.1328302835134,27.622569551089,28.1123088186646,28.2743338823081),
 .UNSPECIFIED.);
#2885=B_SPLINE_CURVE_WITH_KNOTS('',3,(#35473,#35474,#35475,#35476,#35477,
#35478),.UNSPECIFIED.,.F.,.F.,(4,1,1,4),(14.399609326548,14.8893485941236,
15.3790878616992,15.707963267949),.UNSPECIFIED.);
#2886=B_SPLINE_CURVE_WITH_KNOTS('',3,(#35481,#35482,#35483,#35484,#35485,
#35486,#35487),.UNSPECIFIED.,.F.,.F.,(4,1,1,1,4),(13.8747245557601,14.301639202305,
14.7913784698806,15.2811177374562,15.707963267949),.UNSPECIFIED.);
#2887=B_SPLINE_CURVE_WITH_KNOTS('',3,(#35489,#35490,#35491,#35492,#35493,
#35494,#35495,#35496,#35497,#35498,#35499,#35500,#35501,#35502,#35503,#35504,
#35505,#35506,#35507,#35508,#35509,#35510,#35511,#35512,#35513,#35514,#35515,
#35516,#35517,#35518,#35519,#35520,#35521,#35522,#35523,#35524,#35525,#35526,
#35527,#35528,#35529,#35530,#35531,#35532,#35533,#35534,#35535,#35536,#35537,
#35538,#35539,#35540,#35541,#35542,#35543,#35544,#35545,#35546,#35547,#35548,
#35549,#35550,#35551,#35552,#35553,#35554,#35555,#35556,#35557,#35558,#35559,
#35560,#35561,#35562,#35563,#35564,#35565,#35566,#35567,#35568,#35569,#35570,
#35571,#35572,#35573,#35574,#35575,#35576,#35577,#35578,#35579,#35580,#35581,
#35582,#35583,#35584,#35585,#35586,#35587,#35588,#35589,#35590,#35591,#35592,
#35593,#35594,#35595,#35596,#35597),.UNSPECIFIED.,.F.,.F.,(4,3,3,3,3,3,
3,3,3,3,3,3,3,3,3,3,3,3,3,3,3,3,3,3,3,3,3,3,3,3,3,3,3,3,3,3,4),(-0.954382097139102,
-0.915485219868088,-0.876011359398878,-0.858387716138701,-0.851290445572933,
-0.844232875542686,-0.803962784587969,-0.771371663532114,-0.755076103004186,
-0.74670724096049,-0.740703076045499,-0.738780542476259,-0.698754803213944,
-0.658013337818404,-0.616748686984212,-0.590809554692081,-0.56947683727088,
-0.564087732187264,-0.52197879042965,-0.512992157815691,-0.47126838346612,
-0.429066795270051,-0.391147230446158,-0.385001282265118,-0.379585400739026,
-0.33663022313337,-0.293213566977487,-0.277388535974477,-0.234198210308746,
-0.208936638957807,-0.199293375270686,-0.191586968622297,-0.147662130465962,
-0.103303648130549,-0.0589022233416743,-0.0321056395012393,0.),
 .UNSPECIFIED.);
#2888=B_SPLINE_CURVE_WITH_KNOTS('',3,(#35598,#35599,#35600,#35601,#35602,
#35603,#35604,#35605,#35606,#35607,#35608,#35609,#35610,#35611,#35612,#35613,
#35614,#35615,#35616,#35617,#35618,#35619,#35620,#35621,#35622,#35623,#35624,
#35625,#35626,#35627,#35628,#35629,#35630,#35631,#35632,#35633,#35634,#35635,
#35636,#35637,#35638,#35639,#35640,#35641,#35642,#35643,#35644,#35645,#35646,
#35647,#35648,#35649,#35650,#35651,#35652,#35653,#35654,#35655,#35656,#35657,
#35658,#35659,#35660,#35661,#35662,#35663,#35664,#35665,#35666,#35667,#35668,
#35669,#35670,#35671,#35672,#35673,#35674,#35675,#35676,#35677,#35678,#35679,
#35680,#35681,#35682,#35683,#35684,#35685,#35686,#35687,#35688,#35689,#35690,
#35691,#35692,#35693,#35694,#35695,#35696,#35697,#35698,#35699,#35700,#35701,
#35702,#35703,#35704,#35705,#35706,#35707,#35708,#35709),.UNSPECIFIED.,
 .F.,.F.,(4,3,3,3,3,3,3,3,3,3,3,3,3,3,3,3,3,3,3,3,3,3,3,3,3,3,3,3,3,3,3,
3,3,3,3,3,3,4),(-0.950777871811376,-0.906311283561082,-0.86180398566132,
-0.842287018017892,-0.832349797485745,-0.825106830080676,-0.781341119219643,
-0.743504681866769,-0.724586463190332,-0.715675956496024,-0.707599455142323,
-0.705668244513895,-0.662940062790035,-0.619927849095546,-0.577350782543376,
-0.550469628354302,-0.530308762712497,-0.524965684945637,-0.519443984453863,
-0.477671746282991,-0.469826165787081,-0.427882412217812,-0.386078816922957,
-0.350449958940854,-0.344039953632224,-0.338265645217358,-0.297454287905639,
-0.257005929493181,-0.243563384994542,-0.202803272714803,-0.180830798401061,
-0.172157453857976,-0.165074010527136,-0.125309029605361,-0.0856893299734917,
-0.0467731925692476,-0.0270234782048685,0.),.UNSPECIFIED.);
#2889=B_SPLINE_CURVE_WITH_KNOTS('',3,(#35711,#35712,#35713,#35714,#35715,
#35716,#35717,#35718,#35719,#35720,#35721,#35722,#35723,#35724,#35725,#35726,
#35727),.UNSPECIFIED.,.F.,.F.,(4,1,1,1,1,1,1,1,1,1,1,1,1,1,4),(15.707963267949,
15.7708570050318,16.2605962726074,16.750335540183,17.2400748077586,17.7298140753341,
18.2195533429097,18.7092926104853,19.1990318780609,19.6887711456365,20.1785104132121,
20.6682496807877,21.1579889483633,21.6477282159389,21.9911485751285),
 .UNSPECIFIED.);
#2890=B_SPLINE_CURVE_WITH_KNOTS('',3,(#35728,#35729,#35730,#35731,#35732,
#35733,#35734,#35735,#35736,#35737,#35738,#35739,#35740,#35741,#35742,#35743,
#35744),.UNSPECIFIED.,.F.,.F.,(4,1,1,1,1,1,1,1,1,1,1,1,1,1,4),(15.707963267949,
15.8688271292748,16.3585663968504,16.848305664426,17.3380449320016,17.8277841995772,
18.3175234671527,18.8072627347283,19.2970020023039,19.7867412698795,20.2764805374551,
20.7662198050307,21.2559590726063,21.7456983401819,21.9911485751285),
 .UNSPECIFIED.);
#2891=B_SPLINE_CURVE_WITH_KNOTS('',3,(#36001,#36002,#36003,#36004,#36005,
#36006,#36007,#36008,#36009,#36010,#36011,#36012,#36013,#36014,#36015,#36016,
#36017,#36018,#36019,#36020,#36021,#36022,#36023,#36024,#36025,#36026,#36027,
#36028,#36029,#36030,#36031,#36032,#36033,#36034,#36035,#36036,#36037,#36038,
#36039,#36040,#36041,#36042,#36043,#36044,#36045,#36046,#36047,#36048,#36049,
#36050,#36051,#36052,#36053,#36054,#36055,#36056,#36057,#36058,#36059,#36060,
#36061,#36062,#36063,#36064,#36065,#36066,#36067,#36068,#36069,#36070,#36071,
#36072,#36073,#36074,#36075,#36076,#36077,#36078,#36079,#36080,#36081,#36082,
#36083,#36084,#36085,#36086,#36087,#36088,#36089,#36090,#36091,#36092,#36093,
#36094,#36095,#36096,#36097,#36098,#36099,#36100,#36101,#36102,#36103,#36104,
#36105,#36106),.UNSPECIFIED.,.F.,.F.,(4,3,3,3,3,3,3,3,3,3,3,3,3,3,3,3,3,
3,3,3,3,3,3,3,3,3,3,3,3,3,3,3,3,3,3,4),(0.,0.0384977089125158,0.0777077350623172,
0.117481174077728,0.157167741411488,0.165169712071236,0.172509866250956,
0.215216950964984,0.255388062329607,0.296070379047766,0.332110061722789,
0.341131635592327,0.34758681189835,0.389053063764889,0.430985757208201,
0.440229109747859,0.481905267093181,0.506030612217038,0.51916002073821,
0.524507558309914,0.530100422386233,0.57258610074797,0.615488329040074,
0.658430771840619,0.674908028084036,0.705394548776867,0.711667703485966,
0.718009631396055,0.761258294065309,0.800643768955652,0.821412106017802,
0.829287077220563,0.837097365220166,0.881633892178726,0.918800193626682,
0.950777871811493),.UNSPECIFIED.);
#2892=B_SPLINE_CURVE_WITH_KNOTS('',3,(#36107,#36108,#36109,#36110,#36111,
#36112,#36113,#36114,#36115,#36116,#36117,#36118,#36119,#36120,#36121,#36122,
#36123,#36124,#36125,#36126,#36127,#36128,#36129,#36130,#36131,#36132,#36133,
#36134,#36135,#36136,#36137,#36138,#36139,#36140,#36141,#36142,#36143,#36144,
#36145,#36146,#36147,#36148,#36149),.UNSPECIFIED.,.F.,.F.,(4,3,3,3,3,3,
3,3,3,3,3,3,3,3,4),(-10.1382057107015,-9.79478535151183,-9.30504608393623,
-8.81530681636064,-8.32556754878505,-7.83582828120946,-7.34608901363387,
-6.85634974605828,-6.36661047848269,-5.87687121090709,-5.3871319433315,
-4.89739267575591,-4.40765340818032,-3.91791414060473,-3.85502040352192),
 .UNSPECIFIED.);
#2893=B_SPLINE_CURVE_WITH_KNOTS('',3,(#36406,#36407,#36408,#36409,#36410,
#36411,#36412,#36413,#36414,#36415,#36416,#36417,#36418,#36419,#36420,#36421,
#36422,#36423,#36424,#36425,#36426,#36427,#36428,#36429,#36430,#36431,#36432,
#36433,#36434,#36435,#36436,#36437,#36438,#36439,#36440,#36441,#36442,#36443,
#36444,#36445,#36446,#36447,#36448),.UNSPECIFIED.,.F.,.F.,(4,3,3,3,3,3,
3,3,3,3,3,3,3,3,4),(7.59153924858054,7.83582828120946,8.32556754878505,
8.81530681636064,9.30504608393623,9.79478535151182,10.2845246190874,10.774263886663,
11.2640031542386,11.7537424218142,12.2434816893898,12.7332209569654,13.222960224541,
13.7126994921165,13.8747245557601),.UNSPECIFIED.);
#2894=B_SPLINE_CURVE_WITH_KNOTS('',3,(#36449,#36450,#36451,#36452,#36453,
#36454,#36455,#36456,#36457,#36458,#36459,#36460,#36461,#36462,#36463,#36464,
#36465,#36466,#36467,#36468,#36469,#36470,#36471,#36472,#36473,#36474,#36475,
#36476,#36477,#36478,#36479,#36480,#36481,#36482,#36483,#36484,#36485,#36486,
#36487,#36488,#36489,#36490,#36491,#36492,#36493,#36494,#36495,#36496,#36497,
#36498,#36499,#36500,#36501,#36502,#36503,#36504,#36505,#36506,#36507,#36508,
#36509,#36510,#36511,#36512,#36513,#36514,#36515,#36516,#36517,#36518,#36519,
#36520,#36521,#36522,#36523,#36524,#36525,#36526,#36527,#36528,#36529,#36530,
#36531,#36532,#36533,#36534,#36535,#36536,#36537,#36538,#36539,#36540,#36541,
#36542,#36543,#36544,#36545,#36546,#36547,#36548,#36549,#36550,#36551),
 .UNSPECIFIED.,.F.,.F.,(4,3,3,3,3,3,3,3,3,3,3,3,3,3,3,3,3,3,3,3,3,3,3,3,
3,3,3,3,3,3,3,3,3,3,4),(0.,0.0441184545897234,0.0885852303427278,0.132705881239172,
0.176248827766947,0.188641766735101,0.194919743535348,0.201110164739286,
0.246435079457907,0.289836405211179,0.333162204589208,0.37069232129194,
0.380555088969513,0.388891713726302,0.431181300092753,0.473131877202055,
0.483282671400137,0.525568063027558,0.54867105757415,0.563330516703862,
0.568979423171459,0.610227610749445,0.651359426261816,0.691816928157437,
0.710392019400299,0.737503640980283,0.744688179095465,0.751191992318133,
0.79162882737332,0.825542868540032,0.845308948087482,0.852099049520499,
0.89146337026381,0.927284992040167,0.954382097139104),.UNSPECIFIED.);
#2895=B_SPLINE_CURVE_WITH_KNOTS('',3,(#36554,#36555,#36556,#36557,#36558,
#36559,#36560,#36561,#36562,#36563,#36564,#36565,#36566,#36567,#36568,#36569,
#36570,#36571,#36572,#36573,#36574,#36575,#36576,#36577,#36578,#36579,#36580,
#36581,#36582,#36583,#36584,#36585,#36586,#36587,#36588,#36589,#36590,#36591,
#36592,#36593,#36594,#36595,#36596,#36597,#36598,#36599,#36600,#36601,#36602,
#36603,#36604,#36605,#36606,#36607,#36608,#36609,#36610,#36611,#36612,#36613,
#36614,#36615,#36616,#36617,#36618,#36619,#36620,#36621,#36622,#36623,#36624,
#36625,#36626,#36627,#36628,#36629,#36630,#36631,#36632,#36633,#36634,#36635,
#36636,#36637,#36638,#36639,#36640,#36641,#36642,#36643,#36644,#36645,#36646,
#36647,#36648,#36649,#36650,#36651,#36652,#36653,#36654,#36655,#36656,#36657,
#36658,#36659,#36660,#36661,#36662),.UNSPECIFIED.,.F.,.F.,(4,3,3,3,3,3,
3,3,3,3,3,3,3,3,3,3,3,3,3,3,3,3,3,3,3,3,3,3,3,3,3,3,3,3,3,3,4),(-0.954382097139068,
-0.915485230776449,-0.876011377695649,-0.858387741528348,-0.851290401489917,
-0.844232864888672,-0.803962779602644,-0.771371661039454,-0.755076101757858,
-0.746707237711699,-0.740703072512022,-0.738780542476263,-0.698754793624434,
-0.658013320988911,-0.616748667997841,-0.590809540452306,-0.569476809965562,
-0.564087700718665,-0.521978753994884,-0.512992157815699,-0.471268385903021,
-0.429066799073804,-0.391147233298974,-0.385001285630552,-0.379585401384325,
-0.33663022579062,-0.293213570311272,-0.277388535974486,-0.234198210334854,
-0.208936638980652,-0.199293375267056,-0.191586968611106,-0.147662130367022,
-0.103303648093833,-0.058902223280959,-0.0321056395012389,0.),
 .UNSPECIFIED.);
#2896=B_SPLINE_CURVE_WITH_KNOTS('',3,(#36663,#36664,#36665,#36666,#36667,
#36668,#36669,#36670,#36671,#36672,#36673,#36674,#36675,#36676,#36677,#36678,
#36679,#36680,#36681,#36682,#36683,#36684,#36685,#36686,#36687,#36688,#36689,
#36690,#36691,#36692,#36693,#36694,#36695,#36696,#36697,#36698,#36699,#36700,
#36701,#36702,#36703,#36704,#36705,#36706,#36707,#36708,#36709,#36710,#36711,
#36712,#36713,#36714,#36715,#36716,#36717,#36718,#36719,#36720,#36721,#36722,
#36723,#36724,#36725,#36726,#36727,#36728,#36729,#36730,#36731,#36732,#36733,
#36734,#36735,#36736,#36737,#36738,#36739,#36740,#36741,#36742,#36743,#36744,
#36745,#36746,#36747,#36748,#36749,#36750,#36751,#36752,#36753,#36754,#36755,
#36756,#36757,#36758,#36759,#36760,#36761,#36762,#36763,#36764,#36765,#36766,
#36767,#36768,#36769,#36770,#36771,#36772,#36773,#36774),.UNSPECIFIED.,
 .F.,.F.,(4,3,3,3,3,3,3,3,3,3,3,3,3,3,3,3,3,3,3,3,3,3,3,3,3,3,3,3,3,3,3,
3,3,3,3,3,3,4),(-0.950777871811448,-0.906311270744792,-0.861803977893823,
-0.842287011221341,-0.832349777444776,-0.825106814972194,-0.781341114085539,
-0.743504679299753,-0.72458646190686,-0.715675954522707,-0.70759945509899,
-0.705668244513967,-0.662940076465589,-0.619927866635559,-0.577350796294309,
-0.550469638667513,-0.530308770447415,-0.524965697973984,-0.519443987026582,
-0.477671747191907,-0.469826165787123,-0.427882411307492,-0.386078815571722,
-0.350449957927431,-0.344039951609201,-0.338265644735927,-0.297454287004672,
-0.25700592740343,-0.243563384994556,-0.202803273177456,-0.180830798805883,
-0.172157454950964,-0.165074010626906,-0.125309029570385,-0.0856893307960596,
-0.0467731959717267,-0.0270234782048714,0.),.UNSPECIFIED.);
#2897=B_SPLINE_CURVE_WITH_KNOTS('',3,(#36776,#36777,#36778,#36779,#36780,
#36781,#36782,#36783,#36784,#36785,#36786,#36787,#36788,#36789,#36790,#36791,
#36792),.UNSPECIFIED.,.F.,.F.,(4,1,1,1,1,1,1,1,1,1,1,1,1,1,4),(15.707963267949,
15.7708570050318,16.2605962726074,16.750335540183,17.2400748077586,17.7298140753341,
18.2195533429097,18.7092926104853,19.1990318780609,19.6887711456365,20.1785104132121,
20.6682496807877,21.1579889483633,21.6477282159389,21.9911485751285),
 .UNSPECIFIED.);
#2898=B_SPLINE_CURVE_WITH_KNOTS('',3,(#36793,#36794,#36795,#36796,#36797,
#36798,#36799,#36800,#36801,#36802,#36803,#36804,#36805,#36806,#36807,#36808,
#36809),.UNSPECIFIED.,.F.,.F.,(4,1,1,1,1,1,1,1,1,1,1,1,1,1,4),(15.707963267949,
15.8688271292748,16.3585663968504,16.848305664426,17.3380449320016,17.8277841995772,
18.3175234671527,18.8072627347283,19.2970020023039,19.7867412698795,20.2764805374551,
20.7662198050307,21.2559590726063,21.7456983401819,21.9911485751285),
 .UNSPECIFIED.);
#2899=B_SPLINE_CURVE_WITH_KNOTS('',3,(#37066,#37067,#37068,#37069,#37070,
#37071,#37072,#37073,#37074,#37075,#37076,#37077,#37078,#37079,#37080,#37081,
#37082,#37083,#37084,#37085,#37086,#37087,#37088,#37089,#37090,#37091,#37092,
#37093,#37094,#37095,#37096,#37097,#37098,#37099,#37100,#37101,#37102,#37103,
#37104,#37105,#37106,#37107,#37108,#37109,#37110,#37111,#37112,#37113,#37114,
#37115,#37116,#37117,#37118,#37119,#37120,#37121,#37122,#37123,#37124,#37125,
#37126,#37127,#37128,#37129,#37130,#37131,#37132,#37133,#37134,#37135,#37136,
#37137,#37138,#37139,#37140,#37141,#37142,#37143,#37144,#37145,#37146,#37147,
#37148,#37149,#37150,#37151,#37152,#37153,#37154,#37155,#37156,#37157,#37158,
#37159,#37160,#37161,#37162,#37163,#37164,#37165,#37166,#37167,#37168,#37169,
#37170,#37171),.UNSPECIFIED.,.F.,.F.,(4,3,3,3,3,3,3,3,3,3,3,3,3,3,3,3,3,
3,3,3,3,3,3,3,3,3,3,3,3,3,3,3,3,3,3,4),(0.,0.0384977475150248,0.0777078043309608,
0.117481251338807,0.157167811108441,0.165169791324504,0.172509865645824,
0.21521695096498,0.255388037601424,0.296070338910308,0.332110031619694,
0.341131619391498,0.347586807233502,0.389053038740716,0.430985725027015,
0.440229109747851,0.481905272272016,0.506030616748518,0.519160021122491,
0.524507558777488,0.530100422405358,0.572586107541232,0.615488339646026,
0.658430782990829,0.674908028084035,0.705394548776863,0.711667703381707,
0.718009631315357,0.761258293552277,0.800643768570873,0.821412105483859,
0.829287072559959,0.837097364722895,0.881633891927705,0.918800193626661,
0.950777871811476),.UNSPECIFIED.);
#2900=B_SPLINE_CURVE_WITH_KNOTS('',3,(#37172,#37173,#37174,#37175,#37176,
#37177,#37178,#37179,#37180,#37181,#37182,#37183,#37184,#37185,#37186,#37187,
#37188,#37189,#37190,#37191,#37192,#37193,#37194,#37195,#37196,#37197,#37198,
#37199,#37200,#37201,#37202,#37203,#37204,#37205,#37206,#37207,#37208,#37209,
#37210,#37211,#37212,#37213,#37214),.UNSPECIFIED.,.F.,.F.,(4,3,3,3,3,3,
3,3,3,3,3,3,3,3,4),(-10.1382057107015,-9.79478535151183,-9.30504608393623,
-8.81530681636064,-8.32556754878505,-7.83582828120946,-7.34608901363387,
-6.85634974605828,-6.36661047848269,-5.87687121090709,-5.3871319433315,
-4.89739267575591,-4.40765340818032,-3.91791414060473,-3.85502040352192),
 .UNSPECIFIED.);
#2901=B_SPLINE_CURVE_WITH_KNOTS('',3,(#37471,#37472,#37473,#37474,#37475,
#37476,#37477,#37478,#37479,#37480,#37481,#37482,#37483,#37484,#37485,#37486,
#37487,#37488,#37489,#37490,#37491,#37492,#37493,#37494,#37495,#37496,#37497,
#37498,#37499,#37500,#37501,#37502,#37503,#37504,#37505,#37506,#37507,#37508,
#37509,#37510,#37511,#37512,#37513),.UNSPECIFIED.,.F.,.F.,(4,3,3,3,3,3,
3,3,3,3,3,3,3,3,4),(7.59153924858054,7.83582828120946,8.32556754878505,
8.81530681636064,9.30504608393623,9.79478535151182,10.2845246190874,10.774263886663,
11.2640031542386,11.7537424218142,12.2434816893898,12.7332209569654,13.222960224541,
13.7126994921165,13.8747245557601),.UNSPECIFIED.);
#2902=B_SPLINE_CURVE_WITH_KNOTS('',3,(#37514,#37515,#37516,#37517,#37518,
#37519,#37520,#37521,#37522,#37523,#37524,#37525,#37526,#37527,#37528,#37529,
#37530,#37531,#37532,#37533,#37534,#37535,#37536,#37537,#37538,#37539,#37540,
#37541,#37542,#37543,#37544,#37545,#37546,#37547,#37548,#37549,#37550,#37551,
#37552,#37553,#37554,#37555,#37556,#37557,#37558,#37559,#37560,#37561,#37562,
#37563,#37564,#37565,#37566,#37567,#37568,#37569,#37570,#37571,#37572,#37573,
#37574,#37575,#37576,#37577,#37578,#37579,#37580,#37581,#37582,#37583,#37584,
#37585,#37586,#37587,#37588,#37589,#37590,#37591,#37592,#37593,#37594,#37595,
#37596,#37597,#37598,#37599,#37600,#37601,#37602,#37603,#37604,#37605,#37606,
#37607,#37608,#37609,#37610,#37611,#37612,#37613,#37614,#37615,#37616),
 .UNSPECIFIED.,.F.,.F.,(4,3,3,3,3,3,3,3,3,3,3,3,3,3,3,3,3,3,3,3,3,3,3,3,
3,3,3,3,3,3,3,3,3,3,4),(0.,0.0441184469048226,0.0885852208367534,0.132705877001749,
0.176248830667822,0.188641774332082,0.19491905746566,0.201110035903684,
0.246435079457913,0.289836407260929,0.333162206289049,0.370692322566821,
0.380555108078741,0.388891708168043,0.431181294952235,0.473131870976936,
0.483282671400138,0.525568062903358,0.548671057465475,0.563330517012381,
0.568979423553707,0.610227610939762,0.651359426294659,0.691816927448079,
0.710392019400295,0.737503640980278,0.744688179724382,0.751191992440766,
0.79162882740354,0.825542868562695,0.845308948055337,0.852099049553749,
0.891463370783818,0.927284992040159,0.954382097139101),.UNSPECIFIED.);
#2903=B_SPLINE_CURVE_WITH_KNOTS('',3,(#37619,#37620,#37621,#37622,#37623,
#37624,#37625,#37626,#37627,#37628,#37629,#37630,#37631,#37632,#37633,#37634,
#37635,#37636,#37637,#37638,#37639,#37640,#37641,#37642,#37643,#37644,#37645,
#37646,#37647,#37648,#37649,#37650,#37651,#37652,#37653,#37654,#37655,#37656,
#37657,#37658,#37659,#37660,#37661,#37662,#37663,#37664,#37665,#37666,#37667,
#37668,#37669,#37670,#37671,#37672,#37673,#37674,#37675,#37676,#37677,#37678,
#37679,#37680,#37681,#37682,#37683,#37684,#37685,#37686,#37687,#37688,#37689,
#37690,#37691,#37692,#37693,#37694,#37695,#37696,#37697,#37698,#37699,#37700,
#37701,#37702,#37703,#37704,#37705,#37706,#37707,#37708,#37709,#37710,#37711,
#37712,#37713,#37714,#37715,#37716,#37717,#37718,#37719,#37720,#37721,#37722,
#37723,#37724,#37725,#37726,#37727),.UNSPECIFIED.,.F.,.F.,(4,3,3,3,3,3,
3,3,3,3,3,3,3,3,3,3,3,3,3,3,3,3,3,3,3,3,3,3,3,3,3,3,3,3,3,3,4),(-0.954382097138977,
-0.915485207744247,-0.876011339058948,-0.858387687911483,-0.85129049416266,
-0.844232887287554,-0.803962790021771,-0.771371666248987,-0.755076104362594,
-0.74670724449792,-0.74070308011976,-0.738780542476202,-0.698754813889051,
-0.65801335656101,-0.616748708123891,-0.590809570546834,-0.569476867671065,
-0.564087767374825,-0.521978831154271,-0.512992157815662,-0.471268380752573,
-0.429066791033322,-0.391147227268606,-0.385001278360174,-0.379585399990937,
-0.336630220157075,-0.293213563249867,-0.277388535974458,-0.2341982102794,
-0.208936638932129,-0.199293375273106,-0.191586968667389,-0.147662130603415,
-0.103303648196658,-0.05890222343554,-0.0321056395012341,0.),
 .UNSPECIFIED.);
#2904=B_SPLINE_CURVE_WITH_KNOTS('',3,(#37728,#37729,#37730,#37731,#37732,
#37733,#37734,#37735,#37736,#37737,#37738,#37739,#37740,#37741,#37742,#37743,
#37744,#37745,#37746,#37747,#37748,#37749,#37750,#37751,#37752,#37753,#37754,
#37755,#37756,#37757,#37758,#37759,#37760,#37761,#37762,#37763,#37764,#37765,
#37766,#37767,#37768,#37769,#37770,#37771,#37772,#37773,#37774,#37775,#37776,
#37777,#37778,#37779,#37780,#37781,#37782,#37783,#37784,#37785,#37786,#37787,
#37788,#37789,#37790,#37791,#37792,#37793,#37794,#37795,#37796,#37797,#37798,
#37799,#37800,#37801,#37802,#37803,#37804,#37805,#37806,#37807,#37808,#37809,
#37810,#37811,#37812,#37813,#37814,#37815,#37816,#37817,#37818,#37819,#37820,
#37821,#37822,#37823,#37824,#37825,#37826,#37827,#37828,#37829,#37830,#37831,
#37832,#37833,#37834,#37835,#37836,#37837,#37838,#37839),.UNSPECIFIED.,
 .F.,.F.,(4,3,3,3,3,3,3,3,3,3,3,3,3,3,3,3,3,3,3,3,3,3,3,3,3,3,3,3,3,3,3,
3,3,3,3,3,3,4),(-0.950777871811478,-0.906311279635952,-0.861803983277576,
-0.842287015932126,-0.832349791336995,-0.825106825323525,-0.781341117514485,
-0.743504681014231,-0.724586462764104,-0.715675955845772,-0.70759945511304,
-0.705668244513976,-0.662940066976017,-0.619927854462604,-0.577350786751952,
-0.550469631510745,-0.530308765079839,-0.524965688989733,-0.519443985250198,
-0.477671746572218,-0.469826165787122,-0.427882411937048,-0.386078816514926,
-0.350449958634833,-0.344039953072562,-0.338265645084795,-0.297454287641941,
-0.257005928865392,-0.243563384994553,-0.202803272858004,-0.180830798526362,
-0.172157454195869,-0.165074010559054,-0.125309029596673,-0.0856893302259524,
-0.0467731936127253,-0.0270234782048685,0.),.UNSPECIFIED.);
#2905=B_SPLINE_CURVE_WITH_KNOTS('',3,(#37841,#37842,#37843,#37844,#37845,
#37846,#37847,#37848,#37849,#37850,#37851,#37852,#37853,#37854,#37855,#37856,
#37857),.UNSPECIFIED.,.F.,.F.,(4,1,1,1,1,1,1,1,1,1,1,1,1,1,4),(15.707963267949,
15.7708570050318,16.2605962726074,16.750335540183,17.2400748077586,17.7298140753341,
18.2195533429097,18.7092926104853,19.1990318780609,19.6887711456365,20.1785104132121,
20.6682496807877,21.1579889483633,21.6477282159389,21.9911485751285),
 .UNSPECIFIED.);
#2906=B_SPLINE_CURVE_WITH_KNOTS('',3,(#37858,#37859,#37860,#37861,#37862,
#37863,#37864,#37865,#37866,#37867,#37868,#37869,#37870,#37871,#37872,#37873,
#37874),.UNSPECIFIED.,.F.,.F.,(4,1,1,1,1,1,1,1,1,1,1,1,1,1,4),(15.707963267949,
15.8688271292748,16.3585663968504,16.848305664426,17.3380449320016,17.8277841995772,
18.3175234671527,18.8072627347283,19.2970020023039,19.7867412698795,20.2764805374551,
20.7662198050307,21.2559590726063,21.7456983401819,21.9911485751285),
 .UNSPECIFIED.);
#2907=B_SPLINE_CURVE_WITH_KNOTS('',3,(#38131,#38132,#38133,#38134,#38135,
#38136,#38137,#38138,#38139,#38140,#38141,#38142,#38143,#38144,#38145,#38146,
#38147,#38148,#38149,#38150,#38151,#38152,#38153,#38154,#38155,#38156,#38157,
#38158,#38159,#38160,#38161,#38162,#38163,#38164,#38165,#38166,#38167,#38168,
#38169,#38170,#38171,#38172,#38173,#38174,#38175,#38176,#38177,#38178,#38179,
#38180,#38181,#38182,#38183,#38184,#38185,#38186,#38187,#38188,#38189,#38190,
#38191,#38192,#38193,#38194,#38195,#38196,#38197,#38198,#38199,#38200,#38201,
#38202,#38203,#38204,#38205,#38206,#38207,#38208,#38209,#38210,#38211,#38212,
#38213,#38214,#38215,#38216,#38217,#38218,#38219,#38220,#38221,#38222,#38223,
#38224,#38225,#38226,#38227,#38228,#38229,#38230,#38231,#38232,#38233,#38234,
#38235,#38236),.UNSPECIFIED.,.F.,.F.,(4,3,3,3,3,3,3,3,3,3,3,3,3,3,3,3,3,
3,3,3,3,3,3,3,3,3,3,3,3,3,3,3,3,3,3,4),(0.,0.0384977207228922,0.0777077562539873,
0.117481197715763,0.157167762737478,0.165169736321266,0.172509866069542,
0.215216950964976,0.255388054767118,0.29607036677152,0.332110052515598,
0.341131630636987,0.347586810455887,0.389053056094659,0.430985747347695,
0.440229109747833,0.481905268675028,0.50603061360115,0.519160020855356,
0.524507558424947,0.530100422386196,0.572586102817588,0.615488332273333,
0.65843077524041,0.674908028084002,0.705394548776831,0.711667703500688,
0.718009631383646,0.761258293923528,0.800643768849303,0.821412105867649,
0.829287075911994,0.837097365077352,0.88163389211237,0.91880019362663,0.950777871811445),
 .UNSPECIFIED.);
#2908=B_SPLINE_CURVE_WITH_KNOTS('',3,(#38237,#38238,#38239,#38240,#38241,
#38242,#38243,#38244,#38245,#38246,#38247,#38248,#38249,#38250,#38251,#38252,
#38253,#38254,#38255,#38256,#38257,#38258,#38259,#38260,#38261,#38262,#38263,
#38264,#38265,#38266,#38267,#38268,#38269,#38270,#38271,#38272,#38273,#38274,
#38275,#38276,#38277,#38278,#38279),.UNSPECIFIED.,.F.,.F.,(4,3,3,3,3,3,
3,3,3,3,3,3,3,3,4),(-10.1382057107015,-9.79478535151182,-9.30504608393623,
-8.81530681636064,-8.32556754878505,-7.83582828120945,-7.34608901363386,
-6.85634974605827,-6.36661047848268,-5.87687121090709,-5.3871319433315,
-4.89739267575591,-4.40765340818032,-3.91791414060473,-3.85502040352192),
 .UNSPECIFIED.);
#2909=B_SPLINE_CURVE_WITH_KNOTS('',3,(#38536,#38537,#38538,#38539,#38540,
#38541,#38542,#38543,#38544,#38545,#38546,#38547,#38548,#38549,#38550,#38551,
#38552,#38553,#38554,#38555,#38556,#38557,#38558,#38559,#38560,#38561,#38562,
#38563,#38564,#38565,#38566,#38567,#38568,#38569,#38570,#38571,#38572,#38573,
#38574,#38575,#38576,#38577,#38578),.UNSPECIFIED.,.F.,.F.,(4,3,3,3,3,3,
3,3,3,3,3,3,3,3,4),(7.59153924858054,7.83582828120946,8.32556754878505,
8.81530681636064,9.30504608393623,9.79478535151182,10.2845246190874,10.774263886663,
11.2640031542386,11.7537424218142,12.2434816893898,12.7332209569654,13.222960224541,
13.7126994921165,13.8747245557601),.UNSPECIFIED.);
#2910=B_SPLINE_CURVE_WITH_KNOTS('',3,(#38579,#38580,#38581,#38582,#38583,
#38584,#38585,#38586,#38587,#38588,#38589,#38590,#38591,#38592,#38593,#38594,
#38595,#38596,#38597,#38598,#38599,#38600,#38601,#38602,#38603,#38604,#38605,
#38606,#38607,#38608,#38609,#38610,#38611,#38612,#38613,#38614,#38615,#38616,
#38617,#38618,#38619,#38620,#38621,#38622,#38623,#38624,#38625,#38626,#38627,
#38628,#38629,#38630,#38631,#38632,#38633,#38634,#38635,#38636,#38637,#38638,
#38639,#38640,#38641,#38642,#38643,#38644,#38645,#38646,#38647,#38648,#38649,
#38650,#38651,#38652,#38653,#38654,#38655,#38656,#38657,#38658,#38659,#38660,
#38661,#38662,#38663,#38664,#38665,#38666,#38667,#38668,#38669,#38670,#38671,
#38672,#38673,#38674,#38675,#38676,#38677,#38678,#38679,#38680,#38681),
 .UNSPECIFIED.,.F.,.F.,(4,3,3,3,3,3,3,3,3,3,3,3,3,3,3,3,3,3,3,3,3,3,3,3,
3,3,3,3,3,3,3,3,3,3,4),(0.,0.0441184631390831,0.0885852409169272,0.132705885951212,
0.176248824533162,0.188641758266505,0.194920509910256,0.201110308777038,
0.246435079457889,0.289836402930589,0.333162202698913,0.370692319874208,
0.380555067756269,0.388891719911904,0.431181305813495,0.473131884132789,
0.483282671400094,0.525568063164174,0.548671057693681,0.563330516361131,
0.568979422724069,0.610227610515779,0.6513594262039,0.691816928928125,0.710392019400234,
0.737503640980213,0.744688178741843,0.751191992239498,0.791628827388096,
0.825542868551089,0.845308948164629,0.85209904962518,0.891463369824715,
0.927284992040065,0.954382097139),.UNSPECIFIED.);
#2911=B_SPLINE_CURVE_WITH_KNOTS('',3,(#38684,#38685,#38686,#38687,#38688,
#38689,#38690,#38691,#38692,#38693,#38694,#38695,#38696,#38697,#38698,#38699,
#38700,#38701,#38702,#38703,#38704,#38705,#38706,#38707,#38708,#38709,#38710,
#38711,#38712,#38713,#38714,#38715,#38716,#38717,#38718,#38719,#38720,#38721,
#38722,#38723,#38724,#38725,#38726,#38727,#38728,#38729,#38730,#38731,#38732,
#38733,#38734,#38735,#38736,#38737,#38738,#38739,#38740,#38741,#38742,#38743,
#38744,#38745,#38746,#38747,#38748,#38749,#38750,#38751,#38752,#38753,#38754,
#38755,#38756,#38757,#38758,#38759,#38760,#38761,#38762,#38763,#38764,#38765,
#38766,#38767,#38768,#38769,#38770,#38771,#38772,#38773,#38774,#38775,#38776,
#38777,#38778,#38779,#38780,#38781,#38782,#38783,#38784,#38785,#38786,#38787,
#38788,#38789,#38790,#38791,#38792),.UNSPECIFIED.,.F.,.F.,(4,3,3,3,3,3,
3,3,3,3,3,3,3,3,3,3,3,3,3,3,3,3,3,3,3,3,3,3,3,3,3,3,3,3,3,3,4),(-0.954382097139049,
-0.915485243799018,-0.876011399544332,-0.85838777184726,-0.851290348307254,
-0.844232852031221,-0.80396277352234,-0.771371657999283,-0.755076100237755,
-0.746707233752317,-0.740703067945048,-0.738780542476226,-0.698754782173372,
-0.658013300891092,-0.616748645324364,-0.590809523447192,-0.569476777358248,
-0.564087663108025,-0.521978710451211,-0.512992157815676,-0.471268388808549,
-0.429066803611481,-0.391147236702228,-0.385001289855828,-0.379585402193585,
-0.33663022899104,-0.293213574317017,-0.277388535974469,-0.23419821036879,
-0.208936639010346,-0.199293375269724,-0.191586968520703,-0.147662130179972,
-0.1033036479831,-0.0589022231403947,-0.0321056395012349,0.),
 .UNSPECIFIED.);
#2912=B_SPLINE_CURVE_WITH_KNOTS('',3,(#38793,#38794,#38795,#38796,#38797,
#38798,#38799,#38800,#38801,#38802,#38803,#38804,#38805,#38806,#38807,#38808,
#38809,#38810,#38811,#38812,#38813,#38814,#38815,#38816,#38817,#38818,#38819,
#38820,#38821,#38822,#38823,#38824,#38825,#38826,#38827,#38828,#38829,#38830,
#38831,#38832,#38833,#38834,#38835,#38836,#38837,#38838,#38839,#38840,#38841,
#38842,#38843,#38844,#38845,#38846,#38847,#38848,#38849,#38850,#38851,#38852,
#38853,#38854,#38855,#38856,#38857,#38858,#38859,#38860,#38861,#38862,#38863,
#38864,#38865,#38866,#38867,#38868,#38869,#38870,#38871,#38872,#38873,#38874,
#38875,#38876,#38877,#38878,#38879,#38880,#38881,#38882,#38883,#38884,#38885,
#38886,#38887,#38888,#38889,#38890,#38891,#38892,#38893,#38894,#38895,#38896,
#38897,#38898,#38899,#38900,#38901,#38902,#38903,#38904),.UNSPECIFIED.,
 .F.,.F.,(4,3,3,3,3,3,3,3,3,3,3,3,3,3,3,3,3,3,3,3,3,3,3,3,3,3,3,3,3,3,3,
3,3,3,3,3,3,4),(-0.950777871811488,-0.906311274832857,-0.861803980370618,
-0.842287013388538,-0.832349783836988,-0.825106819793286,-0.781341115719767,
-0.743504680116872,-0.724586462315425,-0.715675955150876,-0.707599455145821,
-0.705668244513978,-0.662940072098965,-0.619927861036148,-0.577350791907412,
-0.550469635377338,-0.530308767979781,-0.524965693857714,-0.519443986212373,
-0.477671746910201,-0.469826165787113,-0.427882411597154,-0.386078816010451,
-0.350449958256475,-0.34403995205164,-0.338265644838692,-0.29745428724094,
-0.257005928020942,-0.243563384994547,-0.202803273036419,-0.180830798682476,
-0.172157454615961,-0.165074010553165,-0.125309029539932,-0.0856893304901558,
-0.0467731948431029,-0.0270234782048771,0.),.UNSPECIFIED.);
#2913=B_SPLINE_CURVE_WITH_KNOTS('',3,(#38906,#38907,#38908,#38909,#38910,
#38911,#38912,#38913,#38914,#38915,#38916,#38917,#38918,#38919,#38920,#38921,
#38922),.UNSPECIFIED.,.F.,.F.,(4,1,1,1,1,1,1,1,1,1,1,1,1,1,4),(15.707963267949,
15.7708570050318,16.2605962726074,16.750335540183,17.2400748077586,17.7298140753341,
18.2195533429097,18.7092926104853,19.1990318780609,19.6887711456365,20.1785104132121,
20.6682496807877,21.1579889483633,21.6477282159389,21.9911485751285),
 .UNSPECIFIED.);
#2914=B_SPLINE_CURVE_WITH_KNOTS('',3,(#38923,#38924,#38925,#38926,#38927,
#38928,#38929,#38930,#38931,#38932,#38933,#38934,#38935,#38936,#38937,#38938,
#38939),.UNSPECIFIED.,.F.,.F.,(4,1,1,1,1,1,1,1,1,1,1,1,1,1,4),(15.707963267949,
15.8688271292748,16.3585663968504,16.848305664426,17.3380449320016,17.8277841995772,
18.3175234671527,18.8072627347283,19.2970020023039,19.7867412698795,20.2764805374551,
20.7662198050307,21.2559590726063,21.7456983401819,21.9911485751285),
 .UNSPECIFIED.);
#2915=B_SPLINE_CURVE_WITH_KNOTS('',3,(#39196,#39197,#39198,#39199,#39200,
#39201,#39202,#39203,#39204,#39205,#39206,#39207,#39208,#39209,#39210,#39211,
#39212,#39213,#39214,#39215,#39216,#39217,#39218,#39219,#39220,#39221,#39222,
#39223,#39224,#39225,#39226,#39227,#39228,#39229,#39230,#39231,#39232,#39233,
#39234,#39235,#39236,#39237,#39238,#39239,#39240,#39241,#39242,#39243,#39244,
#39245,#39246,#39247,#39248,#39249,#39250,#39251,#39252,#39253,#39254,#39255,
#39256,#39257,#39258,#39259,#39260,#39261,#39262,#39263,#39264,#39265,#39266,
#39267,#39268,#39269,#39270,#39271,#39272,#39273,#39274,#39275,#39276,#39277,
#39278,#39279,#39280,#39281,#39282,#39283,#39284,#39285,#39286,#39287,#39288,
#39289,#39290,#39291,#39292,#39293,#39294,#39295,#39296,#39297,#39298,#39299,
#39300,#39301),.UNSPECIFIED.,.F.,.F.,(4,3,3,3,3,3,3,3,3,3,3,3,3,3,3,3,3,
3,3,3,3,3,3,3,3,3,3,3,3,3,3,3,3,3,3,4),(0.,0.0384977351933318,0.0777077822193152,
0.117481226676887,0.157167788863923,0.165169766029963,0.17250986583581,
0.215216950964983,0.255388045498387,0.296070351727255,0.332110041232406,
0.341131624564715,0.347586808736851,0.389053046746773,0.430985735316375,
0.440229109747859,0.481905270616845,0.506030615300244,0.519160020999484,
0.524507558604161,0.53010042239424,0.572586105363907,0.61548833624855,0.658430779419949,
0.674908028084036,0.705394548776866,0.711667703489009,0.718009631360576,
0.761258293736136,0.80064376870877,0.821412105671848,0.829287074196938,
0.837097364893477,0.881633892019366,0.918800193626673,0.950777871811486),
 .UNSPECIFIED.);
#2916=B_SPLINE_CURVE_WITH_KNOTS('',3,(#39302,#39303,#39304,#39305,#39306,
#39307,#39308,#39309,#39310,#39311,#39312,#39313,#39314,#39315,#39316,#39317,
#39318,#39319,#39320,#39321,#39322,#39323,#39324,#39325,#39326,#39327,#39328,
#39329,#39330,#39331,#39332,#39333,#39334,#39335,#39336,#39337,#39338,#39339,
#39340,#39341,#39342,#39343,#39344),.UNSPECIFIED.,.F.,.F.,(4,3,3,3,3,3,
3,3,3,3,3,3,3,3,4),(-10.1382057107015,-9.79478535151183,-9.30504608393623,
-8.81530681636065,-8.32556754878505,-7.83582828120946,-7.34608901363387,
-6.85634974605828,-6.36661047848269,-5.8768712109071,-5.3871319433315,-4.89739267575591,
-4.40765340818032,-3.91791414060473,-3.85502040352192),.UNSPECIFIED.);
#2917=B_SPLINE_CURVE_WITH_KNOTS('',3,(#39601,#39602,#39603,#39604,#39605,
#39606,#39607,#39608,#39609,#39610,#39611,#39612,#39613,#39614,#39615,#39616,
#39617,#39618,#39619,#39620,#39621,#39622,#39623,#39624,#39625,#39626,#39627,
#39628,#39629,#39630,#39631,#39632,#39633,#39634,#39635,#39636,#39637,#39638,
#39639,#39640,#39641,#39642,#39643),.UNSPECIFIED.,.F.,.F.,(4,3,3,3,3,3,
3,3,3,3,3,3,3,3,4),(7.59153924858054,7.83582828120945,8.32556754878505,
8.81530681636064,9.30504608393623,9.79478535151182,10.2845246190874,10.774263886663,
11.2640031542386,11.7537424218142,12.2434816893898,12.7332209569654,13.222960224541,
13.7126994921165,13.8747245557601),.UNSPECIFIED.);
#2918=B_SPLINE_CURVE_WITH_KNOTS('',3,(#39644,#39645,#39646,#39647,#39648,
#39649,#39650,#39651,#39652,#39653,#39654,#39655,#39656,#39657,#39658,#39659,
#39660,#39661,#39662,#39663,#39664,#39665,#39666,#39667,#39668,#39669,#39670,
#39671,#39672,#39673,#39674,#39675,#39676,#39677,#39678,#39679,#39680,#39681,
#39682,#39683,#39684,#39685,#39686,#39687,#39688,#39689,#39690,#39691,#39692,
#39693,#39694,#39695,#39696,#39697,#39698,#39699,#39700,#39701,#39702,#39703,
#39704,#39705,#39706,#39707,#39708,#39709,#39710,#39711,#39712,#39713,#39714,
#39715,#39716,#39717,#39718,#39719,#39720,#39721,#39722,#39723,#39724,#39725,
#39726,#39727,#39728,#39729,#39730,#39731,#39732,#39733,#39734,#39735,#39736,
#39737,#39738,#39739,#39740,#39741,#39742,#39743,#39744,#39745,#39746),
 .UNSPECIFIED.,.F.,.F.,(4,3,3,3,3,3,3,3,3,3,3,3,3,3,3,3,3,3,3,3,3,3,3,3,
3,3,3,3,3,3,3,3,3,3,4),(0.,0.0441184377234137,0.0885852094785448,0.132705871934227,
0.176248834126375,0.18864178338789,0.19491823898691,0.201109882338307,0.246435079457898,
0.289836409708683,0.333162208320045,0.370692324090062,0.380555130854219,
0.38889170154541,0.431181288829226,0.473131863558235,0.483282671400115,
0.525568062754779,0.548671057335465,0.56333051737996,0.568979423977601,
0.610227611133655,0.651359426299229,0.691816926566307,0.710392019400264,
0.737503640980246,0.744688180059427,0.751191992518895,0.791628827376913,
0.825542868542715,0.845308947964658,0.852099049499542,0.891463371311063,
0.92728499204012,0.954382097139051),.UNSPECIFIED.);
#2919=B_SPLINE_CURVE_WITH_KNOTS('',3,(#39753,#39754,#39755,#39756,#39757,
#39758,#39759,#39760,#39761,#39762,#39763,#39764,#39765,#39766,#39767,#39768,
#39769,#39770,#39771,#39772,#39773,#39774,#39775,#39776,#39777,#39778,#39779,
#39780,#39781,#39782,#39783,#39784,#39785,#39786,#39787,#39788,#39789,#39790,
#39791,#39792,#39793,#39794,#39795,#39796,#39797,#39798,#39799,#39800,#39801,
#39802,#39803,#39804,#39805,#39806,#39807,#39808,#39809,#39810,#39811,#39812,
#39813,#39814,#39815,#39816,#39817,#39818,#39819,#39820,#39821,#39822,#39823,
#39824,#39825,#39826,#39827,#39828,#39829,#39830,#39831,#39832,#39833,#39834,
#39835,#39836,#39837,#39838,#39839,#39840,#39841,#39842,#39843,#39844,#39845,
#39846,#39847,#39848,#39849,#39850,#39851,#39852),.UNSPECIFIED.,.F.,.F.,
(4,3,3,3,3,3,3,3,3,3,3,3,3,3,3,3,3,3,3,3,3,3,3,3,3,3,3,3,3,3,3,3,3,4),(-0.760759816994569,
-0.72862787829937,-0.695756720514147,-0.68606839026359,-0.679579333012852,
-0.673178904811534,-0.639342185929258,-0.610292612829778,-0.600454920433494,
-0.594751295643759,-0.5602179171347,-0.525201053232817,-0.490288939350313,
-0.469453104796089,-0.455093610752485,-0.450652652628591,-0.414664231423942,
-0.406945601133418,-0.372348152705916,-0.337004174076161,-0.31718673063397,
-0.308923304598713,-0.304448472040256,-0.268404613806068,-0.231699686844986,
-0.194697269281947,-0.172850745496843,-0.161340406317873,-0.156038360829996,
-0.118189716276133,-0.0802678600345118,-0.0429993716816808,-0.0199250790011154,
0.),.UNSPECIFIED.);
#2920=B_SPLINE_CURVE_WITH_KNOTS('',3,(#39853,#39854,#39855,#39856,#39857,
#39858,#39859,#39860,#39861,#39862,#39863,#39864,#39865,#39866,#39867,#39868,
#39869,#39870,#39871,#39872,#39873,#39874,#39875,#39876,#39877,#39878,#39879,
#39880,#39881,#39882,#39883,#39884,#39885,#39886,#39887,#39888,#39889,#39890,
#39891,#39892,#39893,#39894,#39895,#39896,#39897,#39898,#39899,#39900,#39901,
#39902,#39903,#39904,#39905,#39906,#39907,#39908,#39909,#39910,#39911,#39912,
#39913,#39914,#39915,#39916,#39917,#39918,#39919,#39920,#39921,#39922,#39923,
#39924,#39925,#39926,#39927,#39928,#39929,#39930,#39931,#39932,#39933,#39934,
#39935,#39936,#39937,#39938,#39939,#39940,#39941,#39942,#39943,#39944,#39945,
#39946,#39947,#39948,#39949,#39950,#39951,#39952),.UNSPECIFIED.,.F.,.F.,
(4,3,3,3,3,3,3,3,3,3,3,3,3,3,3,3,3,3,3,3,3,3,3,3,3,3,3,3,3,3,3,3,3,4),(-0.757763664684572,
-0.720377639686879,-0.68246665016733,-0.666432992745214,-0.657234612624417,
-0.619826663102441,-0.588739338539928,-0.575138634043828,-0.567711759329971,
-0.562381430293886,-0.525809998287688,-0.489512576741164,-0.454189714609801,
-0.433424302607935,-0.418943938986772,-0.414278003736301,-0.379386458468707,
-0.371128066602335,-0.335727258188192,-0.300034647812248,-0.282321970831172,
-0.275156765762531,-0.270309060105739,-0.23559711240685,-0.200919055510916,
-0.166729845604536,-0.147967591918348,-0.137478179675258,-0.130951779287757,
-0.0975592011702397,-0.0646630819112997,-0.0327161480307065,-0.0166318161150331,
0.),.UNSPECIFIED.);
#2921=B_SPLINE_CURVE_WITH_KNOTS('',3,(#39954,#39955,#39956,#39957,#39958,
#39959,#39960,#39961,#39962,#39963,#39964),.UNSPECIFIED.,.F.,.F.,(4,1,1,
1,1,1,1,1,4),(15.7079632679489,15.7955882081887,16.7801008045318,17.7646134008748,
18.7491259972179,19.733638593561,20.718151189904,21.7026637862471,21.9911485751285),
 .UNSPECIFIED.);
#2922=B_SPLINE_CURVE_WITH_KNOTS('',3,(#39965,#39966,#39967,#39968,#39969,
#39970,#39971,#39972,#39973,#39974),.UNSPECIFIED.,.F.,.F.,(4,1,1,1,1,1,
1,4),(15.7079632679489,16.3681508394037,17.3526634357467,18.3371760320898,
19.3216886284329,20.3062012247759,21.290713821119,21.9911485751285),
 .UNSPECIFIED.);
#2923=B_SPLINE_CURVE_WITH_KNOTS('',3,(#40179,#40180,#40181,#40182,#40183,
#40184,#40185,#40186,#40187,#40188,#40189,#40190,#40191,#40192,#40193,#40194,
#40195,#40196,#40197,#40198,#40199,#40200,#40201,#40202,#40203,#40204,#40205,
#40206,#40207,#40208,#40209,#40210,#40211,#40212,#40213,#40214,#40215,#40216,
#40217,#40218,#40219,#40220,#40221,#40222,#40223,#40224,#40225,#40226,#40227,
#40228,#40229,#40230,#40231,#40232,#40233,#40234,#40235,#40236,#40237,#40238,
#40239,#40240,#40241,#40242,#40243,#40244,#40245,#40246,#40247,#40248,#40249,
#40250,#40251,#40252,#40253,#40254,#40255,#40256,#40257,#40258,#40259,#40260,
#40261,#40262,#40263,#40264,#40265,#40266,#40267,#40268,#40269,#40270,#40271,
#40272),.UNSPECIFIED.,.F.,.F.,(4,3,3,3,3,3,3,3,3,3,3,3,3,3,3,3,3,3,3,3,
3,3,3,3,3,3,3,3,3,3,3,4),(0.,0.0317393131722086,0.0642710888601908,0.0974907644309431,
0.129407607237421,0.134009844296982,0.138840357948445,0.172956104929503,
0.207581737824153,0.243892680088807,0.271125886787297,0.277136007979861,
0.312751955574691,0.348252906207798,0.352825506882768,0.387546385450957,
0.409444611894283,0.417180287420671,0.422139708315971,0.457113923397589,
0.493313993607226,0.529906408582694,0.555907858577878,0.563763193650837,
0.571495314967843,0.608811788498078,0.641088343509601,0.655846955831368,
0.662600714484889,0.700434562175506,0.73791800854417,0.757763664684532),
 .UNSPECIFIED.);
#2924=B_SPLINE_CURVE_WITH_KNOTS('',3,(#40273,#40274,#40275,#40276,#40277,
#40278,#40279,#40280,#40281,#40282,#40283,#40284,#40285,#40286,#40287,#40288,
#40289,#40290,#40291,#40292,#40293,#40294,#40295,#40296,#40297),
 .UNSPECIFIED.,.F.,.F.,(4,3,3,3,3,3,3,3,4),(-10.1336107523121,-9.84512596343066,
-8.86061336708759,-7.87610077074453,-6.89158817440146,-5.9070755780584,
-4.92256298171533,-3.93805038537226,-3.85042544513252),.UNSPECIFIED.);
#2925=B_SPLINE_CURVE_WITH_KNOTS('',3,(#40502,#40503,#40504,#40505,#40506,
#40507,#40508,#40509,#40510,#40511,#40512,#40513,#40514,#40515,#40516,#40517,
#40518,#40519,#40520,#40521,#40522,#40523,#40524,#40525,#40526),
 .UNSPECIFIED.,.F.,.F.,(4,3,3,3,3,3,3,3,4),(7.59202292841098,7.87610077074452,
8.86061336708759,9.84512596343066,10.8296385597737,11.8141511561168,12.7986637524599,
13.7831763488029,13.8752082355906),.UNSPECIFIED.);
#2926=B_SPLINE_CURVE_WITH_KNOTS('',3,(#40527,#40528,#40529,#40530,#40531,
#40532,#40533,#40534,#40535,#40536,#40537,#40538,#40539,#40540,#40541,#40542,
#40543,#40544,#40545,#40546,#40547,#40548,#40549,#40550,#40551,#40552,#40553,
#40554,#40555,#40556,#40557,#40558,#40559,#40560,#40561,#40562,#40563,#40564,
#40565,#40566,#40567,#40568,#40569,#40570,#40571,#40572,#40573,#40574,#40575,
#40576,#40577,#40578,#40579,#40580,#40581,#40582,#40583,#40584,#40585,#40586,
#40587,#40588,#40589,#40590,#40591,#40592,#40593,#40594,#40595,#40596,#40597,
#40598,#40599,#40600,#40601,#40602,#40603,#40604,#40605,#40606,#40607,#40608,
#40609,#40610,#40611,#40612,#40613,#40614,#40615,#40616,#40617,#40618,#40619,
#40620,#40621,#40622,#40623),.UNSPECIFIED.,.F.,.F.,(4,3,3,3,3,3,3,3,3,3,
3,3,3,3,3,3,3,3,3,3,3,3,3,3,3,3,3,3,3,3,3,3,4),(0.,0.0368231104917497,0.0744313668444073,
0.113698757913489,0.148057725098936,0.154809695453249,0.159905279610154,
0.196856237502933,0.233660813338438,0.269922734929624,0.299584675046484,
0.306586456956745,0.311530200028528,0.347067656739102,0.381889315190812,
0.388570495397064,0.424561732072777,0.444531524904213,0.452400918448495,
0.457441217514027,0.493270867496743,0.528364028122716,0.56305045338481,
0.585678948883678,0.594960281935166,0.600628204014577,0.634676029427075,
0.662026626414246,0.675581363680469,0.683279768149963,0.715772844080334,
0.744078417375757,0.760759816994505),.UNSPECIFIED.);
#2927=B_SPLINE_CURVE_WITH_KNOTS('',3,(#40626,#40627,#40628,#40629,#40630,
#40631,#40632,#40633,#40634,#40635,#40636,#40637,#40638,#40639,#40640,#40641,
#40642,#40643,#40644,#40645,#40646,#40647,#40648,#40649,#40650,#40651,#40652,
#40653,#40654,#40655,#40656,#40657,#40658,#40659,#40660,#40661,#40662,#40663,
#40664,#40665,#40666,#40667,#40668,#40669,#40670,#40671,#40672,#40673,#40674,
#40675,#40676,#40677,#40678,#40679,#40680,#40681,#40682,#40683,#40684,#40685,
#40686,#40687,#40688,#40689,#40690,#40691,#40692,#40693,#40694,#40695,#40696,
#40697,#40698,#40699,#40700,#40701,#40702,#40703,#40704,#40705,#40706,#40707,
#40708,#40709,#40710,#40711,#40712,#40713,#40714,#40715,#40716,#40717,#40718,
#40719,#40720,#40721,#40722,#40723,#40724,#40725),.UNSPECIFIED.,.F.,.F.,
(4,3,3,3,3,3,3,3,3,3,3,3,3,3,3,3,3,3,3,3,3,3,3,3,3,3,3,3,3,3,3,3,3,4),(-0.760759816994564,
-0.72862788991672,-0.69575674190594,-0.686068386386768,-0.679579306421937,
-0.673178902123493,-0.639342190945096,-0.610292617218635,-0.600454931774126,
-0.594751307989734,-0.560217937481691,-0.525201077134436,-0.490288959777163,
-0.469453120116225,-0.455093617098093,-0.450652664319302,-0.414664242634724,
-0.40694560113341,-0.372348145271188,-0.337004161764575,-0.317186719091858,
-0.308923268328764,-0.304448416954742,-0.268404551836861,-0.231699621164082,
-0.194697202953257,-0.172850687459238,-0.161340379081848,-0.156038350660818,
-0.118189704854676,-0.080267848749223,-0.0429993598106653,-0.0199250790011036,
0.),.UNSPECIFIED.);
#2928=B_SPLINE_CURVE_WITH_KNOTS('',3,(#40726,#40727,#40728,#40729,#40730,
#40731,#40732,#40733,#40734,#40735,#40736,#40737,#40738,#40739,#40740,#40741,
#40742,#40743,#40744,#40745,#40746,#40747,#40748,#40749,#40750,#40751,#40752,
#40753,#40754,#40755,#40756,#40757,#40758,#40759,#40760,#40761,#40762,#40763,
#40764,#40765,#40766,#40767,#40768,#40769,#40770,#40771,#40772,#40773,#40774,
#40775,#40776,#40777,#40778,#40779,#40780,#40781,#40782,#40783,#40784,#40785,
#40786,#40787,#40788,#40789,#40790,#40791,#40792,#40793,#40794,#40795,#40796,
#40797,#40798,#40799,#40800,#40801,#40802,#40803,#40804,#40805,#40806,#40807,
#40808,#40809,#40810,#40811,#40812,#40813,#40814,#40815,#40816,#40817,#40818,
#40819,#40820,#40821,#40822,#40823,#40824,#40825),.UNSPECIFIED.,.F.,.F.,
(4,3,3,3,3,3,3,3,3,3,3,3,3,3,3,3,3,3,3,3,3,3,3,3,3,3,3,3,3,3,3,3,3,4),(-0.757763664684492,
-0.720377623574381,-0.682466628623801,-0.66643289277039,-0.657234612451942,
-0.619826662873363,-0.588739338339482,-0.575138633855909,-0.567711744977049,
-0.562381426500434,-0.525809996194753,-0.489512580893587,-0.454189724729181,
-0.433424310197464,-0.418943937897784,-0.414278001003576,-0.379386462480084,
-0.371128066602314,-0.335727259413989,-0.300034648045544,-0.282321971049887,
-0.275156772069666,-0.270309064544493,-0.235597116037967,-0.200919059265354,
-0.166729853637965,-0.147967598947598,-0.137478187843834,-0.130951779920804,
-0.0975592047704314,-0.0646630925664832,-0.032716171474427,-0.0166318161150306,
0.),.UNSPECIFIED.);
#2929=B_SPLINE_CURVE_WITH_KNOTS('',3,(#40827,#40828,#40829,#40830,#40831,
#40832,#40833,#40834,#40835,#40836,#40837),.UNSPECIFIED.,.F.,.F.,(4,1,1,
1,1,1,1,1,4),(15.7079632679489,15.7955882081887,16.7801008045318,17.7646134008748,
18.7491259972179,19.733638593561,20.718151189904,21.7026637862471,21.9911485751285),
 .UNSPECIFIED.);
#2930=B_SPLINE_CURVE_WITH_KNOTS('',3,(#40838,#40839,#40840,#40841,#40842,
#40843,#40844,#40845,#40846,#40847),.UNSPECIFIED.,.F.,.F.,(4,1,1,1,1,1,
1,4),(15.7079632679489,16.3681508394037,17.3526634357467,18.3371760320898,
19.3216886284329,20.3062012247759,21.290713821119,21.9911485751285),
 .UNSPECIFIED.);
#2931=B_SPLINE_CURVE_WITH_KNOTS('',3,(#41052,#41053,#41054,#41055,#41056,
#41057,#41058,#41059,#41060,#41061,#41062,#41063,#41064,#41065,#41066,#41067,
#41068,#41069,#41070,#41071,#41072,#41073,#41074,#41075,#41076,#41077,#41078,
#41079,#41080,#41081,#41082,#41083,#41084,#41085,#41086,#41087,#41088,#41089,
#41090,#41091,#41092,#41093,#41094,#41095,#41096,#41097,#41098,#41099,#41100,
#41101,#41102,#41103,#41104,#41105,#41106,#41107,#41108,#41109,#41110,#41111,
#41112,#41113,#41114,#41115,#41116,#41117,#41118,#41119,#41120,#41121,#41122,
#41123,#41124,#41125,#41126,#41127,#41128,#41129,#41130,#41131,#41132,#41133,
#41134,#41135,#41136,#41137,#41138,#41139,#41140,#41141,#41142,#41143,#41144,
#41145),.UNSPECIFIED.,.F.,.F.,(4,3,3,3,3,3,3,3,3,3,3,3,3,3,3,3,3,3,3,3,
3,3,3,3,3,3,3,3,3,3,3,4),(0.,0.0317393385474546,0.0642711372305777,0.0974908302253786,
0.129407664807553,0.134009929659094,0.138840372798717,0.172956137150136,
0.207581778796227,0.243892710817864,0.271125909834093,0.277136017604199,
0.312751969178281,0.34825291267891,0.352825506882778,0.387546373463078,
0.409444600655646,0.417180277227003,0.422139689655615,0.457113887842331,
0.493313950003616,0.529906362555575,0.555907818304148,0.563762874105919,
0.571495346164915,0.60881181674222,0.641088364692705,0.655846960756109,
0.662600717097456,0.700434565111295,0.73791800854416,0.757763664684518),
 .UNSPECIFIED.);
#2932=B_SPLINE_CURVE_WITH_KNOTS('',3,(#41146,#41147,#41148,#41149,#41150,
#41151,#41152,#41153,#41154,#41155,#41156,#41157,#41158,#41159,#41160,#41161,
#41162,#41163,#41164,#41165,#41166,#41167,#41168,#41169,#41170),
 .UNSPECIFIED.,.F.,.F.,(4,3,3,3,3,3,3,3,4),(-10.1336107523121,-9.84512596343066,
-8.86061336708759,-7.87610077074453,-6.89158817440146,-5.9070755780584,
-4.92256298171533,-3.93805038537226,-3.85042544513253),.UNSPECIFIED.);
#2933=B_SPLINE_CURVE_WITH_KNOTS('',3,(#41375,#41376,#41377,#41378,#41379,
#41380,#41381,#41382,#41383,#41384,#41385,#41386,#41387,#41388,#41389,#41390,
#41391,#41392,#41393,#41394,#41395,#41396,#41397,#41398,#41399),
 .UNSPECIFIED.,.F.,.F.,(4,3,3,3,3,3,3,3,4),(7.592022928411,7.87610077074453,
8.8606133670876,9.84512596343066,10.8296385597737,11.8141511561168,12.7986637524599,
13.7831763488029,13.8752082355906),.UNSPECIFIED.);
#2934=B_SPLINE_CURVE_WITH_KNOTS('',3,(#41400,#41401,#41402,#41403,#41404,
#41405,#41406,#41407,#41408,#41409,#41410,#41411,#41412,#41413,#41414,#41415,
#41416,#41417,#41418,#41419,#41420,#41421,#41422,#41423,#41424,#41425,#41426,
#41427,#41428,#41429,#41430,#41431,#41432,#41433,#41434,#41435,#41436,#41437,
#41438,#41439,#41440,#41441,#41442,#41443,#41444,#41445,#41446,#41447,#41448,
#41449,#41450,#41451,#41452,#41453,#41454,#41455,#41456,#41457,#41458,#41459,
#41460,#41461,#41462,#41463,#41464,#41465,#41466,#41467,#41468,#41469,#41470,
#41471,#41472,#41473,#41474,#41475,#41476,#41477,#41478,#41479,#41480,#41481,
#41482,#41483,#41484,#41485,#41486,#41487,#41488,#41489,#41490,#41491,#41492,
#41493,#41494,#41495,#41496),.UNSPECIFIED.,.F.,.F.,(4,3,3,3,3,3,3,3,3,3,
3,3,3,3,3,3,3,3,3,3,3,3,3,3,3,3,3,3,3,3,3,3,4),(0.,0.0368231001962915,0.0744313508791827,
0.113698743943915,0.148057712875556,0.154809587820709,0.159905235470134,
0.196856192833996,0.233660771612868,0.269922697362649,0.299584646871248,
0.306586382979425,0.31153012555125,0.347067586247613,0.38188924839607,0.388570495397043,
0.424561731743958,0.444531524595945,0.452400916951006,0.457441217399145,
0.493270867396221,0.52836402777598,0.563050454529762,0.58567894988551,0.594960252908482,
0.600628199835682,0.634676026456314,0.662026624186173,0.675581364411591,
0.683279768872821,0.71577284943675,0.744078417375749,0.7607598169945),
 .UNSPECIFIED.);
#2935=B_SPLINE_CURVE_WITH_KNOTS('',3,(#41499,#41500,#41501,#41502,#41503,
#41504,#41505,#41506,#41507,#41508,#41509,#41510,#41511,#41512,#41513,#41514,
#41515,#41516,#41517,#41518,#41519,#41520,#41521,#41522,#41523,#41524,#41525,
#41526,#41527,#41528,#41529,#41530,#41531,#41532,#41533,#41534,#41535,#41536,
#41537,#41538,#41539,#41540,#41541,#41542,#41543,#41544,#41545,#41546,#41547,
#41548,#41549,#41550,#41551,#41552,#41553,#41554,#41555,#41556,#41557,#41558,
#41559,#41560,#41561,#41562,#41563,#41564,#41565,#41566,#41567,#41568,#41569,
#41570,#41571,#41572,#41573,#41574,#41575,#41576,#41577,#41578,#41579,#41580,
#41581,#41582,#41583,#41584,#41585,#41586,#41587,#41588,#41589,#41590,#41591,
#41592,#41593,#41594,#41595,#41596,#41597,#41598),.UNSPECIFIED.,.F.,.F.,
(4,3,3,3,3,3,3,3,3,3,3,3,3,3,3,3,3,3,3,3,3,3,3,3,3,3,3,3,3,3,3,3,3,4),(-0.760759816994606,
-0.728627835147078,-0.695756641029334,-0.686068404654108,-0.679579431591451,
-0.673178914772871,-0.639342167265441,-0.610292596498939,-0.600454878237806,
-0.594751249714991,-0.560217841490549,-0.525200964388687,-0.490288863419066,
-0.469453047847656,-0.455093587171559,-0.450652608595185,-0.414664189190038,
-0.406945601133428,-0.372348180330614,-0.337004219823422,-0.317186773522027,
-0.30892343932953,-0.304448676715557,-0.268404844057691,-0.231699930890561,
-0.194697515735063,-0.172850961143318,-0.161340507514556,-0.156038398693486,
-0.118189758791589,-0.0802679020340656,-0.0429994158654706,-0.0199250790011039,
0.),.UNSPECIFIED.);
#2936=B_SPLINE_CURVE_WITH_KNOTS('',3,(#41599,#41600,#41601,#41602,#41603,
#41604,#41605,#41606,#41607,#41608,#41609,#41610,#41611,#41612,#41613,#41614,
#41615,#41616,#41617,#41618,#41619,#41620,#41621,#41622,#41623,#41624,#41625,
#41626,#41627,#41628,#41629,#41630,#41631,#41632,#41633,#41634,#41635,#41636,
#41637,#41638,#41639,#41640,#41641,#41642,#41643,#41644,#41645,#41646,#41647,
#41648,#41649,#41650,#41651,#41652,#41653,#41654,#41655,#41656,#41657,#41658,
#41659,#41660,#41661,#41662,#41663,#41664,#41665,#41666,#41667,#41668,#41669,
#41670,#41671,#41672,#41673,#41674,#41675,#41676,#41677,#41678,#41679,#41680,
#41681,#41682,#41683,#41684,#41685,#41686,#41687,#41688,#41689,#41690,#41691,
#41692,#41693,#41694,#41695,#41696,#41697,#41698),.UNSPECIFIED.,.F.,.F.,
(4,3,3,3,3,3,3,3,3,3,3,3,3,3,3,3,3,3,3,3,3,3,3,3,3,3,3,3,3,3,3,3,3,4),(-0.75776366468449,
-0.720377652726986,-0.682466667598983,-0.666433073646011,-0.657234612750941,
-0.619826663274133,-0.588739338690156,-0.575138634184666,-0.567711770657871,
-0.562381433308457,-0.525809999923709,-0.489512573327164,-0.454189706368117,
-0.433424296426666,-0.418943939880433,-0.414278005844695,-0.379386455118474,
-0.371128066602313,-0.33572725719849,-0.300034647625018,-0.282321970655644,
-0.275156760805834,-0.270309056596631,-0.235597109555266,-0.200919052556176,
-0.166729839187693,-0.147967586303611,-0.137478173109318,-0.130951778681891,
-0.0975591981658623,-0.0646630732109414,-0.0327161289923639,-0.0166318161150331,
0.),.UNSPECIFIED.);
#2937=B_SPLINE_CURVE_WITH_KNOTS('',3,(#41700,#41701,#41702,#41703,#41704,
#41705,#41706,#41707,#41708,#41709,#41710),.UNSPECIFIED.,.F.,.F.,(4,1,1,
1,1,1,1,1,4),(15.7079632679489,15.7955882081887,16.7801008045318,17.7646134008748,
18.7491259972179,19.733638593561,20.718151189904,21.7026637862471,21.9911485751285),
 .UNSPECIFIED.);
#2938=B_SPLINE_CURVE_WITH_KNOTS('',3,(#41711,#41712,#41713,#41714,#41715,
#41716,#41717,#41718,#41719,#41720),.UNSPECIFIED.,.F.,.F.,(4,1,1,1,1,1,
1,4),(15.7079632679489,16.3681508394037,17.3526634357467,18.3371760320898,
19.3216886284329,20.3062012247759,21.290713821119,21.9911485751285),
 .UNSPECIFIED.);
#2939=B_SPLINE_CURVE_WITH_KNOTS('',3,(#41925,#41926,#41927,#41928,#41929,
#41930,#41931,#41932,#41933,#41934,#41935,#41936,#41937,#41938,#41939,#41940,
#41941,#41942,#41943,#41944,#41945,#41946,#41947,#41948,#41949,#41950,#41951,
#41952,#41953,#41954,#41955,#41956,#41957,#41958,#41959,#41960,#41961,#41962,
#41963,#41964,#41965,#41966,#41967,#41968,#41969,#41970,#41971,#41972,#41973,
#41974,#41975,#41976,#41977,#41978,#41979,#41980,#41981,#41982,#41983,#41984,
#41985,#41986,#41987,#41988,#41989,#41990,#41991,#41992,#41993,#41994,#41995,
#41996,#41997,#41998,#41999,#42000,#42001,#42002,#42003,#42004,#42005,#42006,
#42007,#42008,#42009,#42010,#42011,#42012,#42013,#42014,#42015,#42016,#42017,
#42018),.UNSPECIFIED.,.F.,.F.,(4,3,3,3,3,3,3,3,3,3,3,3,3,3,3,3,3,3,3,3,
3,3,3,3,3,3,3,3,3,3,3,4),(0.,0.0317392926390111,0.06427104971894,0.0974907111890735,
0.129407560650786,0.134009775207885,0.138840345930619,0.172956078855192,
0.207581704666645,0.243892655220677,0.271125868136201,0.277136000189074,
0.312751944561103,0.348252900965451,0.352825506882774,0.387546395149149,
0.409444620986338,0.417180295663684,0.422139723441818,0.457113952190099,
0.493314028911904,0.529906445847685,0.555907891184747,0.563763452421676,
0.571495289748545,0.608811765665218,0.641088326384959,0.655846951854627,
0.662600712364462,0.700434559793948,0.737918008544181,0.757763664684543),
 .UNSPECIFIED.);
#2940=B_SPLINE_CURVE_WITH_KNOTS('',3,(#42019,#42020,#42021,#42022,#42023,
#42024,#42025,#42026,#42027,#42028,#42029,#42030,#42031,#42032,#42033,#42034,
#42035,#42036,#42037,#42038,#42039,#42040,#42041,#42042,#42043),
 .UNSPECIFIED.,.F.,.F.,(4,3,3,3,3,3,3,3,4),(-10.1336107523121,-9.84512596343066,
-8.86061336708759,-7.87610077074453,-6.89158817440147,-5.9070755780584,
-4.92256298171533,-3.93805038537227,-3.85042544513253),.UNSPECIFIED.);
#2941=B_SPLINE_CURVE_WITH_KNOTS('',3,(#42248,#42249,#42250,#42251,#42252,
#42253,#42254,#42255,#42256,#42257,#42258,#42259,#42260,#42261,#42262,#42263,
#42264,#42265,#42266,#42267,#42268,#42269,#42270,#42271,#42272),
 .UNSPECIFIED.,.F.,.F.,(4,3,3,3,3,3,3,3,4),(7.592022928411,7.87610077074452,
8.86061336708759,9.84512596343066,10.8296385597737,11.8141511561168,12.7986637524599,
13.7831763488029,13.8752082355906),.UNSPECIFIED.);
#2942=B_SPLINE_CURVE_WITH_KNOTS('',3,(#42273,#42274,#42275,#42276,#42277,
#42278,#42279,#42280,#42281,#42282,#42283,#42284,#42285,#42286,#42287,#42288,
#42289,#42290,#42291,#42292,#42293,#42294,#42295,#42296,#42297,#42298,#42299,
#42300,#42301,#42302,#42303,#42304,#42305,#42306,#42307,#42308,#42309,#42310,
#42311,#42312,#42313,#42314,#42315,#42316,#42317,#42318,#42319,#42320,#42321,
#42322,#42323,#42324,#42325,#42326,#42327,#42328,#42329,#42330,#42331,#42332,
#42333,#42334,#42335,#42336,#42337,#42338,#42339,#42340,#42341,#42342,#42343,
#42344,#42345,#42346,#42347,#42348,#42349,#42350,#42351,#42352,#42353,#42354,
#42355,#42356,#42357,#42358,#42359,#42360,#42361,#42362,#42363,#42364,#42365,
#42366,#42367,#42368,#42369),.UNSPECIFIED.,.F.,.F.,(4,3,3,3,3,3,3,3,3,3,
3,3,3,3,3,3,3,3,3,3,3,3,3,3,3,3,3,3,3,3,3,3,4),(0.,0.0368231487405989,0.0744314261587949,
0.113698809813578,0.148057770511513,0.15481009538365,0.159905443760235,
0.196856403615778,0.233660968511241,0.269922874636576,0.299584779826697,
0.306586732072781,0.311530477043913,0.34706791893824,0.381889563649704,
0.388570495397059,0.424561733289204,0.444531526044614,0.452400923962074,
0.457441217806984,0.493270867753082,0.528364029290525,0.56305044901109,
0.585678945056675,0.594960393985588,0.600628220264455,0.634676041165029,
0.662026635217714,0.675581361298493,0.683279765486755,0.715772824187495,
0.74407841737577,0.760759816994523),.UNSPECIFIED.);
#2943=B_SPLINE_CURVE_WITH_KNOTS('',3,(#42372,#42373,#42374,#42375,#42376,
#42377,#42378,#42379,#42380,#42381,#42382,#42383,#42384,#42385,#42386,#42387,
#42388,#42389,#42390,#42391,#42392,#42393,#42394,#42395,#42396,#42397,#42398,
#42399,#42400,#42401,#42402,#42403,#42404,#42405,#42406,#42407,#42408,#42409,
#42410,#42411,#42412,#42413,#42414,#42415,#42416,#42417,#42418,#42419,#42420,
#42421,#42422,#42423,#42424,#42425,#42426,#42427,#42428,#42429,#42430,#42431,
#42432,#42433,#42434,#42435,#42436,#42437,#42438,#42439,#42440,#42441,#42442,
#42443,#42444,#42445,#42446,#42447,#42448,#42449,#42450,#42451,#42452,#42453,
#42454,#42455,#42456,#42457,#42458,#42459,#42460,#42461,#42462,#42463,#42464,
#42465,#42466,#42467,#42468,#42469,#42470,#42471),.UNSPECIFIED.,.F.,.F.,
(4,3,3,3,3,3,3,3,3,3,3,3,3,3,3,3,3,3,3,3,3,3,3,3,3,3,3,3,3,3,3,3,3,4),(-0.760759816994564,
-0.728627854008442,-0.695756675766866,-0.686068398368336,-0.679579388481393,
-0.673178910415624,-0.639342175416784,-0.610292603631362,-0.600454896667282,
-0.594751269714701,-0.5602178744711,-0.525201003137007,-0.490288896523447,
-0.469453072675938,-0.45509359744204,-0.450652627702033,-0.414664207509709,
-0.40694560113341,-0.37234816825657,-0.33700419983174,-0.317186754779825,
-0.308923380424535,-0.304448587240479,-0.268404743404054,-0.231699824208938,
-0.194697408001487,-0.172850866876439,-0.161340463279929,-0.156038382119757,
-0.118189740184684,-0.0802678836542896,-0.0429993965311957,-0.0199250790011036,
0.),.UNSPECIFIED.);
#2944=B_SPLINE_CURVE_WITH_KNOTS('',3,(#42472,#42473,#42474,#42475,#42476,
#42477,#42478,#42479,#42480,#42481,#42482,#42483,#42484,#42485,#42486,#42487,
#42488,#42489,#42490,#42491,#42492,#42493,#42494,#42495,#42496,#42497,#42498,
#42499,#42500,#42501,#42502,#42503,#42504,#42505,#42506,#42507,#42508,#42509,
#42510,#42511,#42512,#42513,#42514,#42515,#42516,#42517,#42518,#42519,#42520,
#42521,#42522,#42523,#42524,#42525,#42526,#42527,#42528,#42529,#42530,#42531,
#42532,#42533,#42534,#42535,#42536,#42537,#42538,#42539,#42540,#42541,#42542,
#42543,#42544,#42545,#42546,#42547,#42548,#42549,#42550,#42551,#42552,#42553,
#42554,#42555,#42556,#42557,#42558,#42559,#42560,#42561,#42562,#42563,#42564,
#42565,#42566,#42567,#42568,#42569,#42570,#42571),.UNSPECIFIED.,.F.,.F.,
(4,3,3,3,3,3,3,3,3,3,3,3,3,3,3,3,3,3,3,3,3,3,3,3,3,3,3,3,3,3,3,3,3,4),(-0.757763664684492,
-0.72037767484086,-0.682466697174141,-0.666433210881691,-0.657234612921716,
-0.619826663526386,-0.588739338910877,-0.575138634391592,-0.56771178998584,
-0.562381438442901,-0.525810002728897,-0.48951256756756,-0.454189692426994,
-0.433424285970824,-0.418943941384036,-0.414278009542087,-0.379386449564138,
-0.371128066602314,-0.335727255522783,-0.300034647303691,-0.282321970354399,
-0.2751567520521,-0.270309050351438,-0.235597104423164,-0.200919047261525,
-0.166729828033903,-0.147967576544044,-0.137478161837071,-0.130951777779855,
-0.097559193204338,-0.0646630585919135,-0.0327160968510094,-0.0166318161150306,
0.),.UNSPECIFIED.);
#2945=B_SPLINE_CURVE_WITH_KNOTS('',3,(#42573,#42574,#42575,#42576,#42577,
#42578,#42579,#42580,#42581,#42582,#42583),.UNSPECIFIED.,.F.,.F.,(4,1,1,
1,1,1,1,1,4),(15.7079632679489,15.7955882081887,16.7801008045318,17.7646134008748,
18.7491259972179,19.733638593561,20.718151189904,21.7026637862471,21.9911485751285),
 .UNSPECIFIED.);
#2946=B_SPLINE_CURVE_WITH_KNOTS('',3,(#42584,#42585,#42586,#42587,#42588,
#42589,#42590,#42591,#42592,#42593),.UNSPECIFIED.,.F.,.F.,(4,1,1,1,1,1,
1,4),(15.7079632679489,16.3681508394037,17.3526634357467,18.3371760320898,
19.3216886284329,20.3062012247759,21.290713821119,21.9911485751285),
 .UNSPECIFIED.);
#2947=B_SPLINE_CURVE_WITH_KNOTS('',3,(#42798,#42799,#42800,#42801,#42802,
#42803,#42804,#42805,#42806,#42807,#42808,#42809,#42810,#42811,#42812,#42813,
#42814,#42815,#42816,#42817,#42818,#42819,#42820,#42821,#42822,#42823,#42824,
#42825,#42826,#42827,#42828,#42829,#42830,#42831,#42832,#42833,#42834,#42835,
#42836,#42837,#42838,#42839,#42840,#42841,#42842,#42843,#42844,#42845,#42846,
#42847,#42848,#42849,#42850,#42851,#42852,#42853,#42854,#42855,#42856,#42857,
#42858,#42859,#42860,#42861,#42862,#42863,#42864,#42865,#42866,#42867,#42868,
#42869,#42870,#42871,#42872,#42873,#42874,#42875,#42876,#42877,#42878,#42879,
#42880,#42881,#42882,#42883,#42884,#42885,#42886,#42887,#42888,#42889,#42890,
#42891),.UNSPECIFIED.,.F.,.F.,(4,3,3,3,3,3,3,3,3,3,3,3,3,3,3,3,3,3,3,3,
3,3,3,3,3,3,3,3,3,3,3,4),(0.,0.0317392578223645,0.0642709833499116,0.0974906209103936,
0.129407481656942,0.134009658091857,0.138840325560996,0.172956034648678,
0.20758164844901,0.243892613057452,0.271125836513783,0.277135986973077,
0.312751925881509,0.348252892065859,0.352825506882778,0.387546411589169,
0.409444636398856,0.417180309631433,0.422139749096638,0.45711400101409,
0.493314088775489,0.529906509036106,0.555907946474613,0.56376389125674,
0.571495247015118,0.608811726985233,0.641088297374965,0.655846945118752,
0.662600708826001,0.700434555809607,0.73791800854416,0.757763664684518),
 .UNSPECIFIED.);
#2948=B_SPLINE_CURVE_WITH_KNOTS('',3,(#42892,#42893,#42894,#42895,#42896,
#42897,#42898,#42899,#42900,#42901,#42902,#42903,#42904,#42905,#42906,#42907,
#42908,#42909,#42910,#42911,#42912,#42913,#42914,#42915,#42916),
 .UNSPECIFIED.,.F.,.F.,(4,3,3,3,3,3,3,3,4),(-10.1336107523121,-9.84512596343066,
-8.86061336708759,-7.87610077074453,-6.89158817440146,-5.9070755780584,
-4.92256298171533,-3.93805038537226,-3.85042544513253),.UNSPECIFIED.);
#2949=B_SPLINE_CURVE_WITH_KNOTS('',3,(#43121,#43122,#43123,#43124,#43125,
#43126,#43127,#43128,#43129,#43130,#43131,#43132,#43133,#43134,#43135,#43136,
#43137,#43138,#43139,#43140,#43141,#43142,#43143,#43144,#43145),
 .UNSPECIFIED.,.F.,.F.,(4,3,3,3,3,3,3,3,4),(7.592022928411,7.87610077074453,
8.8606133670876,9.84512596343066,10.8296385597737,11.8141511561168,12.7986637524599,
13.7831763488029,13.8752082355906),.UNSPECIFIED.);
#2950=B_SPLINE_CURVE_WITH_KNOTS('',3,(#43146,#43147,#43148,#43149,#43150,
#43151,#43152,#43153,#43154,#43155,#43156,#43157,#43158,#43159,#43160,#43161,
#43162,#43163,#43164,#43165,#43166,#43167,#43168,#43169,#43170,#43171,#43172,
#43173,#43174,#43175,#43176,#43177,#43178,#43179,#43180,#43181,#43182,#43183,
#43184,#43185,#43186,#43187,#43188,#43189,#43190,#43191,#43192,#43193,#43194,
#43195,#43196,#43197,#43198,#43199,#43200,#43201,#43202,#43203,#43204,#43205,
#43206,#43207,#43208,#43209,#43210,#43211,#43212,#43213,#43214,#43215,#43216,
#43217,#43218,#43219,#43220,#43221,#43222,#43223,#43224,#43225,#43226,#43227,
#43228,#43229,#43230,#43231,#43232,#43233,#43234,#43235,#43236,#43237,#43238,
#43239,#43240,#43241,#43242),.UNSPECIFIED.,.F.,.F.,(4,3,3,3,3,3,3,3,3,3,
3,3,3,3,3,3,3,3,3,3,3,3,3,3,3,3,3,3,3,3,3,3,4),(0.,0.0368231320265742,0.0744314002406353,
0.113698787135186,0.148057750667918,0.154809920619753,0.159905372006135,
0.196856331004292,0.233660900681144,0.269922813568411,0.299584734025569,
0.306586611813478,0.311530355932456,0.347067804301497,0.381889455018008,
0.388570495397043,0.424561732757698,0.444531525546326,0.452400921561243,
0.457441217682179,0.493270867643875,0.528364028783657,0.563050450927217,
0.585678946733283,0.594960344676032,0.600628213104039,0.634676035977772,
0.662026631327266,0.675581362311545,0.683279766638027,0.715772832870445,
0.744078417375749,0.7607598169945),.UNSPECIFIED.);
#2951=B_SPLINE_CURVE_WITH_KNOTS('',3,(#43271,#43272,#43273,#43274,#43275,
#43276,#43277,#43278,#43279,#43280,#43281,#43282,#43283,#43284,#43285,#43286,
#43287,#43288,#43289,#43290,#43291,#43292,#43293,#43294,#43295,#43296,#43297,
#43298),.UNSPECIFIED.,.F.,.F.,(4,3,3,3,3,3,3,3,3,4),(177.238751742006,177.553807102306,
178.05255375147,178.551300400634,179.050047049798,179.548793698961,180.047540348125,
180.546286997289,181.045033646453,181.543780295616),.UNSPECIFIED.);
#2952=B_SPLINE_CURVE_WITH_KNOTS('',3,(#43301,#43302,#43303,#43304,#43305,
#43306,#43307,#43308,#43309,#43310,#43311,#43312,#43313,#43314,#43315,#43316,
#43317,#43318,#43319,#43320,#43321,#43322,#43323,#43324,#43325,#43326,#43327,
#43328,#43329,#43330,#43331,#43332,#43333,#43334,#43335,#43336,#43337,#43338,
#43339,#43340),.UNSPECIFIED.,.F.,.F.,(4,3,3,3,3,3,3,3,3,3,3,3,3,4),(-179.519580205131,
-179.050047049798,-178.551300400634,-178.05255375147,-177.553807102306,
-177.055060453142,-176.556313803979,-176.057567154815,-175.558820505651,
-175.060073856487,-174.561327207324,-174.06258055816,-173.563833908996,
-173.502232896947),.UNSPECIFIED.);
#2953=B_SPLINE_CURVE_WITH_KNOTS('',3,(#43345,#43346,#43347,#43348,#43349,
#43350,#43351,#43352,#43353,#43354,#43355,#43356,#43357,#43358,#43359,#43360,
#43361,#43362,#43363,#43364,#43365,#43366,#43367,#43368,#43369,#43370,#43371,
#43372,#43373,#43374,#43375,#43376,#43377,#43378,#43379,#43380,#43381,#43382,
#43383,#43384,#43385,#43386,#43387),.UNSPECIFIED.,.F.,.F.,(4,3,3,3,3,3,
3,3,3,3,3,3,3,3,4),(170.955566434826,171.070100663177,171.568847312341,
172.067593961505,172.566340610668,173.065087259832,173.563833908996,174.06258055816,
174.561327207323,175.060073856487,175.558820505651,176.057567154815,176.556313803979,
177.055060453142,177.238751742006),.UNSPECIFIED.);
#2954=B_SPLINE_CURVE_WITH_KNOTS('',3,(#43388,#43389,#43390,#43391,#43392,
#43393,#43394,#43395,#43396,#43397,#43398,#43399,#43400,#43401,#43402,#43403,
#43404,#43405,#43406,#43407,#43408,#43409,#43410,#43411,#43412,#43413,#43414,
#43415,#43416,#43417,#43418,#43419,#43420,#43421,#43422,#43423,#43424,#43425,
#43426,#43427),.UNSPECIFIED.,.F.,.F.,(4,3,3,3,3,3,3,3,3,3,3,3,3,4),(-173.502232896947,
-173.065087259832,-172.566340610668,-172.067593961505,-171.568847312341,
-171.070100663177,-170.571354014013,-170.072607364849,-169.573860715686,
-169.075114066522,-168.576367417358,-168.077620768194,-167.578874119031,
-167.219047589767),.UNSPECIFIED.);
#2955=B_SPLINE_CURVE_WITH_KNOTS('',3,(#43432,#43433,#43434,#43435,#43436,
#43437,#43438,#43439,#43440,#43441,#43442,#43443,#43444,#43445,#43446,#43447,
#43448,#43449,#43450,#43451,#43452,#43453,#43454,#43455,#43456,#43457,#43458,
#43459,#43460,#43461,#43462,#43463,#43464,#43465,#43466,#43467,#43468,#43469,
#43470,#43471),.UNSPECIFIED.,.F.,.F.,(4,3,3,3,3,3,3,3,3,3,3,3,3,4),(164.672381127646,
165.085140873212,165.583887522375,166.082634171539,166.581380820703,167.080127469867,
167.578874119031,168.077620768194,168.576367417358,169.075114066522,169.573860715686,
170.072607364849,170.571354014013,170.955566434826),.UNSPECIFIED.);
#2956=B_SPLINE_CURVE_WITH_KNOTS('',3,(#43472,#43473,#43474,#43475,#43476,
#43477,#43478,#43479,#43480,#43481,#43482,#43483,#43484,#43485,#43486,#43487,
#43488,#43489,#43490,#43491,#43492,#43493,#43494,#43495,#43496,#43497,#43498,
#43499,#43500,#43501,#43502,#43503,#43504,#43505,#43506,#43507,#43508,#43509,
#43510,#43511,#43512,#43513,#43514),.UNSPECIFIED.,.F.,.F.,(4,3,3,3,3,3,
3,3,3,3,3,3,3,3,4),(-167.219047589767,-167.080127469867,-166.581380820703,
-166.082634171539,-165.583887522375,-165.085140873212,-164.586394224048,
-164.087647574884,-163.58890092572,-163.090154276557,-162.591407627393,
-162.092660978229,-161.593914329065,-161.095167679901,-160.935862282588),
 .UNSPECIFIED.);
#2957=B_SPLINE_CURVE_WITH_KNOTS('',3,(#43519,#43520,#43521,#43522,#43523,
#43524,#43525,#43526,#43527,#43528,#43529,#43530,#43531,#43532,#43533,#43534,
#43535,#43536,#43537,#43538,#43539,#43540,#43541,#43542,#43543,#43544,#43545,
#43546,#43547,#43548,#43549,#43550,#43551,#43552,#43553,#43554,#43555,#43556,
#43557,#43558,#43559,#43560,#43561),.UNSPECIFIED.,.F.,.F.,(4,3,3,3,3,3,
3,3,3,3,3,3,3,3,4),(158.389195820467,158.601434434082,159.100181083246,
159.59892773241,160.097674381574,160.596421030738,161.095167679901,161.593914329065,
162.092660978229,162.591407627393,163.090154276556,163.58890092572,164.087647574884,
164.586394224048,164.672381127646),.UNSPECIFIED.);
#2958=B_SPLINE_CURVE_WITH_KNOTS('',3,(#43562,#43563,#43564,#43565,#43566,
#43567,#43568,#43569,#43570,#43571,#43572,#43573,#43574,#43575,#43576,#43577,
#43578,#43579,#43580,#43581,#43582,#43583,#43584,#43585,#43586,#43587,#43588,
#43589,#43590,#43591,#43592,#43593,#43594,#43595,#43596,#43597,#43598,#43599,
#43600,#43601),.UNSPECIFIED.,.F.,.F.,(4,3,3,3,3,3,3,3,3,3,3,3,3,4),(-160.935862282588,
-160.596421030738,-160.097674381574,-159.59892773241,-159.100181083246,
-158.601434434082,-158.102687784919,-157.603941135755,-157.105194486591,
-156.606447837427,-156.107701188264,-155.6089545391,-155.110207889936,-154.652676975408),
 .UNSPECIFIED.);
#2959=B_SPLINE_CURVE_WITH_KNOTS('',3,(#43606,#43607,#43608,#43609,#43610,
#43611,#43612,#43613,#43614,#43615,#43616,#43617,#43618,#43619,#43620,#43621,
#43622,#43623,#43624,#43625,#43626,#43627,#43628,#43629,#43630,#43631,#43632,
#43633,#43634,#43635,#43636,#43637,#43638,#43639,#43640,#43641,#43642,#43643,
#43644,#43645,#43646,#43647,#43648),.UNSPECIFIED.,.F.,.F.,(4,3,3,3,3,3,
3,3,3,3,3,3,3,3,4),(152.106010513287,152.117727994953,152.616474644117,
153.115221293281,153.613967942445,154.112714591608,154.611461240772,155.110207889936,
155.6089545391,156.107701188264,156.606447837427,157.105194486591,157.603941135755,
158.102687784919,158.389195820467),.UNSPECIFIED.);
#2960=B_SPLINE_CURVE_WITH_KNOTS('',3,(#43649,#43650,#43651,#43652,#43653,
#43654,#43655,#43656,#43657,#43658,#43659,#43660,#43661,#43662,#43663,#43664,
#43665,#43666,#43667,#43668,#43669,#43670,#43671,#43672,#43673,#43674,#43675,
#43676,#43677,#43678,#43679,#43680,#43681,#43682,#43683,#43684,#43685,#43686,
#43687,#43688,#43689,#43690,#43691),.UNSPECIFIED.,.F.,.F.,(4,3,3,3,3,3,
3,3,3,3,3,3,3,3,4),(-154.652676975408,-154.611461240772,-154.112714591608,
-153.613967942445,-153.115221293281,-152.616474644117,-152.117727994953,
-151.61898134579,-151.120234696626,-150.621488047462,-150.122741398298,
-149.623994749134,-149.125248099971,-148.626501450807,-148.369491668229),
 .UNSPECIFIED.);
#2961=B_SPLINE_CURVE_WITH_KNOTS('',3,(#43696,#43697,#43698,#43699,#43700,
#43701,#43702,#43703,#43704,#43705,#43706,#43707,#43708,#43709,#43710,#43711,
#43712,#43713,#43714,#43715,#43716,#43717,#43718,#43719,#43720,#43721,#43722,
#43723,#43724,#43725,#43726,#43727,#43728,#43729,#43730,#43731,#43732,#43733,
#43734,#43735),.UNSPECIFIED.,.F.,.F.,(4,3,3,3,3,3,3,3,3,3,3,3,3,4),(145.822825206108,
146.132768204988,146.631514854152,147.130261503315,147.629008152479,148.127754801643,
148.626501450807,149.125248099971,149.623994749134,150.122741398298,150.621488047462,
151.120234696626,151.61898134579,152.106010513287),.UNSPECIFIED.);
#2962=B_SPLINE_CURVE_WITH_KNOTS('',3,(#43736,#43737,#43738,#43739,#43740,
#43741,#43742,#43743,#43744,#43745,#43746,#43747,#43748,#43749,#43750,#43751,
#43752,#43753,#43754,#43755,#43756,#43757,#43758,#43759,#43760,#43761,#43762,
#43763,#43764,#43765,#43766,#43767,#43768,#43769,#43770,#43771,#43772,#43773,
#43774,#43775,#43776,#43777,#43778),.UNSPECIFIED.,.F.,.F.,(4,3,3,3,3,3,
3,3,3,3,3,3,3,3,4),(-148.369491668229,-148.127754801643,-147.629008152479,
-147.130261503316,-146.631514854152,-146.132768204988,-145.634021555824,
-145.13527490666,-144.636528257497,-144.137781608333,-143.639034959169,
-143.140288310005,-142.641541660841,-142.142795011678,-142.086306361049),
 .UNSPECIFIED.);
#2963=B_SPLINE_CURVE_WITH_KNOTS('',3,(#43783,#43784,#43785,#43786,#43787,
#43788,#43789,#43790,#43791,#43792,#43793,#43794,#43795,#43796,#43797,#43798,
#43799,#43800,#43801,#43802,#43803,#43804,#43805,#43806,#43807,#43808,#43809,
#43810,#43811,#43812,#43813,#43814,#43815,#43816,#43817,#43818,#43819,#43820,
#43821,#43822,#43823,#43824,#43825),.UNSPECIFIED.,.F.,.F.,(4,3,3,3,3,3,
3,3,3,3,3,3,3,3,4),(139.539639898928,139.649061765859,140.147808415023,
140.646555064186,141.14530171335,141.644048362514,142.142795011678,142.641541660841,
143.140288310005,143.639034959169,144.137781608333,144.636528257497,145.13527490666,
145.634021555824,145.822825206108),.UNSPECIFIED.);
#2964=B_SPLINE_CURVE_WITH_KNOTS('',3,(#43826,#43827,#43828,#43829,#43830,
#43831,#43832,#43833,#43834,#43835,#43836,#43837,#43838,#43839,#43840,#43841,
#43842,#43843,#43844,#43845,#43846,#43847,#43848,#43849,#43850,#43851,#43852,
#43853,#43854,#43855,#43856,#43857,#43858,#43859,#43860,#43861,#43862,#43863,
#43864,#43865),.UNSPECIFIED.,.F.,.F.,(4,3,3,3,3,3,3,3,3,3,3,3,3,4),(-142.086306361049,
-141.644048362514,-141.14530171335,-140.646555064186,-140.147808415023,
-139.649061765859,-139.150315116695,-138.651568467531,-138.152821818367,
-137.654075169204,-137.15532852004,-136.656581870876,-136.157835221712,
-135.80312105387),.UNSPECIFIED.);
#2965=B_SPLINE_CURVE_WITH_KNOTS('',3,(#43870,#43871,#43872,#43873,#43874,
#43875,#43876,#43877,#43878,#43879,#43880,#43881,#43882,#43883,#43884,#43885,
#43886,#43887,#43888,#43889,#43890,#43891,#43892,#43893,#43894,#43895,#43896,
#43897,#43898,#43899,#43900,#43901,#43902,#43903,#43904,#43905,#43906,#43907,
#43908,#43909),.UNSPECIFIED.,.F.,.F.,(4,3,3,3,3,3,3,3,3,3,3,3,3,4),(133.256454591749,
133.664101975893,134.162848625057,134.661595274221,135.160341923385,135.659088572549,
136.157835221712,136.656581870876,137.15532852004,137.654075169204,138.152821818367,
138.651568467531,139.150315116695,139.539639898928),.UNSPECIFIED.);
#2966=B_SPLINE_CURVE_WITH_KNOTS('',3,(#43910,#43911,#43912,#43913,#43914,
#43915,#43916,#43917,#43918,#43919,#43920,#43921,#43922,#43923,#43924,#43925,
#43926,#43927,#43928,#43929,#43930,#43931,#43932,#43933,#43934,#43935,#43936,
#43937,#43938,#43939,#43940,#43941,#43942,#43943,#43944,#43945,#43946,#43947,
#43948,#43949,#43950,#43951,#43952),.UNSPECIFIED.,.F.,.F.,(4,3,3,3,3,3,
3,3,3,3,3,3,3,3,4),(-135.80312105387,-135.659088572549,-135.160341923385,
-134.661595274221,-134.162848625057,-133.664101975893,-133.16535532673,
-132.666608677566,-132.167862028402,-131.669115379238,-131.170368730075,
-130.671622080911,-130.172875431747,-129.674128782583,-129.51993574669),
 .UNSPECIFIED.);
#2967=B_SPLINE_CURVE_WITH_KNOTS('',3,(#43957,#43958,#43959,#43960,#43961,
#43962,#43963,#43964,#43965,#43966,#43967,#43968,#43969,#43970,#43971,#43972,
#43973,#43974,#43975,#43976,#43977,#43978,#43979,#43980,#43981,#43982,#43983,
#43984,#43985,#43986,#43987,#43988,#43989,#43990,#43991,#43992,#43993,#43994,
#43995,#43996,#43997,#43998,#43999),.UNSPECIFIED.,.F.,.F.,(4,3,3,3,3,3,
3,3,3,3,3,3,3,3,4),(126.973269284569,127.180395536764,127.679142185928,
128.177888835092,128.676635484256,129.175382133419,129.674128782583,130.172875431747,
130.671622080911,131.170368730074,131.669115379238,132.167862028402,132.666608677566,
133.16535532673,133.256454591749),.UNSPECIFIED.);
#2968=B_SPLINE_CURVE_WITH_KNOTS('',3,(#44000,#44001,#44002,#44003,#44004,
#44005,#44006,#44007,#44008,#44009,#44010,#44011,#44012,#44013,#44014,#44015,
#44016,#44017,#44018,#44019,#44020,#44021,#44022,#44023,#44024,#44025,#44026,
#44027,#44028,#44029,#44030,#44031,#44032,#44033,#44034,#44035,#44036,#44037,
#44038,#44039),.UNSPECIFIED.,.F.,.F.,(4,3,3,3,3,3,3,3,3,3,3,3,3,4),(-129.51993574669,
-129.175382133419,-128.676635484256,-128.177888835092,-127.679142185928,
-127.180395536764,-126.6816488876,-126.182902238437,-125.684155589273,-125.185408940109,
-124.686662290945,-124.187915641782,-123.689168992618,-123.23675043951),
 .UNSPECIFIED.);
#2969=B_SPLINE_CURVE_WITH_KNOTS('',3,(#44044,#44045,#44046,#44047,#44048,
#44049,#44050,#44051,#44052,#44053,#44054,#44055,#44056,#44057,#44058,#44059,
#44060,#44061,#44062,#44063,#44064,#44065,#44066,#44067,#44068,#44069,#44070,
#44071,#44072,#44073,#44074,#44075,#44076,#44077,#44078,#44079,#44080,#44081,
#44082,#44083,#44084,#44085,#44086),.UNSPECIFIED.,.F.,.F.,(4,3,3,3,3,3,
3,3,3,3,3,3,3,3,4),(120.690083977389,120.696689097635,121.195435746799,
121.694182395963,122.192929045126,122.69167569429,123.190422343454,123.689168992618,
124.187915641782,124.686662290945,125.185408940109,125.684155589273,126.182902238437,
126.6816488876,126.973269284569),.UNSPECIFIED.);
#2970=B_SPLINE_CURVE_WITH_KNOTS('',3,(#44087,#44088,#44089,#44090,#44091,
#44092,#44093,#44094,#44095,#44096,#44097,#44098,#44099,#44100,#44101,#44102,
#44103,#44104,#44105,#44106,#44107,#44108,#44109,#44110,#44111,#44112,#44113,
#44114,#44115,#44116,#44117,#44118,#44119,#44120,#44121,#44122,#44123,#44124,
#44125,#44126,#44127,#44128,#44129),.UNSPECIFIED.,.F.,.F.,(4,3,3,3,3,3,
3,3,3,3,3,3,3,3,4),(-123.23675043951,-123.190422343454,-122.69167569429,
-122.192929045126,-121.694182395963,-121.195435746799,-120.696689097635,
-120.197942448471,-119.699195799308,-119.200449150144,-118.70170250098,
-118.202955851816,-117.704209202652,-117.205462553489,-116.953565132331),
 .UNSPECIFIED.);
#2971=B_SPLINE_CURVE_WITH_KNOTS('',3,(#44134,#44135,#44136,#44137,#44138,
#44139,#44140,#44141,#44142,#44143,#44144,#44145,#44146,#44147,#44148,#44149,
#44150,#44151,#44152,#44153,#44154,#44155,#44156,#44157,#44158,#44159,#44160,
#44161,#44162,#44163,#44164,#44165,#44166,#44167,#44168,#44169,#44170,#44171,
#44172,#44173),.UNSPECIFIED.,.F.,.F.,(4,3,3,3,3,3,3,3,3,3,3,3,3,4),(114.40689867021,
114.71172930767,115.210475956833,115.709222605997,116.207969255161,116.706715904325,
117.205462553489,117.704209202652,118.202955851816,118.70170250098,119.200449150144,
119.699195799308,120.197942448471,120.690083977389),.UNSPECIFIED.);
#2972=B_SPLINE_CURVE_WITH_KNOTS('',3,(#44174,#44175,#44176,#44177,#44178,
#44179,#44180,#44181,#44182,#44183,#44184,#44185,#44186,#44187,#44188,#44189,
#44190,#44191,#44192,#44193,#44194,#44195,#44196,#44197,#44198,#44199,#44200,
#44201,#44202,#44203,#44204,#44205,#44206,#44207,#44208,#44209,#44210,#44211,
#44212,#44213,#44214,#44215,#44216),.UNSPECIFIED.,.F.,.F.,(4,3,3,3,3,3,
3,3,3,3,3,3,3,3,4),(-116.953565132331,-116.706715904325,-116.207969255161,
-115.709222605997,-115.210475956834,-114.71172930767,-114.212982658506,
-113.714236009342,-113.215489360178,-112.716742711015,-112.217996061851,
-111.719249412687,-111.220502763523,-110.721756114359,-110.670379825151),
 .UNSPECIFIED.);
#2973=B_SPLINE_CURVE_WITH_KNOTS('',3,(#44221,#44222,#44223,#44224,#44225,
#44226,#44227,#44228,#44229,#44230,#44231,#44232,#44233,#44234,#44235,#44236,
#44237,#44238,#44239,#44240,#44241,#44242,#44243,#44244,#44245,#44246,#44247,
#44248,#44249,#44250,#44251,#44252,#44253,#44254,#44255,#44256,#44257,#44258,
#44259,#44260,#44261,#44262,#44263),.UNSPECIFIED.,.F.,.F.,(4,3,3,3,3,3,
3,3,3,3,3,3,3,3,4),(108.12371336303,108.228022868541,108.726769517704,109.225516166868,
109.724262816032,110.223009465196,110.721756114359,111.220502763523,111.719249412687,
112.217996061851,112.716742711015,113.215489360178,113.714236009342,114.212982658506,
114.40689867021),.UNSPECIFIED.);
#2974=B_SPLINE_CURVE_WITH_KNOTS('',3,(#44264,#44265,#44266,#44267,#44268,
#44269,#44270,#44271,#44272,#44273,#44274,#44275,#44276,#44277,#44278,#44279,
#44280,#44281,#44282,#44283,#44284,#44285,#44286,#44287,#44288,#44289,#44290,
#44291,#44292,#44293,#44294,#44295,#44296,#44297,#44298,#44299,#44300,#44301,
#44302,#44303),.UNSPECIFIED.,.F.,.F.,(4,3,3,3,3,3,3,3,3,3,3,3,3,4),(-110.670379825151,
-110.223009465196,-109.724262816032,-109.225516166868,-108.726769517704,
-108.228022868541,-107.729276219377,-107.230529570213,-106.731782921049,
-106.233036271885,-105.734289622722,-105.235542973558,-104.736796324394,
-104.387194517972),.UNSPECIFIED.);
#2975=B_SPLINE_CURVE_WITH_KNOTS('',3,(#44308,#44309,#44310,#44311,#44312,
#44313,#44314,#44315,#44316,#44317,#44318,#44319,#44320,#44321,#44322,#44323,
#44324,#44325,#44326,#44327,#44328,#44329,#44330,#44331,#44332,#44333,#44334,
#44335,#44336,#44337,#44338,#44339,#44340,#44341,#44342,#44343,#44344,#44345,
#44346,#44347),.UNSPECIFIED.,.F.,.F.,(4,3,3,3,3,3,3,3,3,3,3,3,3,4),(101.840528055851,
102.243063078575,102.741809727739,103.240556376903,103.739303026067,104.23804967523,
104.736796324394,105.235542973558,105.734289622722,106.233036271885,106.731782921049,
107.230529570213,107.729276219377,108.12371336303),.UNSPECIFIED.);
#2976=B_SPLINE_CURVE_WITH_KNOTS('',3,(#44348,#44349,#44350,#44351,#44352,
#44353,#44354,#44355,#44356,#44357,#44358,#44359,#44360,#44361,#44362,#44363,
#44364,#44365,#44366,#44367,#44368,#44369,#44370,#44371,#44372,#44373,#44374,
#44375,#44376,#44377,#44378,#44379,#44380,#44381,#44382,#44383,#44384,#44385,
#44386,#44387,#44388,#44389,#44390),.UNSPECIFIED.,.F.,.F.,(4,3,3,3,3,3,
3,3,3,3,3,3,3,3,4),(-104.387194517972,-104.23804967523,-103.739303026067,
-103.240556376903,-102.741809727739,-102.243063078575,-101.744316429411,
-101.245569780248,-100.746823131084,-100.24807648192,-99.7493298327563,
-99.2505831835925,-98.7518365344287,-98.2530898852649,-98.104009210792),
 .UNSPECIFIED.);
#2977=B_SPLINE_CURVE_WITH_KNOTS('',3,(#44395,#44396,#44397,#44398,#44399,
#44400,#44401,#44402,#44403,#44404,#44405,#44406,#44407,#44408,#44409,#44410,
#44411,#44412,#44413,#44414,#44415,#44416,#44417,#44418,#44419,#44420,#44421,
#44422,#44423,#44424,#44425,#44426,#44427,#44428,#44429,#44430,#44431,#44432,
#44433,#44434,#44435,#44436,#44437),.UNSPECIFIED.,.F.,.F.,(4,3,3,3,3,3,
3,3,3,3,3,3,3,3,4),(95.557342748671,95.759356639446,96.2581032886098,96.7568499377736,
97.2555965869374,97.7543432361011,98.2530898852649,98.7518365344287,99.2505831835925,
99.7493298327563,100.24807648192,100.746823131084,101.245569780248,101.744316429411,
101.840528055851),.UNSPECIFIED.);
#2978=B_SPLINE_CURVE_WITH_KNOTS('',3,(#44438,#44439,#44440,#44441,#44442,
#44443,#44444,#44445,#44446,#44447,#44448,#44449,#44450,#44451,#44452,#44453,
#44454,#44455,#44456,#44457,#44458,#44459,#44460,#44461,#44462,#44463,#44464,
#44465,#44466,#44467,#44468,#44469,#44470,#44471,#44472,#44473,#44474,#44475,
#44476,#44477),.UNSPECIFIED.,.F.,.F.,(4,3,3,3,3,3,3,3,3,3,3,3,3,4),(-98.104009210792,
-97.7543432361011,-97.2555965869374,-96.7568499377736,-96.2581032886098,
-95.759356639446,-95.2606099902822,-94.7618633411185,-94.2631166919547,
-93.7643700427909,-93.2656233936271,-92.7668767444633,-92.2681300952996,
-91.8208239036124),.UNSPECIFIED.);
#2979=B_SPLINE_CURVE_WITH_KNOTS('',3,(#44482,#44483,#44484,#44485,#44486,
#44487,#44488,#44489,#44490,#44491,#44492,#44493,#44494,#44495,#44496,#44497,
#44498,#44499,#44500,#44501,#44502,#44503,#44504,#44505,#44506,#44507,#44508,
#44509,#44510,#44511,#44512,#44513,#44514,#44515,#44516,#44517,#44518,#44519,
#44520,#44521),.UNSPECIFIED.,.F.,.F.,(4,3,3,3,3,3,3,3,3,3,3,3,3,4),(89.2741574414915,
89.7743968494806,90.2731434986444,90.7718901478082,91.270636796972,91.7693834461358,
92.2681300952995,92.7668767444633,93.2656233936271,93.7643700427909,94.2631166919547,
94.7618633411184,95.2606099902822,95.557342748671),.UNSPECIFIED.);
#2980=B_SPLINE_CURVE_WITH_KNOTS('',3,(#44522,#44523,#44524,#44525,#44526,
#44527,#44528,#44529,#44530,#44531,#44532,#44533,#44534,#44535,#44536,#44537,
#44538,#44539,#44540,#44541,#44542,#44543,#44544,#44545,#44546,#44547,#44548,
#44549,#44550,#44551,#44552,#44553,#44554,#44555,#44556,#44557,#44558,#44559,
#44560,#44561,#44562,#44563,#44564),.UNSPECIFIED.,.F.,.F.,(4,3,3,3,3,3,
3,3,3,3,3,3,3,3,4),(-91.8208239036124,-91.7693834461358,-91.270636796972,
-90.7718901478082,-90.2731434986444,-89.7743968494807,-89.2756502003169,
-88.7769035511531,-88.2781569019893,-87.7794102528255,-87.2806636036618,
-86.781916954498,-86.2831703053342,-85.7844236561704,-85.5376385964328),
 .UNSPECIFIED.);
#2981=B_SPLINE_CURVE_WITH_KNOTS('',3,(#44569,#44570,#44571,#44572,#44573,
#44574,#44575,#44576,#44577,#44578,#44579,#44580,#44581,#44582,#44583,#44584,
#44585,#44586,#44587,#44588,#44589,#44590,#44591,#44592,#44593,#44594,#44595,
#44596,#44597,#44598,#44599,#44600,#44601,#44602,#44603,#44604,#44605,#44606,
#44607,#44608),.UNSPECIFIED.,.F.,.F.,(4,3,3,3,3,3,3,3,3,3,3,3,3,4),(82.9909721343118,
83.2906904103515,83.7894370595153,84.288183708679,84.7869303578428,85.2856770070066,
85.7844236561704,86.2831703053342,86.7819169544979,87.2806636036617,87.7794102528255,
88.2781569019893,88.7769035511531,89.2741574414915),.UNSPECIFIED.);
#2982=B_SPLINE_CURVE_WITH_KNOTS('',3,(#44609,#44610,#44611,#44612,#44613,
#44614,#44615,#44616,#44617,#44618,#44619,#44620,#44621,#44622,#44623,#44624,
#44625,#44626,#44627,#44628,#44629,#44630,#44631,#44632,#44633,#44634,#44635,
#44636,#44637,#44638,#44639,#44640,#44641,#44642,#44643,#44644,#44645,#44646,
#44647,#44648,#44649,#44650,#44651),.UNSPECIFIED.,.F.,.F.,(4,3,3,3,3,3,
3,3,3,3,3,3,3,3,4),(-85.5376385964328,-85.2856770070066,-84.7869303578428,
-84.2881837086791,-83.7894370595153,-83.2906904103515,-82.7919437611877,
-82.2931971120239,-81.7944504628602,-81.2957038136964,-80.7969571645326,
-80.2982105153688,-79.799463866205,-79.3007172170413,-79.2544532892532),
 .UNSPECIFIED.);
#2983=B_SPLINE_CURVE_WITH_KNOTS('',3,(#44656,#44657,#44658,#44659,#44660,
#44661,#44662,#44663,#44664,#44665,#44666,#44667,#44668,#44669,#44670,#44671,
#44672,#44673,#44674,#44675,#44676,#44677,#44678,#44679,#44680,#44681,#44682,
#44683,#44684,#44685,#44686,#44687,#44688,#44689,#44690,#44691,#44692,#44693,
#44694,#44695,#44696,#44697,#44698),.UNSPECIFIED.,.F.,.F.,(4,3,3,3,3,3,
3,3,3,3,3,3,3,3,4),(76.7077868271323,76.8069839712223,77.3057306203861,
77.8044772695499,78.3032239187137,78.8019705678775,79.3007172170412,79.799463866205,
80.2982105153688,80.7969571645326,81.2957038136963,81.7944504628601,82.2931971120239,
82.7919437611877,82.9909721343118),.UNSPECIFIED.);
#2984=B_SPLINE_CURVE_WITH_KNOTS('',3,(#44699,#44700,#44701,#44702,#44703,
#44704,#44705,#44706,#44707,#44708,#44709,#44710,#44711,#44712,#44713,#44714,
#44715,#44716,#44717,#44718,#44719,#44720,#44721,#44722,#44723,#44724,#44725,
#44726,#44727,#44728,#44729,#44730,#44731,#44732,#44733,#44734,#44735,#44736,
#44737,#44738),.UNSPECIFIED.,.F.,.F.,(4,3,3,3,3,3,3,3,3,3,3,3,3,4),(-79.2544532892532,
-78.8019705678775,-78.3032239187137,-77.8044772695499,-77.3057306203861,
-76.8069839712224,-76.3082373220585,-75.8094906728948,-75.310744023731,
-74.8119973745672,-74.3132507254034,-73.8145040762396,-73.3157574270759,
-72.9712679820736),.UNSPECIFIED.);
#2985=B_SPLINE_CURVE_WITH_KNOTS('',3,(#44743,#44744,#44745,#44746,#44747,
#44748,#44749,#44750,#44751,#44752,#44753,#44754,#44755,#44756,#44757,#44758,
#44759,#44760,#44761,#44762,#44763,#44764,#44765,#44766,#44767,#44768,#44769,
#44770,#44771,#44772,#44773,#44774,#44775,#44776,#44777,#44778,#44779,#44780,
#44781,#44782),.UNSPECIFIED.,.F.,.F.,(4,3,3,3,3,3,3,3,3,3,3,3,3,4),(70.4246015199527,
70.8220241812569,71.3207708304207,71.8195174795845,72.3182641287483,72.8170107779121,
73.3157574270759,73.8145040762396,74.3132507254034,74.8119973745672,75.310744023731,
75.8094906728948,76.3082373220586,76.7077868271323),.UNSPECIFIED.);
#2986=B_SPLINE_CURVE_WITH_KNOTS('',3,(#44783,#44784,#44785,#44786,#44787,
#44788,#44789,#44790,#44791,#44792,#44793,#44794,#44795,#44796,#44797,#44798,
#44799,#44800,#44801,#44802,#44803,#44804,#44805,#44806,#44807,#44808,#44809,
#44810,#44811,#44812,#44813,#44814,#44815,#44816,#44817,#44818,#44819,#44820,
#44821,#44822,#44823,#44824,#44825),.UNSPECIFIED.,.F.,.F.,(4,3,3,3,3,3,
3,3,3,3,3,3,3,3,4),(-72.9712679820736,-72.8170107779121,-72.3182641287483,
-71.8195174795845,-71.3207708304207,-70.8220241812569,-70.3232775320932,
-69.8245308829294,-69.3257842337656,-68.8270375846018,-68.328290935438,
-67.8295442862743,-67.3307976371105,-66.8320509879467,-66.688082674894),
 .UNSPECIFIED.);
#2987=B_SPLINE_CURVE_WITH_KNOTS('',3,(#44830,#44831,#44832,#44833,#44834,
#44835,#44836,#44837,#44838,#44839,#44840,#44841,#44842,#44843,#44844,#44845,
#44846,#44847,#44848,#44849,#44850,#44851,#44852,#44853,#44854,#44855,#44856,
#44857,#44858,#44859,#44860,#44861,#44862,#44863,#44864,#44865,#44866,#44867,
#44868,#44869,#44870,#44871,#44872),.UNSPECIFIED.,.F.,.F.,(4,3,3,3,3,3,
3,3,3,3,3,3,3,3,4),(64.1414162127731,64.3383177421278,64.8370643912916,
65.3358110404554,65.8345576896191,66.3333043387829,66.8320509879467,67.3307976371105,
67.8295442862743,68.328290935438,68.8270375846018,69.3257842337656,69.8245308829294,
70.3232775320932,70.4246015199527),.UNSPECIFIED.);
#2988=B_SPLINE_CURVE_WITH_KNOTS('',3,(#44873,#44874,#44875,#44876,#44877,
#44878,#44879,#44880,#44881,#44882,#44883,#44884,#44885,#44886,#44887,#44888,
#44889,#44890,#44891,#44892,#44893,#44894,#44895,#44896,#44897,#44898,#44899,
#44900,#44901,#44902,#44903,#44904,#44905,#44906,#44907,#44908,#44909,#44910,
#44911,#44912),.UNSPECIFIED.,.F.,.F.,(4,3,3,3,3,3,3,3,3,3,3,3,3,4),(-66.688082674894,
-66.3333043387829,-65.8345576896191,-65.3358110404554,-64.8370643912916,
-64.3383177421278,-63.839571092964,-63.3408244438002,-62.8420777946365,
-62.3433311454727,-61.8445844963089,-61.3458378471451,-60.8470911979813,
-60.4048973677144),.UNSPECIFIED.);
#2989=B_SPLINE_CURVE_WITH_KNOTS('',3,(#44917,#44918,#44919,#44920,#44921,
#44922,#44923,#44924,#44925,#44926,#44927,#44928,#44929,#44930,#44931,#44932,
#44933,#44934,#44935,#44936,#44937,#44938,#44939,#44940,#44941,#44942,#44943,
#44944,#44945,#44946,#44947,#44948,#44949,#44950,#44951,#44952,#44953,#44954,
#44955,#44956),.UNSPECIFIED.,.F.,.F.,(4,3,3,3,3,3,3,3,3,3,3,3,3,4),(57.8582309055935,
58.3533579521624,58.8521046013262,59.35085125049,59.8495978996538,60.3483445488176,
60.8470911979813,61.3458378471451,61.8445844963089,62.3433311454727,62.8420777946365,
63.3408244438002,63.839571092964,64.1414162127731),.UNSPECIFIED.);
#2990=B_SPLINE_CURVE_WITH_KNOTS('',3,(#44957,#44958,#44959,#44960,#44961,
#44962,#44963,#44964,#44965,#44966,#44967,#44968,#44969,#44970,#44971,#44972,
#44973,#44974,#44975,#44976,#44977,#44978,#44979,#44980,#44981,#44982,#44983,
#44984,#44985,#44986,#44987,#44988,#44989,#44990,#44991,#44992,#44993,#44994,
#44995,#44996,#44997,#44998,#44999),.UNSPECIFIED.,.F.,.F.,(4,3,3,3,3,3,
3,3,3,3,3,3,3,3,4),(-60.4048973677144,-60.3483445488176,-59.8495978996538,
-59.35085125049,-58.8521046013262,-58.3533579521624,-57.8546113029987,-57.3558646538349,
-56.8571180046711,-56.3583713555073,-55.8596247063435,-55.3608780571797,
-54.862131408016,-54.3633847588522,-54.1217120605348),.UNSPECIFIED.);
#2991=B_SPLINE_CURVE_WITH_KNOTS('',3,(#45004,#45005,#45006,#45007,#45008,
#45009,#45010,#45011,#45012,#45013,#45014,#45015,#45016,#45017,#45018,#45019,
#45020,#45021,#45022,#45023,#45024,#45025,#45026,#45027,#45028,#45029,#45030,
#45031,#45032,#45033,#45034,#45035,#45036,#45037,#45038,#45039,#45040,#45041,
#45042,#45043,#45044,#45045,#45046),.UNSPECIFIED.,.F.,.F.,(4,3,3,3,3,3,
3,3,3,3,3,3,3,3,4),(51.5750455984139,51.8696515130333,52.3683981621971,
52.8671448113608,53.3658914605246,53.8646381096884,54.3633847588522,54.862131408016,
55.3608780571797,55.8596247063435,56.3583713555073,56.8571180046711,57.3558646538349,
57.8546113029986,57.8582309055935),.UNSPECIFIED.);
#2992=B_SPLINE_CURVE_WITH_KNOTS('',3,(#45047,#45048,#45049,#45050,#45051,
#45052,#45053,#45054,#45055,#45056,#45057,#45058,#45059,#45060,#45061,#45062,
#45063,#45064,#45065,#45066,#45067,#45068,#45069,#45070,#45071,#45072,#45073,
#45074,#45075,#45076,#45077,#45078,#45079,#45080,#45081,#45082,#45083,#45084,
#45085,#45086,#45087,#45088,#45089),.UNSPECIFIED.,.F.,.F.,(4,3,3,3,3,3,
3,3,3,3,3,3,3,3,4),(-54.1217120605348,-53.8646381096884,-53.3658914605246,
-52.8671448113608,-52.3683981621971,-51.8696515130333,-51.3709048638695,
-50.8721582147057,-50.3734115655419,-49.8746649163781,-49.3759182672144,
-48.8771716180506,-48.3784249688868,-47.879678319723,-47.8385267533553),
 .UNSPECIFIED.);
#2993=B_SPLINE_CURVE_WITH_KNOTS('',3,(#45094,#45095,#45096,#45097,#45098,
#45099,#45100,#45101,#45102,#45103,#45104,#45105,#45106,#45107,#45108,#45109,
#45110,#45111,#45112,#45113,#45114,#45115,#45116,#45117,#45118,#45119,#45120,
#45121,#45122,#45123,#45124,#45125,#45126,#45127,#45128,#45129,#45130,#45131,
#45132,#45133,#45134,#45135,#45136),.UNSPECIFIED.,.F.,.F.,(4,3,3,3,3,3,
3,3,3,3,3,3,3,3,4),(45.2918602912343,45.3859450739041,45.8846917230679,
46.3834383722317,46.8821850213954,47.3809316705592,47.879678319723,48.3784249688868,
48.8771716180506,49.3759182672144,49.8746649163781,50.3734115655419,50.8721582147057,
51.3709048638695,51.5750455984139),.UNSPECIFIED.);
#2994=B_SPLINE_CURVE_WITH_KNOTS('',3,(#45137,#45138,#45139,#45140,#45141,
#45142,#45143,#45144,#45145,#45146,#45147,#45148,#45149,#45150,#45151,#45152,
#45153,#45154,#45155,#45156,#45157,#45158,#45159,#45160,#45161,#45162,#45163,
#45164,#45165,#45166,#45167,#45168,#45169,#45170,#45171,#45172,#45173,#45174,
#45175,#45176),.UNSPECIFIED.,.F.,.F.,(4,3,3,3,3,3,3,3,3,3,3,3,3,4),(-47.8385267533553,
-47.3809316705592,-46.8821850213955,-46.3834383722317,-45.8846917230679,
-45.3859450739041,-44.8871984247403,-44.3884517755765,-43.8897051264128,
-43.390958477249,-42.8922118280852,-42.3934651789214,-41.8947185297576,
-41.5553414461757),.UNSPECIFIED.);
#2995=B_SPLINE_CURVE_WITH_KNOTS('',3,(#45181,#45182,#45183,#45184,#45185,
#45186,#45187,#45188,#45189,#45190,#45191,#45192,#45193,#45194,#45195,#45196,
#45197,#45198,#45199,#45200,#45201,#45202,#45203,#45204,#45205,#45206,#45207,
#45208,#45209,#45210,#45211,#45212,#45213,#45214,#45215,#45216,#45217,#45218,
#45219,#45220),.UNSPECIFIED.,.F.,.F.,(4,3,3,3,3,3,3,3,3,3,3,3,3,4),(39.0086749840547,
39.4009852839387,39.8997319331025,40.3984785822663,40.8972252314301,41.3959718805938,
41.8947185297576,42.3934651789214,42.8922118280852,43.390958477249,43.8897051264128,
44.3884517755765,44.8871984247403,45.2918602912343),.UNSPECIFIED.);
#2996=B_SPLINE_CURVE_WITH_KNOTS('',3,(#45221,#45222,#45223,#45224,#45225,
#45226,#45227,#45228,#45229,#45230,#45231,#45232,#45233,#45234,#45235,#45236,
#45237,#45238,#45239,#45240,#45241,#45242,#45243,#45244,#45245,#45246,#45247,
#45248,#45249,#45250,#45251,#45252,#45253,#45254,#45255,#45256,#45257,#45258,
#45259,#45260,#45261,#45262,#45263),.UNSPECIFIED.,.F.,.F.,(4,3,3,3,3,3,
3,3,3,3,3,3,3,3,4),(-41.5553414461757,-41.3959718805939,-40.8972252314301,
-40.3984785822663,-39.8997319331025,-39.4009852839387,-38.902238634775,
-38.4034919856112,-37.9047453364474,-37.4059986872836,-36.9072520381198,
-36.4085053889561,-35.9097587397923,-35.4110120906285,-35.2721561389961),
 .UNSPECIFIED.);
#2997=B_SPLINE_CURVE_WITH_KNOTS('',3,(#45268,#45269,#45270,#45271,#45272,
#45273,#45274,#45275,#45276,#45277,#45278,#45279,#45280,#45281,#45282,#45283,
#45284,#45285,#45286,#45287,#45288,#45289,#45290,#45291,#45292,#45293,#45294,
#45295,#45296,#45297,#45298,#45299,#45300,#45301,#45302,#45303,#45304,#45305,
#45306,#45307,#45308,#45309,#45310),.UNSPECIFIED.,.F.,.F.,(4,3,3,3,3,3,
3,3,3,3,3,3,3,3,4),(32.7254896768751,32.9172788448096,33.4160254939734,
33.9147721431371,34.4135187923009,34.9122654414647,35.4110120906285,35.9097587397923,
36.408505388956,36.9072520381198,37.4059986872836,37.9047453364474,38.4034919856112,
38.9022386347749,39.0086749840547),.UNSPECIFIED.);
#2998=B_SPLINE_CURVE_WITH_KNOTS('',3,(#45311,#45312,#45313,#45314,#45315,
#45316,#45317,#45318,#45319,#45320,#45321,#45322,#45323,#45324,#45325,#45326,
#45327,#45328,#45329,#45330,#45331,#45332,#45333,#45334,#45335,#45336,#45337,
#45338,#45339,#45340,#45341,#45342,#45343,#45344,#45345,#45346,#45347,#45348,
#45349,#45350),.UNSPECIFIED.,.F.,.F.,(4,3,3,3,3,3,3,3,3,3,3,3,3,4),(-35.2721561389961,
-34.9122654414647,-34.4135187923009,-33.9147721431371,-33.4160254939734,
-32.9172788448096,-32.4185321956458,-31.919785546482,-31.4210388973182,
-30.9222922481544,-30.4235455989907,-29.9247989498269,-29.4260523006631,
-28.9889708318165),.UNSPECIFIED.);
#2999=B_SPLINE_CURVE_WITH_KNOTS('',3,(#45355,#45356,#45357,#45358,#45359,
#45360,#45361,#45362,#45363,#45364,#45365,#45366,#45367,#45368,#45369,#45370,
#45371,#45372,#45373,#45374,#45375,#45376,#45377,#45378,#45379,#45380,#45381,
#45382,#45383,#45384,#45385,#45386,#45387,#45388,#45389,#45390,#45391,#45392,
#45393,#45394),.UNSPECIFIED.,.F.,.F.,(4,3,3,3,3,3,3,3,3,3,3,3,3,4),(26.4423043696955,
26.9323190548442,27.431065704008,27.9298123531718,28.4285590023355,28.9273056514993,
29.4260523006631,29.9247989498269,30.4235455989907,30.9222922481544,31.4210388973182,
31.919785546482,32.4185321956458,32.7254896768751),.UNSPECIFIED.);
#3000=B_SPLINE_CURVE_WITH_KNOTS('',3,(#45395,#45396,#45397,#45398,#45399,
#45400,#45401,#45402,#45403,#45404,#45405,#45406,#45407,#45408,#45409,#45410,
#45411,#45412,#45413,#45414,#45415,#45416,#45417,#45418,#45419,#45420,#45421,
#45422,#45423,#45424,#45425,#45426,#45427,#45428,#45429,#45430,#45431,#45432,
#45433,#45434,#45435,#45436,#45437),.UNSPECIFIED.,.F.,.F.,(4,3,3,3,3,3,
3,3,3,3,3,3,3,3,4),(-28.9889708318165,-28.9273056514993,-28.4285590023355,
-27.9298123531718,-27.431065704008,-26.9323190548442,-26.4335724056804,
-25.9348257565166,-25.4360791073528,-24.9373324581891,-24.4385858090253,
-23.9398391598615,-23.4410925106977,-22.9423458615339,-22.7057855246369),
 .UNSPECIFIED.);
#3001=B_SPLINE_CURVE_WITH_KNOTS('',3,(#45442,#45443,#45444,#45445,#45446,
#45447,#45448,#45449,#45450,#45451,#45452,#45453,#45454,#45455,#45456,#45457,
#45458,#45459,#45460,#45461,#45462,#45463,#45464,#45465,#45466,#45467,#45468,
#45469,#45470,#45471,#45472,#45473,#45474,#45475,#45476,#45477,#45478,#45479,
#45480,#45481,#45482,#45483,#45484),.UNSPECIFIED.,.F.,.F.,(4,3,3,3,3,3,
3,3,3,3,3,3,3,3,4),(20.1591190625159,20.448612615715,20.9473592648788,21.4461059140426,
21.9448525632064,22.4435992123702,22.9423458615339,23.4410925106977,23.9398391598615,
24.4385858090253,24.9373324581891,25.4360791073529,25.9348257565166,26.4335724056804,
26.4423043696955),.UNSPECIFIED.);
#3002=B_SPLINE_CURVE_WITH_KNOTS('',3,(#45485,#45486,#45487,#45488,#45489,
#45490,#45491,#45492,#45493,#45494,#45495,#45496,#45497,#45498,#45499,#45500,
#45501,#45502,#45503,#45504,#45505,#45506,#45507,#45508,#45509,#45510,#45511,
#45512,#45513,#45514,#45515,#45516,#45517,#45518,#45519,#45520,#45521,#45522,
#45523,#45524,#45525,#45526,#45527),.UNSPECIFIED.,.F.,.F.,(4,3,3,3,3,3,
3,3,3,3,3,3,3,3,4),(-22.7057855246369,-22.4435992123702,-21.9448525632064,
-21.4461059140426,-20.9473592648788,-20.448612615715,-19.9498659665513,
-19.4511193173875,-18.9523726682237,-18.4536260190599,-17.9548793698961,
-17.4561327207323,-16.9573860715686,-16.4586394224048,-16.4226002174573),
 .UNSPECIFIED.);
#3003=B_SPLINE_CURVE_WITH_KNOTS('',3,(#45532,#45533,#45534,#45535,#45536,
#45537,#45538,#45539,#45540,#45541,#45542,#45543,#45544,#45545,#45546,#45547,
#45548,#45549,#45550,#45551,#45552,#45553,#45554,#45555,#45556,#45557,#45558,
#45559,#45560,#45561,#45562,#45563,#45564,#45565,#45566,#45567,#45568,#45569,
#45570,#45571,#45572,#45573,#45574),.UNSPECIFIED.,.F.,.F.,(4,3,3,3,3,3,
3,3,3,3,3,3,3,3,4),(13.8759337553364,13.9649061765859,14.4636528257497,
14.9623994749134,15.4611461240772,15.959892773241,16.4586394224048,16.9573860715686,
17.4561327207323,17.9548793698961,18.4536260190599,18.9523726682237,19.4511193173875,
19.9498659665513,20.1591190625159),.UNSPECIFIED.);
#3004=B_SPLINE_CURVE_WITH_KNOTS('',3,(#45575,#45576,#45577,#45578,#45579,
#45580,#45581,#45582,#45583,#45584,#45585,#45586,#45587,#45588,#45589,#45590,
#45591,#45592,#45593,#45594,#45595,#45596,#45597,#45598,#45599,#45600,#45601,
#45602,#45603,#45604,#45605,#45606,#45607,#45608,#45609,#45610,#45611,#45612,
#45613,#45614),.UNSPECIFIED.,.F.,.F.,(4,3,3,3,3,3,3,3,3,3,3,3,3,4),(-16.4226002174573,
-15.959892773241,-15.4611461240772,-14.9623994749134,-14.4636528257497,
-13.9649061765859,-13.4661595274221,-12.9674128782583,-12.4686662290945,
-11.9699195799308,-11.471172930767,-10.9724262816032,-10.4736796324394,
-10.1394149102777),.UNSPECIFIED.);
#3005=B_SPLINE_CURVE_WITH_KNOTS('',3,(#45620,#45621,#45622,#45623,#45624,
#45625,#45626,#45627,#45628,#45629,#45630,#45631,#45632,#45633,#45634,#45635,
#45636,#45637,#45638,#45639,#45640,#45641,#45642,#45643,#45644),
 .UNSPECIFIED.,.F.,.F.,(4,3,3,3,3,3,3,3,4),(-3.85622960309811,-3.49122654414647,
-2.99247989498269,-2.49373324581891,-1.99498659665513,-1.49623994749134,
-0.997493298327563,-0.498746649163781,0.),.UNSPECIFIED.);
#3006=B_SPLINE_CURVE_WITH_KNOTS('',3,(#45647,#45648,#45649,#45650,#45651,
#45652,#45653,#45654,#45655,#45656,#45657,#45658,#45659,#45660,#45661,#45662,
#45663,#45664,#45665,#45666,#45667,#45668,#45669,#45670,#45671,#45672,#45673,
#45674,#45675,#45676,#45677,#45678,#45679,#45680,#45681,#45682,#45683),
 .UNSPECIFIED.,.F.,.F.,(4,3,3,3,3,3,3,3,3,3,3,3,4),(2.02420009048538,2.49373324581891,
2.99247989498269,3.49122654414647,3.98997319331025,4.48871984247403,4.98746649163781,
5.4862131408016,5.98495978996538,6.48370643912916,6.98245308829294,7.48119973745672,
7.59274844815678),.UNSPECIFIED.);
#3007=B_SPLINE_CURVE_WITH_KNOTS('',3,(#45689,#45690,#45691,#45692,#45693,
#45694,#45695),.UNSPECIFIED.,.F.,.F.,(4,1,1,1,4),(191.637151868977,191.899274012976,
192.39802066214,192.896767311304,193.395513960467),.UNSPECIFIED.);
#3008=B_SPLINE_CURVE_WITH_KNOTS('',3,(#45698,#45699,#45700,#45701,#45702,
#45703,#45704,#45705),.UNSPECIFIED.,.F.,.F.,(4,1,1,1,1,4),(191.637151868977,
191.952207229278,192.450953878442,192.949700527606,193.448447176769,193.917980332103),
 .UNSPECIFIED.);
#3009=B_SPLINE_CURVE_WITH_KNOTS('',3,(#45710,#45711,#45712,#45713,#45714,
#45715,#45716,#45717,#45718,#45719,#45720,#45721,#45722,#45723,#45724,#45725,
#45726),.UNSPECIFIED.,.F.,.F.,(4,1,1,1,1,1,1,1,1,1,1,1,1,1,4),(185.353966561798,
185.415567573847,185.914314223011,186.413060872174,186.911807521338,187.410554170502,
187.909300819666,188.40804746883,188.906794117993,189.405540767157,189.904287416321,
190.403034065485,190.901780714648,191.400527363812,191.637151868977),
 .UNSPECIFIED.);
#3010=B_SPLINE_CURVE_WITH_KNOTS('',3,(#45727,#45728,#45729,#45730,#45731,
#45732,#45733,#45734,#45735,#45736,#45737,#45738,#45739,#45740,#45741,#45742,
#45743),.UNSPECIFIED.,.F.,.F.,(4,1,1,1,1,1,1,1,1,1,1,1,1,1,4),(185.353966561798,
185.468500790149,185.967247439313,186.465994088476,186.96474073764,187.463487386804,
187.962234035968,188.460980685132,188.959727334295,189.458473983459,189.957220632623,
190.455967281787,190.954713930951,191.453460580114,191.637151868977),
 .UNSPECIFIED.);
#3011=B_SPLINE_CURVE_WITH_KNOTS('',3,(#45748,#45749,#45750,#45751,#45752,
#45753,#45754,#45755,#45756,#45757,#45758,#45759,#45760,#45761,#45762,#45763),
 .UNSPECIFIED.,.F.,.F.,(4,1,1,1,1,1,1,1,1,1,1,1,1,4),(179.070781254618,
179.430607783881,179.929354433045,180.428101082209,180.926847731373,181.425594380537,
181.9243410297,182.423087678864,182.921834328028,183.420580977192,183.919327626356,
184.418074275519,184.916820924683,185.353966561798),.UNSPECIFIED.);
#3012=B_SPLINE_CURVE_WITH_KNOTS('',3,(#45764,#45765,#45766,#45767,#45768,
#45769,#45770,#45771,#45772,#45773,#45774,#45775,#45776,#45777,#45778,#45779),
 .UNSPECIFIED.,.F.,.F.,(4,1,1,1,1,1,1,1,1,1,1,1,1,4),(179.070781254618,
179.483541000184,179.982287649347,180.481034298511,180.979780947675,181.478527596839,
181.977274246002,182.476020895166,182.97476754433,183.473514193494,183.972260842658,
184.471007491821,184.969754140985,185.353966561798),.UNSPECIFIED.);
#3013=B_SPLINE_CURVE_WITH_KNOTS('',3,(#45784,#45785,#45786,#45787,#45788,
#45789,#45790,#45791,#45792,#45793,#45794,#45795,#45796,#45797,#45798,#45799,
#45800),.UNSPECIFIED.,.F.,.F.,(4,1,1,1,1,1,1,1,1,1,1,1,1,1,4),(172.787595947439,
172.946901344752,173.445647993916,173.94439464308,174.443141292244,174.941887941407,
175.440634590571,175.939381239735,176.438127888899,176.936874538063,177.435621187226,
177.93436783639,178.433114485554,178.931861134718,179.070781254618),
 .UNSPECIFIED.);
#3014=B_SPLINE_CURVE_WITH_KNOTS('',3,(#45801,#45802,#45803,#45804,#45805,
#45806,#45807,#45808,#45809,#45810,#45811,#45812,#45813,#45814,#45815,#45816,
#45817),.UNSPECIFIED.,.F.,.F.,(4,1,1,1,1,1,1,1,1,1,1,1,1,1,4),(172.787595947439,
172.999834561054,173.498581210218,173.997327859382,174.496074508546,174.99482115771,
175.493567806873,175.992314456037,176.491061105201,176.989807754365,177.488554403528,
177.987301052692,178.486047701856,178.98479435102,179.070781254618),
 .UNSPECIFIED.);
#3015=B_SPLINE_CURVE_WITH_KNOTS('',3,(#45822,#45823,#45824,#45825,#45826,
#45827,#45828,#45829,#45830,#45831,#45832,#45833,#45834,#45835,#45836,#45837),
 .UNSPECIFIED.,.F.,.F.,(4,1,1,1,1,1,1,1,1,1,1,1,1,4),(166.504410640259,
166.961941554787,167.460688203951,167.959434853114,168.458181502278,168.956928151442,
169.455674800606,169.95442144977,170.453168098933,170.951914748097,171.450661397261,
171.949408046425,172.448154695589,172.787595947439),.UNSPECIFIED.);
#3016=B_SPLINE_CURVE_WITH_KNOTS('',3,(#45838,#45839,#45840,#45841,#45842,
#45843,#45844,#45845,#45846,#45847,#45848,#45849,#45850,#45851,#45852,#45853,
#45854),.UNSPECIFIED.,.F.,.F.,(4,1,1,1,1,1,1,1,1,1,1,1,1,1,4),(166.504410640259,
166.516128121925,167.014874771089,167.513621420253,168.012368069417,168.51111471858,
169.009861367744,169.508608016908,170.007354666072,170.506101315235,171.004847964399,
171.503594613563,172.002341262727,172.501087911891,172.787595947439),
 .UNSPECIFIED.);
#3017=B_SPLINE_CURVE_WITH_KNOTS('',3,(#45859,#45860,#45861,#45862,#45863,
#45864,#45865,#45866,#45867,#45868,#45869,#45870,#45871,#45872,#45873,#45874,
#45875),.UNSPECIFIED.,.F.,.F.,(4,1,1,1,1,1,1,1,1,1,1,1,1,1,4),(160.22122533308,
160.478235115658,160.976981764822,161.475728413985,161.974475063149,162.473221712313,
162.971968361477,163.47071501064,163.969461659804,164.468208308968,164.966954958132,
165.465701607296,165.964448256459,166.463194905623,166.504410640259),
 .UNSPECIFIED.);
#3018=B_SPLINE_CURVE_WITH_KNOTS('',3,(#45876,#45877,#45878,#45879,#45880,
#45881,#45882,#45883,#45884,#45885,#45886,#45887,#45888,#45889,#45890,#45891),
 .UNSPECIFIED.,.F.,.F.,(4,1,1,1,1,1,1,1,1,1,1,1,1,4),(160.22122533308,160.53116833196,
161.029914981124,161.528661630287,162.027408279451,162.526154928615,163.024901577779,
163.523648226943,164.022394876106,164.52114152527,165.019888174434,165.518634823598,
166.017381472761,166.504410640259),.UNSPECIFIED.);
#3019=B_SPLINE_CURVE_WITH_KNOTS('',3,(#45896,#45897,#45898,#45899,#45900,
#45901,#45902,#45903,#45904,#45905,#45906,#45907,#45908,#45909,#45910,#45911,
#45912),.UNSPECIFIED.,.F.,.F.,(4,1,1,1,1,1,1,1,1,1,1,1,1,1,4),(153.9380400259,
153.994528676529,154.493275325692,154.992021974856,155.49076862402,155.989515273184,
156.488261922348,156.987008571511,157.485755220675,157.984501869839,158.483248519003,
158.981995168166,159.48074181733,159.979488466494,160.22122533308),
 .UNSPECIFIED.);
#3020=B_SPLINE_CURVE_WITH_KNOTS('',3,(#45913,#45914,#45915,#45916,#45917,
#45918,#45919,#45920,#45921,#45922,#45923,#45924,#45925,#45926,#45927,#45928,
#45929),.UNSPECIFIED.,.F.,.F.,(4,1,1,1,1,1,1,1,1,1,1,1,1,1,4),(153.9380400259,
154.047461892831,154.546208541994,155.044955191158,155.543701840322,156.042448489486,
156.54119513865,157.039941787813,157.538688436977,158.037435086141,158.536181735305,
159.034928384469,159.533675033632,160.032421682796,160.22122533308),
 .UNSPECIFIED.);
#3021=B_SPLINE_CURVE_WITH_KNOTS('',3,(#45934,#45935,#45936,#45937,#45938,
#45939,#45940,#45941,#45942,#45943,#45944,#45945,#45946,#45947,#45948,#45949),
 .UNSPECIFIED.,.F.,.F.,(4,1,1,1,1,1,1,1,1,1,1,1,1,4),(147.65485471872,148.009568886563,
148.508315535727,149.007062184891,149.505808834055,150.004555483218,150.503302132382,
151.002048781546,151.50079543071,151.999542079873,152.498288729037,152.997035378201,
153.495782027365,153.9380400259),.UNSPECIFIED.);
#3022=B_SPLINE_CURVE_WITH_KNOTS('',3,(#45950,#45951,#45952,#45953,#45954,
#45955,#45956,#45957,#45958,#45959,#45960,#45961,#45962,#45963,#45964,#45965),
 .UNSPECIFIED.,.F.,.F.,(4,1,1,1,1,1,1,1,1,1,1,1,1,4),(147.65485471872,148.062502102865,
148.561248752029,149.059995401193,149.558742050357,150.05748869952,150.556235348684,
151.054981997848,151.553728647012,152.052475296176,152.551221945339,153.049968594503,
153.548715243667,153.9380400259),.UNSPECIFIED.);
#3023=B_SPLINE_CURVE_WITH_KNOTS('',3,(#45970,#45971,#45972,#45973,#45974,
#45975,#45976,#45977,#45978,#45979,#45980,#45981,#45982,#45983,#45984,#45985,
#45986),.UNSPECIFIED.,.F.,.F.,(4,1,1,1,1,1,1,1,1,1,1,1,1,1,4),(141.371669411541,
141.525862447434,142.024609096598,142.523355745762,143.022102394925,143.520849044089,
144.019595693253,144.518342342417,145.017088991581,145.515835640744,146.014582289908,
146.513328939072,147.012075588236,147.510822237399,147.65485471872),
 .UNSPECIFIED.);
#3024=B_SPLINE_CURVE_WITH_KNOTS('',3,(#45987,#45988,#45989,#45990,#45991,
#45992,#45993,#45994,#45995,#45996,#45997,#45998,#45999,#46000,#46001,#46002,
#46003),.UNSPECIFIED.,.F.,.F.,(4,1,1,1,1,1,1,1,1,1,1,1,1,1,4),(141.371669411541,
141.578795663736,142.0775423129,142.576288962064,143.075035611227,143.573782260391,
144.072528909555,144.571275558719,145.070022207883,145.568768857046,146.06751550621,
146.566262155374,147.065008804538,147.563755453702,147.65485471872),
 .UNSPECIFIED.);
#3025=B_SPLINE_CURVE_WITH_KNOTS('',3,(#46008,#46009,#46010,#46011,#46012,
#46013,#46014,#46015,#46016,#46017,#46018,#46019,#46020,#46021,#46022,#46023),
 .UNSPECIFIED.,.F.,.F.,(4,1,1,1,1,1,1,1,1,1,1,1,1,4),(135.088484104361,
135.540902657469,136.039649306632,136.538395955796,137.03714260496,137.535889254124,
138.034635903288,138.533382552451,139.032129201615,139.530875850779,140.029622499943,
140.528369149107,141.02711579827,141.371669411541),.UNSPECIFIED.);
#3026=B_SPLINE_CURVE_WITH_KNOTS('',3,(#46024,#46025,#46026,#46027,#46028,
#46029,#46030,#46031,#46032,#46033,#46034,#46035,#46036,#46037,#46038,#46039,
#46040),.UNSPECIFIED.,.F.,.F.,(4,1,1,1,1,1,1,1,1,1,1,1,1,1,4),(135.088484104361,
135.095089224607,135.593835873771,136.092582522935,136.591329172098,137.090075821262,
137.588822470426,138.08756911959,138.586315768753,139.085062417917,139.583809067081,
140.082555716245,140.581302365409,141.080049014572,141.371669411541),
 .UNSPECIFIED.);
#3027=B_SPLINE_CURVE_WITH_KNOTS('',3,(#46045,#46046,#46047,#46048,#46049,
#46050,#46051,#46052,#46053,#46054,#46055,#46056,#46057,#46058,#46059,#46060,
#46061),.UNSPECIFIED.,.F.,.F.,(4,1,1,1,1,1,1,1,1,1,1,1,1,1,4),(128.805298797182,
129.05719621834,129.555942867503,130.054689516667,130.553436165831,131.052182814995,
131.550929464158,132.049676113322,132.548422762486,133.04716941165,133.545916060814,
134.044662709977,134.543409359141,135.042156008305,135.088484104361),
 .UNSPECIFIED.);
#3028=B_SPLINE_CURVE_WITH_KNOTS('',3,(#46062,#46063,#46064,#46065,#46066,
#46067,#46068,#46069,#46070,#46071,#46072,#46073,#46074,#46075,#46076,#46077),
 .UNSPECIFIED.,.F.,.F.,(4,1,1,1,1,1,1,1,1,1,1,1,1,4),(128.805298797182,
129.110129434642,129.608876083805,130.107622732969,130.606369382133,131.105116031297,
131.603862680461,132.102609329624,132.601355978788,133.100102627952,133.598849277116,
134.097595926279,134.596342575443,135.088484104361),.UNSPECIFIED.);
#3029=B_SPLINE_CURVE_WITH_KNOTS('',3,(#46082,#46083,#46084,#46085,#46086,
#46087,#46088,#46089,#46090,#46091,#46092,#46093,#46094,#46095,#46096,#46097,
#46098),.UNSPECIFIED.,.F.,.F.,(4,1,1,1,1,1,1,1,1,1,1,1,1,1,4),(122.522113490002,
122.57348977921,123.072236428374,123.570983077538,124.069729726702,124.568476375866,
125.067223025029,125.565969674193,126.064716323357,126.563462972521,127.062209621684,
127.560956270848,128.059702920012,128.558449569176,128.805298797182),
 .UNSPECIFIED.);
#3030=B_SPLINE_CURVE_WITH_KNOTS('',3,(#46099,#46100,#46101,#46102,#46103,
#46104,#46105,#46106,#46107,#46108,#46109,#46110,#46111,#46112,#46113,#46114,
#46115),.UNSPECIFIED.,.F.,.F.,(4,1,1,1,1,1,1,1,1,1,1,1,1,1,4),(122.522113490002,
122.626422995512,123.125169644676,123.62391629384,124.122662943004,124.621409592168,
125.120156241331,125.618902890495,126.117649539659,126.616396188823,127.115142837986,
127.61388948715,128.112636136314,128.611382785478,128.805298797182),
 .UNSPECIFIED.);
#3031=B_SPLINE_CURVE_WITH_KNOTS('',3,(#46120,#46121,#46122,#46123,#46124,
#46125,#46126,#46127,#46128,#46129,#46130,#46131,#46132,#46133,#46134,#46135),
 .UNSPECIFIED.,.F.,.F.,(4,1,1,1,1,1,1,1,1,1,1,1,1,4),(116.238928182823,
116.588529989245,117.087276638409,117.586023287573,118.084769936736,118.5835165859,
119.082263235064,119.581009884228,120.079756533392,120.578503182555,121.077249831719,
121.575996480883,122.074743130047,122.522113490002),.UNSPECIFIED.);
#3032=B_SPLINE_CURVE_WITH_KNOTS('',3,(#46136,#46137,#46138,#46139,#46140,
#46141,#46142,#46143,#46144,#46145,#46146,#46147,#46148,#46149,#46150,#46151),
 .UNSPECIFIED.,.F.,.F.,(4,1,1,1,1,1,1,1,1,1,1,1,1,4),(116.238928182823,
116.641463205547,117.140209854711,117.638956503875,118.137703153038,118.636449802202,
119.135196451366,119.63394310053,120.132689749694,120.631436398857,121.130183048021,
121.628929697185,122.127676346349,122.522113490002),.UNSPECIFIED.);
#3033=B_SPLINE_CURVE_WITH_KNOTS('',3,(#46156,#46157,#46158,#46159,#46160,
#46161,#46162,#46163,#46164,#46165,#46166,#46167,#46168,#46169,#46170,#46171,
#46172),.UNSPECIFIED.,.F.,.F.,(4,1,1,1,1,1,1,1,1,1,1,1,1,1,4),(109.955742875643,
110.104823550116,110.60357019928,111.102316848443,111.601063497607,112.099810146771,
112.598556795935,113.097303445099,113.596050094262,114.094796743426,114.59354339259,
115.092290041754,115.591036690917,116.089783340081,116.238928182823),
 .UNSPECIFIED.);
#3034=B_SPLINE_CURVE_WITH_KNOTS('',3,(#46173,#46174,#46175,#46176,#46177,
#46178,#46179,#46180,#46181,#46182,#46183,#46184,#46185,#46186,#46187,#46188,
#46189),.UNSPECIFIED.,.F.,.F.,(4,1,1,1,1,1,1,1,1,1,1,1,1,1,4),(109.955742875643,
110.157756766418,110.656503415582,111.155250064746,111.653996713909,112.152743363073,
112.651490012237,113.150236661401,113.648983310564,114.147729959728,114.646476608892,
115.145223258056,115.64396990722,116.142716556383,116.238928182823),
 .UNSPECIFIED.);
#3035=B_SPLINE_CURVE_WITH_KNOTS('',3,(#46194,#46195,#46196,#46197,#46198,
#46199,#46200,#46201,#46202,#46203,#46204,#46205,#46206,#46207,#46208,#46209),
 .UNSPECIFIED.,.F.,.F.,(4,1,1,1,1,1,1,1,1,1,1,1,1,4),(103.672557568463,
104.11986376015,104.618610409314,105.117357058478,105.616103707642,106.114850356806,
106.613597005969,107.112343655133,107.611090304297,108.109836953461,108.608583602625,
109.107330251788,109.606076900952,109.955742875643),.UNSPECIFIED.);
#3036=B_SPLINE_CURVE_WITH_KNOTS('',3,(#46210,#46211,#46212,#46213,#46214,
#46215,#46216,#46217,#46218,#46219,#46220,#46221,#46222,#46223,#46224,#46225,
#46226),.UNSPECIFIED.,.F.,.F.,(4,1,1,1,1,1,1,1,1,1,1,1,1,1,4),(103.672557568463,
103.674050327289,104.172796976453,104.671543625616,105.17029027478,105.669036923944,
106.167783573108,106.666530222271,107.165276871435,107.664023520599,108.162770169763,
108.661516818927,109.16026346809,109.659010117254,109.955742875643),
 .UNSPECIFIED.);
#3037=B_SPLINE_CURVE_WITH_KNOTS('',3,(#46231,#46232,#46233,#46234,#46235,
#46236,#46237,#46238,#46239,#46240,#46241,#46242,#46243,#46244,#46245,#46246,
#46247),.UNSPECIFIED.,.F.,.F.,(4,1,1,1,1,1,1,1,1,1,1,1,1,1,4),(97.3893722612838,
97.6361573210213,98.1349039701851,98.6336506193489,99.1323972685127,99.6311439176765,
100.12989056684,100.628637216004,101.127383865168,101.626130514332,102.124877163495,
102.623623812659,103.122370461823,103.621117110987,103.672557568463),
 .UNSPECIFIED.);
#3038=B_SPLINE_CURVE_WITH_KNOTS('',3,(#46248,#46249,#46250,#46251,#46252,
#46253,#46254,#46255,#46256,#46257,#46258,#46259,#46260,#46261,#46262,#46263),
 .UNSPECIFIED.,.F.,.F.,(4,1,1,1,1,1,1,1,1,1,1,1,1,4),(97.3893722612837,
97.6890905373234,98.1878371864872,98.686583835651,99.1853304848147,99.6840771339785,
100.182823783142,100.681570432306,101.18031708147,101.679063730634,102.177810379797,
102.676557028961,103.175303678125,103.672557568463),.UNSPECIFIED.);
#3039=B_SPLINE_CURVE_WITH_KNOTS('',3,(#46268,#46269,#46270,#46271,#46272,
#46273,#46274,#46275,#46276,#46277,#46278,#46279,#46280,#46281,#46282,#46283,
#46284),.UNSPECIFIED.,.F.,.F.,(4,1,1,1,1,1,1,1,1,1,1,1,1,1,4),(91.1061869541041,
91.1524508818922,91.651197531056,92.1499441802197,92.6486908293835,93.1474374785473,
93.6461841277111,94.1449307768749,94.6436774260386,95.1424240752024,95.6411707243662,
96.13991737353,96.6386640226938,97.1374106718576,97.3893722612838),
 .UNSPECIFIED.);
#3040=B_SPLINE_CURVE_WITH_KNOTS('',3,(#46285,#46286,#46287,#46288,#46289,
#46290,#46291,#46292,#46293,#46294,#46295,#46296,#46297,#46298,#46299,#46300,
#46301),.UNSPECIFIED.,.F.,.F.,(4,1,1,1,1,1,1,1,1,1,1,1,1,1,4),(91.1061869541041,
91.2053840981942,91.704130747358,92.2028773965218,92.7016240456856,93.2003706948494,
93.6991173440131,94.1978639931769,94.6966106423407,95.1953572915045,95.6941039406683,
96.1928505898321,96.6915972389958,97.1903438881596,97.3893722612837),
 .UNSPECIFIED.);
#3041=B_SPLINE_CURVE_WITH_KNOTS('',3,(#46306,#46307,#46308,#46309,#46310,
#46311,#46312,#46313,#46314,#46315,#46316,#46317,#46318,#46319,#46320,#46321),
 .UNSPECIFIED.,.F.,.F.,(4,1,1,1,1,1,1,1,1,1,1,1,1,4),(84.8230016469246,
85.1674910919268,85.6662377410906,86.1649843902544,86.6637310394181,87.1624776885819,
87.6612243377457,88.1599709869095,88.6587176360733,89.1574642852371,89.6562109344008,
90.1549575835646,90.6537042327284,91.1061869541041),.UNSPECIFIED.);
#3042=B_SPLINE_CURVE_WITH_KNOTS('',3,(#46322,#46323,#46324,#46325,#46326,
#46327,#46328,#46329,#46330,#46331,#46332,#46333,#46334,#46335,#46336,#46337),
 .UNSPECIFIED.,.F.,.F.,(4,1,1,1,1,1,1,1,1,1,1,1,1,4),(84.8230016469245,
85.2204243082289,85.7191709573926,86.2179176065564,86.7166642557202,87.215410904884,
87.7141575540478,88.2129042032116,88.7116508523753,89.2103975015391,89.7091441507029,
90.2078907998667,90.7066374490305,91.1061869541041),.UNSPECIFIED.);
#3043=B_SPLINE_CURVE_WITH_KNOTS('',3,(#46342,#46343,#46344,#46345,#46346,
#46347,#46348,#46349,#46350,#46351,#46352,#46353,#46354,#46355,#46356,#46357,
#46358),.UNSPECIFIED.,.F.,.F.,(4,1,1,1,1,1,1,1,1,1,1,1,1,1,4),(78.539816339745,
78.6837846527976,79.1825313019614,79.6812779511252,80.180024600289,80.6787712494528,
81.1775178986165,81.6762645477803,82.1750111969441,82.6737578461079,83.1725044952717,
83.6712511444355,84.1699977935992,84.668744442763,84.8230016469246),
 .UNSPECIFIED.);
#3044=B_SPLINE_CURVE_WITH_KNOTS('',3,(#46359,#46360,#46361,#46362,#46363,
#46364,#46365,#46366,#46367,#46368,#46369,#46370,#46371,#46372,#46373,#46374,
#46375),.UNSPECIFIED.,.F.,.F.,(4,1,1,1,1,1,1,1,1,1,1,1,1,1,4),(78.539816339745,
78.7367178690997,79.2354645182635,79.7342111674273,80.2329578165911,80.7317044657548,
81.2304511149186,81.7291977640824,82.2279444132462,82.72669106241,83.2254377115737,
83.7241843607375,84.2229310099013,84.7216776590651,84.8230016469245),
 .UNSPECIFIED.);
#3045=B_SPLINE_CURVE_WITH_KNOTS('',3,(#46380,#46381,#46382,#46383,#46384,
#46385,#46386,#46387,#46388,#46389,#46390,#46391,#46392,#46393,#46394,#46395),
 .UNSPECIFIED.,.F.,.F.,(4,1,1,1,1,1,1,1,1,1,1,1,1,4),(72.2566310325654,
72.6988248628323,73.197571511996,73.6963181611598,74.1950648103236,74.6938114594874,
75.1925581086512,75.6913047578149,76.1900514069787,76.6887980561425,77.1875447053063,
77.6862913544701,78.1850380036339,78.539816339745),.UNSPECIFIED.);
#3046=B_SPLINE_CURVE_WITH_KNOTS('',3,(#46396,#46397,#46398,#46399,#46400,
#46401,#46402,#46403,#46404,#46405,#46406,#46407,#46408,#46409,#46410,#46411),
 .UNSPECIFIED.,.F.,.F.,(4,1,1,1,1,1,1,1,1,1,1,1,1,4),(72.2566310325654,
72.7517580791343,73.2505047282981,73.7492513774619,74.2479980266257,74.7467446757895,
75.2454913249532,75.744237974117,76.2429846232808,76.7417312724446,77.2404779216084,
77.7392245707722,78.2379712199359,78.539816339745),.UNSPECIFIED.);
#3047=B_SPLINE_CURVE_WITH_KNOTS('',3,(#46416,#46417,#46418,#46419,#46420,
#46421,#46422,#46423,#46424,#46425,#46426,#46427,#46428,#46429,#46430,#46431,
#46432),.UNSPECIFIED.,.F.,.F.,(4,1,1,1,1,1,1,1,1,1,1,1,1,1,4),(65.9734457253858,
66.2151184237031,66.7138650728669,67.2126117220307,67.7113583711945,68.2101050203582,
68.708851669522,69.2075983186858,69.7063449678496,70.2050916170134,70.7038382661771,
71.2025849153409,71.7013315645047,72.2000782136685,72.2566310325654),
 .UNSPECIFIED.);
#3048=B_SPLINE_CURVE_WITH_KNOTS('',3,(#46433,#46434,#46435,#46436,#46437,
#46438,#46439,#46440,#46441,#46442,#46443,#46444,#46445,#46446,#46447,#46448,
#46449),.UNSPECIFIED.,.F.,.F.,(4,1,1,1,1,1,1,1,1,1,1,1,1,1,4),(65.9734457253858,
66.2680516400052,66.766798289169,67.2655449383327,67.7642915874965,68.2630382366603,
68.7617848858241,69.2605315349879,69.7592781841516,70.2580248333154,70.7567714824792,
71.255518131643,71.7542647808068,72.2530114299706,72.2566310325654),
 .UNSPECIFIED.);
#3049=B_SPLINE_CURVE_WITH_KNOTS('',3,(#46454,#46455,#46456,#46457,#46458,
#46459,#46460,#46461,#46462,#46463,#46464,#46465,#46466,#46467,#46468,#46469,
#46470),.UNSPECIFIED.,.F.,.F.,(4,1,1,1,1,1,1,1,1,1,1,1,1,1,4),(59.6902604182062,
59.731411984574,60.2301586337377,60.7289052829015,61.2276519320653,61.7263985812291,
62.2251452303929,62.7238918795566,63.2226385287204,63.7213851778842,64.220131827048,
64.7188784762118,65.2176251253755,65.7163717745393,65.9734457253858),
 .UNSPECIFIED.);
#3050=B_SPLINE_CURVE_WITH_KNOTS('',3,(#46471,#46472,#46473,#46474,#46475,
#46476,#46477,#46478,#46479,#46480,#46481,#46482,#46483,#46484,#46485,#46486,
#46487),.UNSPECIFIED.,.F.,.F.,(4,1,1,1,1,1,1,1,1,1,1,1,1,1,4),(59.6902604182062,
59.784345200876,60.2830918500398,60.7818384992036,61.2805851483674,61.7793317975311,
62.2780784466949,62.7768250958587,63.2755717450225,63.7743183941863,64.2730650433501,
64.7718116925138,65.2705583416776,65.7693049908414,65.9734457253858),
 .UNSPECIFIED.);
#3051=B_SPLINE_CURVE_WITH_KNOTS('',3,(#46492,#46493,#46494,#46495,#46496,
#46497,#46498,#46499,#46500,#46501,#46502,#46503,#46504,#46505,#46506,#46507),
 .UNSPECIFIED.,.F.,.F.,(4,1,1,1,1,1,1,1,1,1,1,1,1,4),(53.4070751110266,
53.7464521946086,54.2451988437724,54.7439454929361,55.2426921420999,55.7414387912637,
56.2401854404275,56.7389320895913,57.237678738755,57.7364253879188,58.2351720370826,
58.7339186862464,59.2326653354102,59.6902604182062),.UNSPECIFIED.);
#3052=B_SPLINE_CURVE_WITH_KNOTS('',3,(#46508,#46509,#46510,#46511,#46512,
#46513,#46514,#46515,#46516,#46517,#46518,#46519,#46520,#46521,#46522,#46523),
 .UNSPECIFIED.,.F.,.F.,(4,1,1,1,1,1,1,1,1,1,1,1,1,4),(53.4070751110266,
53.7993854109106,54.2981320600744,54.7968787092382,55.295625358402,55.7943720075658,
56.2931186567296,56.7918653058933,57.2906119550571,57.7893586042209,58.2881052533847,
58.7868519025485,59.2855985517122,59.6902604182062),.UNSPECIFIED.);
#3053=B_SPLINE_CURVE_WITH_KNOTS('',3,(#46528,#46529,#46530,#46531,#46532,
#46533,#46534,#46535,#46536,#46537,#46538,#46539,#46540,#46541,#46542,#46543,
#46544),.UNSPECIFIED.,.F.,.F.,(4,1,1,1,1,1,1,1,1,1,1,1,1,1,4),(47.123889803847,
47.2627457554794,47.7614924046432,48.260239053807,48.7589857029708,49.2577323521345,
49.7564790012983,50.2552256504621,50.7539722996259,51.2527189487897,51.7514655979534,
52.2502122471172,52.748958896281,53.2477055454448,53.4070751110266),
 .UNSPECIFIED.);
#3054=B_SPLINE_CURVE_WITH_KNOTS('',3,(#46545,#46546,#46547,#46548,#46549,
#46550,#46551,#46552,#46553,#46554,#46555,#46556,#46557,#46558,#46559,#46560,
#46561),.UNSPECIFIED.,.F.,.F.,(4,1,1,1,1,1,1,1,1,1,1,1,1,1,4),(47.123889803847,
47.3156789717815,47.8144256209453,48.313172270109,48.8119189192728,49.3106655684366,
49.8094122176004,50.3081588667642,50.806905515928,51.3056521650917,51.8043988142555,
52.3031454634193,52.8018921125831,53.3006387617469,53.4070751110266),
 .UNSPECIFIED.);
#3055=B_SPLINE_CURVE_WITH_KNOTS('',3,(#46566,#46567,#46568,#46569,#46570,
#46571,#46572,#46573,#46574,#46575,#46576,#46577,#46578,#46579,#46580,#46581),
 .UNSPECIFIED.,.F.,.F.,(4,1,1,1,1,1,1,1,1,1,1,1,1,4),(40.8407044966674,
41.277785965514,41.7765326146778,42.2752792638416,42.7740259130054,43.2727725621692,
43.7715192113329,44.2702658604967,44.7690125096605,45.2677591588243,45.7665058079881,
46.2652524571519,46.7639991063156,47.123889803847),.UNSPECIFIED.);
#3056=B_SPLINE_CURVE_WITH_KNOTS('',3,(#46582,#46583,#46584,#46585,#46586,
#46587,#46588,#46589,#46590,#46591,#46592,#46593,#46594,#46595,#46596,#46597),
 .UNSPECIFIED.,.F.,.F.,(4,1,1,1,1,1,1,1,1,1,1,1,1,4),(40.8407044966674,
41.3307191818161,41.8294658309799,42.3282124801437,42.8269591293075,43.3257057784712,
43.824452427635,44.3231990767988,44.8219457259626,45.3206923751264,45.8194390242901,
46.3181856734539,46.8169323226177,47.123889803847),.UNSPECIFIED.);
#3057=B_SPLINE_CURVE_WITH_KNOTS('',3,(#46602,#46603,#46604,#46605,#46606,
#46607,#46608,#46609,#46610,#46611,#46612,#46613,#46614,#46615,#46616,#46617,
#46618),.UNSPECIFIED.,.F.,.F.,(4,1,1,1,1,1,1,1,1,1,1,1,1,1,4),(34.5575191894878,
34.7940795263849,35.2928261755487,35.7915728247124,36.2903194738762,36.78906612304,
37.2878127722038,37.7865594213676,38.2853060705313,38.7840527196951,39.2827993688589,
39.7815460180227,40.2802926671865,40.7790393163503,40.8407044966674),
 .UNSPECIFIED.);
#3058=B_SPLINE_CURVE_WITH_KNOTS('',3,(#46619,#46620,#46621,#46622,#46623,
#46624,#46625,#46626,#46627,#46628,#46629,#46630,#46631,#46632,#46633,#46634,
#46635),.UNSPECIFIED.,.F.,.F.,(4,1,1,1,1,1,1,1,1,1,1,1,1,1,4),(34.5575191894878,
34.847012742687,35.3457593918507,35.8445060410145,36.3432526901783,36.8419993393421,
37.3407459885059,37.8394926376697,38.3382392868334,38.8369859359972,39.335732585161,
39.8344792343248,40.3332258834886,40.8319725326523,40.8407044966674),
 .UNSPECIFIED.);
#3059=B_SPLINE_CURVE_WITH_KNOTS('',3,(#46640,#46641,#46642,#46643,#46644,
#46645,#46646,#46647,#46648,#46649,#46650,#46651,#46652,#46653,#46654,#46655,
#46656),.UNSPECIFIED.,.F.,.F.,(4,1,1,1,1,1,1,1,1,1,1,1,1,1,4),(28.2743338823083,
28.3103730872557,28.8091197364195,29.3078663855833,29.8066130347471,30.3053596839108,
30.8041063330746,31.3028529822384,31.8015996314022,32.300346280566,32.7990929297298,
33.2978395788935,33.7965862280573,34.2953328772211,34.5575191894878),
 .UNSPECIFIED.);
#3060=B_SPLINE_CURVE_WITH_KNOTS('',3,(#46657,#46658,#46659,#46660,#46661,
#46662,#46663,#46664,#46665,#46666,#46667,#46668,#46669,#46670,#46671,#46672,
#46673),.UNSPECIFIED.,.F.,.F.,(4,1,1,1,1,1,1,1,1,1,1,1,1,1,4),(28.2743338823082,
28.3633063035578,28.8620529527216,29.3607996018854,29.8595462510491,30.3582929002129,
30.8570395493767,31.3557861985405,31.8545328477043,32.353279496868,32.8520261460318,
33.3507727951956,33.8495194443594,34.3482660935232,34.5575191894878),
 .UNSPECIFIED.);
#3061=B_SPLINE_CURVE_WITH_KNOTS('',3,(#46678,#46679,#46680,#46681,#46682,
#46683,#46684,#46685,#46686,#46687,#46688,#46689,#46690,#46691,#46692,#46693),
 .UNSPECIFIED.,.F.,.F.,(4,1,1,1,1,1,1,1,1,1,1,1,1,4),(21.9911485751287,
22.3254132972903,22.8241599464541,23.3229065956179,23.8216532447817,24.3203998939455,
24.8191465431093,25.317893192273,25.8166398414368,26.3153864906006,26.8141331397644,
27.3128797889282,27.8116264380919,28.2743338823083),.UNSPECIFIED.);
#3062=B_SPLINE_CURVE_WITH_KNOTS('',3,(#46694,#46695,#46696,#46697,#46698,
#46699,#46700,#46701,#46702,#46703,#46704,#46705,#46706,#46707,#46708,#46709),
 .UNSPECIFIED.,.F.,.F.,(4,1,1,1,1,1,1,1,1,1,1,1,1,4),(21.9911485751286,
22.3783465135924,22.8770931627562,23.37583981192,23.8745864610838,24.3733331102476,
24.8720797594113,25.3708264085751,25.8695730577389,26.3683197069027,26.8670663560665,
27.3658130052302,27.864559654394,28.2743338823082),.UNSPECIFIED.);
#3063=B_SPLINE_CURVE_WITH_KNOTS('',3,(#46715,#46716,#46717,#46718,#46719,
#46720),.UNSPECIFIED.,.F.,.F.,(4,1,1,4),(14.3984001269719,14.8971467761357,
15.3958934252995,15.7079632679491),.UNSPECIFIED.);
#3064=B_SPLINE_CURVE_WITH_KNOTS('',3,(#46723,#46724,#46725,#46726,#46727,
#46728,#46729),.UNSPECIFIED.,.F.,.F.,(4,1,1,1,4),(13.8759337553363,14.3454669106698,
14.8442135598336,15.3429602089974,15.7079632679491),.UNSPECIFIED.);
#3065=B_SPLINE_CURVE_WITH_KNOTS('',3,(#46731,#46732,#46733,#46734,#46735,
#46736,#46737,#46738,#46739,#46740,#46741,#46742,#46743,#46744,#46745,#46746,
#46747),.UNSPECIFIED.,.F.,.F.,(4,1,1,1,1,1,1,1,1,1,1,1,1,1,4),(15.7079632679491,
15.8417068581612,16.340453507325,16.8392001564888,17.3379468056525,17.8366934548163,
18.3354401039801,18.8341867531439,19.3329334023077,19.8316800514714,20.3304267006352,
20.829173349799,21.3279199989628,21.8266666481266,21.9911485751287),
 .UNSPECIFIED.);
#3066=B_SPLINE_CURVE_WITH_KNOTS('',3,(#46748,#46749,#46750,#46751,#46752,
#46753,#46754,#46755,#46756,#46757,#46758,#46759,#46760,#46761,#46762,#46763,
#46764),.UNSPECIFIED.,.F.,.F.,(4,1,1,1,1,1,1,1,1,1,1,1,1,1,4),(15.7079632679491,
15.8946400744633,16.393386723627,16.8921333727908,17.3908800219546,17.8896266711184,
18.3883733202822,18.887119969446,19.3858666186097,19.8846132677735,20.3833599169373,
20.8821065661011,21.3808532152649,21.8795998644286,21.9911485751286),
 .UNSPECIFIED.);
#3067=B_SPLINE_CURVE_WITH_KNOTS('',3,(#48233,#48234,#48235,#48236,#48237,
#48238,#48239,#48240,#48241,#48242,#48243,#48244,#48245,#48246,#48247,#48248,
#48249,#48250,#48251,#48252,#48253,#48254,#48255,#48256,#48257,#48258,#48259,
#48260,#48261,#48262,#48263,#48264,#48265,#48266,#48267,#48268,#48269,#48270,
#48271,#48272,#48273,#48274,#48275,#48276,#48277,#48278,#48279,#48280,#48281,
#48282,#48283,#48284,#48285,#48286,#48287,#48288,#48289,#48290,#48291,#48292,
#48293,#48294,#48295,#48296,#48297,#48298,#48299,#48300,#48301,#48302,#48303,
#48304,#48305,#48306,#48307,#48308,#48309,#48310,#48311,#48312,#48313,#48314,
#48315,#48316,#48317,#48318,#48319,#48320,#48321,#48322,#48323,#48324,#48325,
#48326,#48327,#48328,#48329,#48330,#48331,#48332,#48333,#48334,#48335,#48336,
#48337,#48338,#48339,#48340,#48341,#48342,#48343,#48344),.UNSPECIFIED.,
 .F.,.F.,(4,3,3,3,3,3,3,3,3,3,3,3,3,3,3,3,3,3,3,3,3,3,3,3,3,3,3,3,3,3,3,
3,3,3,3,3,3,4),(0.,0.0505771409544137,0.101554208126943,0.152189059755351,
0.202216159570862,0.226885015823025,0.234012168591673,0.240461808082327,
0.29007953191694,0.300891584579511,0.350695312223996,0.400404404445326,
0.447850031768845,0.461476807659048,0.467766229912276,0.516330065625832,
0.564490190484642,0.590186913739402,0.638696313987249,0.667316948881319,
0.678175806101206,0.686355565587849,0.733761702748627,0.781038646687326,
0.827499605987411,0.867661393139807,0.884230290042188,0.893713740355506,
0.900277340341249,0.946756252637673,0.993258125372732,1.01069632764838,
1.01980492182733,1.02788458752219,1.07342337960794,1.11826391008869,1.13276374357791,
1.14791015664662),.UNSPECIFIED.);
#3068=B_SPLINE_CURVE_WITH_KNOTS('',3,(#48345,#48346,#48347,#48348,#48349,
#48350,#48351,#48352,#48353,#48354,#48355,#48356,#48357,#48358,#48359,#48360,
#48361,#48362,#48363,#48364,#48365,#48366,#48367,#48368,#48369,#48370,#48371,
#48372,#48373,#48374,#48375,#48376,#48377,#48378,#48379,#48380,#48381,#48382,
#48383,#48384,#48385,#48386,#48387,#48388,#48389,#48390,#48391,#48392,#48393,
#48394,#48395,#48396,#48397,#48398,#48399,#48400,#48401,#48402,#48403,#48404,
#48405,#48406,#48407,#48408,#48409,#48410,#48411,#48412,#48413,#48414,#48415,
#48416,#48417,#48418,#48419,#48420,#48421,#48422,#48423,#48424,#48425,#48426,
#48427,#48428,#48429,#48430,#48431,#48432,#48433,#48434,#48435,#48436,#48437,
#48438,#48439,#48440,#48441,#48442,#48443,#48444,#48445,#48446,#48447,#48448,
#48449,#48450,#48451,#48452,#48453,#48454,#48455,#48456),.UNSPECIFIED.,
 .F.,.F.,(4,3,3,3,3,3,3,3,3,3,3,3,3,3,3,3,3,3,3,3,3,3,3,3,3,3,3,3,3,3,3,
3,3,3,3,3,3,4),(0.,0.0443052074552335,0.0893948843442793,0.135141488872234,
0.180815870205597,0.19390940453382,0.201667660370645,0.207452222581038,
0.254168163209598,0.263945580324931,0.310166557321201,0.356931398910231,
0.40263742170911,0.412236182291169,0.41809909587038,0.465725175667907,0.513886757864765,
0.539755490105746,0.587673806547005,0.617618173044032,0.628955317157287,
0.635419183001384,0.684153162333737,0.73336012390645,0.782633804055213,
0.827228738523219,0.845892924266055,0.856064133573895,0.862657049097381,
0.91218656093736,0.962309907572726,0.982868071148884,0.998253759458264,
1.00640638253346,1.05732616428783,1.10834517305652,1.1258557104086,1.14369947197755),
 .UNSPECIFIED.);
#3069=B_SPLINE_CURVE_WITH_KNOTS('',3,(#48457,#48458,#48459,#48460,#48461,
#48462,#48463,#48464,#48465,#48466,#48467,#48468,#48469,#48470,#48471,#48472,
#48473,#48474,#48475,#48476,#48477,#48478,#48479,#48480,#48481,#48482,#48483,
#48484,#48485,#48486,#48487,#48488,#48489,#48490,#48491,#48492,#48493,#48494,
#48495,#48496,#48497,#48498,#48499),.UNSPECIFIED.,.F.,.F.,(4,3,3,3,3,3,
3,3,3,3,3,3,3,3,4),(-10.1394149102777,-9.97493298327562,-9.47618633411184,
-8.97743968494806,-8.47869303578428,-7.9799463866205,-7.48119973745672,
-6.98245308829294,-6.48370643912916,-5.98495978996538,-5.4862131408016,
-4.98746649163782,-4.48871984247403,-3.98997319331025,-3.85622960309811),
 .UNSPECIFIED.);
#3070=B_SPLINE_CURVE_WITH_KNOTS('',3,(#49968,#49969,#49970,#49971,#49972,
#49973,#49974,#49975,#49976,#49977,#49978,#49979,#49980,#49981,#49982,#49983,
#49984,#49985,#49986,#49987,#49988,#49989,#49990,#49991,#49992,#49993,#49994,
#49995,#49996,#49997,#49998,#49999,#50000,#50001,#50002,#50003,#50004,#50005,
#50006,#50007,#50008,#50009,#50010,#50011,#50012,#50013,#50014,#50015,#50016,
#50017,#50018,#50019,#50020,#50021,#50022,#50023,#50024,#50025,#50026,#50027,
#50028,#50029,#50030,#50031,#50032,#50033,#50034,#50035,#50036,#50037,#50038,
#50039,#50040,#50041,#50042,#50043,#50044,#50045,#50046,#50047,#50048,#50049,
#50050,#50051,#50052,#50053,#50054,#50055,#50056,#50057,#50058,#50059,#50060,
#50061,#50062,#50063,#50064,#50065,#50066,#50067,#50068,#50069,#50070,#50071,
#50072,#50073,#50074,#50075,#50076,#50077,#50078,#50079),.UNSPECIFIED.,
 .F.,.F.,(4,3,3,3,3,3,3,3,3,3,3,3,3,3,3,3,3,3,3,3,3,3,3,3,3,3,3,3,3,3,3,
3,3,3,3,3,3,4),(0.,0.0443052464394431,0.0893949539526172,0.13514156535071,
0.180815937906565,0.19390953278588,0.201668332261212,0.207452743931054,
0.254168704708716,0.263945580324925,0.310166527100594,0.356931351724118,
0.402637386319524,0.412236112021009,0.418099029289404,0.465725083881085,
0.513886660859732,0.539755490105741,0.58767381564034,0.617618181000692,
0.628955400664764,0.635419179939423,0.684153173701215,0.733360142889101,
0.782633822702733,0.827228738523158,0.845892924265991,0.856064134176901,
0.862657049292299,0.912186558109282,0.962309904124215,0.98286806942716,
0.998253758909606,1.00640638216257,1.05732616367401,1.1083451721479,1.12585571040848,
1.14369947197742),.UNSPECIFIED.);
#3071=B_SPLINE_CURVE_WITH_KNOTS('',3,(#50080,#50081,#50082,#50083,#50084,
#50085,#50086,#50087,#50088,#50089,#50090,#50091,#50092,#50093,#50094,#50095,
#50096,#50097,#50098,#50099,#50100,#50101,#50102,#50103,#50104,#50105,#50106,
#50107,#50108,#50109,#50110,#50111,#50112,#50113,#50114,#50115,#50116,#50117,
#50118,#50119),.UNSPECIFIED.,.F.,.F.,(4,3,3,3,3,3,3,3,3,3,3,3,3,4),(7.59274844815678,
7.9799463866205,8.47869303578429,8.97743968494807,9.47618633411185,9.97493298327563,
10.4736796324394,10.9724262816032,11.471172930767,11.9699195799308,12.4686662290945,
12.9674128782583,13.4661595274221,13.8759337553364),.UNSPECIFIED.);
#3072=B_SPLINE_CURVE_WITH_KNOTS('',3,(#50120,#50121,#50122,#50123,#50124,
#50125,#50126,#50127,#50128,#50129,#50130,#50131,#50132,#50133,#50134,#50135,
#50136,#50137,#50138,#50139,#50140,#50141,#50142,#50143,#50144,#50145,#50146,
#50147,#50148,#50149,#50150,#50151,#50152,#50153,#50154,#50155,#50156,#50157,
#50158,#50159,#50160,#50161,#50162,#50163,#50164,#50165,#50166,#50167,#50168,
#50169,#50170,#50171,#50172,#50173,#50174,#50175,#50176,#50177,#50178,#50179,
#50180,#50181,#50182,#50183,#50184,#50185,#50186,#50187,#50188,#50189,#50190,
#50191,#50192,#50193,#50194,#50195,#50196,#50197,#50198,#50199,#50200,#50201,
#50202,#50203,#50204,#50205,#50206,#50207,#50208,#50209,#50210,#50211,#50212,
#50213,#50214,#50215,#50216,#50217,#50218,#50219,#50220,#50221,#50222,#50223,
#50224,#50225,#50226,#50227,#50228,#50229,#50230,#50231),.UNSPECIFIED.,
 .F.,.F.,(4,3,3,3,3,3,3,3,3,3,3,3,3,3,3,3,3,3,3,3,3,3,3,3,3,3,3,3,3,3,3,
3,3,3,3,3,3,4),(0.,0.050577164702863,0.101554237110135,0.152189070454327,
0.202216145640601,0.226885005375326,0.234012130381444,0.240461803926884,
0.290079515630049,0.3008915845795,0.350695306957134,0.400404402970159,0.447850030662475,
0.461476805155705,0.46776622895846,0.516330065384172,0.564490196514962,
0.590186913739423,0.638696314494036,0.667316949324757,0.678175808158324,
0.686355565879716,0.7337617036123,0.781038648491377,0.827499614280347,0.867661393139803,
0.884230290042183,0.893713740915346,0.900277341547724,0.946756255255806,
0.993258127336325,1.01069632936652,1.01980492495367,1.02788458707311,1.07342337690414,
1.11826390001064,1.13276374357788,1.14791015664662),.UNSPECIFIED.);
#3073=B_SPLINE_CURVE_WITH_KNOTS('',3,(#50430,#50431,#50432,#50433,#50434,
#50435,#50436,#50437,#50438,#50439,#50440,#50441,#50442,#50443,#50444,#50445),
 .UNSPECIFIED.,.F.,.F.,(4,3,3,3,3,4),(-4.09254174883831,-3.99749770433369,
-3.49781049129198,-2.99812327825027,-2.49843606520856,-2.06980418878614),
 .UNSPECIFIED.);
#3074=B_SPLINE_CURVE_WITH_KNOTS('',3,(#50448,#50449,#50450,#50451,#50452,
#50453,#50454,#50455,#50456,#50457),.UNSPECIFIED.,.F.,.F.,(4,3,3,4),(0.,
0.499687213041709,0.999374426083416,1.11885509353794),.UNSPECIFIED.);
#3075=B_SPLINE_CURVE_WITH_KNOTS('',3,(#50462,#50463,#50464,#50465,#50466,
#50467,#50468,#50469,#50470,#50471,#50472,#50473,#50474,#50475,#50476,#50477,
#50478,#50479,#50480,#50481,#50482,#50483,#50484,#50485,#50486,#50487,#50488,
#50489,#50490,#50491,#50492,#50493,#50494,#50495,#50496,#50497,#50498,#50499,
#50500,#50501),.UNSPECIFIED.,.F.,.F.,(4,3,3,3,3,3,3,3,3,3,3,3,3,4),(-10.3757270560179,
-9.99374426083422,-9.49405704779251,-8.9943698347508,-8.49468262170909,
-7.99499540866738,-7.49530819562566,-6.99562098258395,-6.49593376954224,
-5.99624655650053,-5.49655934345882,-4.99687213041711,-4.4971849173754,
-4.09254174883831),.UNSPECIFIED.);
#3076=B_SPLINE_CURVE_WITH_KNOTS('',3,(#50502,#50503,#50504,#50505,#50506,
#50507,#50508,#50509,#50510,#50511,#50512,#50513,#50514,#50515,#50516,#50517,
#50518,#50519,#50520,#50521,#50522,#50523,#50524,#50525,#50526,#50527,#50528,
#50529,#50530,#50531,#50532,#50533,#50534,#50535,#50536,#50537,#50538,#50539,
#50540,#50541),.UNSPECIFIED.,.F.,.F.,(4,3,3,3,3,3,3,3,3,3,3,3,3,4),(1.11885509353794,
1.49906163912513,1.99874885216684,2.49843606520855,2.99812327825026,3.49781049129198,
3.99749770433369,4.4971849173754,4.99687213041711,5.49655934345882,5.99624655650054,
6.49593376954225,6.99562098258396,7.40204040071752),.UNSPECIFIED.);
#3077=B_SPLINE_CURVE_WITH_KNOTS('',3,(#50546,#50547,#50548,#50549,#50550,
#50551,#50552,#50553,#50554,#50555,#50556,#50557,#50558,#50559,#50560,#50561,
#50562,#50563,#50564,#50565,#50566,#50567,#50568,#50569,#50570,#50571,#50572,
#50573,#50574,#50575,#50576,#50577,#50578,#50579,#50580,#50581,#50582,#50583,
#50584,#50585,#50586,#50587,#50588),.UNSPECIFIED.,.F.,.F.,(4,3,3,3,3,3,
3,3,3,3,3,3,3,3,4),(-16.6589123631975,-16.4896780303765,-15.9899908173347,
-15.490303604293,-14.9906163912513,-14.4909291782096,-13.9912419651679,
-13.4915547521262,-12.9918675390845,-12.4921803260428,-11.9924931130011,
-11.4928058999594,-10.9931186869176,-10.4934314738759,-10.3757270560179),
 .UNSPECIFIED.);
#3078=B_SPLINE_CURVE_WITH_KNOTS('',3,(#50589,#50590,#50591,#50592,#50593,
#50594,#50595,#50596,#50597,#50598,#50599,#50600,#50601,#50602,#50603,#50604,
#50605,#50606,#50607,#50608,#50609,#50610,#50611,#50612,#50613,#50614,#50615,
#50616,#50617,#50618,#50619,#50620,#50621,#50622,#50623,#50624,#50625,#50626,
#50627,#50628,#50629,#50630,#50631),.UNSPECIFIED.,.F.,.F.,(4,3,3,3,3,3,
3,3,3,3,3,3,3,3,4),(7.40204040071752,7.49530819562567,7.99499540866738,
8.49468262170909,8.99436983475081,9.49405704779253,9.99374426083424,10.4934314738759,
10.9931186869177,11.4928058999594,11.9924931130011,12.4921803260428,12.9918675390845,
13.4915547521262,13.6852257078971),.UNSPECIFIED.);
#3079=B_SPLINE_CURVE_WITH_KNOTS('',3,(#50636,#50637,#50638,#50639,#50640,
#50641,#50642,#50643,#50644,#50645,#50646,#50647,#50648,#50649,#50650,#50651,
#50652,#50653,#50654,#50655,#50656,#50657,#50658,#50659,#50660,#50661,#50662,
#50663,#50664,#50665,#50666,#50667,#50668,#50669,#50670,#50671,#50672,#50673,
#50674,#50675),.UNSPECIFIED.,.F.,.F.,(4,3,3,3,3,3,3,3,3,3,3,3,3,4),(-22.9420976703771,
-22.485924586877,-21.9862373738353,-21.4865501607936,-20.9868629477519,
-20.4871757347102,-19.9874885216684,-19.4878013086267,-18.988114095585,
-18.4884268825433,-17.9887396695016,-17.4890524564599,-16.9893652434182,
-16.6589123631975),.UNSPECIFIED.);
#3080=B_SPLINE_CURVE_WITH_KNOTS('',3,(#50676,#50677,#50678,#50679,#50680,
#50681,#50682,#50683,#50684,#50685,#50686,#50687,#50688,#50689,#50690,#50691,
#50692,#50693,#50694,#50695,#50696,#50697,#50698,#50699,#50700,#50701,#50702,
#50703,#50704,#50705,#50706,#50707,#50708,#50709,#50710,#50711,#50712,#50713,
#50714,#50715),.UNSPECIFIED.,.F.,.F.,(4,3,3,3,3,3,3,3,3,3,3,3,3,4),(13.6852257078971,
13.9912419651679,14.4909291782096,14.9906163912513,15.4903036042931,15.9899908173348,
16.4896780303765,16.9893652434182,17.4890524564599,17.9887396695016,18.4884268825433,
18.988114095585,19.4878013086267,19.9684110150767),.UNSPECIFIED.);
#3081=B_SPLINE_CURVE_WITH_KNOTS('',3,(#50720,#50721,#50722,#50723,#50724,
#50725,#50726,#50727,#50728,#50729,#50730,#50731,#50732,#50733,#50734,#50735,
#50736,#50737,#50738,#50739,#50740,#50741,#50742,#50743,#50744,#50745,#50746,
#50747,#50748,#50749,#50750,#50751,#50752,#50753,#50754,#50755,#50756,#50757,
#50758,#50759,#50760,#50761,#50762),.UNSPECIFIED.,.F.,.F.,(4,3,3,3,3,3,
3,3,3,3,3,3,3,3,4),(-29.2252829775567,-28.9818583564192,-28.4821711433775,
-27.9824839303358,-27.4827967172941,-26.9831095042524,-26.4834222912107,
-25.983735078169,-25.4840478651273,-24.9843606520855,-24.4846734390438,
-23.9849862260021,-23.4852990129604,-22.9856117999187,-22.9420976703771),
 .UNSPECIFIED.);
#3082=B_SPLINE_CURVE_WITH_KNOTS('',3,(#50763,#50764,#50765,#50766,#50767,
#50768,#50769,#50770,#50771,#50772,#50773,#50774,#50775,#50776,#50777,#50778,
#50779,#50780,#50781,#50782,#50783,#50784,#50785,#50786,#50787,#50788,#50789,
#50790,#50791,#50792,#50793,#50794,#50795,#50796,#50797,#50798,#50799,#50800,
#50801,#50802,#50803,#50804,#50805),.UNSPECIFIED.,.F.,.F.,(4,3,3,3,3,3,
3,3,3,3,3,3,3,3,4),(19.9684110150767,19.9874885216684,20.4871757347102,
20.9868629477519,21.4865501607936,21.9862373738353,22.485924586877,22.9856117999187,
23.4852990129604,23.9849862260021,24.4846734390438,24.9843606520855,25.4840478651272,
25.983735078169,26.2515963222563),.UNSPECIFIED.);
#3083=B_SPLINE_CURVE_WITH_KNOTS('',3,(#50810,#50811,#50812,#50813,#50814,
#50815,#50816,#50817,#50818,#50819,#50820,#50821,#50822,#50823,#50824,#50825,
#50826,#50827,#50828,#50829,#50830,#50831,#50832,#50833,#50834,#50835,#50836,
#50837,#50838,#50839,#50840,#50841,#50842,#50843,#50844,#50845,#50846,#50847,
#50848,#50849,#50850,#50851,#50852),.UNSPECIFIED.,.F.,.F.,(4,3,3,3,3,3,
3,3,3,3,3,3,3,3,4),(-35.5084682847362,-35.4777921259615,-34.9781049129198,
-34.4784176998781,-33.9787304868363,-33.4790432737946,-32.9793560607529,
-32.4796688477112,-31.9799816346695,-31.4802944216278,-30.9806072085861,
-30.4809199955444,-29.9812327825027,-29.4815455694609,-29.2252829775567),
 .UNSPECIFIED.);
#3084=B_SPLINE_CURVE_WITH_KNOTS('',3,(#50853,#50854,#50855,#50856,#50857,
#50858,#50859,#50860,#50861,#50862,#50863,#50864,#50865,#50866,#50867,#50868,
#50869,#50870,#50871,#50872,#50873,#50874,#50875,#50876,#50877,#50878,#50879,
#50880,#50881,#50882,#50883,#50884,#50885,#50886,#50887,#50888,#50889,#50890,
#50891,#50892,#50893,#50894,#50895),.UNSPECIFIED.,.F.,.F.,(4,3,3,3,3,3,
3,3,3,3,3,3,3,3,4),(26.2515963222563,26.4834222912107,26.9831095042524,
27.4827967172941,27.9824839303358,28.4821711433775,28.9818583564192,29.481545569461,
29.9812327825027,30.4809199955444,30.9806072085861,31.4802944216278,31.9799816346695,
32.4796688477112,32.5347816294359),.UNSPECIFIED.);
#3085=B_SPLINE_CURVE_WITH_KNOTS('',3,(#50900,#50901,#50902,#50903,#50904,
#50905,#50906,#50907,#50908,#50909,#50910,#50911,#50912,#50913,#50914,#50915,
#50916,#50917,#50918,#50919,#50920,#50921,#50922,#50923,#50924,#50925,#50926,
#50927,#50928,#50929,#50930,#50931,#50932,#50933,#50934,#50935,#50936,#50937,
#50938,#50939),.UNSPECIFIED.,.F.,.F.,(4,3,3,3,3,3,3,3,3,3,3,3,3,4),(-41.7916535919158,
-41.474038682462,-40.9743514694203,-40.4746642563786,-39.9749770433369,
-39.4752898302952,-38.9756026172535,-38.4759154042117,-37.97622819117,-37.4765409781283,
-36.9768537650866,-36.4771665520449,-35.9774793390032,-35.5084682847362),
 .UNSPECIFIED.);
#3086=B_SPLINE_CURVE_WITH_KNOTS('',3,(#50940,#50941,#50942,#50943,#50944,
#50945,#50946,#50947,#50948,#50949,#50950,#50951,#50952,#50953,#50954,#50955,
#50956,#50957,#50958,#50959,#50960,#50961,#50962,#50963,#50964,#50965,#50966,
#50967,#50968,#50969,#50970,#50971,#50972,#50973,#50974,#50975,#50976,#50977,
#50978,#50979),.UNSPECIFIED.,.F.,.F.,(4,3,3,3,3,3,3,3,3,3,3,3,3,4),(32.5347816294359,
32.9793560607529,33.4790432737947,33.9787304868364,34.4784176998781,34.9781049129198,
35.4777921259615,35.9774793390032,36.4771665520449,36.9768537650866,37.4765409781283,
37.97622819117,38.4759154042117,38.8179669366154),.UNSPECIFIED.);
#3087=B_SPLINE_CURVE_WITH_KNOTS('',3,(#50984,#50985,#50986,#50987,#50988,
#50989,#50990,#50991,#50992,#50993,#50994,#50995,#50996,#50997,#50998,#50999,
#51000,#51001,#51002,#51003,#51004,#51005,#51006,#51007,#51008,#51009,#51010,
#51011,#51012,#51013,#51014,#51015,#51016,#51017,#51018,#51019,#51020,#51021,
#51022,#51023,#51024,#51025,#51026),.UNSPECIFIED.,.F.,.F.,(4,3,3,3,3,3,
3,3,3,3,3,3,3,3,4),(-48.0748388990954,-47.9699724520042,-47.4702852389625,
-46.9705980259208,-46.4709108128791,-45.9712235998374,-45.4715363867957,
-44.971849173754,-44.4721619607123,-43.9724747476706,-43.4727875346288,
-42.9731003215871,-42.4734131085454,-41.9737258955037,-41.7916535919158),
 .UNSPECIFIED.);
#3088=B_SPLINE_CURVE_WITH_KNOTS('',3,(#51027,#51028,#51029,#51030,#51031,
#51032,#51033,#51034,#51035,#51036,#51037,#51038,#51039,#51040,#51041,#51042,
#51043,#51044,#51045,#51046,#51047,#51048,#51049,#51050,#51051,#51052,#51053,
#51054,#51055,#51056,#51057,#51058,#51059,#51060,#51061,#51062,#51063,#51064,
#51065,#51066,#51067,#51068,#51069),.UNSPECIFIED.,.F.,.F.,(4,3,3,3,3,3,
3,3,3,3,3,3,3,3,4),(38.8179669366154,38.9756026172534,39.4752898302952,
39.9749770433369,40.4746642563786,40.9743514694203,41.474038682462,41.9737258955037,
42.4734131085454,42.9731003215871,43.4727875346289,43.9724747476706,44.4721619607123,
44.971849173754,45.101152243795),.UNSPECIFIED.);
#3089=B_SPLINE_CURVE_WITH_KNOTS('',3,(#51074,#51075,#51076,#51077,#51078,
#51079,#51080,#51081,#51082,#51083,#51084,#51085,#51086,#51087,#51088,#51089,
#51090,#51091,#51092,#51093,#51094,#51095,#51096,#51097,#51098,#51099,#51100,
#51101,#51102,#51103,#51104,#51105,#51106,#51107,#51108,#51109,#51110,#51111,
#51112,#51113),.UNSPECIFIED.,.F.,.F.,(4,3,3,3,3,3,3,3,3,3,3,3,3,4),(-54.358024206275,
-53.9662190085048,-53.4665317954631,-52.9668445824214,-52.4671573693797,
-51.9674701563379,-51.4677829432962,-50.9680957302545,-50.4684085172128,
-49.9687213041711,-49.4690340911294,-48.9693468780877,-48.469659665046,
-48.0748388990954),.UNSPECIFIED.);
#3090=B_SPLINE_CURVE_WITH_KNOTS('',3,(#51114,#51115,#51116,#51117,#51118,
#51119,#51120,#51121,#51122,#51123,#51124,#51125,#51126,#51127,#51128,#51129,
#51130,#51131,#51132,#51133,#51134,#51135,#51136,#51137,#51138,#51139,#51140,
#51141,#51142,#51143,#51144,#51145,#51146,#51147,#51148,#51149,#51150,#51151,
#51152,#51153),.UNSPECIFIED.,.F.,.F.,(4,3,3,3,3,3,3,3,3,3,3,3,3,4),(45.101152243795,
45.4715363867957,45.9712235998374,46.4709108128791,46.9705980259208,47.4702852389625,
47.9699724520043,48.469659665046,48.9693468780877,49.4690340911294,49.9687213041711,
50.4684085172128,50.9680957302545,51.3843375509746),.UNSPECIFIED.);
#3091=B_SPLINE_CURVE_WITH_KNOTS('',3,(#51158,#51159,#51160,#51161,#51162,
#51163,#51164,#51165,#51166,#51167,#51168,#51169,#51170,#51171,#51172,#51173,
#51174,#51175,#51176,#51177,#51178,#51179,#51180,#51181,#51182,#51183,#51184,
#51185,#51186,#51187,#51188,#51189,#51190,#51191,#51192,#51193,#51194,#51195,
#51196,#51197,#51198,#51199,#51200),.UNSPECIFIED.,.F.,.F.,(4,3,3,3,3,3,
3,3,3,3,3,3,3,3,4),(-60.6412095134546,-60.462152778047,-59.9624655650053,
-59.4627783519636,-58.9630911389219,-58.4634039258802,-57.9637167128385,
-57.4640294997968,-56.964342286755,-56.4646550737133,-55.9649678606716,
-55.4652806476299,-54.9655934345882,-54.4659062215465,-54.358024206275),
 .UNSPECIFIED.);
#3092=B_SPLINE_CURVE_WITH_KNOTS('',3,(#51201,#51202,#51203,#51204,#51205,
#51206,#51207,#51208,#51209,#51210,#51211,#51212,#51213,#51214,#51215,#51216,
#51217,#51218,#51219,#51220,#51221,#51222,#51223,#51224,#51225,#51226,#51227,
#51228,#51229,#51230,#51231,#51232,#51233,#51234,#51235,#51236,#51237,#51238,
#51239,#51240,#51241,#51242,#51243),.UNSPECIFIED.,.F.,.F.,(4,3,3,3,3,3,
3,3,3,3,3,3,3,3,4),(51.3843375509746,51.4677829432962,51.967470156338,52.4671573693797,
52.9668445824214,53.4665317954631,53.9662190085048,54.4659062215465,54.9655934345882,
55.4652806476299,55.9649678606716,56.4646550737133,56.964342286755,57.4640294997968,
57.6675228581542),.UNSPECIFIED.);
#3093=B_SPLINE_CURVE_WITH_KNOTS('',3,(#51248,#51249,#51250,#51251,#51252,
#51253,#51254,#51255,#51256,#51257,#51258,#51259,#51260,#51261,#51262,#51263,
#51264,#51265,#51266,#51267,#51268,#51269,#51270,#51271,#51272,#51273,#51274,
#51275,#51276,#51277,#51278,#51279,#51280,#51281,#51282,#51283,#51284,#51285,
#51286,#51287),.UNSPECIFIED.,.F.,.F.,(4,3,3,3,3,3,3,3,3,3,3,3,3,4),(-66.9243948206342,
-66.4583993345476,-65.9587121215058,-65.4590249084641,-64.9593376954224,
-64.4596504823807,-63.959963269339,-63.4602760562973,-62.9605888432556,
-62.4609016302139,-61.9612144171722,-61.4615272041304,-60.9618399910887,
-60.6412095134546),.UNSPECIFIED.);
#3094=B_SPLINE_CURVE_WITH_KNOTS('',3,(#51288,#51289,#51290,#51291,#51292,
#51293,#51294,#51295,#51296,#51297,#51298,#51299,#51300,#51301,#51302,#51303,
#51304,#51305,#51306,#51307,#51308,#51309,#51310,#51311,#51312,#51313,#51314,
#51315,#51316,#51317,#51318,#51319,#51320,#51321,#51322,#51323,#51324,#51325,
#51326,#51327),.UNSPECIFIED.,.F.,.F.,(4,3,3,3,3,3,3,3,3,3,3,3,3,4),(57.6675228581542,
57.9637167128385,58.4634039258802,58.9630911389219,59.4627783519636,59.9624655650053,
60.462152778047,60.9618399910887,61.4615272041304,61.9612144171722,62.4609016302139,
62.9605888432556,63.4602760562973,63.9507081653338),.UNSPECIFIED.);
#3095=B_SPLINE_CURVE_WITH_KNOTS('',3,(#51332,#51333,#51334,#51335,#51336,
#51337,#51338,#51339,#51340,#51341,#51342,#51343,#51344,#51345,#51346,#51347,
#51348,#51349,#51350,#51351,#51352,#51353,#51354,#51355,#51356,#51357,#51358,
#51359,#51360,#51361,#51362,#51363,#51364,#51365,#51366,#51367,#51368,#51369,
#51370,#51371,#51372,#51373,#51374),.UNSPECIFIED.,.F.,.F.,(4,3,3,3,3,3,
3,3,3,3,3,3,3,3,4),(-73.2075801278138,-72.9543331040898,-72.4546458910481,
-71.9549586780064,-71.4552714649647,-70.9555842519229,-70.4558970388812,
-69.9562098258395,-69.4565226127978,-68.9568353997561,-68.4571481867144,
-67.9574609736727,-67.457773760631,-66.9580865475893,-66.9243948206342),
 .UNSPECIFIED.);
#3096=B_SPLINE_CURVE_WITH_KNOTS('',3,(#51375,#51376,#51377,#51378,#51379,
#51380,#51381,#51382,#51383,#51384,#51385,#51386,#51387,#51388,#51389,#51390,
#51391,#51392,#51393,#51394,#51395,#51396,#51397,#51398,#51399,#51400,#51401,
#51402,#51403,#51404,#51405,#51406,#51407,#51408,#51409,#51410,#51411,#51412,
#51413,#51414,#51415,#51416,#51417),.UNSPECIFIED.,.F.,.F.,(4,3,3,3,3,3,
3,3,3,3,3,3,3,3,4),(63.9507081653338,63.959963269339,64.4596504823807,64.9593376954224,
65.4590249084641,65.9587121215058,66.4583993345476,66.9580865475893,67.457773760631,
67.9574609736727,68.4571481867144,68.9568353997561,69.4565226127979,69.9562098258396,
70.2338934725134),.UNSPECIFIED.);
#3097=B_SPLINE_CURVE_WITH_KNOTS('',3,(#51422,#51423,#51424,#51425,#51426,
#51427,#51428,#51429,#51430,#51431,#51432,#51433,#51434,#51435,#51436,#51437,
#51438,#51439,#51440,#51441,#51442,#51443,#51444,#51445,#51446,#51447,#51448,
#51449,#51450,#51451,#51452,#51453,#51454,#51455,#51456,#51457,#51458,#51459,
#51460,#51461,#51462,#51463,#51464),.UNSPECIFIED.,.F.,.F.,(4,3,3,3,3,3,
3,3,3,3,3,3,3,3,4),(-79.4907654349934,-79.450266873632,-78.9505796605903,
-78.4508924475486,-77.9512052345069,-77.4515180214652,-76.9518308084235,
-76.4521435953818,-75.9524563823401,-75.4527691692983,-74.9530819562566,
-74.4533947432149,-73.9537075301732,-73.4540203171315,-73.2075801278138),
 .UNSPECIFIED.);
#3098=B_SPLINE_CURVE_WITH_KNOTS('',3,(#51465,#51466,#51467,#51468,#51469,
#51470,#51471,#51472,#51473,#51474,#51475,#51476,#51477,#51478,#51479,#51480,
#51481,#51482,#51483,#51484,#51485,#51486,#51487,#51488,#51489,#51490,#51491,
#51492,#51493,#51494,#51495,#51496,#51497,#51498,#51499,#51500,#51501,#51502,
#51503,#51504,#51505,#51506,#51507),.UNSPECIFIED.,.F.,.F.,(4,3,3,3,3,3,
3,3,3,3,3,3,3,3,4),(70.2338934725134,70.4558970388813,70.955584251923,71.4552714649647,
71.9549586780064,72.4546458910481,72.9543331040898,73.4540203171315,73.9537075301732,
74.4533947432149,74.9530819562566,75.4527691692983,75.95245638234,76.4521435953817,
76.517078779693),.UNSPECIFIED.);
#3099=B_SPLINE_CURVE_WITH_KNOTS('',3,(#51512,#51513,#51514,#51515,#51516,
#51517,#51518,#51519,#51520,#51521,#51522,#51523,#51524,#51525,#51526,#51527,
#51528,#51529,#51530,#51531,#51532,#51533,#51534,#51535,#51536,#51537,#51538,
#51539,#51540,#51541,#51542,#51543,#51544,#51545,#51546,#51547,#51548,#51549,
#51550,#51551),.UNSPECIFIED.,.F.,.F.,(4,3,3,3,3,3,3,3,3,3,3,3,3,4),(-85.773950742173,
-85.4465134301326,-84.9468262170908,-84.4471390040491,-83.9474517910074,
-83.4477645779657,-82.948077364924,-82.4483901518823,-81.9487029388406,
-81.4490157257989,-80.9493285127572,-80.4496412997155,-79.9499540866738,
-79.4907654349934),.UNSPECIFIED.);
#3100=B_SPLINE_CURVE_WITH_KNOTS('',3,(#51552,#51553,#51554,#51555,#51556,
#51557,#51558,#51559,#51560,#51561,#51562,#51563,#51564,#51565,#51566,#51567,
#51568,#51569,#51570,#51571,#51572,#51573,#51574,#51575,#51576,#51577,#51578,
#51579,#51580,#51581,#51582,#51583,#51584,#51585,#51586,#51587,#51588,#51589,
#51590,#51591),.UNSPECIFIED.,.F.,.F.,(4,3,3,3,3,3,3,3,3,3,3,3,3,4),(76.517078779693,
76.9518308084235,77.4515180214652,77.9512052345069,78.4508924475486,78.9505796605903,
79.450266873632,79.9499540866737,80.4496412997155,80.9493285127572,81.4490157257989,
81.9487029388406,82.4483901518823,82.8002640868726),.UNSPECIFIED.);
#3101=B_SPLINE_CURVE_WITH_KNOTS('',3,(#51596,#51597,#51598,#51599,#51600,
#51601,#51602,#51603,#51604,#51605,#51606,#51607,#51608,#51609,#51610,#51611,
#51612,#51613,#51614,#51615,#51616,#51617,#51618,#51619,#51620,#51621,#51622,
#51623,#51624,#51625,#51626,#51627,#51628,#51629,#51630,#51631,#51632,#51633,
#51634,#51635,#51636,#51637,#51638),.UNSPECIFIED.,.F.,.F.,(4,3,3,3,3,3,
3,3,3,3,3,3,3,3,4),(-92.0571360493526,-91.9424471996748,-91.4427599866331,
-90.9430727735914,-90.4433855605497,-89.943698347508,-89.4440111344663,
-88.9443239214246,-88.4446367083828,-87.9449494953411,-87.4452622822994,
-86.9455750692577,-86.445887856216,-85.9462006431743,-85.773950742173),
 .UNSPECIFIED.);
#3102=B_SPLINE_CURVE_WITH_KNOTS('',3,(#51639,#51640,#51641,#51642,#51643,
#51644,#51645,#51646,#51647,#51648,#51649,#51650,#51651,#51652,#51653,#51654,
#51655,#51656,#51657,#51658,#51659,#51660,#51661,#51662,#51663,#51664,#51665,
#51666,#51667,#51668,#51669,#51670,#51671,#51672,#51673,#51674,#51675,#51676,
#51677,#51678,#51679,#51680,#51681),.UNSPECIFIED.,.F.,.F.,(4,3,3,3,3,3,
3,3,3,3,3,3,3,3,4),(82.8002640868726,82.948077364924,83.4477645779658,83.9474517910075,
84.4471390040491,84.9468262170909,85.4465134301326,85.9462006431743,86.445887856216,
86.9455750692577,87.4452622822994,87.9449494953411,88.4446367083828,88.9443239214245,
89.0834493940522),.UNSPECIFIED.);
#3103=B_SPLINE_CURVE_WITH_KNOTS('',3,(#51686,#51687,#51688,#51689,#51690,
#51691,#51692,#51693,#51694,#51695,#51696,#51697,#51698,#51699,#51700,#51701,
#51702,#51703,#51704,#51705,#51706,#51707,#51708,#51709,#51710,#51711,#51712,
#51713,#51714,#51715,#51716,#51717,#51718,#51719,#51720,#51721,#51722,#51723,
#51724,#51725),.UNSPECIFIED.,.F.,.F.,(4,3,3,3,3,3,3,3,3,3,3,3,3,4),(-98.3403213565322,
-97.9386937561753,-97.4390065431336,-96.9393193300919,-96.4396321170502,
-95.9399449040085,-95.4402576909668,-94.940570477925,-94.4408832648834,
-93.9411960518416,-93.4415088387999,-92.9418216257582,-92.4421344127165,
-92.0571360493526),.UNSPECIFIED.);
#3104=B_SPLINE_CURVE_WITH_KNOTS('',3,(#51726,#51727,#51728,#51729,#51730,
#51731,#51732,#51733,#51734,#51735,#51736,#51737,#51738,#51739,#51740,#51741,
#51742,#51743,#51744,#51745,#51746,#51747,#51748,#51749,#51750,#51751,#51752,
#51753,#51754,#51755,#51756,#51757,#51758,#51759,#51760,#51761,#51762,#51763,
#51764,#51765),.UNSPECIFIED.,.F.,.F.,(4,3,3,3,3,3,3,3,3,3,3,3,3,4),(89.0834493940522,
89.4440111344662,89.943698347508,90.4433855605497,90.9430727735914,91.4427599866331,
91.9424471996748,92.4421344127165,92.9418216257583,93.4415088388,93.9411960518417,
94.4408832648834,94.9405704779251,95.3666347012318),.UNSPECIFIED.);
#3105=B_SPLINE_CURVE_WITH_KNOTS('',3,(#51770,#51771,#51772,#51773,#51774,
#51775,#51776,#51777,#51778,#51779,#51780,#51781,#51782,#51783,#51784,#51785,
#51786,#51787,#51788,#51789,#51790,#51791,#51792,#51793,#51794,#51795,#51796,
#51797,#51798,#51799,#51800,#51801,#51802,#51803,#51804,#51805,#51806,#51807,
#51808,#51809,#51810,#51811,#51812),.UNSPECIFIED.,.F.,.F.,(4,3,3,3,3,3,
3,3,3,3,3,3,3,3,4),(-104.623506663712,-104.434627525718,-103.934940312676,
-103.435253099634,-102.935565886592,-102.435878673551,-101.936191460509,
-101.436504247467,-100.936817034426,-100.437129821384,-99.9374426083422,
-99.4377553953005,-98.9380681822588,-98.4383809692171,-98.3403213565322),
 .UNSPECIFIED.);
#3106=B_SPLINE_CURVE_WITH_KNOTS('',3,(#51813,#51814,#51815,#51816,#51817,
#51818,#51819,#51820,#51821,#51822,#51823,#51824,#51825,#51826,#51827,#51828,
#51829,#51830,#51831,#51832,#51833,#51834,#51835,#51836,#51837,#51838,#51839,
#51840,#51841,#51842,#51843,#51844,#51845,#51846,#51847,#51848,#51849,#51850,
#51851,#51852,#51853,#51854,#51855),.UNSPECIFIED.,.F.,.F.,(4,3,3,3,3,3,
3,3,3,3,3,3,3,3,4),(95.3666347012318,95.4402576909668,95.9399449040085,
96.4396321170502,96.9393193300919,97.4390065431336,97.9386937561753,98.438380969217,
98.9380681822587,99.4377553953005,99.9374426083422,100.437129821384,100.936817034426,
101.436504247467,101.649820008411),.UNSPECIFIED.);
#3107=B_SPLINE_CURVE_WITH_KNOTS('',3,(#51860,#51861,#51862,#51863,#51864,
#51865,#51866,#51867,#51868,#51869,#51870,#51871,#51872,#51873,#51874,#51875,
#51876,#51877,#51878,#51879,#51880,#51881,#51882,#51883,#51884,#51885,#51886,
#51887,#51888,#51889,#51890,#51891,#51892,#51893,#51894,#51895,#51896,#51897,
#51898,#51899),.UNSPECIFIED.,.F.,.F.,(4,3,3,3,3,3,3,3,3,3,3,3,3,4),(-110.906691970891,
-110.430874082218,-109.931186869176,-109.431499656135,-108.931812443093,
-108.432125230051,-107.93243801701,-107.432750803968,-106.933063590926,
-106.433376377884,-105.933689164843,-105.434001951801,-104.934314738759,
-104.623506663712),.UNSPECIFIED.);
#3108=B_SPLINE_CURVE_WITH_KNOTS('',3,(#51900,#51901,#51902,#51903,#51904,
#51905,#51906,#51907,#51908,#51909,#51910,#51911,#51912,#51913,#51914,#51915,
#51916,#51917,#51918,#51919,#51920,#51921,#51922,#51923,#51924,#51925,#51926,
#51927,#51928,#51929,#51930,#51931,#51932,#51933,#51934,#51935,#51936,#51937,
#51938,#51939),.UNSPECIFIED.,.F.,.F.,(4,3,3,3,3,3,3,3,3,3,3,3,3,4),(101.649820008411,
101.936191460509,102.435878673551,102.935565886592,103.435253099634,103.934940312676,
104.434627525718,104.934314738759,105.434001951801,105.933689164843,106.433376377884,
106.933063590926,107.432750803968,107.933005315591),.UNSPECIFIED.);
#3109=B_SPLINE_CURVE_WITH_KNOTS('',3,(#51944,#51945,#51946,#51947,#51948,
#51949,#51950,#51951,#51952,#51953,#51954,#51955,#51956,#51957,#51958,#51959,
#51960,#51961,#51962,#51963,#51964,#51965,#51966,#51967,#51968,#51969,#51970,
#51971,#51972,#51973,#51974,#51975,#51976,#51977,#51978,#51979,#51980,#51981,
#51982,#51983,#51984,#51985,#51986),.UNSPECIFIED.,.F.,.F.,(4,3,3,3,3,3,
3,3,3,3,3,3,3,3,4),(-117.189877278071,-116.92680785176,-116.427120638719,
-115.927433425677,-115.427746212635,-114.928058999594,-114.428371786552,
-113.92868457351,-113.428997360468,-112.929310147427,-112.429622934385,
-111.929935721343,-111.430248508302,-110.93056129526,-110.906691970891),
 .UNSPECIFIED.);
#3110=B_SPLINE_CURVE_WITH_KNOTS('',3,(#51987,#51988,#51989,#51990,#51991,
#51992,#51993,#51994,#51995,#51996,#51997,#51998,#51999,#52000,#52001,#52002,
#52003,#52004,#52005,#52006,#52007,#52008,#52009,#52010,#52011,#52012,#52013,
#52014,#52015,#52016,#52017,#52018,#52019,#52020,#52021,#52022,#52023,#52024,
#52025,#52026),.UNSPECIFIED.,.F.,.F.,(4,3,3,3,3,3,3,3,3,3,3,3,3,4),(107.933005315591,
108.432125230051,108.931812443093,109.431499656135,109.931186869176,110.430874082218,
110.93056129526,111.430248508302,111.929935721343,112.429622934385,112.929310147427,
113.428997360468,113.92868457351,114.216190622771),.UNSPECIFIED.);
#3111=B_SPLINE_CURVE_WITH_KNOTS('',3,(#52031,#52032,#52033,#52034,#52035,
#52036,#52037,#52038,#52039,#52040,#52041,#52042,#52043,#52044,#52045,#52046,
#52047,#52048,#52049,#52050,#52051,#52052,#52053,#52054,#52055,#52056,#52057,
#52058,#52059,#52060,#52061,#52062,#52063,#52064,#52065,#52066,#52067,#52068,
#52069,#52070,#52071,#52072,#52073),.UNSPECIFIED.,.F.,.F.,(4,3,3,3,3,3,
3,3,3,3,3,3,3,3,4),(-123.473062585251,-123.422741621303,-122.923054408261,
-122.423367195219,-121.923679982177,-121.423992769136,-120.924305556094,
-120.424618343052,-119.924931130011,-119.425243916969,-118.925556703927,
-118.425869490885,-117.926182277844,-117.426495064802,-117.189877278071),
 .UNSPECIFIED.);
#3112=B_SPLINE_CURVE_WITH_KNOTS('',3,(#52074,#52075,#52076,#52077,#52078,
#52079,#52080,#52081,#52082,#52083,#52084,#52085,#52086,#52087,#52088,#52089,
#52090,#52091,#52092,#52093,#52094,#52095,#52096,#52097,#52098,#52099,#52100,
#52101,#52102,#52103,#52104,#52105,#52106,#52107,#52108,#52109,#52110,#52111,
#52112,#52113,#52114,#52115,#52116),.UNSPECIFIED.,.F.,.F.,(4,3,3,3,3,3,
3,3,3,3,3,3,3,3,4),(114.216190622771,114.428371786552,114.928058999594,
115.427746212635,115.927433425677,116.427120638719,116.92680785176,117.426495064802,
117.926182277844,118.425869490886,118.925556703927,119.425243916969,119.924931130011,
120.424618343052,120.49937592995),.UNSPECIFIED.);
#3113=B_SPLINE_CURVE_WITH_KNOTS('',3,(#52121,#52122,#52123,#52124,#52125,
#52126,#52127,#52128,#52129,#52130,#52131,#52132,#52133,#52134,#52135,#52136,
#52137,#52138,#52139,#52140,#52141,#52142,#52143,#52144,#52145,#52146,#52147,
#52148,#52149,#52150,#52151,#52152,#52153,#52154,#52155,#52156,#52157,#52158,
#52159,#52160),.UNSPECIFIED.,.F.,.F.,(4,3,3,3,3,3,3,3,3,3,3,3,3,4),(-129.75624789243,
-129.418988177803,-128.919300964761,-128.41961375172,-127.919926538678,
-127.420239325636,-126.920552112595,-126.420864899553,-125.921177686511,
-125.421490473469,-124.921803260428,-124.422116047386,-123.922428834344,
-123.473062585251),.UNSPECIFIED.);
#3114=B_SPLINE_CURVE_WITH_KNOTS('',3,(#52161,#52162,#52163,#52164,#52165,
#52166,#52167,#52168,#52169,#52170,#52171,#52172,#52173,#52174,#52175,#52176,
#52177,#52178,#52179,#52180,#52181,#52182,#52183,#52184,#52185,#52186,#52187,
#52188,#52189,#52190,#52191,#52192,#52193,#52194,#52195,#52196,#52197,#52198,
#52199,#52200),.UNSPECIFIED.,.F.,.F.,(4,3,3,3,3,3,3,3,3,3,3,3,3,4),(120.49937592995,
120.924305556094,121.423992769136,121.923679982177,122.423367195219,122.923054408261,
123.422741621303,123.922428834344,124.422116047386,124.921803260428,125.421490473469,
125.921177686511,126.420864899553,126.78256123713),.UNSPECIFIED.);
#3115=B_SPLINE_CURVE_WITH_KNOTS('',3,(#52205,#52206,#52207,#52208,#52209,
#52210,#52211,#52212,#52213,#52214,#52215,#52216,#52217,#52218,#52219,#52220,
#52221,#52222,#52223,#52224,#52225,#52226,#52227,#52228,#52229,#52230,#52231,
#52232,#52233,#52234,#52235,#52236,#52237,#52238,#52239,#52240,#52241,#52242,
#52243,#52244,#52245,#52246,#52247),.UNSPECIFIED.,.F.,.F.,(4,3,3,3,3,3,
3,3,3,3,3,3,3,3,4),(-136.03943319961,-135.914921947345,-135.415234734304,
-134.915547521262,-134.41586030822,-133.916173095179,-133.416485882137,
-132.916798669095,-132.417111456053,-131.917424243012,-131.41773702997,
-130.918049816928,-130.418362603887,-129.918675390845,-129.75624789243),
 .UNSPECIFIED.);
#3116=B_SPLINE_CURVE_WITH_KNOTS('',3,(#52248,#52249,#52250,#52251,#52252,
#52253,#52254,#52255,#52256,#52257,#52258,#52259,#52260,#52261,#52262,#52263,
#52264,#52265,#52266,#52267,#52268,#52269,#52270,#52271,#52272,#52273,#52274,
#52275,#52276,#52277,#52278,#52279,#52280,#52281,#52282,#52283,#52284,#52285,
#52286,#52287,#52288,#52289,#52290),.UNSPECIFIED.,.F.,.F.,(4,3,3,3,3,3,
3,3,3,3,3,3,3,3,4),(126.78256123713,126.920552112595,127.420239325636,127.919926538678,
128.41961375172,128.919300964761,129.418988177803,129.918675390845,130.418362603887,
130.918049816928,131.41773702997,131.917424243012,132.417111456053,132.916798669095,
133.065746544309),.UNSPECIFIED.);
#3117=B_SPLINE_CURVE_WITH_KNOTS('',3,(#52295,#52296,#52297,#52298,#52299,
#52300,#52301,#52302,#52303,#52304,#52305,#52306,#52307,#52308,#52309,#52310,
#52311,#52312,#52313,#52314,#52315,#52316,#52317,#52318,#52319,#52320,#52321,
#52322,#52323,#52324,#52325,#52326,#52327,#52328,#52329,#52330,#52331,#52332,
#52333,#52334),.UNSPECIFIED.,.F.,.F.,(4,3,3,3,3,3,3,3,3,3,3,3,3,4),(-142.322618506789,
-141.911168503846,-141.411481290804,-140.911794077762,-140.412106864721,
-139.912419651679,-139.412732438637,-138.913045225596,-138.413358012554,
-137.913670799512,-137.41398358647,-136.914296373429,-136.414609160387,
-136.03943319961),.UNSPECIFIED.);
#3118=B_SPLINE_CURVE_WITH_KNOTS('',3,(#52335,#52336,#52337,#52338,#52339,
#52340,#52341,#52342,#52343,#52344,#52345,#52346,#52347,#52348,#52349,#52350,
#52351,#52352,#52353,#52354,#52355,#52356,#52357,#52358,#52359,#52360,#52361,
#52362,#52363,#52364,#52365,#52366,#52367,#52368,#52369,#52370,#52371,#52372,
#52373,#52374),.UNSPECIFIED.,.F.,.F.,(4,3,3,3,3,3,3,3,3,3,3,3,3,4),(133.065746544309,
133.416485882137,133.916173095178,134.41586030822,134.915547521262,135.415234734304,
135.914921947345,136.414609160387,136.914296373429,137.41398358647,137.913670799512,
138.413358012554,138.913045225596,139.348931851489),.UNSPECIFIED.);
#3119=B_SPLINE_CURVE_WITH_KNOTS('',3,(#52379,#52380,#52381,#52382,#52383,
#52384,#52385,#52386,#52387,#52388,#52389,#52390,#52391,#52392,#52393,#52394,
#52395,#52396,#52397,#52398,#52399,#52400,#52401,#52402,#52403,#52404,#52405,
#52406,#52407,#52408,#52409,#52410,#52411,#52412,#52413,#52414,#52415,#52416,
#52417,#52418,#52419,#52420,#52421),.UNSPECIFIED.,.F.,.F.,(4,3,3,3,3,3,
3,3,3,3,3,3,3,3,4),(-148.605803813969,-148.407102273388,-147.907415060346,
-147.407727847305,-146.908040634263,-146.408353421221,-145.90866620818,
-145.408978995138,-144.909291782096,-144.409604569054,-143.909917356013,
-143.410230142971,-142.910542929929,-142.410855716888,-142.322618506789),
 .UNSPECIFIED.);
#3120=B_SPLINE_CURVE_WITH_KNOTS('',3,(#52422,#52423,#52424,#52425,#52426,
#52427,#52428,#52429,#52430,#52431,#52432,#52433,#52434,#52435,#52436,#52437,
#52438,#52439,#52440,#52441,#52442,#52443,#52444,#52445,#52446,#52447,#52448,
#52449,#52450,#52451,#52452,#52453,#52454,#52455,#52456,#52457,#52458,#52459,
#52460,#52461,#52462,#52463,#52464),.UNSPECIFIED.,.F.,.F.,(4,3,3,3,3,3,
3,3,3,3,3,3,3,3,4),(139.348931851489,139.412732438637,139.912419651679,
140.412106864721,140.911794077762,141.411481290804,141.911168503846,142.410855716888,
142.910542929929,143.410230142971,143.909917356013,144.409604569054,144.909291782096,
145.408978995138,145.632117158668),.UNSPECIFIED.);
#3121=B_SPLINE_CURVE_WITH_KNOTS('',3,(#52469,#52470,#52471,#52472,#52473,
#52474,#52475,#52476,#52477,#52478,#52479,#52480,#52481,#52482,#52483,#52484,
#52485,#52486,#52487,#52488,#52489,#52490,#52491,#52492,#52493,#52494,#52495,
#52496,#52497,#52498,#52499,#52500,#52501,#52502,#52503,#52504,#52505,#52506,
#52507,#52508),.UNSPECIFIED.,.F.,.F.,(4,3,3,3,3,3,3,3,3,3,3,3,3,4),(-154.888989121148,
-154.403348829889,-153.903661616847,-153.403974403805,-152.904287190764,
-152.404599977722,-151.90491276468,-151.405225551638,-150.905538338597,
-150.405851125555,-149.906163912513,-149.406476699472,-148.90678948643,
-148.605803813969),.UNSPECIFIED.);
#3122=B_SPLINE_CURVE_WITH_KNOTS('',3,(#52509,#52510,#52511,#52512,#52513,
#52514,#52515,#52516,#52517,#52518,#52519,#52520,#52521,#52522,#52523,#52524,
#52525,#52526,#52527,#52528,#52529,#52530,#52531,#52532,#52533,#52534,#52535,
#52536,#52537,#52538,#52539,#52540,#52541,#52542,#52543,#52544,#52545,#52546,
#52547,#52548,#52549,#52550,#52551),.UNSPECIFIED.,.F.,.F.,(4,3,3,3,3,3,
3,3,3,3,3,3,3,3,4),(145.632117158668,145.90866620818,146.408353421221,146.908040634263,
147.407727847305,147.907415060346,148.407102273388,148.90678948643,149.406476699472,
149.906163912513,150.405851125555,150.905538338597,151.405225551638,151.90491276468,
151.915302465848),.UNSPECIFIED.);
#3123=B_SPLINE_CURVE_WITH_KNOTS('',3,(#52556,#52557,#52558,#52559,#52560,
#52561,#52562,#52563,#52564,#52565,#52566,#52567,#52568,#52569,#52570,#52571,
#52572,#52573,#52574,#52575,#52576,#52577,#52578,#52579,#52580,#52581,#52582,
#52583,#52584,#52585,#52586,#52587,#52588,#52589,#52590,#52591,#52592,#52593,
#52594,#52595,#52596,#52597,#52598),.UNSPECIFIED.,.F.,.F.,(4,3,3,3,3,3,
3,3,3,3,3,3,3,3,4),(-161.172174428328,-160.899282599431,-160.399595386389,
-159.899908173348,-159.400220960306,-158.900533747264,-158.400846534222,
-157.901159321181,-157.401472108139,-156.901784895097,-156.402097682056,
-155.902410469014,-155.402723255972,-154.90303604293,-154.888989121148),
 .UNSPECIFIED.);
#3124=B_SPLINE_CURVE_WITH_KNOTS('',3,(#52599,#52600,#52601,#52602,#52603,
#52604,#52605,#52606,#52607,#52608,#52609,#52610,#52611,#52612,#52613,#52614,
#52615,#52616,#52617,#52618,#52619,#52620,#52621,#52622,#52623,#52624,#52625,
#52626,#52627,#52628,#52629,#52630,#52631,#52632,#52633,#52634,#52635,#52636,
#52637,#52638),.UNSPECIFIED.,.F.,.F.,(4,3,3,3,3,3,3,3,3,3,3,3,3,4),(151.915302465848,
152.404599977722,152.904287190763,153.403974403805,153.903661616847,154.403348829889,
154.90303604293,155.402723255972,155.902410469014,156.402097682055,156.901784895097,
157.401472108139,157.901159321181,158.198487773028),.UNSPECIFIED.);
#3125=B_SPLINE_CURVE_WITH_KNOTS('',3,(#52643,#52644,#52645,#52646,#52647,
#52648,#52649,#52650,#52651,#52652,#52653,#52654,#52655,#52656,#52657,#52658,
#52659,#52660,#52661,#52662,#52663,#52664,#52665,#52666,#52667,#52668,#52669,
#52670,#52671,#52672,#52673,#52674,#52675,#52676,#52677,#52678,#52679,#52680,
#52681,#52682,#52683,#52684,#52685),.UNSPECIFIED.,.F.,.F.,(4,3,3,3,3,3,
3,3,3,3,3,3,3,3,4),(-167.455359735508,-167.395216368973,-166.895529155931,
-166.39584194289,-165.896154729848,-165.396467516806,-164.896780303765,
-164.397093090723,-163.897405877681,-163.397718664639,-162.898031451598,
-162.398344238556,-161.898657025514,-161.398969812473,-161.172174428328),
 .UNSPECIFIED.);
#3126=B_SPLINE_CURVE_WITH_KNOTS('',3,(#52686,#52687,#52688,#52689,#52690,
#52691,#52692,#52693,#52694,#52695,#52696,#52697,#52698,#52699,#52700,#52701,
#52702,#52703,#52704,#52705,#52706,#52707,#52708,#52709,#52710,#52711,#52712,
#52713,#52714,#52715,#52716,#52717,#52718,#52719,#52720,#52721,#52722,#52723,
#52724,#52725,#52726,#52727,#52728),.UNSPECIFIED.,.F.,.F.,(4,3,3,3,3,3,
3,3,3,3,3,3,3,3,4),(158.198487773028,158.400846534222,158.900533747264,
159.400220960306,159.899908173347,160.399595386389,160.899282599431,161.398969812473,
161.898657025514,162.398344238556,162.898031451598,163.397718664639,163.897405877681,
164.397093090723,164.481673080207),.UNSPECIFIED.);
#3127=B_SPLINE_CURVE_WITH_KNOTS('',3,(#52733,#52734,#52735,#52736,#52737,
#52738,#52739,#52740,#52741,#52742,#52743,#52744,#52745,#52746,#52747,#52748,
#52749,#52750,#52751,#52752,#52753,#52754,#52755,#52756,#52757,#52758,#52759,
#52760,#52761,#52762,#52763,#52764,#52765,#52766,#52767,#52768,#52769,#52770,
#52771,#52772),.UNSPECIFIED.,.F.,.F.,(4,3,3,3,3,3,3,3,3,3,3,3,3,4),(-173.738545042687,
-173.391462925474,-172.891775712432,-172.39208849939,-171.892401286349,
-171.392714073307,-170.893026860265,-170.393339647223,-169.893652434182,
-169.39396522114,-168.894278008098,-168.394590795057,-167.894903582015,
-167.455359735508),.UNSPECIFIED.);
#3128=B_SPLINE_CURVE_WITH_KNOTS('',3,(#52773,#52774,#52775,#52776,#52777,
#52778,#52779,#52780,#52781,#52782,#52783,#52784,#52785,#52786,#52787,#52788,
#52789,#52790,#52791,#52792,#52793,#52794,#52795,#52796,#52797,#52798,#52799,
#52800,#52801,#52802,#52803,#52804,#52805,#52806,#52807,#52808,#52809,#52810,
#52811,#52812),.UNSPECIFIED.,.F.,.F.,(4,3,3,3,3,3,3,3,3,3,3,3,3,4),(164.481673080207,
164.896780303765,165.396467516806,165.896154729848,166.39584194289,166.895529155931,
167.395216368973,167.894903582015,168.394590795057,168.894278008098,169.39396522114,
169.893652434182,170.393339647223,170.764858387387),.UNSPECIFIED.);
#3129=B_SPLINE_CURVE_WITH_KNOTS('',3,(#52817,#52818,#52819,#52820,#52821,
#52822,#52823,#52824,#52825,#52826,#52827,#52828,#52829,#52830,#52831,#52832,
#52833,#52834,#52835,#52836,#52837,#52838,#52839,#52840,#52841,#52842,#52843,
#52844,#52845,#52846,#52847,#52848,#52849,#52850,#52851,#52852,#52853,#52854,
#52855,#52856,#52857,#52858,#52859),.UNSPECIFIED.,.F.,.F.,(4,3,3,3,3,3,
3,3,3,3,3,3,3,3,4),(-180.021730349867,-179.887396695016,-179.387709481974,
-178.888022268933,-178.388335055891,-177.888647842849,-177.388960629807,
-176.889273416766,-176.389586203724,-175.889898990682,-175.390211777641,
-174.890524564599,-174.390837351557,-173.891150138515,-173.738545042687),
 .UNSPECIFIED.);
#3130=B_SPLINE_CURVE_WITH_KNOTS('',3,(#52860,#52861,#52862,#52863,#52864,
#52865,#52866,#52867,#52868,#52869,#52870,#52871,#52872,#52873,#52874,#52875,
#52876,#52877,#52878,#52879,#52880,#52881,#52882,#52883,#52884,#52885,#52886,
#52887,#52888,#52889,#52890,#52891,#52892,#52893,#52894,#52895,#52896,#52897,
#52898,#52899,#52900,#52901,#52902),.UNSPECIFIED.,.F.,.F.,(4,3,3,3,3,3,
3,3,3,3,3,3,3,3,4),(170.764858387387,170.893026860265,171.392714073307,
171.892401286349,172.39208849939,172.891775712432,173.391462925474,173.891150138515,
174.390837351557,174.890524564599,175.390211777641,175.889898990682,176.389586203724,
176.889273416766,177.048043694566),.UNSPECIFIED.);
#3131=B_SPLINE_CURVE_WITH_KNOTS('',3,(#52907,#52908,#52909,#52910,#52911,
#52912,#52913,#52914,#52915,#52916,#52917,#52918,#52919,#52920,#52921,#52922,
#52923,#52924,#52925,#52926,#52927,#52928,#52929,#52930,#52931,#52932,#52933,
#52934,#52935,#52936,#52937,#52938,#52939,#52940,#52941,#52942,#52943,#52944,
#52945,#52946),.UNSPECIFIED.,.F.,.F.,(4,3,3,3,3,3,3,3,3,3,3,3,3,4),(-186.304915657046,
-185.883643251516,-185.383956038475,-184.884268825433,-184.384581612391,
-183.88489439935,-183.385207186308,-182.885519973266,-182.385832760224,
-181.886145547183,-181.386458334141,-180.886771121099,-180.387083908058,
-180.021730349867),.UNSPECIFIED.);
#3132=B_SPLINE_CURVE_WITH_KNOTS('',3,(#52947,#52948,#52949,#52950,#52951,
#52952,#52953,#52954,#52955,#52956,#52957,#52958,#52959,#52960,#52961,#52962,
#52963,#52964,#52965,#52966,#52967,#52968,#52969,#52970,#52971,#52972,#52973,
#52974,#52975,#52976,#52977,#52978,#52979,#52980,#52981,#52982,#52983,#52984,
#52985,#52986),.UNSPECIFIED.,.F.,.F.,(4,3,3,3,3,3,3,3,3,3,3,3,3,4),(177.048043694566,
177.388960629807,177.888647842849,178.388335055891,178.888022268932,179.387709481974,
179.887396695016,180.387083908058,180.886771121099,181.386458334141,181.886145547183,
182.385832760225,182.885519973266,183.331229001746),.UNSPECIFIED.);
#3133=B_SPLINE_CURVE_WITH_KNOTS('',3,(#52991,#52992,#52993,#52994,#52995,
#52996,#52997,#52998,#52999,#53000,#53001,#53002,#53003,#53004,#53005,#53006,
#53007,#53008,#53009,#53010,#53011,#53012,#53013,#53014,#53015,#53016,#53017,
#53018,#53019,#53020,#53021,#53022,#53023,#53024,#53025,#53026,#53027,#53028,
#53029,#53030,#53031,#53032,#53033),.UNSPECIFIED.,.F.,.F.,(4,3,3,3,3,3,
3,3,3,3,3,3,3,3,4),(-192.588100964226,-192.379577021059,-191.879889808017,
-191.380202594975,-190.880515381934,-190.380828168892,-189.88114095585,
-189.381453742808,-188.881766529767,-188.382079316725,-187.882392103683,
-187.382704890642,-186.8830176776,-186.383330464558,-186.304915657046),
 .UNSPECIFIED.);
#3134=B_SPLINE_CURVE_WITH_KNOTS('',3,(#53034,#53035,#53036,#53037,#53038,
#53039,#53040,#53041,#53042,#53043,#53044,#53045,#53046,#53047,#53048,#53049,
#53050,#53051,#53052,#53053,#53054,#53055,#53056,#53057,#53058,#53059,#53060,
#53061,#53062,#53063,#53064,#53065,#53066,#53067,#53068,#53069,#53070,#53071,
#53072,#53073,#53074,#53075,#53076),.UNSPECIFIED.,.F.,.F.,(4,3,3,3,3,3,
3,3,3,3,3,3,3,3,4),(183.331229001746,183.385207186308,183.88489439935,184.384581612391,
184.884268825433,185.383956038475,185.883643251516,186.383330464558,186.8830176776,
187.382704890642,187.882392103683,188.382079316725,188.881766529767,189.381453742808,
189.614414308925),.UNSPECIFIED.);
#3135=B_SPLINE_CURVE_WITH_KNOTS('',3,(#53081,#53082,#53083,#53084,#53085,
#53086,#53087,#53088,#53089,#53090,#53091,#53092,#53093,#53094,#53095,#53096,
#53097,#53098,#53099,#53100,#53101,#53102,#53103,#53104,#53105,#53106,#53107,
#53108,#53109,#53110,#53111,#53112,#53113,#53114,#53115,#53116,#53117,#53118,
#53119,#53120),.UNSPECIFIED.,.F.,.F.,(4,3,3,3,3,3,3,3,3,3,3,3,3,4),(-198.871286271405,
-198.375823577559,-197.876136364518,-197.376449151476,-196.876761938434,
-196.377074725392,-195.877387512351,-195.377700299309,-194.878013086267,
-194.378325873226,-193.878638660184,-193.378951447142,-192.8792642341,-192.588100964226),
 .UNSPECIFIED.);
#3136=B_SPLINE_CURVE_WITH_KNOTS('',3,(#53121,#53122,#53123,#53124,#53125,
#53126,#53127,#53128,#53129,#53130,#53131,#53132,#53133,#53134,#53135,#53136,
#53137,#53138,#53139,#53140,#53141,#53142,#53143,#53144,#53145,#53146,#53147,
#53148,#53149,#53150,#53151,#53152,#53153,#53154,#53155,#53156,#53157,#53158,
#53159,#53160,#53161,#53162,#53163),.UNSPECIFIED.,.F.,.F.,(4,3,3,3,3,3,
3,3,3,3,3,3,3,3,4),(189.614414308925,189.88114095585,190.380828168892,190.880515381934,
191.380202594975,191.879889808017,192.379577021059,192.8792642341,193.378951447142,
193.878638660184,194.378325873226,194.878013086267,195.377700299309,195.877387512351,
195.897599616105),.UNSPECIFIED.);
#3137=B_SPLINE_CURVE_WITH_KNOTS('',3,(#53168,#53169,#53170,#53171,#53172,
#53173,#53174,#53175,#53176,#53177,#53178,#53179,#53180,#53181,#53182,#53183,
#53184,#53185,#53186,#53187,#53188,#53189,#53190,#53191,#53192,#53193,#53194,
#53195,#53196,#53197,#53198,#53199,#53200,#53201,#53202,#53203,#53204,#53205,
#53206,#53207,#53208,#53209,#53210),.UNSPECIFIED.,.F.,.F.,(4,3,3,3,3,3,
3,3,3,3,3,3,3,3,4),(-205.154471578585,-204.871757347102,-204.37207013406,
-203.872382921018,-203.372695707976,-202.873008494935,-202.373321281893,
-201.873634068851,-201.373946855809,-200.874259642768,-200.374572429726,
-199.874885216684,-199.375198003643,-198.875510790601,-198.871286271405),
 .UNSPECIFIED.);
#3138=B_SPLINE_CURVE_WITH_KNOTS('',3,(#53211,#53212,#53213,#53214,#53215,
#53216,#53217,#53218,#53219,#53220,#53221,#53222,#53223,#53224,#53225,#53226,
#53227,#53228,#53229,#53230,#53231,#53232,#53233,#53234,#53235,#53236,#53237,
#53238,#53239,#53240,#53241,#53242,#53243,#53244,#53245,#53246,#53247,#53248,
#53249,#53250),.UNSPECIFIED.,.F.,.F.,(4,3,3,3,3,3,3,3,3,3,3,3,3,4),(195.897599616105,
196.377074725392,196.876761938434,197.376449151476,197.876136364518,198.375823577559,
198.875510790601,199.375198003643,199.874885216684,200.374572429726,200.874259642768,
201.373946855809,201.873634068851,202.180784923285),.UNSPECIFIED.);
#3139=B_SPLINE_CURVE_WITH_KNOTS('',3,(#53255,#53256,#53257,#53258,#53259,
#53260,#53261,#53262,#53263,#53264,#53265,#53266,#53267,#53268,#53269,#53270,
#53271,#53272,#53273,#53274,#53275,#53276,#53277,#53278,#53279,#53280,#53281,
#53282,#53283,#53284,#53285,#53286,#53287,#53288,#53289,#53290,#53291,#53292,
#53293,#53294,#53295,#53296,#53297),.UNSPECIFIED.,.F.,.F.,(4,3,3,3,3,3,
3,3,3,3,3,3,3,3,4),(-211.437656885764,-211.367691116644,-210.868003903602,
-210.36831669056,-209.868629477519,-209.368942264477,-208.869255051435,
-208.369567838393,-207.869880625352,-207.37019341231,-206.870506199268,
-206.370818986227,-205.871131773185,-205.371444560143,-205.154471578585),
 .UNSPECIFIED.);
#3140=B_SPLINE_CURVE_WITH_KNOTS('',3,(#53298,#53299,#53300,#53301,#53302,
#53303,#53304,#53305,#53306,#53307,#53308,#53309,#53310,#53311,#53312,#53313,
#53314,#53315,#53316,#53317,#53318,#53319,#53320,#53321,#53322,#53323,#53324,
#53325,#53326,#53327,#53328,#53329,#53330,#53331,#53332,#53333,#53334,#53335,
#53336,#53337,#53338,#53339,#53340),.UNSPECIFIED.,.F.,.F.,(4,3,3,3,3,3,
3,3,3,3,3,3,3,3,4),(202.180784923285,202.373321281893,202.873008494935,
203.372695707976,203.872382921018,204.37207013406,204.871757347101,205.371444560143,
205.871131773185,206.370818986227,206.870506199268,207.37019341231,207.869880625352,
208.369567838393,208.463970230464),.UNSPECIFIED.);
#3141=B_SPLINE_CURVE_WITH_KNOTS('',3,(#53345,#53346,#53347,#53348,#53349,
#53350,#53351,#53352,#53353,#53354,#53355,#53356,#53357,#53358,#53359,#53360,
#53361,#53362,#53363,#53364,#53365,#53366,#53367,#53368,#53369,#53370,#53371,
#53372,#53373,#53374,#53375,#53376,#53377,#53378,#53379,#53380,#53381,#53382,
#53383,#53384),.UNSPECIFIED.,.F.,.F.,(4,3,3,3,3,3,3,3,3,3,3,3,3,4),(-217.720842192944,
-217.363937673144,-216.864250460103,-216.364563247061,-215.864876034019,
-215.365188820977,-214.865501607936,-214.365814394894,-213.866127181852,
-213.366439968811,-212.866752755769,-212.367065542727,-211.867378329685,
-211.437656885764),.UNSPECIFIED.);
#3142=B_SPLINE_CURVE_WITH_KNOTS('',3,(#53385,#53386,#53387,#53388,#53389,
#53390,#53391,#53392,#53393,#53394,#53395,#53396,#53397,#53398,#53399,#53400,
#53401,#53402,#53403,#53404,#53405,#53406,#53407,#53408,#53409,#53410,#53411,
#53412,#53413,#53414,#53415,#53416,#53417,#53418,#53419,#53420,#53421,#53422,
#53423,#53424),.UNSPECIFIED.,.F.,.F.,(4,3,3,3,3,3,3,3,3,3,3,3,3,4),(208.463970230464,
208.869255051435,209.368942264477,209.868629477519,210.36831669056,210.868003903602,
211.367691116644,211.867378329685,212.367065542727,212.866752755769,213.366439968811,
213.866127181852,214.365814394894,214.747155537644),.UNSPECIFIED.);
#3143=B_SPLINE_CURVE_WITH_KNOTS('',3,(#53429,#53430,#53431,#53432,#53433,
#53434,#53435,#53436,#53437,#53438,#53439,#53440,#53441,#53442,#53443,#53444,
#53445,#53446,#53447,#53448,#53449,#53450,#53451,#53452,#53453,#53454,#53455,
#53456,#53457,#53458,#53459,#53460,#53461,#53462,#53463,#53464,#53465,#53466,
#53467,#53468,#53469,#53470,#53471),.UNSPECIFIED.,.F.,.F.,(4,3,3,3,3,3,
3,3,3,3,3,3,3,3,4),(-224.004027500124,-223.859871442686,-223.360184229645,
-222.860497016603,-222.360809803561,-221.86112259052,-221.361435377478,
-220.861748164436,-220.362060951395,-219.862373738353,-219.362686525311,
-218.862999312269,-218.363312099228,-217.863624886186,-217.720842192944),
 .UNSPECIFIED.);
#3144=B_SPLINE_CURVE_WITH_KNOTS('',3,(#53472,#53473,#53474,#53475,#53476,
#53477,#53478,#53479,#53480,#53481,#53482,#53483,#53484,#53485,#53486,#53487,
#53488,#53489,#53490,#53491,#53492,#53493,#53494,#53495,#53496,#53497,#53498,
#53499,#53500,#53501,#53502,#53503,#53504,#53505,#53506,#53507,#53508,#53509,
#53510,#53511,#53512,#53513,#53514),.UNSPECIFIED.,.F.,.F.,(4,3,3,3,3,3,
3,3,3,3,3,3,3,3,4),(214.747155537644,214.865501607936,215.365188820977,
215.864876034019,216.364563247061,216.864250460103,217.363937673144,217.863624886186,
218.363312099228,218.862999312269,219.362686525311,219.862373738353,220.362060951395,
220.861748164436,221.030340844823),.UNSPECIFIED.);
#3145=B_SPLINE_CURVE_WITH_KNOTS('',3,(#53523,#53524,#53525,#53526,#53527,
#53528,#53529,#53530,#53531,#53532,#53533,#53534,#53535),.UNSPECIFIED.,
 .F.,.F.,(4,3,3,3,4),(-231.854866851354,-231.355179638312,-230.85549242527,
-230.355805212229,-230.287212807303),.UNSPECIFIED.);
#3146=B_SPLINE_CURVE_WITH_KNOTS('',3,(#53539,#53540,#53541,#53542,#53543,
#53544,#53545,#53546,#53547,#53548,#53549,#53550,#53551,#53552,#53553,#53554,
#53555,#53556,#53557),.UNSPECIFIED.,.F.,.F.,(4,3,3,3,3,3,4),(227.313526152003,
227.357681933978,227.85736914702,228.357056360062,228.856743573104,229.356430786145,
229.785062662568),.UNSPECIFIED.);
#3147=B_SPLINE_CURVE_WITH_KNOTS('',3,(#53564,#53565,#53566,#53567,#53568,
#53569,#53570,#53571,#53572,#53573,#53574,#53575,#53576,#53577,#53578),
 .UNSPECIFIED.,.F.,.F.,(4,1,1,1,1,1,1,1,1,1,1,1,4),(235.619449019234,235.974980174839,
236.474667387881,236.974354600923,237.474041813964,237.973729027006,238.473416240048,
238.973103453089,239.472790666131,239.972477879173,240.472165092214,240.971852305256,
241.400484181679),.UNSPECIFIED.);
#3148=B_SPLINE_CURVE_WITH_KNOTS('',3,(#53581,#53582,#53583,#53584,#53585,
#53586,#53587,#53588,#53589,#53590,#53591,#53592,#53593),.UNSPECIFIED.,
 .F.,.F.,(4,1,1,1,1,1,1,1,1,1,4),(235.619449019234,235.66360480121,236.163292014252,
236.662979227294,237.162666440336,237.662353653377,238.162040866419,238.661728079461,
239.161415292502,239.661102505544,240.160789718586),.UNSPECIFIED.);
#3149=B_SPLINE_CURVE_WITH_KNOTS('',3,(#53598,#53599,#53600,#53601,#53602,
#53603,#53604,#53605,#53606,#53607,#53608,#53609,#53610,#53611,#53612,#53613,
#53614),.UNSPECIFIED.,.F.,.F.,(4,1,1,1,1,1,1,1,1,1,1,1,1,1,4),(229.336263712055,
229.479046405297,229.978733618339,230.47842083138,230.978108044422,231.477795257464,
231.977482470505,232.477169683547,232.976856896589,233.476544109631,233.976231322672,
234.475918535714,234.975605748756,235.475292961797,235.619449019234),
 .UNSPECIFIED.);
#3150=B_SPLINE_CURVE_WITH_KNOTS('',3,(#53615,#53616,#53617,#53618,#53619,
#53620,#53621,#53622,#53623,#53624,#53625,#53626,#53627,#53628,#53629,#53630),
 .UNSPECIFIED.,.F.,.F.,(4,1,1,1,1,1,1,1,1,1,1,1,1,4),(229.336263712055,
229.66735824471,230.167045457752,230.666732670793,231.166419883835,231.666107096877,
232.165794309918,232.66548152296,233.165168736002,233.664855949044,234.164543162085,
234.664230375127,235.163917588169,235.619449019234),.UNSPECIFIED.);
#3151=B_SPLINE_CURVE_WITH_KNOTS('',3,(#53635,#53636,#53637,#53638,#53639,
#53640,#53641,#53642,#53643,#53644,#53645,#53646,#53647,#53648,#53649,#53650),
 .UNSPECIFIED.,.F.,.F.,(4,1,1,1,1,1,1,1,1,1,1,1,1,4),(223.053078404875,
223.482799848796,223.982487061838,224.48217427488,224.981861487921,225.481548700963,
225.981235914005,226.480923127047,226.980610340088,227.48029755313,227.979984766172,
228.479671979213,228.979359192255,229.336263712055),.UNSPECIFIED.);
#3152=B_SPLINE_CURVE_WITH_KNOTS('',3,(#53651,#53652,#53653,#53654,#53655,
#53656,#53657,#53658,#53659,#53660,#53661,#53662,#53663,#53664,#53665,#53666,
#53667),.UNSPECIFIED.,.F.,.F.,(4,1,1,1,1,1,1,1,1,1,1,1,1,1,4),(223.053078404875,
223.171424475168,223.671111688209,224.170798901251,224.670486114293,225.170173327334,
225.669860540376,226.169547753418,226.66923496646,227.168922179501,227.668609392543,
228.168296605585,228.667983818626,229.167671031668,229.336263712055),
 .UNSPECIFIED.);
#3153=B_SPLINE_CURVE_WITH_KNOTS('',3,(#53672,#53673,#53674,#53675,#53676,
#53677,#53678,#53679,#53680,#53681,#53682,#53683,#53684,#53685,#53686,#53687,
#53688),.UNSPECIFIED.,.F.,.F.,(4,1,1,1,1,1,1,1,1,1,1,1,1,1,4),(216.769893097696,
216.986866079254,217.486553292296,217.986240505338,218.485927718379,218.985614931421,
219.485302144463,219.984989357504,220.484676570546,220.984363783588,221.484050996629,
221.983738209671,222.483425422713,222.983112635755,223.053078404875),
 .UNSPECIFIED.);
#3154=B_SPLINE_CURVE_WITH_KNOTS('',3,(#53689,#53690,#53691,#53692,#53693,
#53694,#53695,#53696,#53697,#53698,#53699,#53700,#53701,#53702,#53703,#53704),
 .UNSPECIFIED.,.F.,.F.,(4,1,1,1,1,1,1,1,1,1,1,1,1,4),(216.769893097696,
217.175177918667,217.674865131709,218.174552344751,218.674239557792,219.173926770834,
219.673613983876,220.173301196917,220.672988409959,221.172675623001,221.672362836043,
222.172050049084,222.671737262126,223.053078404875),.UNSPECIFIED.);
#3155=B_SPLINE_CURVE_WITH_KNOTS('',3,(#53709,#53710,#53711,#53712,#53713,
#53714,#53715,#53716,#53717,#53718,#53719,#53720,#53721,#53722,#53723,#53724,
#53725),.UNSPECIFIED.,.F.,.F.,(4,1,1,1,1,1,1,1,1,1,1,1,1,1,4),(210.486707790516,
210.490932309712,210.990619522754,211.490306735795,211.989993948837,212.489681161879,
212.98936837492,213.489055587962,213.988742801004,214.488430014046,214.988117227087,
215.487804440129,215.987491653171,216.487178866212,216.769893097696),
 .UNSPECIFIED.);
#3156=B_SPLINE_CURVE_WITH_KNOTS('',3,(#53726,#53727,#53728,#53729,#53730,
#53731,#53732,#53733,#53734,#53735,#53736,#53737,#53738,#53739,#53740,#53741,
#53742),.UNSPECIFIED.,.F.,.F.,(4,1,1,1,1,1,1,1,1,1,1,1,1,1,4),(210.486707790516,
210.679244149125,211.178931362167,211.678618575208,212.17830578825,212.677993001292,
213.177680214333,213.677367427375,214.177054640417,214.676741853459,215.1764290665,
215.676116279542,216.175803492584,216.675490705625,216.769893097696),
 .UNSPECIFIED.);
#3157=B_SPLINE_CURVE_WITH_KNOTS('',3,(#53747,#53748,#53749,#53750,#53751,
#53752,#53753,#53754,#53755,#53756,#53757,#53758,#53759,#53760,#53761,#53762),
 .UNSPECIFIED.,.F.,.F.,(4,1,1,1,1,1,1,1,1,1,1,1,1,4),(204.203522483337,
204.494685753211,204.994372966253,205.494060179295,205.993747392336,206.493434605378,
206.99312181842,207.492809031462,207.992496244503,208.492183457545,208.991870670587,
209.491557883628,209.99124509667,210.486707790516),.UNSPECIFIED.);
#3158=B_SPLINE_CURVE_WITH_KNOTS('',3,(#53763,#53764,#53765,#53766,#53767,
#53768,#53769,#53770,#53771,#53772,#53773,#53774,#53775,#53776,#53777,#53778),
 .UNSPECIFIED.,.F.,.F.,(4,1,1,1,1,1,1,1,1,1,1,1,1,4),(204.203522483337,
204.682997592624,205.182684805666,205.682372018708,206.182059231749,206.681746444791,
207.181433657833,207.681120870875,208.180808083916,208.680495296958,209.18018251,
209.679869723041,210.179556936083,210.486707790516),.UNSPECIFIED.);
#3159=B_SPLINE_CURVE_WITH_KNOTS('',3,(#53783,#53784,#53785,#53786,#53787,
#53788,#53789,#53790,#53791,#53792,#53793,#53794,#53795,#53796,#53797,#53798,
#53799),.UNSPECIFIED.,.F.,.F.,(4,1,1,1,1,1,1,1,1,1,1,1,1,1,4),(197.920337176157,
197.998751983669,198.498439196711,198.998126409752,199.497813622794,199.997500835836,
200.497188048878,200.996875261919,201.496562474961,201.996249688003,202.495936901044,
202.995624114086,203.495311327128,203.99499854017,204.203522483337),
 .UNSPECIFIED.);
#3160=B_SPLINE_CURVE_WITH_KNOTS('',3,(#53800,#53801,#53802,#53803,#53804,
#53805,#53806,#53807,#53808,#53809,#53810,#53811,#53812,#53813,#53814,#53815,
#53816),.UNSPECIFIED.,.F.,.F.,(4,1,1,1,1,1,1,1,1,1,1,1,1,1,4),(197.920337176157,
198.187063823082,198.686751036124,199.186438249166,199.686125462207,200.185812675249,
200.685499888291,201.185187101332,201.684874314374,202.184561527416,202.684248740457,
203.183935953499,203.683623166541,204.183310379583,204.203522483337),
 .UNSPECIFIED.);
#3161=B_SPLINE_CURVE_WITH_KNOTS('',3,(#53821,#53822,#53823,#53824,#53825,
#53826,#53827,#53828,#53829,#53830,#53831,#53832,#53833,#53834,#53835,#53836),
 .UNSPECIFIED.,.F.,.F.,(4,1,1,1,1,1,1,1,1,1,1,1,1,4),(191.637151868977,
192.002505427169,192.50219264021,193.001879853252,193.501567066294,194.001254279335,
194.500941492377,195.000628705419,195.500315918461,196.000003131502,196.499690344544,
196.999377557586,197.499064770627,197.920337176157),.UNSPECIFIED.);
#3162=B_SPLINE_CURVE_WITH_KNOTS('',3,(#53837,#53838,#53839,#53840,#53841,
#53842,#53843,#53844,#53845,#53846,#53847,#53848,#53849,#53850,#53851,#53852,
#53853),.UNSPECIFIED.,.F.,.F.,(4,1,1,1,1,1,1,1,1,1,1,1,1,1,4),(191.637151868977,
191.69113005354,192.190817266582,192.690504479623,193.190191692665,193.689878905707,
194.189566118748,194.68925333179,195.188940544832,195.688627757874,196.188314970915,
196.688002183957,197.187689396999,197.68737661004,197.920337176157),
 .UNSPECIFIED.);
#3163=B_SPLINE_CURVE_WITH_KNOTS('',3,(#53858,#53859,#53860,#53861,#53862,
#53863,#53864,#53865,#53866,#53867,#53868,#53869,#53870,#53871,#53872,#53873,
#53874),.UNSPECIFIED.,.F.,.F.,(4,1,1,1,1,1,1,1,1,1,1,1,1,1,4),(185.353966561798,
185.506571657626,186.006258870668,186.50594608371,187.005633296751,187.505320509793,
188.005007722835,188.504694935877,189.004382148918,189.50406936196,190.003756575002,
190.503443788043,191.003131001085,191.502818214127,191.637151868977),
 .UNSPECIFIED.);
#3164=B_SPLINE_CURVE_WITH_KNOTS('',3,(#53875,#53876,#53877,#53878,#53879,
#53880,#53881,#53882,#53883,#53884,#53885,#53886,#53887,#53888,#53889,#53890),
 .UNSPECIFIED.,.F.,.F.,(4,1,1,1,1,1,1,1,1,1,1,1,1,4),(185.353966561798,
185.694883497039,186.194570710081,186.694257923123,187.193945136164,187.693632349206,
188.193319562248,188.69300677529,189.192693988331,189.692381201373,190.192068414415,
190.691755627456,191.191442840498,191.637151868977),.UNSPECIFIED.);
#3165=B_SPLINE_CURVE_WITH_KNOTS('',3,(#53895,#53896,#53897,#53898,#53899,
#53900,#53901,#53902,#53903,#53904,#53905,#53906,#53907,#53908,#53909,#53910),
 .UNSPECIFIED.,.F.,.F.,(4,1,1,1,1,1,1,1,1,1,1,1,1,4),(179.070781254618,
179.510325101126,180.010012314167,180.509699527209,181.009386740251,181.509073953293,
182.008761166334,182.508448379376,183.008135592418,183.507822805459,184.007510018501,
184.507197231543,185.006884444585,185.353966561798),.UNSPECIFIED.);
#3166=B_SPLINE_CURVE_WITH_KNOTS('',3,(#53911,#53912,#53913,#53914,#53915,
#53916,#53917,#53918,#53919,#53920,#53921,#53922,#53923,#53924,#53925,#53926,
#53927),.UNSPECIFIED.,.F.,.F.,(4,1,1,1,1,1,1,1,1,1,1,1,1,1,4),(179.070781254618,
179.198949727497,179.698636940539,180.198324153581,180.698011366622,181.197698579664,
181.697385792706,182.197073005747,182.696760218789,183.196447431831,183.696134644872,
184.195821857914,184.695509070956,185.195196283998,185.353966561798),
 .UNSPECIFIED.);
#3167=B_SPLINE_CURVE_WITH_KNOTS('',3,(#53932,#53933,#53934,#53935,#53936,
#53937,#53938,#53939,#53940,#53941,#53942,#53943,#53944,#53945,#53946,#53947,
#53948),.UNSPECIFIED.,.F.,.F.,(4,1,1,1,1,1,1,1,1,1,1,1,1,1,4),(172.787595947439,
173.014391331584,173.514078544625,174.013765757667,174.513452970709,175.01314018375,
175.512827396792,176.012514609834,176.512201822876,177.011889035917,177.511576248959,
178.011263462001,178.510950675042,179.010637888084,179.070781254618),
 .UNSPECIFIED.);
#3168=B_SPLINE_CURVE_WITH_KNOTS('',3,(#53949,#53950,#53951,#53952,#53953,
#53954,#53955,#53956,#53957,#53958,#53959,#53960,#53961,#53962,#53963,#53964),
 .UNSPECIFIED.,.F.,.F.,(4,1,1,1,1,1,1,1,1,1,1,1,1,4),(172.787595947439,
173.202703170997,173.702390384038,174.20207759708,174.701764810122,175.201452023163,
175.701139236205,176.200826449247,176.700513662289,177.20020087533,177.699888088372,
178.199575301414,178.699262514455,179.070781254618),.UNSPECIFIED.);
#3169=B_SPLINE_CURVE_WITH_KNOTS('',3,(#53969,#53970,#53971,#53972,#53973,
#53974,#53975,#53976,#53977,#53978,#53979,#53980,#53981,#53982,#53983,#53984,
#53985),.UNSPECIFIED.,.F.,.F.,(4,1,1,1,1,1,1,1,1,1,1,1,1,1,4),(166.504410640259,
166.518457562041,167.018144775083,167.517831988125,168.017519201166,168.517206414208,
169.01689362725,169.516580840292,170.016268053333,170.515955266375,171.015642479417,
171.515329692458,172.0150169055,172.514704118542,172.787595947439),
 .UNSPECIFIED.);
#3170=B_SPLINE_CURVE_WITH_KNOTS('',3,(#53986,#53987,#53988,#53989,#53990,
#53991,#53992,#53993,#53994,#53995,#53996,#53997,#53998,#53999,#54000,#54001,
#54002),.UNSPECIFIED.,.F.,.F.,(4,1,1,1,1,1,1,1,1,1,1,1,1,1,4),(166.504410640259,
166.706769401454,167.206456614496,167.706143827538,168.205831040579,168.705518253621,
169.205205466663,169.704892679705,170.204579892746,170.704267105788,171.20395431883,
171.703641531871,172.203328744913,172.703015957955,172.787595947439),
 .UNSPECIFIED.);
#3171=B_SPLINE_CURVE_WITH_KNOTS('',3,(#54007,#54008,#54009,#54010,#54011,
#54012,#54013,#54014,#54015,#54016,#54017,#54018,#54019,#54020,#54021,#54022),
 .UNSPECIFIED.,.F.,.F.,(4,1,1,1,1,1,1,1,1,1,1,1,1,4),(160.22122533308,160.522211005541,
161.021898218582,161.521585431624,162.021272644666,162.520959857708,163.020647070749,
163.520334283791,164.020021496833,164.519708709874,165.019395922916,165.519083135958,
166.018770349,166.504410640259),.UNSPECIFIED.);
#3172=B_SPLINE_CURVE_WITH_KNOTS('',3,(#54023,#54024,#54025,#54026,#54027,
#54028,#54029,#54030,#54031,#54032,#54033,#54034,#54035,#54036,#54037,#54038),
 .UNSPECIFIED.,.F.,.F.,(4,1,1,1,1,1,1,1,1,1,1,1,1,4),(160.22122533308,160.710522844954,
161.210210057995,161.709897271037,162.209584484079,162.709271697121,163.208958910162,
163.708646123204,164.208333336246,164.708020549287,165.207707762329,165.707394975371,
166.207082188413,166.504410640259),.UNSPECIFIED.);
#3173=B_SPLINE_CURVE_WITH_KNOTS('',3,(#54043,#54044,#54045,#54046,#54047,
#54048,#54049,#54050,#54051,#54052,#54053,#54054,#54055,#54056,#54057,#54058,
#54059),.UNSPECIFIED.,.F.,.F.,(4,1,1,1,1,1,1,1,1,1,1,1,1,1,4),(153.9380400259,
154.026277235998,154.52596444904,155.025651662082,155.525338875124,156.025026088165,
156.524713301207,157.024400514249,157.52408772729,158.023774940332,158.523462153374,
159.023149366416,159.522836579457,160.022523792499,160.22122533308),
 .UNSPECIFIED.);
#3174=B_SPLINE_CURVE_WITH_KNOTS('',3,(#54060,#54061,#54062,#54063,#54064,
#54065,#54066,#54067,#54068,#54069,#54070,#54071,#54072,#54073,#54074,#54075,
#54076),.UNSPECIFIED.,.F.,.F.,(4,1,1,1,1,1,1,1,1,1,1,1,1,1,4),(153.9380400259,
154.214589075412,154.714276288453,155.213963501495,155.713650714537,156.213337927578,
156.71302514062,157.212712353662,157.712399566704,158.212086779745,158.711773992787,
159.211461205829,159.71114841887,160.210835631912,160.22122533308),
 .UNSPECIFIED.);
#3175=B_SPLINE_CURVE_WITH_KNOTS('',3,(#54081,#54082,#54083,#54084,#54085,
#54086,#54087,#54088,#54089,#54090,#54091,#54092,#54093,#54094,#54095,#54096),
 .UNSPECIFIED.,.F.,.F.,(4,1,1,1,1,1,1,1,1,1,1,1,1,4),(147.654854718721,
148.030030679498,148.52971789254,149.029405105581,149.529092318623,150.028779531665,
150.528466744707,151.028153957748,151.52784117079,152.027528383832,152.527215596873,
153.026902809915,153.526590022957,153.9380400259),.UNSPECIFIED.);
#3176=B_SPLINE_CURVE_WITH_KNOTS('',3,(#54097,#54098,#54099,#54100,#54101,
#54102,#54103,#54104,#54105,#54106,#54107,#54108,#54109,#54110,#54111,#54112,
#54113),.UNSPECIFIED.,.F.,.F.,(4,1,1,1,1,1,1,1,1,1,1,1,1,1,4),(147.654854718721,
147.718655305869,148.218342518911,148.718029731953,149.217716944994,149.717404158036,
150.217091371078,150.71677858412,151.216465797161,151.716153010203,152.215840223245,
152.715527436286,153.215214649328,153.71490186237,153.9380400259),
 .UNSPECIFIED.);
#3177=B_SPLINE_CURVE_WITH_KNOTS('',3,(#54118,#54119,#54120,#54121,#54122,
#54123,#54124,#54125,#54126,#54127,#54128,#54129,#54130,#54131,#54132,#54133,
#54134),.UNSPECIFIED.,.F.,.F.,(4,1,1,1,1,1,1,1,1,1,1,1,1,1,4),(141.371669411541,
141.534096909956,142.033784122997,142.533471336039,143.033158549081,143.532845762123,
144.032532975164,144.532220188206,145.031907401248,145.531594614289,146.031281827331,
146.530969040373,147.030656253415,147.530343466456,147.654854718721),
 .UNSPECIFIED.);
#3178=B_SPLINE_CURVE_WITH_KNOTS('',3,(#54135,#54136,#54137,#54138,#54139,
#54140,#54141,#54142,#54143,#54144,#54145,#54146,#54147,#54148,#54149,#54150),
 .UNSPECIFIED.,.F.,.F.,(4,1,1,1,1,1,1,1,1,1,1,1,1,4),(141.371669411541,
141.722408749369,142.22209596241,142.721783175452,143.221470388494,143.721157601536,
144.220844814577,144.720532027619,145.220219240661,145.719906453702,146.219593666744,
146.719280879786,147.218968092828,147.654854718721),.UNSPECIFIED.);
#3179=B_SPLINE_CURVE_WITH_KNOTS('',3,(#54155,#54156,#54157,#54158,#54159,
#54160,#54161,#54162,#54163,#54164,#54165,#54166,#54167,#54168,#54169,#54170),
 .UNSPECIFIED.,.F.,.F.,(4,1,1,1,1,1,1,1,1,1,1,1,1,4),(135.088484104361,
135.537850353455,136.037537566497,136.537224779539,137.03691199258,137.536599205622,
138.036286418664,138.535973631705,139.035660844747,139.535348057789,140.035035270831,
140.534722483872,141.034409696914,141.371669411541),.UNSPECIFIED.);
#3180=B_SPLINE_CURVE_WITH_KNOTS('',3,(#54171,#54172,#54173,#54174,#54175,
#54176,#54177,#54178,#54179,#54180,#54181,#54182,#54183,#54184,#54185,#54186,
#54187),.UNSPECIFIED.,.F.,.F.,(4,1,1,1,1,1,1,1,1,1,1,1,1,1,4),(135.088484104361,
135.226474979827,135.726162192868,136.22584940591,136.725536618952,137.225223831993,
137.724911045035,138.224598258077,138.724285471118,139.22397268416,139.723659897202,
140.223347110244,140.723034323285,141.222721536327,141.371669411541),
 .UNSPECIFIED.);
#3181=B_SPLINE_CURVE_WITH_KNOTS('',3,(#54192,#54193,#54194,#54195,#54196,
#54197,#54198,#54199,#54200,#54201,#54202,#54203,#54204,#54205,#54206,#54207,
#54208),.UNSPECIFIED.,.F.,.F.,(4,1,1,1,1,1,1,1,1,1,1,1,1,1,4),(128.805298797182,
129.041916583913,129.541603796955,130.041291009996,130.540978223038,131.04066543608,
131.540352649122,132.040039862163,132.539727075205,133.039414288247,133.539101501288,
134.03878871433,134.538475927372,135.038163140414,135.088484104361),
 .UNSPECIFIED.);
#3182=B_SPLINE_CURVE_WITH_KNOTS('',3,(#54209,#54210,#54211,#54212,#54213,
#54214,#54215,#54216,#54217,#54218,#54219,#54220,#54221,#54222,#54223,#54224),
 .UNSPECIFIED.,.F.,.F.,(4,1,1,1,1,1,1,1,1,1,1,1,1,4),(128.805298797182,
129.230228423326,129.729915636368,130.229602849409,130.729290062451,131.228977275493,
131.728664488535,132.228351701576,132.728038914618,133.22772612766,133.727413340701,
134.227100553743,134.726787766785,135.088484104361),.UNSPECIFIED.);
#3183=B_SPLINE_CURVE_WITH_KNOTS('',3,(#54229,#54230,#54231,#54232,#54233,
#54234,#54235,#54236,#54237,#54238,#54239,#54240,#54241,#54242,#54243,#54244,
#54245),.UNSPECIFIED.,.F.,.F.,(4,1,1,1,1,1,1,1,1,1,1,1,1,1,4),(122.522113490002,
122.545982814371,123.045670027412,123.545357240454,124.045044453496,124.544731666538,
125.044418879579,125.544106092621,126.043793305663,126.543480518704,127.043167731746,
127.542854944788,128.04254215783,128.542229370871,128.805298797182),
 .UNSPECIFIED.);
#3184=B_SPLINE_CURVE_WITH_KNOTS('',3,(#54246,#54247,#54248,#54249,#54250,
#54251,#54252,#54253,#54254,#54255,#54256,#54257,#54258,#54259,#54260,#54261,
#54262),.UNSPECIFIED.,.F.,.F.,(4,1,1,1,1,1,1,1,1,1,1,1,1,1,4),(122.522113490002,
122.734294653784,123.233981866825,123.733669079867,124.233356292909,124.733043505951,
125.232730718992,125.732417932034,126.232105145076,126.731792358117,127.231479571159,
127.731166784201,128.230853997243,128.730541210284,128.805298797182),
 .UNSPECIFIED.);
#3185=B_SPLINE_CURVE_WITH_KNOTS('',3,(#54267,#54268,#54269,#54270,#54271,
#54272,#54273,#54274,#54275,#54276,#54277,#54278,#54279,#54280,#54281,#54282),
 .UNSPECIFIED.,.F.,.F.,(4,1,1,1,1,1,1,1,1,1,1,1,1,4),(116.238928182823,
116.54973625787,117.049423470912,117.549110683954,118.048797896995,118.548485110037,
119.048172323079,119.54785953612,120.047546749162,120.547233962204,121.046921175246,
121.546608388287,122.046295601329,122.522113490002),.UNSPECIFIED.);
#3186=B_SPLINE_CURVE_WITH_KNOTS('',3,(#54283,#54284,#54285,#54286,#54287,
#54288,#54289,#54290,#54291,#54292,#54293,#54294,#54295,#54296,#54297,#54298),
 .UNSPECIFIED.,.F.,.F.,(4,1,1,1,1,1,1,1,1,1,1,1,1,4),(116.238928182823,
116.738048097283,117.237735310325,117.737422523367,118.237109736408,118.73679694945,
119.236484162492,119.736171375533,120.235858588575,120.735545801617,121.235233014659,
121.7349202277,122.234607440742,122.522113490002),.UNSPECIFIED.);
#3187=B_SPLINE_CURVE_WITH_KNOTS('',3,(#54303,#54304,#54305,#54306,#54307,
#54308,#54309,#54310,#54311,#54312,#54313,#54314,#54315,#54316,#54317,#54318,
#54319),.UNSPECIFIED.,.F.,.F.,(4,1,1,1,1,1,1,1,1,1,1,1,1,1,4),(109.955742875643,
110.053802488328,110.55348970137,111.053176914411,111.552864127453,112.052551340495,
112.552238553537,113.051925766578,113.55161297962,114.051300192662,114.550987405703,
115.050674618745,115.550361831787,116.050049044828,116.238928182823),
 .UNSPECIFIED.);
#3188=B_SPLINE_CURVE_WITH_KNOTS('',3,(#54320,#54321,#54322,#54323,#54324,
#54325,#54326,#54327,#54328,#54329,#54330,#54331,#54332,#54333,#54334,#54335,
#54336),.UNSPECIFIED.,.F.,.F.,(4,1,1,1,1,1,1,1,1,1,1,1,1,1,4),(109.955742875643,
110.242114327741,110.741801540783,111.241488753824,111.741175966866,112.240863179908,
112.74055039295,113.240237605991,113.739924819033,114.239612032075,114.739299245116,
115.238986458158,115.7386736712,116.238360884242,116.238928182823),
 .UNSPECIFIED.);
#3189=B_SPLINE_CURVE_WITH_KNOTS('',3,(#54341,#54342,#54343,#54344,#54345,
#54346,#54347,#54348,#54349,#54350,#54351,#54352,#54353,#54354,#54355,#54356),
 .UNSPECIFIED.,.F.,.F.,(4,1,1,1,1,1,1,1,1,1,1,1,1,4),(103.672557568463,
104.057555931827,104.557243144869,105.056930357911,105.556617570953,106.056304783994,
106.555991997036,107.055679210078,107.555366423119,108.055053636161,108.554740849203,
109.054428062245,109.554115275286,109.955742875643),.UNSPECIFIED.);
#3190=B_SPLINE_CURVE_WITH_KNOTS('',3,(#54357,#54358,#54359,#54360,#54361,
#54362,#54363,#54364,#54365,#54366,#54367,#54368,#54369,#54370,#54371,#54372,
#54373),.UNSPECIFIED.,.F.,.F.,(4,1,1,1,1,1,1,1,1,1,1,1,1,1,4),(103.672557568464,
103.746180558199,104.24586777124,104.745554984282,105.245242197324,105.744929410366,
106.244616623407,106.744303836449,107.243991049491,107.743678262532,108.243365475574,
108.743052688616,109.242739901658,109.742427114699,109.955742875643),
 .UNSPECIFIED.);
#3191=B_SPLINE_CURVE_WITH_KNOTS('',3,(#54378,#54379,#54380,#54381,#54382,
#54383,#54384,#54385,#54386,#54387,#54388,#54389,#54390,#54391,#54392,#54393,
#54394),.UNSPECIFIED.,.F.,.F.,(4,1,1,1,1,1,1,1,1,1,1,1,1,1,4),(97.3893722612838,
97.5616221622852,98.0613093753269,98.5609965883686,99.0606838014103,99.560371014452,
100.060058227494,100.559745440535,101.059432653577,101.559119866619,102.058807079661,
102.558494292702,103.058181505744,103.557868718786,103.672557568463),
 .UNSPECIFIED.);
#3192=B_SPLINE_CURVE_WITH_KNOTS('',3,(#54395,#54396,#54397,#54398,#54399,
#54400,#54401,#54402,#54403,#54404,#54405,#54406,#54407,#54408,#54409,#54410),
 .UNSPECIFIED.,.F.,.F.,(4,1,1,1,1,1,1,1,1,1,1,1,1,4),(97.3893722612839,
97.7499340016982,98.2496212147399,98.7493084277816,99.2489956408234,99.7486828538651,
100.248370066907,100.748057279948,101.24774449299,101.747431706032,102.247118919074,
102.746806132115,103.246493345157,103.672557568464),.UNSPECIFIED.);
#3193=B_SPLINE_CURVE_WITH_KNOTS('',3,(#54415,#54416,#54417,#54418,#54419,
#54420,#54421,#54422,#54423,#54424,#54425,#54426,#54427,#54428,#54429,#54430),
 .UNSPECIFIED.,.F.,.F.,(4,1,1,1,1,1,1,1,1,1,1,1,1,4),(91.1061869541043,
91.5653756057847,92.0650628188264,92.5647500318681,93.0644372449098,93.5641244579515,
94.0638116709932,94.5634988840349,95.0631860970766,95.5628733101183,96.06256052316,
96.5622477362018,97.0619349492435,97.3893722612838),.UNSPECIFIED.);
#3194=B_SPLINE_CURVE_WITH_KNOTS('',3,(#54431,#54432,#54433,#54434,#54435,
#54436,#54437,#54438,#54439,#54440,#54441,#54442,#54443,#54444,#54445,#54446,
#54447),.UNSPECIFIED.,.F.,.F.,(4,1,1,1,1,1,1,1,1,1,1,1,1,1,4),(91.1061869541043,
91.254000232156,91.7536874451977,92.2533746582394,92.7530618712811,93.2527490843228,
93.7524362973645,94.2521235104062,94.7518107234479,95.2514979364897,95.7511851495314,
96.2508723625731,96.7505595756148,97.2502467886565,97.3893722612839),
 .UNSPECIFIED.);
#3195=B_SPLINE_CURVE_WITH_KNOTS('',3,(#54452,#54453,#54454,#54455,#54456,
#54457,#54458,#54459,#54460,#54461,#54462,#54463,#54464,#54465,#54466,#54467,
#54468),.UNSPECIFIED.,.F.,.F.,(4,1,1,1,1,1,1,1,1,1,1,1,1,1,4),(84.8230016469247,
85.0694418362424,85.5691290492841,86.0688162623258,86.5685034753675,87.0681906884093,
87.567877901451,88.0675651144927,88.5672523275344,89.0669395405761,89.5666267536178,
90.0663139666595,90.5660011797012,91.0656883927429,91.1061869541043),
 .UNSPECIFIED.);
#3196=B_SPLINE_CURVE_WITH_KNOTS('',3,(#54469,#54470,#54471,#54472,#54473,
#54474,#54475,#54476,#54477,#54478,#54479,#54480,#54481,#54482,#54483,#54484),
 .UNSPECIFIED.,.F.,.F.,(4,1,1,1,1,1,1,1,1,1,1,1,1,4),(84.8230016469247,
85.2577536756554,85.7574408886971,86.2571281017389,86.7568153147806,87.2565025278223,
87.756189740864,88.2558769539057,88.7555641669474,89.2552513799891,89.7549385930308,
90.2546258060726,90.7543130191143,91.1061869541043),.UNSPECIFIED.);
#3197=B_SPLINE_CURVE_WITH_KNOTS('',3,(#54489,#54490,#54491,#54492,#54493,
#54494,#54495,#54496,#54497,#54498,#54499,#54500,#54501,#54502,#54503,#54504,
#54505),.UNSPECIFIED.,.F.,.F.,(4,1,1,1,1,1,1,1,1,1,1,1,1,1,4),(78.5398163397451,
78.5735080667002,79.0731952797419,79.5728824927836,80.0725697058253,80.572256918867,
81.0719441319087,81.5716313449504,82.0713185579921,82.5710057710339,83.0706929840756,
83.5703801971173,84.070067410159,84.5697546232007,84.8230016469247),
 .UNSPECIFIED.);
#3198=B_SPLINE_CURVE_WITH_KNOTS('',3,(#54506,#54507,#54508,#54509,#54510,
#54511,#54512,#54513,#54514,#54515,#54516,#54517,#54518,#54519,#54520,#54521,
#54522),.UNSPECIFIED.,.F.,.F.,(4,1,1,1,1,1,1,1,1,1,1,1,1,1,4),(78.5398163397451,
78.7618199061132,79.2615071191549,79.7611943321966,80.2608815452383,80.76056875828,
81.2602559713218,81.7599431843635,82.2596303974052,82.7593176104469,83.2590048234886,
83.7586920365303,84.258379249572,84.7580664626137,84.8230016469247),
 .UNSPECIFIED.);
#3199=B_SPLINE_CURVE_WITH_KNOTS('',3,(#54527,#54528,#54529,#54530,#54531,
#54532,#54533,#54534,#54535,#54536,#54537,#54538,#54539,#54540,#54541,#54542),
 .UNSPECIFIED.,.F.,.F.,(4,1,1,1,1,1,1,1,1,1,1,1,1,4),(72.2566310325655,
72.5772615101996,73.0769487232413,73.5766359362831,74.0763231493248,74.5760103623665,
75.0756975754082,75.5753847884499,76.0750720014916,76.5747592145333,77.074446427575,
77.5741336406168,78.0738208536585,78.5398163397451),.UNSPECIFIED.);
#3200=B_SPLINE_CURVE_WITH_KNOTS('',3,(#54543,#54544,#54545,#54546,#54547,
#54548,#54549,#54550,#54551,#54552,#54553,#54554,#54555,#54556,#54557,#54558,
#54559),.UNSPECIFIED.,.F.,.F.,(4,1,1,1,1,1,1,1,1,1,1,1,1,1,4),(72.2566310325655,
72.265886136571,72.7655733496127,73.2652605626544,73.7649477756961,74.2646349887378,
74.7643222017795,75.2640094148212,75.7636966278629,76.2633838409046,76.7630710539463,
77.2627582669881,77.7624454800298,78.2621326930715,78.5398163397451),
 .UNSPECIFIED.);
#3201=B_SPLINE_CURVE_WITH_KNOTS('',3,(#54564,#54565,#54566,#54567,#54568,
#54569,#54570,#54571,#54572,#54573,#54574,#54575,#54576,#54577,#54578,#54579,
#54580),.UNSPECIFIED.,.F.,.F.,(4,1,1,1,1,1,1,1,1,1,1,1,1,1,4),(65.9734457253859,
66.0813277406574,66.5810149536991,67.0807021667408,67.5803893797825,68.0800765928242,
68.579763805866,69.0794510189077,69.5791382319494,70.0788254449911,70.5785126580328,
71.0781998710745,71.5778870841162,72.0775742971579,72.2566310325655),
 .UNSPECIFIED.);
#3202=B_SPLINE_CURVE_WITH_KNOTS('',3,(#54581,#54582,#54583,#54584,#54585,
#54586,#54587,#54588,#54589,#54590,#54591,#54592,#54593,#54594,#54595,#54596),
 .UNSPECIFIED.,.F.,.F.,(4,1,1,1,1,1,1,1,1,1,1,1,1,4),(65.9734457253859,
66.2696395800704,66.7693267931121,67.2690140061538,67.7687012191955,68.2683884322373,
68.768075645279,69.2677628583207,69.7674500713624,70.2671372844041,70.7668244974458,
71.2665117104875,71.7661989235292,72.2566310325655),.UNSPECIFIED.);
#3203=B_SPLINE_CURVE_WITH_KNOTS('',3,(#54601,#54602,#54603,#54604,#54605,
#54606,#54607,#54608,#54609,#54610,#54611,#54612,#54613,#54614,#54615,#54616),
 .UNSPECIFIED.,.F.,.F.,(4,1,1,1,1,1,1,1,1,1,1,1,1,4),(59.6902604182063,
60.0850811841569,60.5847683971986,61.0844556102403,61.584142823282,62.0838300363237,
62.5835172493654,63.0832044624071,63.5828916754488,64.0825788884906,64.5822661015323,
65.081953314574,65.5816405276157,65.9734457253859),.UNSPECIFIED.);
#3204=B_SPLINE_CURVE_WITH_KNOTS('',3,(#54617,#54618,#54619,#54620,#54621,
#54622,#54623,#54624,#54625,#54626,#54627,#54628,#54629,#54630,#54631,#54632,
#54633),.UNSPECIFIED.,.F.,.F.,(4,1,1,1,1,1,1,1,1,1,1,1,1,1,4),(59.6902604182063,
59.7737058105282,60.2733930235699,60.7730802366116,61.2727674496533,61.772454662695,
62.2721418757367,62.7718290887784,63.2715163018202,63.7712035148619,64.2708907279036,
64.7705779409453,65.270265153987,65.7699523670287,65.9734457253859),
 .UNSPECIFIED.);
#3205=B_SPLINE_CURVE_WITH_KNOTS('',3,(#54638,#54639,#54640,#54641,#54642,
#54643,#54644,#54645,#54646,#54647,#54648,#54649,#54650,#54651,#54652,#54653,
#54654),.UNSPECIFIED.,.F.,.F.,(4,1,1,1,1,1,1,1,1,1,1,1,1,1,4),(53.4070751110267,
53.5891474146146,54.0888346276563,54.588521840698,55.0882090537398,55.5878962667815,
56.0875834798232,56.5872706928649,57.0869579059066,57.5866451189483,58.08633233199,
58.5860195450317,59.0857067580734,59.5853939711152,59.6902604182063),
 .UNSPECIFIED.);
#3206=B_SPLINE_CURVE_WITH_KNOTS('',3,(#54655,#54656,#54657,#54658,#54659,
#54660,#54661,#54662,#54663,#54664,#54665,#54666,#54667,#54668,#54669,#54670),
 .UNSPECIFIED.,.F.,.F.,(4,1,1,1,1,1,1,1,1,1,1,1,1,4),(53.4070751110268,
53.7774592540276,54.2771464670694,54.7768336801111,55.2765208931528,55.7762081061945,
56.2758953192362,56.7755825322779,57.2752697453196,57.7749569583613,58.274644171403,
58.7743313844448,59.2740185974865,59.6902604182063),.UNSPECIFIED.);
#3207=B_SPLINE_CURVE_WITH_KNOTS('',3,(#54675,#54676,#54677,#54678,#54679,
#54680,#54681,#54682,#54683,#54684,#54685,#54686,#54687,#54688,#54689,#54690),
 .UNSPECIFIED.,.F.,.F.,(4,1,1,1,1,1,1,1,1,1,1,1,1,4),(47.1238898038471,
47.5929008581141,48.0925880711558,48.5922752841975,49.0919624972392,49.5916497102809,
50.0913369233227,50.5910241363644,51.0907113494061,51.5903985624478,52.0900857754895,
52.5897729885312,53.0894602015729,53.4070751110267),.UNSPECIFIED.);
#3208=B_SPLINE_CURVE_WITH_KNOTS('',3,(#54691,#54692,#54693,#54694,#54695,
#54696,#54697,#54698,#54699,#54700,#54701,#54702,#54703,#54704,#54705,#54706,
#54707),.UNSPECIFIED.,.F.,.F.,(4,1,1,1,1,1,1,1,1,1,1,1,1,1,4),(47.1238898038472,
47.2815254844854,47.7812126975271,48.2808999105688,48.7805871236105,49.2802743366523,
49.779961549694,50.2796487627357,50.7793359757774,51.2790231888191,51.7787104018608,
52.2783976149025,52.7780848279442,53.2777720409859,53.4070751110268),
 .UNSPECIFIED.);
#3209=B_SPLINE_CURVE_WITH_KNOTS('',3,(#54712,#54713,#54714,#54715,#54716,
#54717,#54718,#54719,#54720,#54721,#54722,#54723,#54724,#54725,#54726,#54727,
#54728),.UNSPECIFIED.,.F.,.F.,(4,1,1,1,1,1,1,1,1,1,1,1,1,1,4),(40.8407044966675,
41.0969670885719,41.5966543016136,42.0963415146553,42.596028727697,43.0957159407387,
43.5954031537804,44.0950903668221,44.5947775798638,45.0944647929055,45.5941520059473,
46.093839218989,46.5935264320307,47.0932136450724,47.1238898038471),
 .UNSPECIFIED.);
#3210=B_SPLINE_CURVE_WITH_KNOTS('',3,(#54729,#54730,#54731,#54732,#54733,
#54734,#54735,#54736,#54737,#54738,#54739,#54740,#54741,#54742,#54743,#54744),
 .UNSPECIFIED.,.F.,.F.,(4,1,1,1,1,1,1,1,1,1,1,1,1,4),(40.8407044966676,
41.2852789279849,41.7849661410266,42.2846533540683,42.78434056711,43.2840277801517,
43.7837149931934,44.2834022062351,44.7830894192769,45.2827766323186,45.7824638453603,
46.282151058402,46.7818382714437,47.1238898038472),.UNSPECIFIED.);
#3211=B_SPLINE_CURVE_WITH_KNOTS('',3,(#54749,#54750,#54751,#54752,#54753,
#54754,#54755,#54756,#54757,#54758,#54759,#54760,#54761,#54762,#54763,#54764,
#54765),.UNSPECIFIED.,.F.,.F.,(4,1,1,1,1,1,1,1,1,1,1,1,1,1,4),(34.5575191894879,
34.6010333190296,35.1007205320713,35.600407745113,36.1000949581547,36.5997821711965,
37.0994693842382,37.5991565972799,38.0988438103216,38.5985310233633,39.098218236405,
39.5979054494467,40.0975926624884,40.5972798755301,40.8407044966675),
 .UNSPECIFIED.);
#3212=B_SPLINE_CURVE_WITH_KNOTS('',3,(#54766,#54767,#54768,#54769,#54770,
#54771,#54772,#54773,#54774,#54775,#54776,#54777,#54778,#54779,#54780,#54781,
#54782),.UNSPECIFIED.,.F.,.F.,(4,1,1,1,1,1,1,1,1,1,1,1,1,1,4),(34.557519189488,
34.7893451584426,35.2890323714843,35.7887195845261,36.2884067975678,36.7880940106095,
37.2877812236512,37.7874684366929,38.2871556497346,38.7868428627763,39.286530075818,
39.7862172888597,40.2859045019015,40.7855917149432,40.8407044966676),
 .UNSPECIFIED.);
#3213=B_SPLINE_CURVE_WITH_KNOTS('',3,(#54787,#54788,#54789,#54790,#54791,
#54792,#54793,#54794,#54795,#54796,#54797,#54798,#54799,#54800,#54801,#54802),
 .UNSPECIFIED.,.F.,.F.,(4,1,1,1,1,1,1,1,1,1,1,1,1,4),(28.2743338823083,
28.6047867625291,29.1044739755708,29.6041611886125,30.1038484016542,30.6035356146959,
31.1032228277376,31.6029100407793,32.1025972538211,32.6022844668628,33.1019716799045,
33.6016588929462,34.1013461059879,34.5575191894879),.UNSPECIFIED.);
#3214=B_SPLINE_CURVE_WITH_KNOTS('',3,(#54803,#54804,#54805,#54806,#54807,
#54808,#54809,#54810,#54811,#54812,#54813,#54814,#54815,#54816,#54817,#54818,
#54819),.UNSPECIFIED.,.F.,.F.,(4,1,1,1,1,1,1,1,1,1,1,1,1,1,4),(28.2743338823084,
28.2934113889004,28.7930986019421,29.2927858149838,29.7924730280255,30.2921602410672,
30.7918474541089,31.2915346671507,31.7912218801924,32.2909090932341,32.7905963062758,
33.2902835193175,33.7899707323592,34.2896579454009,34.557519189488),
 .UNSPECIFIED.);
#3215=B_SPLINE_CURVE_WITH_KNOTS('',3,(#54824,#54825,#54826,#54827,#54828,
#54829,#54830,#54831,#54832,#54833,#54834,#54835,#54836,#54837,#54838,#54839,
#54840),.UNSPECIFIED.,.F.,.F.,(4,1,1,1,1,1,1,1,1,1,1,1,1,1,4),(21.9911485751287,
22.1088529929868,22.6085402060286,23.1082274190703,23.607914632112,24.1076018451537,
24.6072890581954,25.1069762712371,25.6066634842788,26.1063506973205,26.6060379103622,
27.1057251234039,27.6054123364457,28.1050995494874,28.2743338823083),
 .UNSPECIFIED.);
#3216=B_SPLINE_CURVE_WITH_KNOTS('',3,(#54841,#54842,#54843,#54844,#54845,
#54846,#54847,#54848,#54849,#54850,#54851,#54852,#54853,#54854,#54855,#54856),
 .UNSPECIFIED.,.F.,.F.,(4,1,1,1,1,1,1,1,1,1,1,1,1,4),(21.9911485751288,
22.2971648323999,22.7968520454416,23.2965392584833,23.796226471525,24.2959136845667,
24.7956008976084,25.2952881106501,25.7949753236918,26.2946625367335,26.7943497497753,
27.294036962817,27.7937241758587,28.2743338823084),.UNSPECIFIED.);
#3217=B_SPLINE_CURVE_WITH_KNOTS('',3,(#54861,#54862,#54863,#54864,#54865,
#54866,#54867,#54868,#54869,#54870,#54871,#54872,#54873,#54874,#54875,#54876),
 .UNSPECIFIED.,.F.,.F.,(4,1,1,1,1,1,1,1,1,1,1,1,1,4),(15.7079632679492,
16.1126064364863,16.612293649528,17.1119808625697,17.6116680756114,18.1113552886532,
18.6110425016949,19.1107297147366,19.6104169277783,20.11010414082,20.6097913538617,
21.1094785669034,21.6091657799451,21.9911485751287),.UNSPECIFIED.);
#3218=B_SPLINE_CURVE_WITH_KNOTS('',3,(#54877,#54878,#54879,#54880,#54881,
#54882,#54883,#54884,#54885,#54886,#54887,#54888,#54889,#54890,#54891,#54892,
#54893),.UNSPECIFIED.,.F.,.F.,(4,1,1,1,1,1,1,1,1,1,1,1,1,1,4),(15.7079632679492,
15.8012310628576,16.3009182758993,16.800605488941,17.3002927019828,17.7999799150245,
18.2996671280662,18.7993543411079,19.2990415541496,19.7987287671913,20.298415980233,
20.7981031932747,21.2977904063164,21.7974776193581,21.9911485751288),
 .UNSPECIFIED.);
#3219=B_SPLINE_CURVE_WITH_KNOTS('',3,(#54946,#54947,#54948,#54949,#54950,
#54951,#54952,#54953,#54954,#54955,#54956,#54957,#54958,#54959,#54960,#54961,
#54962,#54963,#54964,#54965,#54966,#54967,#54968,#54969,#54970,#54971,#54972,
#54973,#54974,#54975,#54976,#54977,#54978,#54979,#54980,#54981,#54982,#54983,
#54984,#54985,#54986,#54987,#54988,#54989,#54990,#54991,#54992,#54993,#54994,
#54995,#54996,#54997,#54998,#54999,#55000,#55001,#55002,#55003,#55004,#55005,
#55006,#55007,#55008,#55009,#55010,#55011,#55012,#55013,#55014,#55015,#55016,
#55017,#55018,#55019,#55020,#55021,#55022,#55023,#55024,#55025,#55026,#55027,
#55028,#55029,#55030,#55031,#55032,#55033,#55034,#55035,#55036,#55037,#55038,
#55039,#55040,#55041,#55042,#55043,#55044,#55045,#55046,#55047,#55048,#55049,
#55050,#55051,#55052,#55053,#55054,#55055,#55056,#55057),.UNSPECIFIED.,
 .F.,.F.,(4,3,3,3,3,3,3,3,3,3,3,3,3,3,3,3,3,3,3,3,3,3,3,3,3,3,3,3,3,3,3,
3,3,3,3,3,3,4),(-1.13094109509802,-1.09555301847653,-1.05191077246943,-1.02403062395787,
-1.00813854529478,-1.00052830557018,-0.993876160984945,-0.949033314345626,
-0.903913416286832,-0.871831333015361,-0.865263807587487,-0.858234145025541,
-0.839749249743891,-0.794775856894288,-0.749099847114423,-0.702998994975979,
-0.67015530307118,-0.65938726757389,-0.653338187751441,-0.606207711122551,
-0.571624227356783,-0.52477896769309,-0.4775450680471,-0.45430610006491,
-0.447310014249259,-0.440818772196958,-0.392835159315427,-0.342234241752502,
-0.291633324189578,-0.255179158665881,-0.239230461249263,-0.229162927859656,
-0.222808275366792,-0.174282107380972,-0.12474438340666,-0.0750152592867178,
-0.0256716031603919,0.),.UNSPECIFIED.);
#3220=B_SPLINE_CURVE_WITH_KNOTS('',3,(#55058,#55059,#55060,#55061,#55062,
#55063,#55064,#55065,#55066,#55067,#55068,#55069,#55070,#55071,#55072,#55073,
#55074,#55075,#55076,#55077,#55078,#55079,#55080,#55081,#55082,#55083,#55084,
#55085,#55086,#55087,#55088,#55089,#55090,#55091,#55092,#55093,#55094,#55095,
#55096,#55097,#55098,#55099,#55100,#55101,#55102,#55103,#55104,#55105,#55106,
#55107,#55108,#55109,#55110,#55111,#55112,#55113,#55114,#55115,#55116,#55117,
#55118,#55119,#55120,#55121,#55122,#55123,#55124,#55125,#55126,#55127,#55128,
#55129,#55130,#55131,#55132,#55133,#55134,#55135,#55136,#55137,#55138,#55139,
#55140,#55141,#55142,#55143,#55144,#55145,#55146,#55147,#55148,#55149,#55150,
#55151,#55152,#55153,#55154,#55155,#55156,#55157,#55158,#55159,#55160,#55161,
#55162,#55163,#55164,#55165,#55166),.UNSPECIFIED.,.F.,.F.,(4,3,3,3,3,3,
3,3,3,3,3,3,3,3,3,3,3,3,3,3,3,3,3,3,3,3,3,3,3,3,3,3,3,3,3,3,4),(-1.12653966532771,
-1.08458299748631,-1.03483149315989,-0.985279599381992,-0.975815498433229,
-0.967599728292632,-0.918737646949452,-0.870231088088996,-0.833191367947055,
-0.824932489274649,-0.81718932838954,-0.796151647805113,-0.748401850681541,
-0.700478100468338,-0.653200435706217,-0.619650854833934,-0.606444877375552,
-0.599947690904268,-0.553426660564813,-0.519002112217086,-0.472281839936397,
-0.425888913622091,-0.404346747613177,-0.397440927235775,-0.39106097225247,
-0.345595566799898,-0.299573576175339,-0.253551585550779,-0.221857637356932,
-0.205368177310387,-0.194980811358931,-0.189035396833246,-0.144860126169755,
-0.100702737474855,-0.0569688291873824,-0.0141848851110983,0.),
 .UNSPECIFIED.);
#3221=B_SPLINE_CURVE_WITH_KNOTS('',3,(#57035,#57036,#57037,#57038,#57039,
#57040,#57041,#57042,#57043,#57044,#57045,#57046,#57047,#57048,#57049,#57050,
#57051,#57052,#57053,#57054,#57055,#57056,#57057,#57058,#57059,#57060,#57061,
#57062,#57063,#57064,#57065,#57066,#57067,#57068,#57069,#57070,#57071,#57072,
#57073,#57074),.UNSPECIFIED.,.F.,.F.,(4,3,3,3,3,3,3,3,3,3,3,3,3,4),(221.030340844823,
221.361435377478,221.86112259052,222.360809803561,222.860497016603,223.360184229645,
223.859871442686,224.359558655728,224.85924586877,225.358933081812,225.858620294853,
226.358307507895,226.857994720937,227.313526152003),.UNSPECIFIED.);
#3222=B_SPLINE_CURVE_WITH_KNOTS('',3,(#57076,#57077,#57078,#57079,#57080,
#57081,#57082,#57083,#57084,#57085,#57086,#57087,#57088,#57089,#57090,#57091,
#57092,#57093,#57094,#57095,#57096,#57097,#57098,#57099,#57100,#57101,#57102,
#57103,#57104,#57105,#57106,#57107,#57108,#57109,#57110,#57111,#57112,#57113,
#57114,#57115,#57116,#57117,#57118,#57119,#57120,#57121,#57122,#57123,#57124,
#57125,#57126,#57127,#57128,#57129,#57130,#57131,#57132,#57133,#57134,#57135,
#57136,#57137,#57138,#57139,#57140,#57141,#57142,#57143,#57144,#57145,#57146,
#57147,#57148,#57149,#57150,#57151,#57152,#57153,#57154,#57155,#57156,#57157,
#57158,#57159,#57160,#57161,#57162,#57163,#57164,#57165,#57166,#57167,#57168,
#57169,#57170,#57171,#57172,#57173,#57174,#57175,#57176,#57177,#57178,#57179,
#57180,#57181),.UNSPECIFIED.,.F.,.F.,(4,3,3,3,3,3,3,3,3,3,3,3,3,3,3,3,3,
3,3,3,3,3,3,3,3,3,3,3,3,3,3,3,3,3,3,4),(0.,0.0352857241728138,0.0785968005211441,
0.122543680878482,0.164561866032942,0.181925963986356,0.191292943908678,
0.198769809597266,0.244693115546795,0.290616421496325,0.335746406070846,
0.381175755521027,0.394700494941097,0.400587470417484,0.446722411686962,
0.493312170072264,0.539988246407058,0.557729506053438,0.592565372786847,
0.602152221655606,0.609811280274756,0.656489736582357,0.704212096377392,
0.7521337137357,0.794275076828207,0.81534575837446,0.822329730595576,0.836416439920714,
0.88442476768464,0.933058731823078,0.957243848511161,0.968294021888866,
0.977747896967412,1.02724813744154,1.07696146625084,1.12653966532774),
 .UNSPECIFIED.);
#3223=B_SPLINE_CURVE_WITH_KNOTS('',3,(#57182,#57183,#57184,#57185,#57186,
#57187,#57188,#57189,#57190,#57191,#57192,#57193,#57194,#57195),
 .UNSPECIFIED.,.F.,.F.,(4,1,1,1,1,1,1,1,1,1,1,4),(10.3757270560181,10.8043589324405,
11.3040461454822,11.8037333585239,12.3034205715656,12.8031077846074,13.3027949976491,
13.8024822106908,14.3021694237325,14.8018566367742,15.3015438498159,15.7079632679492),
 .UNSPECIFIED.);
#3224=B_SPLINE_CURVE_WITH_KNOTS('',3,(#57199,#57200,#57201,#57202,#57203,
#57204,#57205,#57206,#57207,#57208,#57209,#57210),.UNSPECIFIED.,.F.,.F.,
(4,1,1,1,1,1,1,1,1,4),(11.6154215191109,12.1151087321526,12.6147959451943,
13.114483158236,13.6141703712778,14.1138575843195,14.6135447973612,15.1132320104029,
15.6129192234446,15.7079632679492),.UNSPECIFIED.);
#3225=B_SPLINE_CURVE_WITH_KNOTS('',3,(#59079,#59080,#59081,#59082,#59083,
#59084,#59085,#59086,#59087,#59088,#59089,#59090,#59091,#59092,#59093,#59094,
#59095,#59096,#59097,#59098,#59099,#59100,#59101,#59102,#59103,#59104,#59105,
#59106,#59107,#59108,#59109,#59110,#59111,#59112,#59113,#59114,#59115,#59116,
#59117,#59118,#59119,#59120,#59121,#59122,#59123,#59124,#59125,#59126,#59127,
#59128,#59129,#59130,#59131,#59132,#59133,#59134,#59135,#59136,#59137,#59138,
#59139,#59140,#59141,#59142,#59143,#59144,#59145,#59146,#59147,#59148,#59149,
#59150,#59151,#59152,#59153,#59154,#59155,#59156,#59157,#59158,#59159,#59160,
#59161,#59162,#59163,#59164,#59165,#59166,#59167,#59168,#59169,#59170,#59171,
#59172,#59173,#59174,#59175,#59176,#59177,#59178,#59179,#59180,#59181,#59182,
#59183,#59184),.UNSPECIFIED.,.F.,.F.,(4,3,3,3,3,3,3,3,3,3,3,3,3,3,3,3,3,
3,3,3,3,3,3,3,3,3,3,3,3,3,3,3,3,3,3,4),(0.,0.0421292382714313,0.091750200305321,
0.141456976711247,0.189144780929015,0.226472585797489,0.232898121965279,
0.282553157773798,0.332208193582317,0.380717833282778,0.4288180329463,0.441643201872779,
0.447579677179949,0.494878310127159,0.542047678686319,0.58849366827198,
0.610502777243903,0.643793248697581,0.654127499556154,0.660011487124506,
0.705941659246836,0.75196767154723,0.797593194966215,0.83720987191977,0.857018210396548,
0.863932831637979,0.870762041059155,0.876826548873325,0.921927000756489,
0.966986484162723,0.987480810529615,0.996684100011213,1.00397890643578,
1.04815620422644,1.09160411182441,1.13094109509786),.UNSPECIFIED.);
#3226=B_SPLINE_CURVE_WITH_KNOTS('',3,(#59185,#59186,#59187,#59188,#59189,
#59190,#59191,#59192,#59193,#59194,#59195,#59196,#59197,#59198,#59199,#59200,
#59201,#59202,#59203,#59204,#59205,#59206,#59207,#59208,#59209,#59210,#59211,
#59212,#59213,#59214,#59215,#59216,#59217,#59218,#59219,#59220,#59221,#59222,
#59223,#59224),.UNSPECIFIED.,.F.,.F.,(4,3,3,3,3,3,3,3,3,3,3,3,3,4),(-230.287212807303,
-229.856117999187,-229.356430786145,-228.856743573104,-228.357056360062,
-227.85736914702,-227.357681933978,-226.857994720937,-226.358307507895,
-225.858620294853,-225.358933081812,-224.85924586877,-224.359558655728,
-224.004027500124),.UNSPECIFIED.);
#3227=B_SPLINE_CURVE_WITH_KNOTS('',3,(#59298,#59299,#59300,#59301,#59302,
#59303,#59304,#59305,#59306,#59307),.UNSPECIFIED.,.F.,.F.,(4,3,3,4),(-4.09293042013064,
-3.99986567308015,-2.99989925481011,-2.06863817490912),.UNSPECIFIED.);
#3228=B_SPLINE_CURVE_WITH_KNOTS('',3,(#59310,#59311,#59312,#59313,#59314,
#59315,#59316),.UNSPECIFIED.,.F.,.F.,(4,3,4),(0.,0.996270937794229,1.11730040836874),
 .UNSPECIFIED.);
#3229=B_SPLINE_CURVE_WITH_KNOTS('',3,(#59321,#59322,#59323,#59324,#59325,
#59326,#59327,#59328,#59329,#59330,#59331,#59332,#59333,#59334,#59335,#59336,
#59337,#59338,#59339,#59340,#59341,#59342),.UNSPECIFIED.,.F.,.F.,(4,3,3,
3,3,3,3,4),(-10.3761157273102,-9.99966418270038,-8.99969776443034,-7.9997313461603,
-6.99976492789026,-5.99979850962022,-4.99983209135019,-4.09293042013064),
 .UNSPECIFIED.);
#3230=B_SPLINE_CURVE_WITH_KNOTS('',3,(#59343,#59344,#59345,#59346,#59347,
#59348,#59349,#59350,#59351,#59352,#59353,#59354,#59355,#59356,#59357,#59358,
#59359,#59360,#59361,#59362,#59363,#59364),.UNSPECIFIED.,.F.,.F.,(4,3,3,
3,3,3,3,4),(1.11730040836874,1.99254187558847,2.98881281338272,3.98508375117696,
4.98135468897121,5.97762562676545,6.97389656455969,7.40048571554833),
 .UNSPECIFIED.);
#3231=B_SPLINE_CURVE_WITH_KNOTS('',3,(#59369,#59370,#59371,#59372,#59373,
#59374,#59375,#59376,#59377,#59378,#59379,#59380,#59381,#59382,#59383,#59384,
#59385,#59386,#59387,#59388,#59389,#59390),.UNSPECIFIED.,.F.,.F.,(4,3,3,
3,3,3,3,4),(-16.6593010344898,-15.9994626923206,-14.9994962740506,-13.9995298557805,
-12.9995634375105,-11.9995970192405,-10.9996306009704,-10.3761157273102),
 .UNSPECIFIED.);
#3232=B_SPLINE_CURVE_WITH_KNOTS('',3,(#59391,#59392,#59393,#59394,#59395,
#59396,#59397,#59398,#59399,#59400,#59401,#59402,#59403,#59404,#59405,#59406,
#59407,#59408,#59409,#59410,#59411,#59412),.UNSPECIFIED.,.F.,.F.,(4,3,3,
3,3,3,3,4),(7.40048571554833,7.97016750235394,8.96643844014818,9.96270937794242,
10.9589803157367,11.9552512535309,12.9515221913251,13.6836710227279),
 .UNSPECIFIED.);
#3233=B_SPLINE_CURVE_WITH_KNOTS('',3,(#59417,#59418,#59419,#59420,#59421,
#59422,#59423,#59424,#59425,#59426,#59427,#59428,#59429,#59430,#59431,#59432,
#59433,#59434,#59435,#59436,#59437,#59438),.UNSPECIFIED.,.F.,.F.,(4,3,3,
3,3,3,3,4),(-22.9424863416694,-21.9992612019408,-20.9992947836708,-19.9993283654008,
-18.9993619471307,-17.9993955288607,-16.9994291105906,-16.6593010344898),
 .UNSPECIFIED.);
#3234=B_SPLINE_CURVE_WITH_KNOTS('',3,(#59439,#59440,#59441,#59442,#59443,
#59444,#59445,#59446,#59447,#59448,#59449,#59450,#59451,#59452,#59453,#59454,
#59455,#59456,#59457,#59458,#59459,#59460,#59461,#59462,#59463),
 .UNSPECIFIED.,.F.,.F.,(4,3,3,3,3,3,3,3,4),(13.6836710227279,13.9477931291194,
14.9440640669136,15.9403350047079,16.9366059425021,17.9328768802963,18.9291478180906,
19.9254187558848,19.9668563299075),.UNSPECIFIED.);
#3235=B_SPLINE_CURVE_WITH_KNOTS('',3,(#59468,#59469,#59470,#59471,#59472,
#59473,#59474,#59475,#59476,#59477,#59478,#59479,#59480,#59481,#59482,#59483,
#59484,#59485,#59486,#59487,#59488,#59489,#59490,#59491,#59492),
 .UNSPECIFIED.,.F.,.F.,(4,3,3,3,3,3,3,3,4),(-29.225671648849,-28.9990261298311,
-27.9990597115611,-26.999093293291,-25.999126875021,-24.9991604567509,-23.9991940384809,
-22.9992276202109,-22.9424863416694),.UNSPECIFIED.);
#3236=B_SPLINE_CURVE_WITH_KNOTS('',3,(#59493,#59494,#59495,#59496,#59497,
#59498,#59499,#59500,#59501,#59502,#59503,#59504,#59505,#59506,#59507,#59508,
#59509,#59510,#59511,#59512,#59513,#59514),.UNSPECIFIED.,.F.,.F.,(4,3,3,
3,3,3,3,4),(19.9668563299075,20.9216896936791,21.9179606314733,22.9142315692675,
23.9105025070618,24.906773444856,25.9030443826502,26.2500416370871),
 .UNSPECIFIED.);
#3237=B_SPLINE_CURVE_WITH_KNOTS('',3,(#59519,#59520,#59521,#59522,#59523,
#59524,#59525,#59526,#59527,#59528,#59529,#59530,#59531,#59532,#59533,#59534,
#59535,#59536,#59537,#59538,#59539,#59540),.UNSPECIFIED.,.F.,.F.,(4,3,3,
3,3,3,3,4),(-35.5088569560286,-34.9988246394513,-33.9988582211813,-32.9988918029113,
-31.9989253846412,-30.9989589663712,-29.9989925481011,-29.225671648849),
 .UNSPECIFIED.);
#3238=B_SPLINE_CURVE_WITH_KNOTS('',3,(#59541,#59542,#59543,#59544,#59545,
#59546,#59547,#59548,#59549,#59550,#59551,#59552,#59553,#59554,#59555,#59556,
#59557,#59558,#59559,#59560,#59561,#59562),.UNSPECIFIED.,.F.,.F.,(4,3,3,
3,3,3,3,4),(26.2500416370871,26.8993153204445,27.8955862582387,28.891857196033,
29.8881281338272,30.8843990716215,31.8806700094157,32.5332269442667),
 .UNSPECIFIED.);
#3239=B_SPLINE_CURVE_WITH_KNOTS('',3,(#59567,#59568,#59569,#59570,#59571,
#59572,#59573,#59574,#59575,#59576,#59577,#59578,#59579,#59580,#59581,#59582,
#59583,#59584,#59585,#59586,#59587,#59588),.UNSPECIFIED.,.F.,.F.,(4,3,3,
3,3,3,3,4),(-41.7920422632082,-40.9986231490716,-39.9986567308015,-38.9986903125315,
-37.9987238942614,-36.9987574759914,-35.9987910577214,-35.5088569560286),
 .UNSPECIFIED.);
#3240=B_SPLINE_CURVE_WITH_KNOTS('',3,(#59589,#59590,#59591,#59592,#59593,
#59594,#59595,#59596,#59597,#59598,#59599,#59600,#59601,#59602,#59603,#59604,
#59605,#59606,#59607,#59608,#59609,#59610),.UNSPECIFIED.,.F.,.F.,(4,3,3,
3,3,3,3,4),(32.5332269442667,32.87694094721,33.8732118850042,34.8694828227984,
35.8657537605927,36.8620246983869,37.8582956361812,38.8164122514463),
 .UNSPECIFIED.);
#3241=B_SPLINE_CURVE_WITH_KNOTS('',3,(#59615,#59616,#59617,#59618,#59619,
#59620,#59621,#59622,#59623,#59624,#59625,#59626,#59627,#59628,#59629,#59630,
#59631,#59632,#59633,#59634,#59635,#59636,#59637,#59638,#59639),
 .UNSPECIFIED.,.F.,.F.,(4,3,3,3,3,3,3,3,4),(-48.0752275703878,-47.9983880769618,
-46.9984216586918,-45.9984552404217,-44.9984888221517,-43.9985224038817,
-42.9985559856116,-41.9985895673416,-41.7920422632082),.UNSPECIFIED.);
#3242=B_SPLINE_CURVE_WITH_KNOTS('',3,(#59640,#59641,#59642,#59643,#59644,
#59645,#59646,#59647,#59648,#59649,#59650,#59651,#59652,#59653,#59654,#59655,
#59656,#59657,#59658,#59659,#59660,#59661,#59662,#59663,#59664),
 .UNSPECIFIED.,.F.,.F.,(4,3,3,3,3,3,3,3,4),(38.8164122514463,38.8545665739754,
39.8508375117697,40.8471084495639,41.8433793873581,42.8396503251524,43.8359212629466,
44.8321922007408,45.0995975586259),.UNSPECIFIED.);
#3243=B_SPLINE_CURVE_WITH_KNOTS('',3,(#59669,#59670,#59671,#59672,#59673,
#59674,#59675,#59676,#59677,#59678,#59679,#59680,#59681,#59682,#59683,#59684,
#59685,#59686,#59687,#59688,#59689,#59690),.UNSPECIFIED.,.F.,.F.,(4,3,3,
3,3,3,3,4),(-54.3584128775673,-53.998186586582,-52.998220168312,-51.998253750042,
-50.9982873317719,-49.9983209135019,-48.9983544952319,-48.0752275703878),
 .UNSPECIFIED.);
#3244=B_SPLINE_CURVE_WITH_KNOTS('',3,(#59691,#59692,#59693,#59694,#59695,
#59696,#59697,#59698,#59699,#59700,#59701,#59702,#59703,#59704,#59705,#59706,
#59707,#59708,#59709,#59710,#59711,#59712),.UNSPECIFIED.,.F.,.F.,(4,3,3,
3,3,3,3,4),(45.0995975586259,45.8284631385351,46.8247340763293,47.8210050141236,
48.8172759519178,49.8135468897121,50.8098178275063,51.3827828658055),
 .UNSPECIFIED.);
#3245=B_SPLINE_CURVE_WITH_KNOTS('',3,(#59717,#59718,#59719,#59720,#59721,
#59722,#59723,#59724,#59725,#59726,#59727,#59728,#59729,#59730,#59731,#59732,
#59733,#59734,#59735,#59736,#59737,#59738),.UNSPECIFIED.,.F.,.F.,(4,3,3,
3,3,3,3,4),(-60.6415981847469,-59.9979850962023,-58.9980186779322,-57.9980522596622,
-56.9980858413922,-55.9981194231221,-54.9981530048521,-54.3584128775673),
 .UNSPECIFIED.);
#3246=B_SPLINE_CURVE_WITH_KNOTS('',3,(#59739,#59740,#59741,#59742,#59743,
#59744,#59745,#59746,#59747,#59748,#59749,#59750,#59751,#59752,#59753,#59754,
#59755,#59756,#59757,#59758,#59759,#59760),.UNSPECIFIED.,.F.,.F.,(4,3,3,
3,3,3,3,4),(51.3827828658055,51.8060887653006,52.8023597030948,53.798630640889,
54.7949015786833,55.7911725164775,56.7874434542717,57.665968172985),
 .UNSPECIFIED.);
#3247=B_SPLINE_CURVE_WITH_KNOTS('',3,(#59765,#59766,#59767,#59768,#59769,
#59770,#59771,#59772,#59773,#59774,#59775,#59776,#59777,#59778,#59779,#59780,
#59781,#59782,#59783,#59784,#59785,#59786),.UNSPECIFIED.,.F.,.F.,(4,3,3,
3,3,3,3,4),(-66.9247834919265,-65.9977836058225,-64.9978171875525,-63.9978507692824,
-62.9978843510124,-61.9979179327423,-60.9979515144723,-60.6415981847469),
 .UNSPECIFIED.);
#3248=B_SPLINE_CURVE_WITH_KNOTS('',3,(#59787,#59788,#59789,#59790,#59791,
#59792,#59793,#59794,#59795,#59796,#59797,#59798,#59799,#59800,#59801,#59802,
#59803,#59804,#59805,#59806,#59807,#59808,#59809,#59810,#59811),
 .UNSPECIFIED.,.F.,.F.,(4,3,3,3,3,3,3,3,4),(57.665968172985,57.783714392066,
58.7799853298602,59.7762562676544,60.7725272054487,61.7687981432429,62.7650690810372,
63.7613400188314,63.9491534801646),.UNSPECIFIED.);
#3249=B_SPLINE_CURVE_WITH_KNOTS('',3,(#59816,#59817,#59818,#59819,#59820,
#59821,#59822,#59823,#59824,#59825,#59826,#59827,#59828,#59829,#59830,#59831,
#59832,#59833,#59834,#59835,#59836,#59837,#59838,#59839,#59840),
 .UNSPECIFIED.,.F.,.F.,(4,3,3,3,3,3,3,3,4),(-73.2079687991061,-72.9975485337127,
-71.9975821154427,-70.9976156971727,-69.9976492789027,-68.9976828606326,
-67.9977164423626,-66.9977500240925,-66.9247834919265),.UNSPECIFIED.);
#3250=B_SPLINE_CURVE_WITH_KNOTS('',3,(#59841,#59842,#59843,#59844,#59845,
#59846,#59847,#59848,#59849,#59850,#59851,#59852,#59853,#59854,#59855,#59856,
#59857,#59858,#59859,#59860,#59861,#59862),.UNSPECIFIED.,.F.,.F.,(4,3,3,
3,3,3,3,4),(63.9491534801646,64.7576109566257,65.7538818944199,66.7501528322141,
67.7464237700084,68.7426947078026,69.7389656455968,70.2323387873442),
 .UNSPECIFIED.);
#3251=B_SPLINE_CURVE_WITH_KNOTS('',3,(#59867,#59868,#59869,#59870,#59871,
#59872,#59873,#59874,#59875,#59876,#59877,#59878,#59879,#59880,#59881,#59882,
#59883,#59884,#59885,#59886,#59887,#59888),.UNSPECIFIED.,.F.,.F.,(4,3,3,
3,3,3,3,4),(-79.4911541062857,-78.997347043333,-77.997380625063,-76.9974142067929,
-75.9974477885229,-74.9974813702528,-73.9975149519828,-73.2079687991061),
 .UNSPECIFIED.);
#3252=B_SPLINE_CURVE_WITH_KNOTS('',3,(#59889,#59890,#59891,#59892,#59893,
#59894,#59895,#59896,#59897,#59898,#59899,#59900,#59901,#59902,#59903,#59904,
#59905,#59906,#59907,#59908,#59909,#59910),.UNSPECIFIED.,.F.,.F.,(4,3,3,
3,3,3,3,4),(70.2323387873442,70.7352365833911,71.7315075211853,72.7277784589796,
73.7240493967738,74.7203203345681,75.7165912723623,76.5155240945238),
 .UNSPECIFIED.);
#3253=B_SPLINE_CURVE_WITH_KNOTS('',3,(#59915,#59916,#59917,#59918,#59919,
#59920,#59921,#59922,#59923,#59924,#59925,#59926,#59927,#59928,#59929,#59930,
#59931,#59932,#59933,#59934,#59935,#59936),.UNSPECIFIED.,.F.,.F.,(4,3,3,
3,3,3,3,4),(-85.7743394134653,-84.9971455529532,-83.9971791346832,-82.9972127164132,
-81.9972462981431,-80.9972798798731,-79.997313461603,-79.4911541062857),
 .UNSPECIFIED.);
#3254=B_SPLINE_CURVE_WITH_KNOTS('',3,(#59937,#59938,#59939,#59940,#59941,
#59942,#59943,#59944,#59945,#59946,#59947,#59948,#59949,#59950,#59951,#59952,
#59953,#59954,#59955,#59956,#59957,#59958,#59959,#59960,#59961),
 .UNSPECIFIED.,.F.,.F.,(4,3,3,3,3,3,3,3,4),(76.5155240945238,76.7128622101565,
77.7091331479508,78.705404085745,79.7016750235393,80.6979459613335,81.6942168991278,
82.690487836922,82.7987094017034),.UNSPECIFIED.);
#3255=B_SPLINE_CURVE_WITH_KNOTS('',3,(#59966,#59967,#59968,#59969,#59970,
#59971,#59972,#59973,#59974,#59975,#59976,#59977,#59978,#59979,#59980,#59981,
#59982,#59983,#59984,#59985,#59986,#59987,#59988,#59989,#59990),
 .UNSPECIFIED.,.F.,.F.,(4,3,3,3,3,3,3,3,4),(-92.0575247206449,-91.9969104808435,
-90.9969440625734,-89.9969776443034,-88.9970112260334,-87.9970448077633,
-86.9970783894933,-85.9971119712233,-85.7743394134653),.UNSPECIFIED.);
#3256=B_SPLINE_CURVE_WITH_KNOTS('',3,(#59991,#59992,#59993,#59994,#59995,
#59996,#59997,#59998,#59999,#60000,#60001,#60002,#60003,#60004,#60005,#60006,
#60007,#60008,#60009,#60010,#60011,#60012),.UNSPECIFIED.,.F.,.F.,(4,3,3,
3,3,3,3,4),(82.7987094017034,83.6867587747162,84.6830297125105,85.6793006503047,
86.675571588099,87.6718425258932,88.6681134636875,89.081894708883),
 .UNSPECIFIED.);
#3257=B_SPLINE_CURVE_WITH_KNOTS('',3,(#60017,#60018,#60019,#60020,#60021,
#60022,#60023,#60024,#60025,#60026,#60027,#60028,#60029,#60030,#60031,#60032,
#60033,#60034,#60035,#60036,#60037,#60038),.UNSPECIFIED.,.F.,.F.,(4,3,3,
3,3,3,3,4),(-98.3407100278245,-97.9967089904637,-96.9967425721937,-95.9967761539236,
-94.9968097356536,-93.9968433173836,-92.9968768991135,-92.0575247206449),
 .UNSPECIFIED.);
#3258=B_SPLINE_CURVE_WITH_KNOTS('',3,(#60039,#60040,#60041,#60042,#60043,
#60044,#60045,#60046,#60047,#60048,#60049,#60050,#60051,#60052,#60053,#60054,
#60055,#60056,#60057,#60058,#60059,#60060),.UNSPECIFIED.,.F.,.F.,(4,3,3,
3,3,3,3,4),(89.081894708883,89.6643844014817,90.6606553392759,91.6569262770702,
92.6531972148644,93.6494681526586,94.6457390904529,95.3650800160626),
 .UNSPECIFIED.);
#3259=B_SPLINE_CURVE_WITH_KNOTS('',3,(#60065,#60066,#60067,#60068,#60069,
#60070,#60071,#60072,#60073,#60074,#60075,#60076,#60077,#60078,#60079,#60080,
#60081,#60082,#60083,#60084,#60085,#60086),.UNSPECIFIED.,.F.,.F.,(4,3,3,
3,3,3,3,4),(-104.623895335004,-103.996507500084,-102.996541081814,-101.996574663544,
-100.996608245274,-99.9966418270038,-98.9966754087338,-98.3407100278245),
 .UNSPECIFIED.);
#3260=B_SPLINE_CURVE_WITH_KNOTS('',3,(#60087,#60088,#60089,#60090,#60091,
#60092,#60093,#60094,#60095,#60096,#60097,#60098,#60099,#60100,#60101,#60102,
#60103,#60104,#60105,#60106,#60107,#60108,#60109,#60110,#60111),
 .UNSPECIFIED.,.F.,.F.,(4,3,3,3,3,3,3,3,4),(95.3650800160626,95.6420100282471,
96.6382809660413,97.6345519038356,98.6308228416299,99.6270937794241,100.623364717218,
101.619635655013,101.648265323242),.UNSPECIFIED.);
#3261=B_SPLINE_CURVE_WITH_KNOTS('',3,(#60116,#60117,#60118,#60119,#60120,
#60121,#60122,#60123,#60124,#60125,#60126,#60127,#60128,#60129,#60130,#60131,
#60132,#60133,#60134,#60135,#60136,#60137),.UNSPECIFIED.,.F.,.F.,(4,3,3,
3,3,3,3,4),(-110.907080642184,-109.996306009704,-108.996339591434,-107.996373173164,
-106.996406754894,-105.996440336624,-104.996473918354,-104.623895335004),
 .UNSPECIFIED.);
#3262=B_SPLINE_CURVE_WITH_KNOTS('',3,(#60138,#60139,#60140,#60141,#60142,
#60143,#60144,#60145,#60146,#60147,#60148,#60149,#60150,#60151,#60152,#60153,
#60154,#60155,#60156,#60157,#60158,#60159),.UNSPECIFIED.,.F.,.F.,(4,3,3,
3,3,3,3,4),(101.648265323242,102.615906592807,103.612177530601,104.608448468395,
105.60471940619,106.600990343984,107.597261281778,107.931450630422),
 .UNSPECIFIED.);
#3263=B_SPLINE_CURVE_WITH_KNOTS('',3,(#60164,#60165,#60166,#60167,#60168,
#60169,#60170,#60171,#60172,#60173,#60174,#60175,#60176,#60177,#60178,#60179,
#60180,#60181,#60182,#60183,#60184,#60185,#60186,#60187,#60188),
 .UNSPECIFIED.,.F.,.F.,(4,3,3,3,3,3,3,3,4),(-117.190265949363,-116.996070937594,
-115.996104519324,-114.996138101054,-113.996171682784,-112.996205264514,
-111.996238846244,-110.996272427974,-110.907080642184),.UNSPECIFIED.);
#3264=B_SPLINE_CURVE_WITH_KNOTS('',3,(#60189,#60190,#60191,#60192,#60193,
#60194,#60195,#60196,#60197,#60198,#60199,#60200,#60201,#60202,#60203,#60204,
#60205,#60206,#60207,#60208,#60209,#60210),.UNSPECIFIED.,.F.,.F.,(4,3,3,
3,3,3,3,4),(107.931450630422,108.593532219572,109.589803157367,110.586074095161,
111.582345032955,112.578615970749,113.574886908543,114.214635937601),
 .UNSPECIFIED.);
#3265=B_SPLINE_CURVE_WITH_KNOTS('',3,(#60215,#60216,#60217,#60218,#60219,
#60220,#60221,#60222,#60223,#60224,#60225,#60226,#60227,#60228,#60229,#60230,
#60231,#60232,#60233,#60234,#60235,#60236),.UNSPECIFIED.,.F.,.F.,(4,3,3,
3,3,3,3,4),(-123.473451256543,-122.995869447215,-121.995903028945,-120.995936610675,
-119.995970192405,-118.996003774135,-117.996037355864,-117.190265949363),
 .UNSPECIFIED.);
#3266=B_SPLINE_CURVE_WITH_KNOTS('',3,(#60237,#60238,#60239,#60240,#60241,
#60242,#60243,#60244,#60245,#60246,#60247,#60248,#60249,#60250,#60251,#60252,
#60253,#60254,#60255,#60256,#60257,#60258),.UNSPECIFIED.,.F.,.F.,(4,3,3,
3,3,3,3,4),(114.214635937601,114.571157846338,115.567428784132,116.563699721926,
117.55997065972,118.556241597515,119.552512535309,120.497821244781),
 .UNSPECIFIED.);
#3267=B_SPLINE_CURVE_WITH_KNOTS('',3,(#60263,#60264,#60265,#60266,#60267,
#60268,#60269,#60270,#60271,#60272,#60273,#60274,#60275,#60276,#60277,#60278,
#60279,#60280,#60281,#60282,#60283,#60284),.UNSPECIFIED.,.F.,.F.,(4,3,3,
3,3,3,3,4),(-129.756636563722,-128.995667956835,-127.995701538565,-126.995735120295,
-125.995768702025,-124.995802283755,-123.995835865485,-123.473451256543),
 .UNSPECIFIED.);
#3268=B_SPLINE_CURVE_WITH_KNOTS('',3,(#60285,#60286,#60287,#60288,#60289,
#60290,#60291,#60292,#60293,#60294,#60295,#60296,#60297,#60298,#60299,#60300,
#60301,#60302,#60303,#60304,#60305,#60306,#60307,#60308,#60309),
 .UNSPECIFIED.,.F.,.F.,(4,3,3,3,3,3,3,3,4),(120.497821244781,120.548783473103,
121.545054410897,122.541325348692,123.537596286486,124.53386722428,125.530138162074,
126.526409099869,126.781006551961),.UNSPECIFIED.);
#3269=B_SPLINE_CURVE_WITH_KNOTS('',3,(#60314,#60315,#60316,#60317,#60318,
#60319,#60320,#60321,#60322,#60323,#60324,#60325,#60326,#60327,#60328,#60329,
#60330,#60331,#60332,#60333,#60334,#60335,#60336,#60337,#60338),
 .UNSPECIFIED.,.F.,.F.,(4,3,3,3,3,3,3,3,4),(-136.039821870902,-135.995432884725,
-134.995466466455,-133.995500048185,-132.995533629915,-131.995567211645,
-130.995600793375,-129.995634375105,-129.756636563722),.UNSPECIFIED.);
#3270=B_SPLINE_CURVE_WITH_KNOTS('',3,(#60339,#60340,#60341,#60342,#60343,
#60344,#60345,#60346,#60347,#60348,#60349,#60350,#60351,#60352,#60353,#60354,
#60355,#60356,#60357,#60358,#60359,#60360),.UNSPECIFIED.,.F.,.F.,(4,3,3,
3,3,3,3,4),(126.781006551961,127.522680037663,128.518950975457,129.515221913251,
130.511492851046,131.50776378884,132.504034726634,133.06419185914),
 .UNSPECIFIED.);
#3271=B_SPLINE_CURVE_WITH_KNOTS('',3,(#60365,#60366,#60367,#60368,#60369,
#60370,#60371,#60372,#60373,#60374,#60375,#60376,#60377,#60378,#60379,#60380,
#60381,#60382,#60383,#60384,#60385,#60386),.UNSPECIFIED.,.F.,.F.,(4,3,3,
3,3,3,3,4),(-142.323007178082,-141.995231394345,-140.995264976075,-139.995298557805,
-138.995332139535,-137.995365721265,-136.995399302995,-136.039821870902),
 .UNSPECIFIED.);
#3272=B_SPLINE_CURVE_WITH_KNOTS('',3,(#60387,#60388,#60389,#60390,#60391,
#60392,#60393,#60394,#60395,#60396,#60397,#60398,#60399,#60400,#60401,#60402,
#60403,#60404,#60405,#60406,#60407,#60408),.UNSPECIFIED.,.F.,.F.,(4,3,3,
3,3,3,3,4),(133.06419185914,133.500305664428,134.496576602223,135.492847540017,
136.489118477811,137.485389415605,138.481660353399,139.34737716632),
 .UNSPECIFIED.);
#3273=B_SPLINE_CURVE_WITH_KNOTS('',3,(#60413,#60414,#60415,#60416,#60417,
#60418,#60419,#60420,#60421,#60422,#60423,#60424,#60425,#60426,#60427,#60428,
#60429,#60430,#60431,#60432,#60433,#60434),.UNSPECIFIED.,.F.,.F.,(4,3,3,
3,3,3,3,4),(-148.606192485261,-147.995029903966,-146.995063485696,-145.995097067426,
-144.995130649155,-143.995164230885,-142.995197812615,-142.323007178082),
 .UNSPECIFIED.);
#3274=B_SPLINE_CURVE_WITH_KNOTS('',3,(#60435,#60436,#60437,#60438,#60439,
#60440,#60441,#60442,#60443,#60444,#60445,#60446,#60447,#60448,#60449,#60450,
#60451,#60452,#60453,#60454,#60455,#60456,#60457,#60458,#60459),
 .UNSPECIFIED.,.F.,.F.,(4,3,3,3,3,3,3,3,4),(139.34737716632,139.477931291194,
140.474202228988,141.470473166782,142.466744104576,143.463015042371,144.459285980165,
145.455556917959,145.630562473499),.UNSPECIFIED.);
#3275=B_SPLINE_CURVE_WITH_KNOTS('',3,(#60464,#60465,#60466,#60467,#60468,
#60469,#60470,#60471,#60472,#60473,#60474,#60475,#60476,#60477,#60478,#60479,
#60480,#60481,#60482,#60483,#60484,#60485),.UNSPECIFIED.,.F.,.F.,(4,3,3,
3,3,3,3,4),(-154.889377792441,-153.994828413586,-152.994861995316,-151.994895577046,
-150.994929158776,-149.994962740506,-148.994996322236,-148.606192485261),
 .UNSPECIFIED.);
#3276=B_SPLINE_CURVE_WITH_KNOTS('',3,(#60486,#60487,#60488,#60489,#60490,
#60491,#60492,#60493,#60494,#60495,#60496,#60497,#60498,#60499,#60500,#60501,
#60502,#60503,#60504,#60505,#60506,#60507),.UNSPECIFIED.,.F.,.F.,(4,3,3,
3,3,3,3,4),(145.630562473499,146.451827855753,147.448098793548,148.444369731342,
149.440640669136,150.43691160693,151.433182544725,151.913747780679),
 .UNSPECIFIED.);
#3277=B_SPLINE_CURVE_WITH_KNOTS('',3,(#60512,#60513,#60514,#60515,#60516,
#60517,#60518,#60519,#60520,#60521,#60522,#60523,#60524,#60525,#60526,#60527,
#60528,#60529,#60530,#60531,#60532,#60533,#60534,#60535,#60536),
 .UNSPECIFIED.,.F.,.F.,(4,3,3,3,3,3,3,3,4),(-161.17256309962,-160.994593341476,
-159.994626923206,-158.994660504936,-157.994694086666,-156.994727668396,
-155.994761250126,-154.994794831856,-154.889377792441),.UNSPECIFIED.);
#3278=B_SPLINE_CURVE_WITH_KNOTS('',3,(#60537,#60538,#60539,#60540,#60541,
#60542,#60543,#60544,#60545,#60546,#60547,#60548,#60549,#60550,#60551,#60552,
#60553,#60554,#60555,#60556,#60557,#60558),.UNSPECIFIED.,.F.,.F.,(4,3,3,
3,3,3,3,4),(151.913747780679,152.429453482519,153.425724420313,154.421995358107,
155.418266295902,156.414537233696,157.41080817149,158.196933087858),
 .UNSPECIFIED.);
#3279=B_SPLINE_CURVE_WITH_KNOTS('',3,(#60563,#60564,#60565,#60566,#60567,
#60568,#60569,#60570,#60571,#60572,#60573,#60574,#60575,#60576,#60577,#60578,
#60579,#60580,#60581,#60582,#60583,#60584),.UNSPECIFIED.,.F.,.F.,(4,3,3,
3,3,3,3,4),(-167.4557484068,-166.994391851096,-165.994425432826,-164.994459014556,
-163.994492596286,-162.994526178016,-161.994559759746,-161.17256309962),
 .UNSPECIFIED.);
#3280=B_SPLINE_CURVE_WITH_KNOTS('',3,(#60585,#60586,#60587,#60588,#60589,
#60590,#60591,#60592,#60593,#60594,#60595,#60596,#60597,#60598,#60599,#60600,
#60601,#60602,#60603,#60604,#60605,#60606,#60607,#60608,#60609),
 .UNSPECIFIED.,.F.,.F.,(4,3,3,3,3,3,3,3,4),(158.196933087858,158.407079109284,
159.403350047079,160.399620984873,161.395891922667,162.392162860461,163.388433798255,
164.38470473605,164.480118395038),.UNSPECIFIED.);
#3281=B_SPLINE_CURVE_WITH_KNOTS('',3,(#60614,#60615,#60616,#60617,#60618,
#60619,#60620,#60621,#60622,#60623,#60624,#60625,#60626,#60627,#60628,#60629,
#60630,#60631,#60632,#60633,#60634,#60635),.UNSPECIFIED.,.F.,.F.,(4,3,3,
3,3,3,3,4),(-173.738933713979,-172.994190360717,-171.994223942447,-170.994257524176,
-169.994291105906,-168.994324687636,-167.994358269366,-167.4557484068),
 .UNSPECIFIED.);
#3282=B_SPLINE_CURVE_WITH_KNOTS('',3,(#60636,#60637,#60638,#60639,#60640,
#60641,#60642,#60643,#60644,#60645,#60646,#60647,#60648,#60649,#60650,#60651,
#60652,#60653,#60654,#60655,#60656,#60657),.UNSPECIFIED.,.F.,.F.,(4,3,3,
3,3,3,3,4),(164.480118395038,165.380975673844,166.377246611638,167.373517549432,
168.369788487227,169.366059425021,170.362330362815,170.763303702218),
 .UNSPECIFIED.);
#3283=B_SPLINE_CURVE_WITH_KNOTS('',3,(#60662,#60663,#60664,#60665,#60666,
#60667,#60668,#60669,#60670,#60671,#60672,#60673,#60674,#60675,#60676,#60677,
#60678,#60679,#60680,#60681,#60682,#60683,#60684,#60685,#60686),
 .UNSPECIFIED.,.F.,.F.,(4,3,3,3,3,3,3,3,4),(-180.022119021159,-179.993955288607,
-178.993988870337,-177.994022452067,-176.994056033797,-175.994089615527,
-174.994123197257,-173.994156778987,-173.738933713979),.UNSPECIFIED.);
#3284=B_SPLINE_CURVE_WITH_KNOTS('',3,(#60687,#60688,#60689,#60690,#60691,
#60692,#60693,#60694,#60695,#60696,#60697,#60698,#60699,#60700,#60701,#60702,
#60703,#60704,#60705,#60706,#60707,#60708),.UNSPECIFIED.,.F.,.F.,(4,3,3,
3,3,3,3,4),(170.763303702218,171.358601300609,172.354872238404,173.351143176198,
174.347414113992,175.343685051786,176.339955989581,177.046489009397),
 .UNSPECIFIED.);
#3285=B_SPLINE_CURVE_WITH_KNOTS('',3,(#60713,#60714,#60715,#60716,#60717,
#60718,#60719,#60720,#60721,#60722,#60723,#60724,#60725,#60726,#60727,#60728,
#60729,#60730,#60731,#60732,#60733,#60734),.UNSPECIFIED.,.F.,.F.,(4,3,3,
3,3,3,3,4),(-186.305304328339,-185.993753798227,-184.993787379957,-183.993820961687,
-182.993854543417,-181.993888125147,-180.993921706877,-180.022119021159),
 .UNSPECIFIED.);
#3286=B_SPLINE_CURVE_WITH_KNOTS('',3,(#60735,#60736,#60737,#60738,#60739,
#60740,#60741,#60742,#60743,#60744,#60745,#60746,#60747,#60748,#60749,#60750,
#60751,#60752,#60753,#60754,#60755,#60756,#60757,#60758,#60759),
 .UNSPECIFIED.,.F.,.F.,(4,3,3,3,3,3,3,3,4),(177.046489009397,177.336226927375,
178.332497865169,179.328768802963,180.325039740758,181.321310678552,182.317581616346,
183.31385255414,183.329674316577),.UNSPECIFIED.);
#3287=B_SPLINE_CURVE_WITH_KNOTS('',3,(#60764,#60765,#60766,#60767,#60768,
#60769,#60770,#60771,#60772,#60773,#60774,#60775,#60776,#60777,#60778,#60779,
#60780,#60781,#60782,#60783,#60784,#60785),.UNSPECIFIED.,.F.,.F.,(4,3,3,
3,3,3,3,4),(-192.588489635518,-191.993552307847,-190.993585889577,-189.993619471307,
-188.993653053037,-187.993686634767,-186.993720216497,-186.305304328339),
 .UNSPECIFIED.);
#3288=B_SPLINE_CURVE_WITH_KNOTS('',3,(#60786,#60787,#60788,#60789,#60790,
#60791,#60792,#60793,#60794,#60795,#60796,#60797,#60798,#60799,#60800,#60801,
#60802,#60803,#60804,#60805,#60806,#60807),.UNSPECIFIED.,.F.,.F.,(4,3,3,
3,3,3,3,4),(183.329674316577,184.310123491935,185.306394429729,186.302665367523,
187.298936305317,188.295207243112,189.291478180906,189.612859623756),
 .UNSPECIFIED.);
#3289=B_SPLINE_CURVE_WITH_KNOTS('',3,(#60812,#60813,#60814,#60815,#60816,
#60817,#60818,#60819,#60820,#60821,#60822,#60823,#60824,#60825,#60826,#60827,
#60828,#60829,#60830,#60831,#60832,#60833),.UNSPECIFIED.,.F.,.F.,(4,3,3,
3,3,3,3,4),(-198.871674942698,-197.993350817467,-196.993384399197,-195.993417980927,
-194.993451562657,-193.993485144387,-192.993518726117,-192.588489635518),
 .UNSPECIFIED.);
#3290=B_SPLINE_CURVE_WITH_KNOTS('',3,(#60834,#60835,#60836,#60837,#60838,
#60839,#60840,#60841,#60842,#60843,#60844,#60845,#60846,#60847,#60848,#60849,
#60850,#60851,#60852,#60853,#60854,#60855),.UNSPECIFIED.,.F.,.F.,(4,3,3,
3,3,3,3,4),(189.612859623756,190.2877491187,191.284020056494,192.280290994288,
193.276561932083,194.272832869877,195.269103807671,195.896044930936),
 .UNSPECIFIED.);
#3291=B_SPLINE_CURVE_WITH_KNOTS('',3,(#60860,#60861,#60862,#60863,#60864,
#60865,#60866,#60867,#60868,#60869,#60870,#60871,#60872,#60873,#60874,#60875,
#60876,#60877,#60878,#60879,#60880,#60881,#60882,#60883,#60884),
 .UNSPECIFIED.,.F.,.F.,(4,3,3,3,3,3,3,3,4),(-205.154860249877,-204.993115745358,
-203.993149327088,-202.993182908818,-201.993216490548,-200.993250072278,
-199.993283654008,-198.993317235738,-198.871674942698),.UNSPECIFIED.);
#3292=B_SPLINE_CURVE_WITH_KNOTS('',3,(#60885,#60886,#60887,#60888,#60889,
#60890,#60891,#60892,#60893,#60894,#60895,#60896,#60897,#60898,#60899,#60900,
#60901,#60902,#60903,#60904,#60905,#60906),.UNSPECIFIED.,.F.,.F.,(4,3,3,
3,3,3,3,4),(195.896044930936,196.265374745465,197.26164568326,198.257916621054,
199.254187558848,200.250458496642,201.246729434437,202.179230238115),
 .UNSPECIFIED.);
#3293=B_SPLINE_CURVE_WITH_KNOTS('',3,(#60911,#60912,#60913,#60914,#60915,
#60916,#60917,#60918,#60919,#60920,#60921,#60922,#60923,#60924,#60925,#60926,
#60927,#60928,#60929,#60930,#60931,#60932),.UNSPECIFIED.,.F.,.F.,(4,3,3,
3,3,3,3,4),(-211.438045557057,-210.992914254978,-209.992947836708,-208.992981418438,
-207.993015000168,-206.993048581898,-205.993082163628,-205.154860249877),
 .UNSPECIFIED.);
#3294=B_SPLINE_CURVE_WITH_KNOTS('',3,(#60933,#60934,#60935,#60936,#60937,
#60938,#60939,#60940,#60941,#60942,#60943,#60944,#60945,#60946,#60947,#60948,
#60949,#60950,#60951,#60952,#60953,#60954,#60955,#60956,#60957),
 .UNSPECIFIED.,.F.,.F.,(4,3,3,3,3,3,3,3,4),(202.179230238115,202.243000372231,
203.239271310025,204.235542247819,205.231813185614,206.228084123408,207.224355061202,
208.220625998996,208.462415545295),.UNSPECIFIED.);
#3295=B_SPLINE_CURVE_WITH_KNOTS('',3,(#60962,#60963,#60964,#60965,#60966,
#60967,#60968,#60969,#60970,#60971,#60972,#60973,#60974,#60975,#60976,#60977,
#60978,#60979,#60980,#60981,#60982,#60983),.UNSPECIFIED.,.F.,.F.,(4,3,3,
3,3,3,3,4),(-217.721230864236,-216.992712764598,-215.992746346328,-214.992779928058,
-213.992813509788,-212.992847091518,-211.992880673248,-211.438045557057),
 .UNSPECIFIED.);
#3296=B_SPLINE_CURVE_WITH_KNOTS('',3,(#60984,#60985,#60986,#60987,#60988,
#60989,#60990,#60991,#60992,#60993,#60994,#60995,#60996,#60997,#60998,#60999,
#61000,#61001,#61002,#61003,#61004,#61005),.UNSPECIFIED.,.F.,.F.,(4,3,3,
3,3,3,3,4),(208.462415545295,209.216896936791,210.213167874585,211.209438812379,
212.205709750173,213.201980687968,214.198251625762,214.745600852474),
 .UNSPECIFIED.);
#3297=B_SPLINE_CURVE_WITH_KNOTS('',3,(#61010,#61011,#61012,#61013,#61014,
#61015,#61016,#61017,#61018,#61019,#61020,#61021,#61022,#61023,#61024,#61025,
#61026,#61027,#61028,#61029,#61030,#61031,#61032,#61033,#61034),
 .UNSPECIFIED.,.F.,.F.,(4,3,3,3,3,3,3,3,4),(-224.004416171416,-223.992477692488,
-222.992511274218,-221.992544855948,-220.992578437678,-219.992612019408,
-218.992645601138,-217.992679182868,-217.721230864236),.UNSPECIFIED.);
#3298=B_SPLINE_CURVE_WITH_KNOTS('',3,(#61035,#61036,#61037,#61038,#61039,
#61040,#61041,#61042,#61043,#61044,#61045,#61046,#61047,#61048,#61049,#61050,
#61051,#61052,#61053,#61054,#61055,#61056),.UNSPECIFIED.,.F.,.F.,(4,3,3,
3,3,3,3,4),(214.745600852474,215.194522563556,216.19079350135,217.187064439145,
218.183335376939,219.179606314733,220.175877252527,221.028786159654),
 .UNSPECIFIED.);
#3299=B_SPLINE_CURVE_WITH_KNOTS('',3,(#61061,#61062,#61063,#61064,#61065,
#61066,#61067,#61068,#61069,#61070,#61071,#61072,#61073,#61074,#61075,#61076,
#61077,#61078,#61079,#61080,#61081,#61082),.UNSPECIFIED.,.F.,.F.,(4,3,3,
3,3,3,3,4),(-230.287601478595,-229.992276202109,-228.992309783839,-227.992343365569,
-226.992376947299,-225.992410529029,-224.992444110759,-224.004416171416),
 .UNSPECIFIED.);
#3300=B_SPLINE_CURVE_WITH_KNOTS('',3,(#61083,#61084,#61085,#61086,#61087,
#61088,#61089,#61090,#61091,#61092,#61093,#61094,#61095,#61096,#61097,#61098,
#61099,#61100,#61101,#61102,#61103,#61104,#61105,#61106,#61107),
 .UNSPECIFIED.,.F.,.F.,(4,3,3,3,3,3,3,3,4),(221.028786159654,221.172148190321,
222.168419128116,223.16469006591,224.160961003704,225.157231941498,226.153502879293,
227.149773817087,227.311971466834),.UNSPECIFIED.);
#3301=B_SPLINE_CURVE_WITH_KNOTS('',3,(#61112,#61113,#61114,#61115,#61116,
#61117,#61118,#61119,#61120,#61121,#61122,#61123,#61124,#61125,#61126,#61127,
#61128,#61129,#61130,#61131,#61132,#61133),.UNSPECIFIED.,.F.,.F.,(4,3,3,
3,3,3,3,4),(-236.570786785775,-235.992074711729,-234.992108293459,-233.992141875189,
-232.992175456919,-231.992209038649,-230.992242620379,-230.287601478595),
 .UNSPECIFIED.);
#3302=B_SPLINE_CURVE_WITH_KNOTS('',3,(#61134,#61135,#61136,#61137,#61138,
#61139,#61140,#61141,#61142,#61143,#61144,#61145,#61146,#61147,#61148,#61149,
#61150,#61151,#61152,#61153,#61154,#61155),.UNSPECIFIED.,.F.,.F.,(4,3,3,
3,3,3,3,4),(227.311971466834,228.146044754881,229.142315692675,230.13858663047,
231.134857568264,232.131128506058,233.127399443852,233.595156774013),
 .UNSPECIFIED.);
#3303=B_SPLINE_CURVE_WITH_KNOTS('',3,(#61160,#61161,#61162,#61163,#61164,
#61165,#61166,#61167,#61168,#61169,#61170,#61171,#61172,#61173,#61174,#61175,
#61176,#61177,#61178,#61179,#61180,#61181),.UNSPECIFIED.,.F.,.F.,(4,3,3,
3,3,3,3,4),(-242.853972092955,-241.991873221349,-240.991906803079,-239.991940384809,
-238.991973966539,-237.992007548269,-236.992041129999,-236.570786785775),
 .UNSPECIFIED.);
#3304=B_SPLINE_CURVE_WITH_KNOTS('',3,(#61182,#61183,#61184,#61185,#61186,
#61187,#61188,#61189,#61190,#61191,#61192,#61193,#61194,#61195,#61196,#61197,
#61198,#61199,#61200,#61201,#61202,#61203),.UNSPECIFIED.,.F.,.F.,(4,3,3,
3,3,3,3,4),(233.595156774013,234.123670381647,235.119941319441,236.116212257235,
237.112483195029,238.108754132824,239.105025070618,239.878342081193),
 .UNSPECIFIED.);
#3305=B_SPLINE_CURVE_WITH_KNOTS('',3,(#61209,#61210,#61211,#61212,#61213,
#61214,#61215,#61216,#61217,#61218),.UNSPECIFIED.,.F.,.F.,(4,1,1,1,1,1,
1,4),(254.469004940773,254.606872487438,255.606838905708,256.606805323978,
257.606771742248,258.606738160518,259.606704578788,260.606670997058),
 .UNSPECIFIED.);
#3306=B_SPLINE_CURVE_WITH_KNOTS('',3,(#61221,#61222,#61223,#61224,#61225,
#61226,#61227,#61228),.UNSPECIFIED.,.F.,.F.,(4,1,1,1,1,4),(254.469004940773,
255.382670125373,256.378941063167,257.375212000962,258.371482938756,259.36775387655),
 .UNSPECIFIED.);
#3307=B_SPLINE_CURVE_WITH_KNOTS('',3,(#61233,#61234,#61235,#61236,#61237,
#61238,#61239,#61240,#61241,#61242),.UNSPECIFIED.,.F.,.F.,(4,1,1,1,1,1,
1,4),(248.185819633594,248.607073977818,249.607040396088,250.607006814358,
251.606973232628,252.606939650898,253.606906069168,254.469004940773),
 .UNSPECIFIED.);
#3308=B_SPLINE_CURVE_WITH_KNOTS('',3,(#61243,#61244,#61245,#61246,#61247,
#61248,#61249,#61250,#61251,#61252,#61253),.UNSPECIFIED.,.F.,.F.,(4,1,1,
1,1,1,1,1,4),(248.185819633594,248.408773560813,249.405044498608,250.401315436402,
251.397586374196,252.39385731199,253.390128249785,254.386399187579,254.469004940773),
 .UNSPECIFIED.);
#3309=B_SPLINE_CURVE_WITH_KNOTS('',3,(#61258,#61259,#61260,#61261,#61262,
#61263,#61264,#61265,#61266,#61267),.UNSPECIFIED.,.F.,.F.,(4,1,1,1,1,1,
1,4),(241.902634326414,242.607275468197,243.607241886467,244.607208304738,
245.607174723008,246.607141141278,247.607107559548,248.185819633594),
 .UNSPECIFIED.);
#3310=B_SPLINE_CURVE_WITH_KNOTS('',3,(#61268,#61269,#61270,#61271,#61272,
#61273,#61274,#61275,#61276,#61277),.UNSPECIFIED.,.F.,.F.,(4,1,1,1,1,1,
1,4),(241.902634326414,242.431147934048,243.427418871842,244.423689809636,
245.419960747431,246.416231685225,247.412502623019,248.185819633594),
 .UNSPECIFIED.);
#3311=B_SPLINE_CURVE_WITH_KNOTS('',3,(#61282,#61283,#61284,#61285,#61286,
#61287,#61288,#61289,#61290,#61291),.UNSPECIFIED.,.F.,.F.,(4,1,1,1,1,1,
1,4),(235.619449019234,236.607476958577,237.607443376847,238.607409795117,
239.607376213387,240.607342631657,241.607309049927,241.902634326414),
 .UNSPECIFIED.);
#3312=B_SPLINE_CURVE_WITH_KNOTS('',3,(#61292,#61293,#61294,#61295,#61296,
#61297,#61298,#61299,#61300,#61301),.UNSPECIFIED.,.F.,.F.,(4,1,1,1,1,1,
1,4),(235.619449019235,236.453522307283,237.449793245077,238.446064182871,
239.442335120665,240.438606058459,241.434876996254,241.902634326414),
 .UNSPECIFIED.);
#3313=B_SPLINE_CURVE_WITH_KNOTS('',3,(#61306,#61307,#61308,#61309,#61310,
#61311,#61312,#61313,#61314,#61315,#61316),.UNSPECIFIED.,.F.,.F.,(4,1,1,
1,1,1,1,1,4),(229.336263712055,229.607712030687,230.607678448957,231.607644867227,
232.607611285497,233.607577703767,234.607544122037,235.607510540307,235.619449019234),
 .UNSPECIFIED.);
#3314=B_SPLINE_CURVE_WITH_KNOTS('',3,(#61317,#61318,#61319,#61320,#61321,
#61322,#61323,#61324,#61325,#61326,#61327),.UNSPECIFIED.,.F.,.F.,(4,1,1,
1,1,1,1,1,4),(229.336263712055,229.479625742723,230.475896680517,231.472167618311,
232.468438556106,233.4647094939,234.460980431694,235.457251369488,235.619449019235),
 .UNSPECIFIED.);
#3315=B_SPLINE_CURVE_WITH_KNOTS('',3,(#61332,#61333,#61334,#61335,#61336,
#61337,#61338,#61339,#61340,#61341),.UNSPECIFIED.,.F.,.F.,(4,1,1,1,1,1,
1,4),(223.053078404875,223.607913521067,224.607879939337,225.607846357607,
226.607812775877,227.607779194147,228.607745612417,229.336263712055),
 .UNSPECIFIED.);
#3316=B_SPLINE_CURVE_WITH_KNOTS('',3,(#61342,#61343,#61344,#61345,#61346,
#61347,#61348,#61349,#61350,#61351),.UNSPECIFIED.,.F.,.F.,(4,1,1,1,1,1,
1,4),(223.053078404875,223.502000115957,224.498271053752,225.494541991546,
226.49081292934,227.487083867134,228.483354804929,229.336263712055),
 .UNSPECIFIED.);
#3317=B_SPLINE_CURVE_WITH_KNOTS('',3,(#61356,#61357,#61358,#61359,#61360,
#61361,#61362,#61363,#61364,#61365),.UNSPECIFIED.,.F.,.F.,(4,1,1,1,1,1,
1,4),(216.769893097696,217.608115011447,218.608081429717,219.608047847987,
220.608014266257,221.607980684527,222.607947102797,223.053078404875),
 .UNSPECIFIED.);
#3318=B_SPLINE_CURVE_WITH_KNOTS('',3,(#61366,#61367,#61368,#61369,#61370,
#61371,#61372,#61373,#61374,#61375),.UNSPECIFIED.,.F.,.F.,(4,1,1,1,1,1,
1,4),(216.769893097696,217.524374489192,218.520645426986,219.51691636478,
220.513187302575,221.509458240369,222.505729178163,223.053078404875),
 .UNSPECIFIED.);
#3319=B_SPLINE_CURVE_WITH_KNOTS('',3,(#61380,#61381,#61382,#61383,#61384,
#61385,#61386,#61387,#61388,#61389,#61390),.UNSPECIFIED.,.F.,.F.,(4,1,1,
1,1,1,1,1,4),(210.486707790516,210.608350083556,211.608316501826,212.608282920096,
213.608249338366,214.608215756636,215.608182174906,216.608148593176,216.769893097696),
 .UNSPECIFIED.);
#3320=B_SPLINE_CURVE_WITH_KNOTS('',3,(#61391,#61392,#61393,#61394,#61395,
#61396,#61397,#61398,#61399,#61400,#61401),.UNSPECIFIED.,.F.,.F.,(4,1,1,
1,1,1,1,1,4),(210.486707790516,210.550477924632,211.546748862427,212.543019800221,
213.539290738015,214.535561675809,215.531832613603,216.528103551398,216.769893097696),
 .UNSPECIFIED.);
#3321=B_SPLINE_CURVE_WITH_KNOTS('',3,(#61406,#61407,#61408,#61409,#61410,
#61411,#61412,#61413,#61414,#61415),.UNSPECIFIED.,.F.,.F.,(4,1,1,1,1,1,
1,4),(204.203522483337,204.608551573936,205.608517992206,206.608484410476,
207.608450828746,208.608417247016,209.608383665286,210.486707790516),
 .UNSPECIFIED.);
#3322=B_SPLINE_CURVE_WITH_KNOTS('',3,(#61416,#61417,#61418,#61419,#61420,
#61421,#61422,#61423,#61424,#61425),.UNSPECIFIED.,.F.,.F.,(4,1,1,1,1,1,
1,4),(204.203522483337,204.572852297867,205.569123235661,206.565394173455,
207.56166511125,208.557936049044,209.554206986838,210.486707790516),
 .UNSPECIFIED.);
#3323=B_SPLINE_CURVE_WITH_KNOTS('',3,(#61430,#61431,#61432,#61433,#61434,
#61435,#61436,#61437,#61438,#61439),.UNSPECIFIED.,.F.,.F.,(4,1,1,1,1,1,
1,4),(197.920337176157,198.608753064316,199.608719482586,200.608685900856,
201.608652319126,202.608618737396,203.608585155666,204.203522483337),
 .UNSPECIFIED.);
#3324=B_SPLINE_CURVE_WITH_KNOTS('',3,(#61440,#61441,#61442,#61443,#61444,
#61445,#61446,#61447,#61448,#61449),.UNSPECIFIED.,.F.,.F.,(4,1,1,1,1,1,
1,4),(197.920337176157,198.595226671101,199.591497608896,200.58776854669,
201.584039484484,202.580310422278,203.576581360073,204.203522483337),
 .UNSPECIFIED.);
#3325=B_SPLINE_CURVE_WITH_KNOTS('',3,(#61454,#61455,#61456,#61457,#61458,
#61459,#61460,#61461,#61462,#61463),.UNSPECIFIED.,.F.,.F.,(4,1,1,1,1,1,
1,4),(191.637151868977,192.608954554696,193.608920972966,194.608887391236,
195.608853809506,196.608820227776,197.608786646046,197.920337176157),
 .UNSPECIFIED.);
#3326=B_SPLINE_CURVE_WITH_KNOTS('',3,(#61464,#61465,#61466,#61467,#61468,
#61469,#61470,#61471,#61472,#61473),.UNSPECIFIED.,.F.,.F.,(4,1,1,1,1,1,
1,4),(191.637151868978,192.617601044336,193.61387198213,194.610142919924,
195.606413857719,196.602684795513,197.598955733307,197.920337176157),
 .UNSPECIFIED.);
#3327=B_SPLINE_CURVE_WITH_KNOTS('',3,(#61478,#61479,#61480,#61481,#61482,
#61483,#61484,#61485,#61486,#61487,#61488),.UNSPECIFIED.,.F.,.F.,(4,1,1,
1,1,1,1,1,4),(185.353966561798,185.609189626805,186.609156045075,187.609122463345,
188.609088881615,189.609055299885,190.609021718155,191.608988136425,191.637151868977),
 .UNSPECIFIED.);
#3328=B_SPLINE_CURVE_WITH_KNOTS('',3,(#61489,#61490,#61491,#61492,#61493,
#61494,#61495,#61496,#61497,#61498,#61499),.UNSPECIFIED.,.F.,.F.,(4,1,1,
1,1,1,1,1,4),(185.353966561798,185.643704479776,186.63997541757,187.636246355365,
188.632517293159,189.628788230953,190.625059168747,191.621330106542,191.637151868978),
 .UNSPECIFIED.);
#3329=B_SPLINE_CURVE_WITH_KNOTS('',3,(#61504,#61505,#61506,#61507,#61508,
#61509,#61510,#61511,#61512,#61513),.UNSPECIFIED.,.F.,.F.,(4,1,1,1,1,1,
1,4),(179.070781254618,179.609391117185,180.609357535455,181.609323953725,
182.609290371995,183.609256790265,184.609223208535,185.353966561798),
 .UNSPECIFIED.);
#3330=B_SPLINE_CURVE_WITH_KNOTS('',3,(#61514,#61515,#61516,#61517,#61518,
#61519,#61520,#61521,#61522,#61523),.UNSPECIFIED.,.F.,.F.,(4,1,1,1,1,1,
1,4),(179.070781254618,179.666078853011,180.662349790805,181.658620728599,
182.654891666394,183.651162604188,184.647433541982,185.353966561798),
 .UNSPECIFIED.);
#3331=B_SPLINE_CURVE_WITH_KNOTS('',3,(#61528,#61529,#61530,#61531,#61532,
#61533,#61534,#61535,#61536,#61537),.UNSPECIFIED.,.F.,.F.,(4,1,1,1,1,1,
1,4),(172.787595947439,173.609592607565,174.609559025835,175.609525444105,
176.609491862375,177.609458280645,178.609424698915,179.070781254618),
 .UNSPECIFIED.);
#3332=B_SPLINE_CURVE_WITH_KNOTS('',3,(#61538,#61539,#61540,#61541,#61542,
#61543,#61544,#61545,#61546,#61547),.UNSPECIFIED.,.F.,.F.,(4,1,1,1,1,1,
1,4),(172.787595947439,173.688453226245,174.68472416404,175.680995101834,
176.677266039628,177.673536977422,178.669807915217,179.070781254618),
 .UNSPECIFIED.);
#3333=B_SPLINE_CURVE_WITH_KNOTS('',3,(#61552,#61553,#61554,#61555,#61556,
#61557,#61558,#61559,#61560,#61561,#61562),.UNSPECIFIED.,.F.,.F.,(4,1,1,
1,1,1,1,1,4),(166.504410640259,166.609827679675,167.609794097945,168.609760516215,
169.609726934485,170.609693352755,171.609659771025,172.609626189295,172.787595947439),
 .UNSPECIFIED.);
#3334=B_SPLINE_CURVE_WITH_KNOTS('',3,(#61563,#61564,#61565,#61566,#61567,
#61568,#61569,#61570,#61571,#61572,#61573),.UNSPECIFIED.,.F.,.F.,(4,1,1,
1,1,1,1,1,4),(166.504410640259,166.714556661686,167.71082759948,168.707098537274,
169.703369475068,170.699640412863,171.695911350657,172.692182288451,172.787595947439),
 .UNSPECIFIED.);
#3335=B_SPLINE_CURVE_WITH_KNOTS('',3,(#61578,#61579,#61580,#61581,#61582,
#61583,#61584,#61585,#61586,#61587),.UNSPECIFIED.,.F.,.F.,(4,1,1,1,1,1,
1,4),(160.22122533308,160.610029170054,161.609995588324,162.609962006594,
163.609928424864,164.609894843134,165.609861261405,166.504410640259),
 .UNSPECIFIED.);
#3336=B_SPLINE_CURVE_WITH_KNOTS('',3,(#61588,#61589,#61590,#61591,#61592,
#61593,#61594,#61595,#61596,#61597),.UNSPECIFIED.,.F.,.F.,(4,1,1,1,1,1,
1,4),(160.22122533308,160.73693103492,161.733201972714,162.729472910509,
163.725743848303,164.722014786097,165.718285723891,166.504410640259),
 .UNSPECIFIED.);
#3337=B_SPLINE_CURVE_WITH_KNOTS('',3,(#61602,#61603,#61604,#61605,#61606,
#61607,#61608,#61609,#61610,#61611),.UNSPECIFIED.,.F.,.F.,(4,1,1,1,1,1,
1,4),(153.9380400259,154.610230660434,155.610197078704,156.610163496974,
157.610129915244,158.610096333514,159.610062751784,160.22122533308),
 .UNSPECIFIED.);
#3338=B_SPLINE_CURVE_WITH_KNOTS('',3,(#61612,#61613,#61614,#61615,#61616,
#61617,#61618,#61619,#61620,#61621),.UNSPECIFIED.,.F.,.F.,(4,1,1,1,1,1,
1,4),(153.9380400259,154.759305408155,155.755576345949,156.751847283743,
157.748118221538,158.744389159332,159.740660097126,160.22122533308),
 .UNSPECIFIED.);
#3339=B_SPLINE_CURVE_WITH_KNOTS('',3,(#61626,#61627,#61628,#61629,#61630,
#61631,#61632,#61633,#61634,#61635),.UNSPECIFIED.,.F.,.F.,(4,1,1,1,1,1,
1,4),(147.654854718721,148.610432150814,149.610398569084,150.610364987354,
151.610331405624,152.610297823894,153.610264242164,153.9380400259),
 .UNSPECIFIED.);
#3340=B_SPLINE_CURVE_WITH_KNOTS('',3,(#61636,#61637,#61638,#61639,#61640,
#61641,#61642,#61643,#61644,#61645,#61646),.UNSPECIFIED.,.F.,.F.,(4,1,1,
1,1,1,1,1,4),(147.654854718721,147.785408843595,148.781679781389,149.777950719184,
150.774221656978,151.770492594772,152.766763532566,153.763034470361,153.9380400259),
 .UNSPECIFIED.);
#3341=B_SPLINE_CURVE_WITH_KNOTS('',3,(#61651,#61652,#61653,#61654,#61655,
#61656,#61657,#61658,#61659,#61660,#61661),.UNSPECIFIED.,.F.,.F.,(4,1,1,
1,1,1,1,1,4),(141.371669411541,141.610667222924,142.610633641194,143.610600059464,
144.610566477734,145.610532896004,146.610499314274,147.610465732544,147.654854718721),
 .UNSPECIFIED.);
#3342=B_SPLINE_CURVE_WITH_KNOTS('',3,(#61662,#61663,#61664,#61665,#61666,
#61667,#61668,#61669,#61670,#61671),.UNSPECIFIED.,.F.,.F.,(4,1,1,1,1,1,
1,4),(141.371669411541,141.80778321683,142.804054154624,143.800325092418,
144.796596030212,145.792866968007,146.789137905801,147.654854718721),
 .UNSPECIFIED.);
#3343=B_SPLINE_CURVE_WITH_KNOTS('',3,(#61676,#61677,#61678,#61679,#61680,
#61681,#61682,#61683,#61684,#61685),.UNSPECIFIED.,.F.,.F.,(4,1,1,1,1,1,
1,4),(135.088484104361,135.610868713303,136.610835131573,137.610801549843,
138.610767968113,139.610734386384,140.610700804654,141.371669411541),
 .UNSPECIFIED.);
#3344=B_SPLINE_CURVE_WITH_KNOTS('',3,(#61686,#61687,#61688,#61689,#61690,
#61691,#61692,#61693,#61694,#61695),.UNSPECIFIED.,.F.,.F.,(4,1,1,1,1,1,
1,4),(135.088484104361,135.830157590064,136.826428527858,137.822699465653,
138.818970403447,139.815241341241,140.811512279035,141.371669411541),
 .UNSPECIFIED.);
#3345=B_SPLINE_CURVE_WITH_KNOTS('',3,(#61700,#61701,#61702,#61703,#61704,
#61705,#61706,#61707,#61708,#61709),.UNSPECIFIED.,.F.,.F.,(4,1,1,1,1,1,
1,4),(128.805298797182,129.611070203683,130.611036621953,131.611003040223,
132.610969458493,133.610935876763,134.610902295033,135.088484104361),
 .UNSPECIFIED.);
#3346=B_SPLINE_CURVE_WITH_KNOTS('',3,(#61710,#61711,#61712,#61713,#61714,
#61715,#61716,#61717,#61718,#61719,#61720),.UNSPECIFIED.,.F.,.F.,(4,1,1,
1,1,1,1,1,4),(128.805298797182,128.856261025505,129.852531963299,130.848802901093,
131.845073838887,132.841344776681,133.837615714476,134.83388665227,135.088484104361),
 .UNSPECIFIED.);
#3347=B_SPLINE_CURVE_WITH_KNOTS('',3,(#61725,#61726,#61727,#61728,#61729,
#61730,#61731,#61732,#61733,#61734,#61735),.UNSPECIFIED.,.F.,.F.,(4,1,1,
1,1,1,1,1,4),(122.522113490002,122.611305275793,123.611271694063,124.611238112333,
125.611204530603,126.611170948873,127.611137367143,128.611103785413,128.805298797182),
 .UNSPECIFIED.);
#3348=B_SPLINE_CURVE_WITH_KNOTS('',3,(#61736,#61737,#61738,#61739,#61740,
#61741,#61742,#61743,#61744,#61745),.UNSPECIFIED.,.F.,.F.,(4,1,1,1,1,1,
1,4),(122.522113490002,122.878635398739,123.874906336533,124.871177274328,
125.867448212122,126.863719149916,127.85999008771,128.805298797182),
 .UNSPECIFIED.);
#3349=B_SPLINE_CURVE_WITH_KNOTS('',3,(#61750,#61751,#61752,#61753,#61754,
#61755,#61756,#61757,#61758,#61759),.UNSPECIFIED.,.F.,.F.,(4,1,1,1,1,1,
1,4),(116.238928182823,116.611506766173,117.611473184443,118.611439602713,
119.611406020983,120.611372439253,121.611338857523,122.522113490002),
 .UNSPECIFIED.);
#3350=B_SPLINE_CURVE_WITH_KNOTS('',3,(#61760,#61761,#61762,#61763,#61764,
#61765,#61766,#61767,#61768,#61769),.UNSPECIFIED.,.F.,.F.,(4,1,1,1,1,1,
1,4),(116.238928182823,116.901009771974,117.897280709768,118.893551647562,
119.889822585356,120.886093523151,121.882364460945,122.522113490002),
 .UNSPECIFIED.);
#3351=B_SPLINE_CURVE_WITH_KNOTS('',3,(#61774,#61775,#61776,#61777,#61778,
#61779,#61780,#61781,#61782,#61783),.UNSPECIFIED.,.F.,.F.,(4,1,1,1,1,1,
1,4),(109.955742875643,110.611708256552,111.611674674822,112.611641093093,
113.611607511363,114.611573929633,115.611540347903,116.238928182823),
 .UNSPECIFIED.);
#3352=B_SPLINE_CURVE_WITH_KNOTS('',3,(#61784,#61785,#61786,#61787,#61788,
#61789,#61790,#61791,#61792,#61793),.UNSPECIFIED.,.F.,.F.,(4,1,1,1,1,1,
1,4),(109.955742875643,110.923384145208,111.919655083002,112.915926020797,
113.912196958591,114.908467896385,115.904738834179,116.238928182823),
 .UNSPECIFIED.);
#3353=B_SPLINE_CURVE_WITH_KNOTS('',3,(#61798,#61799,#61800,#61801,#61802,
#61803,#61804,#61805,#61806,#61807),.UNSPECIFIED.,.F.,.F.,(4,1,1,1,1,1,
1,4),(103.672557568463,104.611909746932,105.611876165202,106.611842583472,
107.611809001742,108.611775420012,109.611741838282,109.955742875643),
 .UNSPECIFIED.);
#3354=B_SPLINE_CURVE_WITH_KNOTS('',3,(#61808,#61809,#61810,#61811,#61812,
#61813,#61814,#61815,#61816,#61817,#61818),.UNSPECIFIED.,.F.,.F.,(4,1,1,
1,1,1,1,1,4),(103.672557568464,103.949487580649,104.945758518443,105.942029456237,
106.938300394031,107.934571331825,108.93084226962,109.927113207414,109.955742875643),
 .UNSPECIFIED.);
#3355=B_SPLINE_CURVE_WITH_KNOTS('',3,(#61823,#61824,#61825,#61826,#61827,
#61828,#61829,#61830,#61831,#61832,#61833),.UNSPECIFIED.,.F.,.F.,(4,1,1,
1,1,1,1,1,4),(97.3893722612839,97.612144819042,98.612111237312,99.612077655582,
100.612044073852,101.612010492122,102.611976910392,103.611943328662,103.672557568463),
 .UNSPECIFIED.);
#3356=B_SPLINE_CURVE_WITH_KNOTS('',3,(#61834,#61835,#61836,#61837,#61838,
#61839,#61840,#61841,#61842,#61843),.UNSPECIFIED.,.F.,.F.,(4,1,1,1,1,1,
1,4),(97.389372261284,97.9718619538831,98.9681328916773,99.9644038294716,
100.960674767266,101.95694570506,102.953216642854,103.672557568464),
 .UNSPECIFIED.);
#3357=B_SPLINE_CURVE_WITH_KNOTS('',3,(#61848,#61849,#61850,#61851,#61852,
#61853,#61854,#61855,#61856,#61857),.UNSPECIFIED.,.F.,.F.,(4,1,1,1,1,1,
1,4),(91.1061869541042,91.6123463094217,92.6123127276918,93.6122791459618,
94.6122455642318,95.6122119825019,96.6121784007719,97.3893722612839),
 .UNSPECIFIED.);
#3358=B_SPLINE_CURVE_WITH_KNOTS('',3,(#61858,#61859,#61860,#61861,#61862,
#61863,#61864,#61865,#61866,#61867),.UNSPECIFIED.,.F.,.F.,(4,1,1,1,1,1,
1,4),(91.1061869541043,91.9942363271176,92.9905072649119,93.9867782027061,
94.9830491405003,95.9793200782946,96.9755910160888,97.389372261284),
 .UNSPECIFIED.);
#3359=B_SPLINE_CURVE_WITH_KNOTS('',3,(#61872,#61873,#61874,#61875,#61876,
#61877,#61878,#61879,#61880,#61881),.UNSPECIFIED.,.F.,.F.,(4,1,1,1,1,1,
1,4),(84.8230016469247,85.6125477998015,86.6125142180715,87.6124806363416,
88.6124470546116,89.6124134728817,90.6123798911517,91.1061869541042),
 .UNSPECIFIED.);
#3360=B_SPLINE_CURVE_WITH_KNOTS('',3,(#61882,#61883,#61884,#61885,#61886,
#61887,#61888,#61889,#61890,#61891,#61892),.UNSPECIFIED.,.F.,.F.,(4,1,1,
1,1,1,1,1,4),(84.8230016469248,85.0203397625579,86.0166107003522,87.0128816381464,
88.0091525759407,89.0054235137349,90.0016944515291,90.9979653893234,91.1061869541043),
 .UNSPECIFIED.);
#3361=B_SPLINE_CURVE_WITH_KNOTS('',3,(#61897,#61898,#61899,#61900,#61901,
#61902,#61903,#61904,#61905,#61906,#61907),.UNSPECIFIED.,.F.,.F.,(4,1,1,
1,1,1,1,1,4),(78.5398163397451,78.6127828719112,79.6127492901813,80.6127157084513,
81.6126821267214,82.6126485449914,83.6126149632614,84.6125813815315,84.8230016469247),
 .UNSPECIFIED.);
#3362=B_SPLINE_CURVE_WITH_KNOTS('',3,(#61908,#61909,#61910,#61911,#61912,
#61913,#61914,#61915,#61916,#61917),.UNSPECIFIED.,.F.,.F.,(4,1,1,1,1,1,
1,4),(78.5398163397452,79.0427141357925,80.0389850735867,81.035256011381,
82.0315269491752,83.0277978869695,84.0240688247637,84.8230016469248),
 .UNSPECIFIED.);
#3363=B_SPLINE_CURVE_WITH_KNOTS('',3,(#61922,#61923,#61924,#61925,#61926,
#61927,#61928,#61929,#61930,#61931),.UNSPECIFIED.,.F.,.F.,(4,1,1,1,1,1,
1,4),(72.2566310325655,72.612984362291,73.612950780561,74.6129171988311,
75.6128836171011,76.6128500353712,77.6128164536412,78.5398163397451),
 .UNSPECIFIED.);
#3364=B_SPLINE_CURVE_WITH_KNOTS('',3,(#61932,#61933,#61934,#61935,#61936,
#61937,#61938,#61939,#61940,#61941),.UNSPECIFIED.,.F.,.F.,(4,1,1,1,1,1,
1,4),(72.2566310325656,73.065088509027,74.0613594468213,75.0576303846155,
76.0539013224098,77.050172260204,78.0464431979982,78.5398163397452),
 .UNSPECIFIED.);
#3365=B_SPLINE_CURVE_WITH_KNOTS('',3,(#61946,#61947,#61948,#61949,#61950,
#61951,#61952,#61953,#61954,#61955),.UNSPECIFIED.,.F.,.F.,(4,1,1,1,1,1,
1,4),(65.9734457253859,66.6131858526708,67.6131522709408,68.6131186892109,
69.6130851074809,70.6130515257509,71.613017944021,72.2566310325655),
 .UNSPECIFIED.);
#3366=B_SPLINE_CURVE_WITH_KNOTS('',3,(#61956,#61957,#61958,#61959,#61960,
#61961,#61962,#61963,#61964,#61965,#61966),.UNSPECIFIED.,.F.,.F.,(4,1,1,
1,1,1,1,1,4),(65.973445725386,66.0911919444674,67.0874628822616,68.0837338200558,
69.0800047578501,70.0762756956443,71.0725466334385,72.0688175712328,72.2566310325656),
 .UNSPECIFIED.);
#3367=B_SPLINE_CURVE_WITH_KNOTS('',3,(#61971,#61972,#61973,#61974,#61975,
#61976,#61977,#61978,#61979,#61980),.UNSPECIFIED.,.F.,.F.,(4,1,1,1,1,1,
1,4),(59.6902604182063,60.6133873430505,61.6133537613206,62.6133201795906,
63.6132865978607,64.6132530161307,65.6132194344007,65.9734457253859),
 .UNSPECIFIED.);
#3368=B_SPLINE_CURVE_WITH_KNOTS('',3,(#61981,#61982,#61983,#61984,#61985,
#61986,#61987,#61988,#61989,#61990),.UNSPECIFIED.,.F.,.F.,(4,1,1,1,1,1,
1,4),(59.6902604182064,60.1135663177019,61.1098372554961,62.1061081932904,
63.1023791310846,64.0986500688789,65.0949210066731,65.973445725386),
 .UNSPECIFIED.);
#3369=B_SPLINE_CURVE_WITH_KNOTS('',3,(#61995,#61996,#61997,#61998,#61999,
#62000,#62001,#62002,#62003,#62004,#62005),.UNSPECIFIED.,.F.,.F.,(4,1,1,
1,1,1,1,1,4),(53.4070751110267,53.6136224151603,54.6135888334303,55.6135552517004,
56.6135216699704,57.6134880882404,58.6134545065105,59.6134209247805,59.6902604182063),
 .UNSPECIFIED.);
#3370=B_SPLINE_CURVE_WITH_KNOTS('',3,(#62006,#62007,#62008,#62009,#62010,
#62011,#62012,#62013,#62014,#62015),.UNSPECIFIED.,.F.,.F.,(4,1,1,1,1,1,
1,4),(53.4070751110268,54.1359406909365,55.1322116287307,56.1284825665249,
57.1247535043192,58.1210244421134,59.1172953799077,59.6902604182064),
 .UNSPECIFIED.);
#3371=B_SPLINE_CURVE_WITH_KNOTS('',3,(#62020,#62021,#62022,#62023,#62024,
#62025,#62026,#62027,#62028,#62029),.UNSPECIFIED.,.F.,.F.,(4,1,1,1,1,1,
1,4),(47.1238898038471,47.6138239055401,48.6137903238101,49.6137567420801,
50.6137231603502,51.6136895786202,52.6136559968902,53.4070751110267),
 .UNSPECIFIED.);
#3372=B_SPLINE_CURVE_WITH_KNOTS('',3,(#62030,#62031,#62032,#62033,#62034,
#62035,#62036,#62037,#62038,#62039,#62040),.UNSPECIFIED.,.F.,.F.,(4,1,1,
1,1,1,1,1,4),(47.1238898038472,47.1620441263768,48.158315064171,49.1545860019653,
50.1508569397595,51.1471278775537,52.143398815348,53.1396697531422,53.4070751110268),
 .UNSPECIFIED.);
#3373=B_SPLINE_CURVE_WITH_KNOTS('',3,(#62045,#62046,#62047,#62048,#62049,
#62050,#62051,#62052,#62053,#62054),.UNSPECIFIED.,.F.,.F.,(4,1,1,1,1,1,
1,4),(40.8407044966675,41.6140253959198,42.6139918141899,43.6139582324599,
44.6139246507299,45.613891069,46.61385748727,47.1238898038471),
 .UNSPECIFIED.);
#3374=B_SPLINE_CURVE_WITH_KNOTS('',3,(#62055,#62056,#62057,#62058,#62059,
#62060,#62061,#62062,#62063,#62064),.UNSPECIFIED.,.F.,.F.,(4,1,1,1,1,1,
1,4),(40.8407044966676,41.1844184996113,42.1806894374056,43.1769603751998,
44.1732313129941,45.1695022507883,46.1657731885825,47.1238898038472),
 .UNSPECIFIED.);
#3375=B_SPLINE_CURVE_WITH_KNOTS('',3,(#62069,#62070,#62071,#62072,#62073,
#62074,#62075,#62076,#62077,#62078,#62079),.UNSPECIFIED.,.F.,.F.,(4,1,1,
1,1,1,1,1,4),(34.5575191894879,34.6142604680296,35.6142268862996,36.6141933045696,
37.6141597228397,38.6141261411097,39.6140925593798,40.6140589776498,40.8407044966675),
 .UNSPECIFIED.);
#3376=B_SPLINE_CURVE_WITH_KNOTS('',3,(#62080,#62081,#62082,#62083,#62084,
#62085,#62086,#62087,#62088,#62089),.UNSPECIFIED.,.F.,.F.,(4,1,1,1,1,1,
1,4),(34.557519189488,35.2067928728459,36.2030638106401,37.1993347484344,
38.1956056862286,39.1918766240228,40.1881475618171,40.8407044966676),
 .UNSPECIFIED.);
#3377=B_SPLINE_CURVE_WITH_KNOTS('',3,(#62094,#62095,#62096,#62097,#62098,
#62099,#62100,#62101,#62102,#62103),.UNSPECIFIED.,.F.,.F.,(4,1,1,1,1,1,
1,4),(28.2743338823083,28.6144619584093,29.6144283766794,30.6143947949494,
31.6143612132194,32.6143276314895,33.6142940497595,34.5575191894879),
 .UNSPECIFIED.);
#3378=B_SPLINE_CURVE_WITH_KNOTS('',3,(#62104,#62105,#62106,#62107,#62108,
#62109,#62110,#62111,#62112,#62113),.UNSPECIFIED.,.F.,.F.,(4,1,1,1,1,1,
1,4),(28.2743338823084,29.2291672460804,30.2254381838747,31.2217091216689,
32.2179800594632,33.2142509972574,34.2105219350516,34.557519189488),
 .UNSPECIFIED.);
#3379=B_SPLINE_CURVE_WITH_KNOTS('',3,(#62118,#62119,#62120,#62121,#62122,
#62123,#62124,#62125,#62126,#62127),.UNSPECIFIED.,.F.,.F.,(4,1,1,1,1,1,
1,4),(21.9911485751287,22.6146634487891,23.6146298670591,24.6145962853292,
25.6145627035992,26.6145291218693,27.6144955401393,28.2743338823083),
 .UNSPECIFIED.);
#3380=B_SPLINE_CURVE_WITH_KNOTS('',3,(#62128,#62129,#62130,#62131,#62132,
#62133,#62134,#62135,#62136,#62137,#62138),.UNSPECIFIED.,.F.,.F.,(4,1,1,
1,1,1,1,1,4),(21.9911485751289,22.2552706815207,23.251541619315,24.2478125571092,
25.2440834949035,26.2403544326977,27.236625370492,28.2328963082862,28.2743338823084),
 .UNSPECIFIED.);
#3381=B_SPLINE_CURVE_WITH_KNOTS('',3,(#62143,#62144,#62145,#62146,#62147,
#62148,#62149,#62150,#62151,#62152),.UNSPECIFIED.,.F.,.F.,(4,1,1,1,1,1,
1,4),(15.7079632679492,16.6148649391689,17.6148313574389,18.614797775709,
19.614764193979,20.614730612249,21.6146970305191,21.9911485751287),
 .UNSPECIFIED.);
#3382=B_SPLINE_CURVE_WITH_KNOTS('',3,(#62153,#62154,#62155,#62156,#62157,
#62158,#62159,#62160,#62161,#62162),.UNSPECIFIED.,.F.,.F.,(4,1,1,1,1,1,
1,4),(15.7079632679493,16.2776450547553,17.2739159925495,18.2701869303438,
19.266457868138,20.2627288059323,21.2589997437265,21.9911485751289),
 .UNSPECIFIED.);
#3383=B_SPLINE_CURVE_WITH_KNOTS('',3,(#62165,#62166,#62167,#62168,#62169,
#62170,#62171,#62172,#62173,#62174,#62175,#62176,#62177,#62178,#62179,#62180,
#62181,#62182,#62183,#62184,#62185,#62186,#62187,#62188,#62189,#62190,#62191,
#62192,#62193,#62194,#62195,#62196,#62197,#62198,#62199,#62200,#62201,#62202,
#62203,#62204,#62205,#62206,#62207,#62208,#62209,#62210,#62211,#62212,#62213,
#62214,#62215,#62216,#62217,#62218,#62219,#62220,#62221,#62222,#62223,#62224,
#62225,#62226,#62227,#62228,#62229,#62230,#62231,#62232,#62233,#62234,#62235,
#62236,#62237,#62238,#62239,#62240,#62241,#62242,#62243,#62244,#62245,#62246,
#62247,#62248,#62249,#62250,#62251,#62252,#62253,#62254,#62255,#62256,#62257,
#62258,#62259,#62260,#62261,#62262,#62263,#62264,#62265,#62266,#62267,#62268,
#62269,#62270,#62271,#62272,#62273,#62274,#62275,#62276,#62277,#62278,#62279,
#62280,#62281,#62282,#62283,#62284,#62285,#62286,#62287,#62288,#62289,#62290,
#62291,#62292,#62293,#62294,#62295,#62296,#62297,#62298,#62299,#62300,#62301,
#62302,#62303,#62304,#62305,#62306,#62307,#62308,#62309,#62310,#62311,#62312,
#62313,#62314,#62315,#62316,#62317,#62318,#62319,#62320,#62321,#62322,#62323,
#62324,#62325,#62326,#62327,#62328,#62329,#62330,#62331,#62332,#62333,#62334,
#62335,#62336,#62337,#62338,#62339,#62340,#62341,#62342,#62343,#62344,#62345,
#62346,#62347,#62348,#62349,#62350,#62351,#62352,#62353,#62354,#62355,#62356,
#62357,#62358,#62359,#62360,#62361,#62362,#62363,#62364,#62365,#62366,#62367,
#62368,#62369,#62370,#62371,#62372,#62373,#62374,#62375,#62376,#62377,#62378,
#62379,#62380,#62381,#62382,#62383,#62384,#62385,#62386,#62387,#62388,#62389,
#62390),.UNSPECIFIED.,.F.,.F.,(4,3,3,3,3,3,3,3,3,3,3,3,3,3,3,3,3,3,3,3,
3,3,3,3,3,3,3,3,3,3,3,3,3,3,3,3,3,3,3,3,3,3,3,3,3,3,3,3,3,3,3,3,3,3,3,3,
3,3,3,3,3,3,3,3,3,3,3,3,3,3,3,3,3,3,3,4),(-1.5115530493712,-1.48679646988231,
-1.46138327157041,-1.44931403653187,-1.44201521738479,-1.4372364069369,
-1.41130073666512,-1.3851364793294,-1.36882167524197,-1.36489335463821,
-1.33844118737752,-1.31212405971847,-1.29019978533613,-1.27923764814496,
-1.27341919949145,-1.26903466137048,-1.26827551095379,-1.24293973226305,
-1.21686129007046,-1.19161648481995,-1.18057188252285,-1.17415589095891,
-1.17024744553752,-1.14344439633044,-1.11634682592921,-1.0909858314635,
-1.08147545853886,-1.07621433222182,-1.07212128966627,-1.04351206886633,
-1.0165509628589,-1.01490284806638,-0.988030199407108,-0.977552081199909,
-0.973437277723626,-0.945726987414166,-0.918214262331309,-0.890537857808272,
-0.880398328972147,-0.87237005911237,-0.867956987444107,-0.838906479395067,
-0.811044859415748,-0.783625034708112,-0.772915569760388,-0.768645334133187,
-0.764137890402299,-0.751754955247948,-0.724693670921933,-0.696925419694083,
-0.669642708112985,-0.663192181598675,-0.658947817948324,-0.630700019923219,
-0.602103353566958,-0.573605985023947,-0.561738202776617,-0.556716888407782,
-0.552057825803808,-0.523179250890329,-0.494755452697743,-0.478663727045304,
-0.462934741526935,-0.451680956559048,-0.447722787491454,-0.419466033709138,
-0.390586852248759,-0.36140366189149,-0.344603198998977,-0.339184578268993,
-0.335360215694789,-0.305911623051275,-0.276431237914502,-0.247572950493138,
-0.22699995875139,-0.219677966287888),.UNSPECIFIED.);
#3384=B_SPLINE_CURVE_WITH_KNOTS('',3,(#62392,#62393,#62394,#62395,#62396,
#62397,#62398,#62399,#62400,#62401,#62402,#62403,#62404,#62405,#62406,#62407,
#62408,#62409,#62410,#62411,#62412,#62413,#62414,#62415,#62416,#62417,#62418,
#62419,#62420,#62421,#62422,#62423,#62424,#62425,#62426,#62427,#62428,#62429,
#62430,#62431,#62432,#62433,#62434,#62435,#62436,#62437,#62438,#62439,#62440,
#62441,#62442,#62443,#62444,#62445,#62446,#62447,#62448,#62449,#62450,#62451,
#62452,#62453,#62454,#62455),.UNSPECIFIED.,.F.,.F.,(4,3,3,3,3,3,3,3,3,3,
3,3,3,3,3,3,3,3,3,3,3,4),(-0.410648750432358,-0.381299282375245,-0.351451987365484,
-0.32338277226279,-0.31441918992071,-0.307886057995154,-0.302748807341755,
-0.275195476204274,-0.2619101023362,-0.23366962500355,-0.204460921878106,
-0.199264215741705,-0.195568173418504,-0.168370897549803,-0.141281081328714,
-0.114654976955625,-0.100323104836172,-0.0960558144650962,-0.0702818786829607,
-0.044890002900036,-0.02024436392036,0.),.UNSPECIFIED.);
#3385=B_SPLINE_CURVE_WITH_KNOTS('',3,(#62458,#62459,#62460,#62461,#62462,
#62463,#62464,#62465,#62466,#62467,#62468,#62469,#62470,#62471,#62472,#62473,
#62474,#62475,#62476,#62477,#62478,#62479,#62480,#62481,#62482,#62483,#62484,
#62485,#62486,#62487,#62488),.UNSPECIFIED.,.F.,.F.,(4,3,3,3,3,3,3,3,3,3,
4),(-0.219677966287888,-0.195864471024291,-0.166952662475248,-0.137468548387315,
-0.120284979838901,-0.114251963704818,-0.109988263453048,-0.080302546936133,
-0.0502597344232586,-0.0203206940376301,0.),.UNSPECIFIED.);
#3386=B_SPLINE_CURVE_WITH_KNOTS('',3,(#63501,#63502,#63503,#63504,#63505,
#63506,#63507,#63508),.UNSPECIFIED.,.F.,.F.,(4,1,1,1,1,4),(11.6150328478187,
12.6149992660887,13.6149656843588,14.6149321026288,15.6148985208988,15.7079632679492),
 .UNSPECIFIED.);
#3387=B_SPLINE_CURVE_WITH_KNOTS('',3,(#63509,#63510,#63511,#63512,#63513,
#63514,#63515,#63516,#63517,#63518,#63519,#63520,#63521,#63522,#63523,#63524,
#63525,#63526,#63527,#63528,#63529,#63530,#63531,#63532,#63533,#63534,#63535,
#63536,#63537,#63538,#63539,#63540,#63541,#63542,#63543,#63544,#63545,#63546,
#63547,#63548,#63549,#63550,#63551,#63552,#63553,#63554,#63555,#63556,#63557,
#63558,#63559,#63560,#63561,#63562,#63563,#63564,#63565,#63566,#63567,#63568,
#63569,#63570,#63571,#63572,#63573,#63574,#63575,#63576,#63577,#63578,#63579,
#63580,#63581,#63582,#63583,#63584,#63585,#63586,#63587,#63588,#63589,#63590,
#63591,#63592,#63593,#63594,#63595,#63596,#63597,#63598,#63599,#63600,#63601,
#63602),.UNSPECIFIED.,.F.,.F.,(4,3,3,3,3,3,3,3,3,3,3,3,3,3,3,3,3,3,3,3,
3,3,3,3,3,3,3,3,3,3,3,4),(-0.552745378375066,-0.53257041253064,-0.503209833963106,
-0.487569744740098,-0.475817235384553,-0.470703937755808,-0.441646149367916,
-0.418061431496298,-0.407743117427465,-0.402003725693741,-0.397456462704961,
-0.369148821319412,-0.340103717588302,-0.312985901936444,-0.297779959016177,
-0.291309037186587,-0.264507979745426,-0.252968406394974,-0.225608178960633,
-0.197407156590554,-0.192288000083304,-0.188202033999832,-0.161559009732277,
-0.134959874297392,-0.108788470827791,-0.0997870868716052,-0.094523571416419,
-0.0902265394264102,-0.064682595398749,-0.0395411867789222,-0.0151843303020833,
0.),.UNSPECIFIED.);
#3388=B_SPLINE_CURVE_WITH_KNOTS('',3,(#63603,#63604,#63605,#63606,#63607,
#63608,#63609,#63610,#63611,#63612,#63613,#63614,#63615,#63616,#63617,#63618,
#63619,#63620,#63621),.UNSPECIFIED.,.F.,.F.,(4,3,3,3,3,3,4),(-247.477289902729,
-246.991705312699,-245.991738894429,-244.991772476159,-243.991806057889,
-242.991839639619,-242.853972092955),.UNSPECIFIED.);
#3389=B_SPLINE_CURVE_WITH_KNOTS('',3,(#63624,#63625,#63626,#63627,#63628,
#63629,#63630,#63631,#63632),.UNSPECIFIED.,.F.,.F.,(4,1,1,1,1,1,4),(10.3761157273106,
11.2962903657841,12.2925613035783,13.2888322413726,14.2851031791668,15.2813741169611,
15.7079632679493),.UNSPECIFIED.);
#3390=B_SPLINE_CURVE_WITH_KNOTS('',3,(#64654,#64655,#64656,#64657,#64658,
#64659,#64660,#64661,#64662,#64663,#64664,#64665,#64666,#64667,#64668,#64669,
#64670,#64671,#64672,#64673,#64674,#64675),.UNSPECIFIED.,.F.,.F.,(4,3,3,
3,3,3,3,4),(239.878342081193,240.101296008412,241.097566946206,242.093837884001,
243.090108821795,244.086379759589,245.082650697383,245.40865172782),
 .UNSPECIFIED.);
#3391=B_SPLINE_CURVE_WITH_KNOTS('',3,(#64676,#64677,#64678,#64679,#64680,
#64681,#64682,#64683,#64684,#64685,#64686,#64687,#64688,#64689,#64690,#64691,
#64692,#64693,#64694,#64695,#64696,#64697,#64698,#64699,#64700,#64701,#64702,
#64703,#64704,#64705,#64706,#64707,#64708,#64709,#64710,#64711,#64712,#64713,
#64714,#64715,#64716,#64717,#64718,#64719,#64720,#64721,#64722,#64723,#64724,
#64725,#64726,#64727,#64728,#64729,#64730,#64731,#64732,#64733,#64734,#64735,
#64736,#64737,#64738,#64739,#64740,#64741,#64742,#64743,#64744,#64745,#64746,
#64747,#64748,#64749,#64750,#64751,#64752,#64753,#64754,#64755,#64756,#64757,
#64758,#64759,#64760,#64761,#64762,#64763,#64764,#64765,#64766),
 .UNSPECIFIED.,.F.,.F.,(4,3,3,3,3,3,3,3,3,3,3,3,3,3,3,3,3,3,3,3,3,3,3,3,
3,3,3,3,3,3,4),(-0.555272788399356,-0.536933533817927,-0.512218003438917,
-0.497827681018193,-0.492206798870043,-0.487869646287534,-0.462091513356309,
-0.439576679775185,-0.428764166378627,-0.422010894528083,-0.395425506675213,
-0.367062341183239,-0.345789967064259,-0.329835686475024,-0.325431154183988,
-0.320888849595204,-0.292973404720077,-0.281972844707319,-0.255027785728263,
-0.227542539987006,-0.221779606338387,-0.218030423923514,-0.190105025722723,
-0.161634029602592,-0.13290803371308,-0.116294529498945,-0.111891296080701,
-0.0824377575584239,-0.0528856925172319,-0.0238818739582312,0.),
 .UNSPECIFIED.);
#3392=B_SPLINE_CURVE_WITH_KNOTS('',3,(#64835,#64836,#64837,#64838,#64839,
#64840,#64841,#64842,#64843,#64844),.UNSPECIFIED.,.F.,.F.,(4,3,3,4),(-4.09274904019422,
-3.99884532416016,-2.99913399312012,-2.06120159751576),.UNSPECIFIED.);
#3393=B_SPLINE_CURVE_WITH_KNOTS('',3,(#64847,#64848,#64849,#64850,#64851,
#64852,#64853),.UNSPECIFIED.,.F.,.F.,(4,3,4),(0.,0.995090974411437,1.11004521091154),
 .UNSPECIFIED.);
#3394=B_SPLINE_CURVE_WITH_KNOTS('',3,(#64858,#64859,#64860,#64861,#64862,
#64863,#64864,#64865,#64866,#64867,#64868,#64869,#64870,#64871,#64872,#64873,
#64874,#64875,#64876,#64877,#64878,#64879),.UNSPECIFIED.,.F.,.F.,(4,3,3,
3,3,3,3,4),(-10.3759343473738,-9.99711331040039,-8.99740197936035,-7.99769064832031,
-6.99797931728027,-5.99826798624023,-4.99855665520019,-4.09274904019422),
 .UNSPECIFIED.);
#3395=B_SPLINE_CURVE_WITH_KNOTS('',3,(#64880,#64881,#64882,#64883,#64884,
#64885,#64886,#64887,#64888,#64889,#64890,#64891,#64892,#64893,#64894,#64895,
#64896,#64897,#64898,#64899,#64900,#64901),.UNSPECIFIED.,.F.,.F.,(4,3,3,
3,3,3,3,4),(1.11004521091154,1.99018194882289,2.98527292323434,3.98036389764579,
4.97545487205724,5.97054584646869,6.96563682088014,7.39323051809113),
 .UNSPECIFIED.);
#3396=B_SPLINE_CURVE_WITH_KNOTS('',3,(#64906,#64907,#64908,#64909,#64910,
#64911,#64912,#64913,#64914,#64915,#64916,#64917,#64918,#64919,#64920,#64921,
#64922,#64923,#64924,#64925,#64926,#64927),.UNSPECIFIED.,.F.,.F.,(4,3,3,
3,3,3,3,4),(-16.6591196545534,-15.9953812966406,-14.9956699656006,-13.9959586345605,
-12.9962473035205,-11.9965359724805,-10.9968246414404,-10.3759343473738),
 .UNSPECIFIED.);
#3397=B_SPLINE_CURVE_WITH_KNOTS('',3,(#64928,#64929,#64930,#64931,#64932,
#64933,#64934,#64935,#64936,#64937,#64938,#64939,#64940,#64941,#64942,#64943,
#64944,#64945,#64946,#64947,#64948,#64949),.UNSPECIFIED.,.F.,.F.,(4,3,3,
3,3,3,3,4),(7.39323051809113,7.96072779529158,8.95581876970303,9.95090974411446,
10.9460007185259,11.9410916929373,12.9361826673488,13.6764158252707),
 .UNSPECIFIED.);
#3398=B_SPLINE_CURVE_WITH_KNOTS('',3,(#64954,#64955,#64956,#64957,#64958,
#64959,#64960,#64961,#64962,#64963,#64964,#64965,#64966,#64967,#64968,#64969,
#64970,#64971,#64972,#64973,#64974,#64975),.UNSPECIFIED.,.F.,.F.,(4,3,3,
3,3,3,3,4),(-22.942304961733,-21.9936492828808,-20.9939379518408,-19.9942266208008,
-18.9945152897607,-17.9948039587207,-16.9950926276807,-16.6591196545534),
 .UNSPECIFIED.);
#3399=B_SPLINE_CURVE_WITH_KNOTS('',3,(#64976,#64977,#64978,#64979,#64980,
#64981,#64982,#64983,#64984,#64985,#64986,#64987,#64988,#64989,#64990,#64991,
#64992,#64993,#64994,#64995,#64996,#64997,#64998,#64999,#65000),
 .UNSPECIFIED.,.F.,.F.,(4,3,3,3,3,3,3,3,4),(13.6764158252707,13.9312736417602,
14.9263646161717,15.9214555905831,16.9165465649946,17.911637539406,18.9067285138175,
19.9018194882289,19.9596011324503),.UNSPECIFIED.);
#3400=B_SPLINE_CURVE_WITH_KNOTS('',3,(#65005,#65006,#65007,#65008,#65009,
#65010,#65011,#65012,#65013,#65014,#65015,#65016,#65017,#65018,#65019,#65020,
#65021,#65022,#65023,#65024,#65025,#65026,#65027,#65028,#65029),
 .UNSPECIFIED.,.F.,.F.,(4,3,3,3,3,3,3,3,4),(-29.2254902689126,-28.9916286001611,
-27.9919172691211,-26.992205938081,-25.992494607041,-24.992783276001,-23.9930719449609,
-22.9933606139209,-22.942304961733),.UNSPECIFIED.);
#3401=B_SPLINE_CURVE_WITH_KNOTS('',3,(#65030,#65031,#65032,#65033,#65034,
#65035,#65036,#65037,#65038,#65039,#65040,#65041,#65042,#65043,#65044,#65045,
#65046,#65047,#65048,#65049,#65050,#65051),.UNSPECIFIED.,.F.,.F.,(4,3,3,
3,3,3,3,4),(19.9596011324503,20.8969104626403,21.8920014370518,22.8870924114632,
23.8821833858747,24.8772743602861,25.8723653346976,26.2427864396299),
 .UNSPECIFIED.);
#3402=B_SPLINE_CURVE_WITH_KNOTS('',3,(#65056,#65057,#65058,#65059,#65060,
#65061,#65062,#65063,#65064,#65065,#65066,#65067,#65068,#65069,#65070,#65071,
#65072,#65073,#65074,#65075,#65076,#65077),.UNSPECIFIED.,.F.,.F.,(4,3,3,
3,3,3,3,4),(-35.5086755760921,-34.9898965864014,-33.9901852553613,-32.9904739243213,
-31.9907625932812,-30.9910512622412,-29.9913399312012,-29.2254902689126),
 .UNSPECIFIED.);
#3403=B_SPLINE_CURVE_WITH_KNOTS('',3,(#65078,#65079,#65080,#65081,#65082,
#65083,#65084,#65085,#65086,#65087,#65088,#65089,#65090,#65091,#65092,#65093,
#65094,#65095,#65096,#65097,#65098,#65099),.UNSPECIFIED.,.F.,.F.,(4,3,3,
3,3,3,3,4),(26.2427864396299,26.867456309109,27.8625472835205,28.8576382579319,
29.8527292323434,30.8478202067548,31.8429111811663,32.5259717468095),
 .UNSPECIFIED.);
#3404=B_SPLINE_CURVE_WITH_KNOTS('',3,(#65104,#65105,#65106,#65107,#65108,
#65109,#65110,#65111,#65112,#65113,#65114,#65115,#65116,#65117,#65118,#65119,
#65120,#65121,#65122,#65123,#65124,#65125),.UNSPECIFIED.,.F.,.F.,(4,3,3,
3,3,3,3,4),(-41.7918608832717,-40.9881645726416,-39.9884532416015,-38.9887419105615,
-37.9890305795215,-36.9893192484814,-35.9896079174414,-35.5086755760921),
 .UNSPECIFIED.);
#3405=B_SPLINE_CURVE_WITH_KNOTS('',3,(#65126,#65127,#65128,#65129,#65130,
#65131,#65132,#65133,#65134,#65135,#65136,#65137,#65138,#65139,#65140,#65141,
#65142,#65143,#65144,#65145,#65146,#65147),.UNSPECIFIED.,.F.,.F.,(4,3,3,
3,3,3,3,4),(32.5259717468095,32.8380021555777,33.8330931299892,34.8281841044006,
35.823275078812,36.8183660532235,37.8134570276349,38.8091570539891),
 .UNSPECIFIED.);
#3406=B_SPLINE_CURVE_WITH_KNOTS('',3,(#65152,#65153,#65154,#65155,#65156,
#65157,#65158,#65159,#65160,#65161,#65162,#65163,#65164,#65165,#65166,#65167,
#65168,#65169,#65170,#65171,#65172,#65173,#65174,#65175,#65176),
 .UNSPECIFIED.,.F.,.F.,(4,3,3,3,3,3,3,3,4),(-48.0750461904513,-47.9861438899218,
-46.9864325588818,-45.9867212278418,-44.9870098968017,-43.9872985657617,
-42.9875872347217,-41.9878759036816,-41.7918608832717),.UNSPECIFIED.);
#3407=B_SPLINE_CURVE_WITH_KNOTS('',3,(#65177,#65178,#65179,#65180,#65181,
#65182,#65183,#65184,#65185,#65186,#65187,#65188,#65189,#65190,#65191,#65192,
#65193,#65194,#65195,#65196,#65197,#65198),.UNSPECIFIED.,.F.,.F.,(4,3,3,
3,3,3,3,4),(38.8091570539891,39.8036389764578,40.7987299508693,41.7938209252807,
42.7889118996922,43.7840028741036,44.7790938485151,45.0923423611687),
 .UNSPECIFIED.);
#3408=B_SPLINE_CURVE_WITH_KNOTS('',3,(#65203,#65204,#65205,#65206,#65207,
#65208,#65209,#65210,#65211,#65212,#65213,#65214,#65215,#65216,#65217,#65218,
#65219,#65220,#65221,#65222,#65223,#65224),.UNSPECIFIED.,.F.,.F.,(4,3,3,
3,3,3,3,4),(-54.3582314976309,-53.9844118761621,-52.9847005451221,-51.984989214082,
-50.985277883042,-49.9855665520019,-48.9858552209619,-48.0750461904513),
 .UNSPECIFIED.);
#3409=B_SPLINE_CURVE_WITH_KNOTS('',3,(#65225,#65226,#65227,#65228,#65229,
#65230,#65231,#65232,#65233,#65234,#65235,#65236,#65237,#65238,#65239,#65240,
#65241,#65242,#65243,#65244,#65245,#65246),.UNSPECIFIED.,.F.,.F.,(4,3,3,
3,3,3,3,4),(45.0923423611687,45.7741848229265,46.769275797338,47.7643667717494,
48.7594577461608,49.7545487205723,50.7496396949837,51.3755276683482),
 .UNSPECIFIED.);
#3410=B_SPLINE_CURVE_WITH_KNOTS('',3,(#65251,#65252,#65253,#65254,#65255,
#65256,#65257,#65258,#65259,#65260,#65261,#65262,#65263,#65264,#65265,#65266,
#65267,#65268,#65269,#65270,#65271,#65272),.UNSPECIFIED.,.F.,.F.,(4,3,3,
3,3,3,3,4),(-60.6414168048105,-59.9826798624023,-58.9829685313623,-57.9832572003222,
-56.9835458692822,-55.9838345382421,-54.9841232072021,-54.3582314976309),
 .UNSPECIFIED.);
#3411=B_SPLINE_CURVE_WITH_KNOTS('',3,(#65273,#65274,#65275,#65276,#65277,
#65278,#65279,#65280,#65281,#65282,#65283,#65284,#65285,#65286,#65287,#65288,
#65289,#65290,#65291,#65292,#65293,#65294),.UNSPECIFIED.,.F.,.F.,(4,3,3,
3,3,3,3,4),(51.3755276683482,51.7447306693952,52.7398216438066,53.7349126182181,
54.7300035926295,55.725094567041,56.7201855414524,57.6587129755278),
 .UNSPECIFIED.);
#3412=B_SPLINE_CURVE_WITH_KNOTS('',3,(#65299,#65300,#65301,#65302,#65303,
#65304,#65305,#65306,#65307,#65308,#65309,#65310,#65311,#65312,#65313,#65314,
#65315,#65316,#65317,#65318,#65319,#65320),.UNSPECIFIED.,.F.,.F.,(4,3,3,
3,3,3,3,4),(-66.9246021119901,-65.9809478486425,-64.9812365176025,-63.9815251865625,
-62.9818138555224,-61.9821025244824,-60.9823911934423,-60.6414168048105),
 .UNSPECIFIED.);
#3413=B_SPLINE_CURVE_WITH_KNOTS('',3,(#65321,#65322,#65323,#65324,#65325,
#65326,#65327,#65328,#65329,#65330,#65331,#65332,#65333,#65334,#65335,#65336,
#65337,#65338,#65339,#65340,#65341,#65342,#65343,#65344,#65345),
 .UNSPECIFIED.,.F.,.F.,(4,3,3,3,3,3,3,3,4),(57.6587129755278,57.7152765158638,
58.7103674902753,59.7054584646867,60.7005494390982,61.6956404135096,62.690731387921,
63.6858223623325,63.9418982827074),.UNSPECIFIED.);
#3414=B_SPLINE_CURVE_WITH_KNOTS('',3,(#65350,#65351,#65352,#65353,#65354,
#65355,#65356,#65357,#65358,#65359,#65360,#65361,#65362,#65363,#65364,#65365,
#65366,#65367,#65368,#65369,#65370,#65371,#65372,#65373,#65374),
 .UNSPECIFIED.,.F.,.F.,(4,3,3,3,3,3,3,3,4),(-73.2077874191697,-72.9789271659228,
-71.9792158348828,-70.9795045038427,-69.9797931728027,-68.9800818417627,
-67.9803705107226,-66.9806591796826,-66.9246021119901),.UNSPECIFIED.);
#3415=B_SPLINE_CURVE_WITH_KNOTS('',3,(#65375,#65376,#65377,#65378,#65379,
#65380,#65381,#65382,#65383,#65384,#65385,#65386,#65387,#65388,#65389,#65390,
#65391,#65392,#65393,#65394,#65395,#65396),.UNSPECIFIED.,.F.,.F.,(4,3,3,
3,3,3,3,4),(63.9418982827074,64.6809133367439,65.6760043111554,66.6710952855668,
67.6661862599783,68.6612772343897,69.6563682088012,70.225083589887),
 .UNSPECIFIED.);
#3416=B_SPLINE_CURVE_WITH_KNOTS('',3,(#65401,#65402,#65403,#65404,#65405,
#65406,#65407,#65408,#65409,#65410,#65411,#65412,#65413,#65414,#65415,#65416,
#65417,#65418,#65419,#65420,#65421,#65422),.UNSPECIFIED.,.F.,.F.,(4,3,3,
3,3,3,3,4),(-79.4909727263493,-78.977195152163,-77.977483821123,-76.977772490083,
-75.9780611590429,-74.9783498280029,-73.9786384969629,-73.2077874191697),
 .UNSPECIFIED.);
#3417=B_SPLINE_CURVE_WITH_KNOTS('',3,(#65423,#65424,#65425,#65426,#65427,
#65428,#65429,#65430,#65431,#65432,#65433,#65434,#65435,#65436,#65437,#65438,
#65439,#65440,#65441,#65442,#65443,#65444),.UNSPECIFIED.,.F.,.F.,(4,3,3,
3,3,3,3,4),(70.225083589887,70.6514591832126,71.646550157624,72.6416411320355,
73.6367321064469,74.6318230808584,75.6269140552698,76.5082688970666),
 .UNSPECIFIED.);
#3418=B_SPLINE_CURVE_WITH_KNOTS('',3,(#65449,#65450,#65451,#65452,#65453,
#65454,#65455,#65456,#65457,#65458,#65459,#65460,#65461,#65462,#65463,#65464,
#65465,#65466,#65467,#65468,#65469,#65470),.UNSPECIFIED.,.F.,.F.,(4,3,3,
3,3,3,3,4),(-85.7741580335289,-84.9754631384033,-83.9757518073632,-82.9760404763232,
-81.9763291452832,-80.9766178142431,-79.9769064832031,-79.4909727263493),
 .UNSPECIFIED.);
#3419=B_SPLINE_CURVE_WITH_KNOTS('',3,(#65471,#65472,#65473,#65474,#65475,
#65476,#65477,#65478,#65479,#65480,#65481,#65482,#65483,#65484,#65485,#65486,
#65487,#65488,#65489,#65490,#65491,#65492,#65493,#65494,#65495),
 .UNSPECIFIED.,.F.,.F.,(4,3,3,3,3,3,3,3,4),(76.5082688970666,76.6220050296813,
77.6170960040927,78.6121869785042,79.6072779529156,80.6023689273271,81.5974599017385,
82.59255087615,82.7914542042462),.UNSPECIFIED.);
#3420=B_SPLINE_CURVE_WITH_KNOTS('',3,(#65500,#65501,#65502,#65503,#65504,
#65505,#65506,#65507,#65508,#65509,#65510,#65511,#65512,#65513,#65514,#65515,
#65516,#65517,#65518,#65519,#65520,#65521,#65522,#65523,#65524),
 .UNSPECIFIED.,.F.,.F.,(4,3,3,3,3,3,3,3,4),(-92.0573433407085,-91.9734424556835,
-90.9737311246435,-89.9740197936035,-88.9743084625634,-87.9745971315234,
-86.9748858004833,-85.9751744694433,-85.7741580335289),.UNSPECIFIED.);
#3421=B_SPLINE_CURVE_WITH_KNOTS('',3,(#65525,#65526,#65527,#65528,#65529,
#65530,#65531,#65532,#65533,#65534,#65535,#65536,#65537,#65538,#65539,#65540,
#65541,#65542,#65543,#65544,#65545,#65546),.UNSPECIFIED.,.F.,.F.,(4,3,3,
3,3,3,3,4),(82.7914542042462,83.5876418505614,84.5827328249729,85.5778237993843,
86.5729147737958,87.5680057482072,88.5630967226186,89.0746395114258),
 .UNSPECIFIED.);
#3422=B_SPLINE_CURVE_WITH_KNOTS('',3,(#65551,#65552,#65553,#65554,#65555,
#65556,#65557,#65558,#65559,#65560,#65561,#65562,#65563,#65564,#65565,#65566,
#65567,#65568,#65569,#65570,#65571,#65572),.UNSPECIFIED.,.F.,.F.,(4,3,3,
3,3,3,3,4),(-98.3405286478881,-97.9717104419238,-96.9719991108837,-95.9722877798437,
-94.9725764488037,-93.9728651177636,-92.9731537867236,-92.0573433407085),
 .UNSPECIFIED.);
#3423=B_SPLINE_CURVE_WITH_KNOTS('',3,(#65573,#65574,#65575,#65576,#65577,
#65578,#65579,#65580,#65581,#65582,#65583,#65584,#65585,#65586,#65587,#65588,
#65589,#65590,#65591,#65592,#65593,#65594),.UNSPECIFIED.,.F.,.F.,(4,3,3,
3,3,3,3,4),(89.0746395114258,89.5581876970301,90.5532786714415,91.548369645853,
92.5434606202644,93.5385515946759,94.5336425690873,95.3578248186054),
 .UNSPECIFIED.);
#3424=B_SPLINE_CURVE_WITH_KNOTS('',3,(#65599,#65600,#65601,#65602,#65603,
#65604,#65605,#65606,#65607,#65608,#65609,#65610,#65611,#65612,#65613,#65614,
#65615,#65616,#65617,#65618,#65619,#65620),.UNSPECIFIED.,.F.,.F.,(4,3,3,
3,3,3,3,4),(-104.623713955068,-103.969978428164,-102.970267097124,-101.970555766084,
-100.970844435044,-99.9711331040039,-98.9714217729638,-98.3405286478881),
 .UNSPECIFIED.);
#3425=B_SPLINE_CURVE_WITH_KNOTS('',3,(#65621,#65622,#65623,#65624,#65625,
#65626,#65627,#65628,#65629,#65630,#65631,#65632,#65633,#65634,#65635,#65636,
#65637,#65638,#65639,#65640,#65641,#65642,#65643,#65644,#65645),
 .UNSPECIFIED.,.F.,.F.,(4,3,3,3,3,3,3,3,4),(95.3578248186054,95.5287335434987,
96.5238245179102,97.5189154923216,98.5140064667331,99.5090974411445,100.504188415556,
101.499279389967,101.641010125785),.UNSPECIFIED.);
#3426=B_SPLINE_CURVE_WITH_KNOTS('',3,(#65650,#65651,#65652,#65653,#65654,
#65655,#65656,#65657,#65658,#65659,#65660,#65661,#65662,#65663,#65664,#65665,
#65666,#65667,#65668,#65669,#65670,#65671),.UNSPECIFIED.,.F.,.F.,(4,3,3,
3,3,3,3,4),(-110.906899262247,-109.968246414404,-108.968535083364,-107.968823752324,
-106.969112421284,-105.969401090244,-104.969689759204,-104.623713955068),
 .UNSPECIFIED.);
#3427=B_SPLINE_CURVE_WITH_KNOTS('',3,(#65672,#65673,#65674,#65675,#65676,
#65677,#65678,#65679,#65680,#65681,#65682,#65683,#65684,#65685,#65686,#65687,
#65688,#65689,#65690,#65691,#65692,#65693),.UNSPECIFIED.,.F.,.F.,(4,3,3,
3,3,3,3,4),(101.641010125785,102.494370364379,103.48946133879,104.484552313202,
105.479643287613,106.474734262025,107.469825236436,107.924195432965),
 .UNSPECIFIED.);
#3428=B_SPLINE_CURVE_WITH_KNOTS('',3,(#65698,#65699,#65700,#65701,#65702,
#65703,#65704,#65705,#65706,#65707,#65708,#65709,#65710,#65711,#65712,#65713,
#65714,#65715,#65716,#65717,#65718,#65719,#65720,#65721,#65722),
 .UNSPECIFIED.,.F.,.F.,(4,3,3,3,3,3,3,3,4),(-117.190084569427,-116.966225731684,
-115.966514400644,-114.966803069604,-113.967091738564,-112.967380407524,
-111.967669076484,-110.967957745444,-110.906899262247),.UNSPECIFIED.);
#3429=B_SPLINE_CURVE_WITH_KNOTS('',3,(#65723,#65724,#65725,#65726,#65727,
#65728,#65729,#65730,#65731,#65732,#65733,#65734,#65735,#65736,#65737,#65738,
#65739,#65740,#65741,#65742,#65743,#65744),.UNSPECIFIED.,.F.,.F.,(4,3,3,
3,3,3,3,4),(107.924195432965,108.464916210848,109.460007185259,110.45509815967,
111.450189134082,112.445280108493,113.440371082905,114.207380740144),
 .UNSPECIFIED.);
#3430=B_SPLINE_CURVE_WITH_KNOTS('',3,(#65749,#65750,#65751,#65752,#65753,
#65754,#65755,#65756,#65757,#65758,#65759,#65760,#65761,#65762,#65763,#65764,
#65765,#65766,#65767,#65768,#65769,#65770),.UNSPECIFIED.,.F.,.F.,(4,3,3,
3,3,3,3,4),(-123.473269876606,-122.964493717925,-121.964782386885,-120.965071055845,
-119.965359724805,-118.965648393765,-117.965937062725,-117.190084569427),
 .UNSPECIFIED.);
#3431=B_SPLINE_CURVE_WITH_KNOTS('',3,(#65771,#65772,#65773,#65774,#65775,
#65776,#65777,#65778,#65779,#65780,#65781,#65782,#65783,#65784,#65785,#65786,
#65787,#65788,#65789,#65790,#65791,#65792,#65793,#65794,#65795),
 .UNSPECIFIED.,.F.,.F.,(4,3,3,3,3,3,3,3,4),(114.207380740144,114.435462057316,
115.430553031728,116.425644006139,117.420734980551,118.415825954962,119.410916929373,
120.406007903785,120.490566047324),.UNSPECIFIED.);
#3432=B_SPLINE_CURVE_WITH_KNOTS('',3,(#65800,#65801,#65802,#65803,#65804,
#65805,#65806,#65807,#65808,#65809,#65810,#65811,#65812,#65813,#65814,#65815,
#65816,#65817,#65818,#65819,#65820,#65821),.UNSPECIFIED.,.F.,.F.,(4,3,3,
3,3,3,3,4),(-129.756455183786,-128.962761704165,-127.963050373125,-126.963339042085,
-125.963627711045,-124.963916380005,-123.964205048965,-123.473269876606),
 .UNSPECIFIED.);
#3433=B_SPLINE_CURVE_WITH_KNOTS('',3,(#65822,#65823,#65824,#65825,#65826,
#65827,#65828,#65829,#65830,#65831,#65832,#65833,#65834,#65835,#65836,#65837,
#65838,#65839,#65840,#65841,#65842,#65843),.UNSPECIFIED.,.F.,.F.,(4,3,3,
3,3,3,3,4),(120.490566047324,121.401098878196,122.396189852608,123.391280827019,
124.386371801431,125.381462775842,126.376553750254,126.773751354503),
 .UNSPECIFIED.);
#3434=B_SPLINE_CURVE_WITH_KNOTS('',3,(#65848,#65849,#65850,#65851,#65852,
#65853,#65854,#65855,#65856,#65857,#65858,#65859,#65860,#65861,#65862,#65863,
#65864,#65865,#65866,#65867,#65868,#65869,#65870,#65871,#65872),
 .UNSPECIFIED.,.F.,.F.,(4,3,3,3,3,3,3,3,4),(-136.039640490966,-135.960741021445,
-134.961029690405,-133.961318359365,-132.961607028325,-131.961895697285,
-130.962184366245,-129.962473035205,-129.756455183786),.UNSPECIFIED.);
#3435=B_SPLINE_CURVE_WITH_KNOTS('',3,(#65873,#65874,#65875,#65876,#65877,
#65878,#65879,#65880,#65881,#65882,#65883,#65884,#65885,#65886,#65887,#65888,
#65889,#65890,#65891,#65892,#65893,#65894),.UNSPECIFIED.,.F.,.F.,(4,3,3,
3,3,3,3,4),(126.773751354503,127.371644724665,128.366735699076,129.361826673488,
130.356917647899,131.352008622311,132.347099596722,133.056936661683),
 .UNSPECIFIED.);
#3436=B_SPLINE_CURVE_WITH_KNOTS('',3,(#65899,#65900,#65901,#65902,#65903,
#65904,#65905,#65906,#65907,#65908,#65909,#65910,#65911,#65912,#65913,#65914,
#65915,#65916,#65917,#65918,#65919,#65920),.UNSPECIFIED.,.F.,.F.,(4,3,3,
3,3,3,3,4),(-142.322825798145,-141.959009007685,-140.959297676645,-139.959586345605,
-138.959875014565,-137.960163683525,-136.960452352485,-136.039640490966),
 .UNSPECIFIED.);
#3437=B_SPLINE_CURVE_WITH_KNOTS('',3,(#65921,#65922,#65923,#65924,#65925,
#65926,#65927,#65928,#65929,#65930,#65931,#65932,#65933,#65934,#65935,#65936,
#65937,#65938,#65939,#65940,#65941,#65942,#65943,#65944,#65945),
 .UNSPECIFIED.,.F.,.F.,(4,3,3,3,3,3,3,3,4),(133.056936661683,133.342190571134,
134.337281545545,135.332372519957,136.327463494368,137.322554468779,138.317645443191,
139.312736417602,139.340121968862),.UNSPECIFIED.);
#3438=B_SPLINE_CURVE_WITH_KNOTS('',3,(#65950,#65951,#65952,#65953,#65954,
#65955,#65956,#65957,#65958,#65959,#65960,#65961,#65962,#65963,#65964,#65965,
#65966,#65967,#65968,#65969,#65970,#65971),.UNSPECIFIED.,.F.,.F.,(4,3,3,
3,3,3,3,4),(-148.606011105325,-147.957276993926,-146.957565662886,-145.957854331846,
-144.958143000806,-143.958431669766,-142.958720338725,-142.322825798145),
 .UNSPECIFIED.);
#3439=B_SPLINE_CURVE_WITH_KNOTS('',3,(#65972,#65973,#65974,#65975,#65976,
#65977,#65978,#65979,#65980,#65981,#65982,#65983,#65984,#65985,#65986,#65987,
#65988,#65989,#65990,#65991,#65992,#65993),.UNSPECIFIED.,.F.,.F.,(4,3,3,
3,3,3,3,4),(139.340121968862,140.307827392014,141.302918366425,142.298009340837,
143.293100315248,144.28819128966,145.283282264071,145.623307276042),
 .UNSPECIFIED.);
#3440=B_SPLINE_CURVE_WITH_KNOTS('',3,(#65998,#65999,#66000,#66001,#66002,
#66003,#66004,#66005,#66006,#66007,#66008,#66009,#66010,#66011,#66012,#66013,
#66014,#66015,#66016,#66017,#66018,#66019),.UNSPECIFIED.,.F.,.F.,(4,3,3,
3,3,3,3,4),(-154.889196412504,-153.955544980166,-152.955833649126,-151.956122318086,
-150.956410987046,-149.956699656006,-148.956988324966,-148.606011105325),
 .UNSPECIFIED.);
#3441=B_SPLINE_CURVE_WITH_KNOTS('',3,(#66020,#66021,#66022,#66023,#66024,
#66025,#66026,#66027,#66028,#66029,#66030,#66031,#66032,#66033,#66034,#66035,
#66036,#66037,#66038,#66039,#66040,#66041),.UNSPECIFIED.,.F.,.F.,(4,3,3,
3,3,3,3,4),(145.623307276042,146.278373238482,147.273464212894,148.268555187305,
149.263646161717,150.258737136128,151.25382811054,151.906492583222),
 .UNSPECIFIED.);
#3442=B_SPLINE_CURVE_WITH_KNOTS('',3,(#66046,#66047,#66048,#66049,#66050,
#66051,#66052,#66053,#66054,#66055,#66056,#66057,#66058,#66059,#66060,#66061,
#66062,#66063,#66064,#66065,#66066,#66067,#66068,#66069,#66070),
 .UNSPECIFIED.,.F.,.F.,(4,3,3,3,3,3,3,3,4),(-161.172381719684,-160.953524297446,
-159.953812966406,-158.954101635366,-157.954390304326,-156.954678973286,
-155.954967642246,-154.955256311206,-154.889196412504),.UNSPECIFIED.);
#3443=B_SPLINE_CURVE_WITH_KNOTS('',3,(#66071,#66072,#66073,#66074,#66075,
#66076,#66077,#66078,#66079,#66080,#66081,#66082,#66083,#66084,#66085,#66086,
#66087,#66088,#66089,#66090,#66091,#66092),.UNSPECIFIED.,.F.,.F.,(4,3,3,
3,3,3,3,4),(151.906492583222,152.248919084951,153.244010059363,154.239101033774,
155.234192008185,156.229282982597,157.224373957008,158.189677890401),
 .UNSPECIFIED.);
#3444=B_SPLINE_CURVE_WITH_KNOTS('',3,(#66097,#66098,#66099,#66100,#66101,
#66102,#66103,#66104,#66105,#66106,#66107,#66108,#66109,#66110,#66111,#66112,
#66113,#66114,#66115,#66116,#66117,#66118),.UNSPECIFIED.,.F.,.F.,(4,3,3,
3,3,3,3,4),(-167.455567026863,-166.951792283686,-165.952080952646,-164.952369621606,
-163.952658290566,-162.952946959526,-161.953235628486,-161.172381719684),
 .UNSPECIFIED.);
#3445=B_SPLINE_CURVE_WITH_KNOTS('',3,(#66119,#66120,#66121,#66122,#66123,
#66124,#66125,#66126,#66127,#66128,#66129,#66130,#66131,#66132,#66133,#66134,
#66135,#66136,#66137,#66138,#66139,#66140,#66141,#66142,#66143),
 .UNSPECIFIED.,.F.,.F.,(4,3,3,3,3,3,3,3,4),(158.189677890401,158.21946493142,
159.214555905831,160.209646880243,161.204737854654,162.199828829066,163.194919803477,
164.190010777888,164.472863197581),.UNSPECIFIED.);
#3446=B_SPLINE_CURVE_WITH_KNOTS('',3,(#66148,#66149,#66150,#66151,#66152,
#66153,#66154,#66155,#66156,#66157,#66158,#66159,#66160,#66161,#66162,#66163,
#66164,#66165,#66166,#66167,#66168,#66169),.UNSPECIFIED.,.F.,.F.,(4,3,3,
3,3,3,3,4),(-173.738752334043,-172.950060269927,-171.950348938887,-170.950637607847,
-169.950926276807,-168.951214945766,-167.951503614726,-167.455567026863),
 .UNSPECIFIED.);
#3447=B_SPLINE_CURVE_WITH_KNOTS('',3,(#66170,#66171,#66172,#66173,#66174,
#66175,#66176,#66177,#66178,#66179,#66180,#66181,#66182,#66183,#66184,#66185,
#66186,#66187,#66188,#66189,#66190,#66191),.UNSPECIFIED.,.F.,.F.,(4,3,3,
3,3,3,3,4),(164.472863197581,165.1851017523,166.180192726711,167.175283701123,
168.170374675534,169.165465649946,170.160556624357,170.75604850476),
 .UNSPECIFIED.);
#3448=B_SPLINE_CURVE_WITH_KNOTS('',3,(#66196,#66197,#66198,#66199,#66200,
#66201,#66202,#66203,#66204,#66205,#66206,#66207,#66208,#66209,#66210,#66211,
#66212,#66213,#66214,#66215,#66216,#66217,#66218,#66219,#66220),
 .UNSPECIFIED.,.F.,.F.,(4,3,3,3,3,3,3,3,4),(-180.021937641223,-179.948039587207,
-178.948328256167,-177.948616925127,-176.948905594087,-175.949194263047,
-174.949482932007,-173.949771600967,-173.738752334043),.UNSPECIFIED.);
#3449=B_SPLINE_CURVE_WITH_KNOTS('',3,(#66221,#66222,#66223,#66224,#66225,
#66226,#66227,#66228,#66229,#66230,#66231,#66232,#66233,#66234,#66235,#66236,
#66237,#66238,#66239,#66240,#66241,#66242),.UNSPECIFIED.,.F.,.F.,(4,3,3,
3,3,3,3,4),(170.75604850476,171.155647598769,172.15073857318,173.145829547591,
174.140920522003,175.136011496414,176.131102470826,177.03923381194),
 .UNSPECIFIED.);
#3450=B_SPLINE_CURVE_WITH_KNOTS('',3,(#66247,#66248,#66249,#66250,#66251,
#66252,#66253,#66254,#66255,#66256,#66257,#66258,#66259,#66260,#66261,#66262,
#66263,#66264,#66265,#66266,#66267,#66268),.UNSPECIFIED.,.F.,.F.,(4,3,3,
3,3,3,3,4),(-186.305122948402,-185.946307573447,-184.946596242407,-183.946884911367,
-182.947173580327,-181.947462249287,-180.947750918247,-180.021937641223),
 .UNSPECIFIED.);
#3451=B_SPLINE_CURVE_WITH_KNOTS('',3,(#66269,#66270,#66271,#66272,#66273,
#66274,#66275,#66276,#66277,#66278,#66279,#66280,#66281,#66282,#66283,#66284,
#66285,#66286,#66287,#66288,#66289,#66290,#66291,#66292,#66293),
 .UNSPECIFIED.,.F.,.F.,(4,3,3,3,3,3,3,3,4),(177.03923381194,177.126193445237,
178.121284419649,179.11637539406,180.111466368472,181.106557342883,182.101648317294,
183.096739291706,183.322419119119),.UNSPECIFIED.);
#3452=B_SPLINE_CURVE_WITH_KNOTS('',3,(#66298,#66299,#66300,#66301,#66302,
#66303,#66304,#66305,#66306,#66307,#66308,#66309,#66310,#66311,#66312,#66313,
#66314,#66315,#66316,#66317,#66318,#66319),.UNSPECIFIED.,.F.,.F.,(4,3,3,
3,3,3,3,4),(-192.588308255582,-191.944575559687,-190.944864228647,-189.945152897607,
-188.945441566567,-187.945730235527,-186.946018904487,-186.305122948402),
 .UNSPECIFIED.);
#3453=B_SPLINE_CURVE_WITH_KNOTS('',3,(#66320,#66321,#66322,#66323,#66324,
#66325,#66326,#66327,#66328,#66329,#66330,#66331,#66332,#66333,#66334,#66335,
#66336,#66337,#66338,#66339,#66340,#66341),.UNSPECIFIED.,.F.,.F.,(4,3,3,
3,3,3,3,4),(183.322419119119,184.091830266117,185.086921240529,186.08201221494,
187.077103189352,188.072194163763,189.067285138175,189.605604426299),
 .UNSPECIFIED.);
#3454=B_SPLINE_CURVE_WITH_KNOTS('',3,(#66348,#66349,#66350,#66351,#66352,
#66353,#66354,#66355,#66356,#66357,#66358,#66359,#66360,#66361,#66362,#66363,
#66364,#66365,#66366,#66367,#66368,#66369),.UNSPECIFIED.,.F.,.F.,(4,3,3,
3,3,3,3,4),(-198.433361913984,-197.942843545928,-196.943132214888,-195.943420883848,
-194.943709552807,-193.943998221767,-192.944286890727,-192.588308255582),
 .UNSPECIFIED.);
#3455=B_SPLINE_CURVE_WITH_KNOTS('',3,(#66370,#66371,#66372,#66373,#66374,
#66375,#66376,#66377,#66378,#66379,#66380,#66381,#66382,#66383,#66384,#66385,
#66386,#66387,#66388,#66389,#66390,#66391),.UNSPECIFIED.,.F.,.F.,(4,3,3,
3,3,3,3,4),(189.605604426299,190.062376112586,191.057467086998,192.052558061409,
193.04764903582,194.042740010232,195.037830984643,195.888789733479),
 .UNSPECIFIED.);
#3456=B_SPLINE_CURVE_WITH_KNOTS('',3,(#66397,#66398,#66399,#66400,#66401),
 .UNSPECIFIED.,.F.,.F.,(4,1,4),(210.486707790516,210.557769104723,211.557480435763),
 .UNSPECIFIED.);
#3457=B_SPLINE_CURVE_WITH_KNOTS('',3,(#66407,#66408,#66409,#66410,#66411,
#66412,#66413,#66414,#66415,#66416),.UNSPECIFIED.,.F.,.F.,(4,1,1,1,1,1,
1,4),(204.203522483337,204.559501118482,205.559212449522,206.558923780562,
207.558635111602,208.558346442642,209.558057773683,210.486707790516),
 .UNSPECIFIED.);
#3458=B_SPLINE_CURVE_WITH_KNOTS('',3,(#66419,#66420,#66421,#66422,#66423,
#66424,#66425,#66426,#66427,#66428),.UNSPECIFIED.,.F.,.F.,(4,1,1,1,1,1,
1,4),(204.203522483337,204.347654708913,205.342745683324,206.337836657736,
207.332927632147,208.328018606559,209.32310958097,210.318200555382),
 .UNSPECIFIED.);
#3459=B_SPLINE_CURVE_WITH_KNOTS('',3,(#66433,#66434,#66435,#66436,#66437,
#66438,#66439,#66440,#66441,#66442),.UNSPECIFIED.,.F.,.F.,(4,1,1,1,1,1,
1,4),(197.920337176157,198.561233132242,199.560944463282,200.560655794322,
201.560367125362,202.560078456402,203.559789787442,204.203522483337),
 .UNSPECIFIED.);
#3460=B_SPLINE_CURVE_WITH_KNOTS('',3,(#66443,#66444,#66445,#66446,#66447,
#66448,#66449,#66450,#66451,#66452),.UNSPECIFIED.,.F.,.F.,(4,1,1,1,1,1,
1,4),(197.920337176157,198.377108862444,199.372199836856,200.367290811267,
201.362381785679,202.35747276009,203.352563734501,204.203522483337),
 .UNSPECIFIED.);
#3461=B_SPLINE_CURVE_WITH_KNOTS('',3,(#66457,#66458,#66459,#66460,#66461,
#66462,#66463,#66464,#66465,#66466),.UNSPECIFIED.,.F.,.F.,(4,1,1,1,1,1,
1,4),(191.637151868977,192.562965146002,193.562676477042,194.562387808082,
195.562099139122,196.561810470162,197.561521801202,197.920337176157),
 .UNSPECIFIED.);
#3462=B_SPLINE_CURVE_WITH_KNOTS('',3,(#66467,#66468,#66469,#66470,#66471,
#66472,#66473,#66474,#66475,#66476),.UNSPECIFIED.,.F.,.F.,(4,1,1,1,1,1,
1,4),(191.637151868977,192.406563015976,193.401653990387,194.396744964798,
195.39183593921,196.386926913621,197.382017888033,197.920337176157),
 .UNSPECIFIED.);
#3463=B_SPLINE_CURVE_WITH_KNOTS('',3,(#66481,#66482,#66483,#66484,#66485,
#66486,#66487,#66488,#66489,#66490,#66491),.UNSPECIFIED.,.F.,.F.,(4,1,1,
1,1,1,1,1,4),(185.353966561798,185.564985828722,186.564697159762,187.564408490802,
188.564119821842,189.563831152882,190.563542483922,191.563253814962,191.637151868977),
 .UNSPECIFIED.);
#3464=B_SPLINE_CURVE_WITH_KNOTS('',3,(#66492,#66493,#66494,#66495,#66496,
#66497,#66498,#66499,#66500,#66501,#66502),.UNSPECIFIED.,.F.,.F.,(4,1,1,
1,1,1,1,1,4),(185.353966561798,185.440926195095,186.436017169507,187.431108143918,
188.42619911833,189.421290092741,190.416381067153,191.411472041564,191.637151868977),
 .UNSPECIFIED.);
#3465=B_SPLINE_CURVE_WITH_KNOTS('',3,(#66507,#66508,#66509,#66510,#66511,
#66512,#66513,#66514,#66515,#66516),.UNSPECIFIED.,.F.,.F.,(4,1,1,1,1,1,
1,4),(179.070781254618,179.566717842481,180.566429173521,181.566140504561,
182.565851835602,183.565563166642,184.565274497682,185.353966561798),
 .UNSPECIFIED.);
#3466=B_SPLINE_CURVE_WITH_KNOTS('',3,(#66517,#66518,#66519,#66520,#66521,
#66522,#66523,#66524,#66525,#66526),.UNSPECIFIED.,.F.,.F.,(4,1,1,1,1,1,
1,4),(179.070781254618,179.470380348627,180.465471323038,181.46056229745,
182.455653271861,183.450744246273,184.445835220684,185.353966561798),
 .UNSPECIFIED.);
#3467=B_SPLINE_CURVE_WITH_KNOTS('',3,(#66531,#66532,#66533,#66534,#66535,
#66536,#66537,#66538,#66539,#66540),.UNSPECIFIED.,.F.,.F.,(4,1,1,1,1,1,
1,4),(172.787595947439,173.568449856241,174.568161187281,175.567872518321,
176.567583849361,177.567295180401,178.567006511441,179.070781254618),
 .UNSPECIFIED.);
#3468=B_SPLINE_CURVE_WITH_KNOTS('',3,(#66541,#66542,#66543,#66544,#66545,
#66546,#66547,#66548,#66549,#66550),.UNSPECIFIED.,.F.,.F.,(4,1,1,1,1,1,
1,4),(172.787595947439,173.499834502158,174.49492547657,175.490016450981,
176.485107425392,177.480198399804,178.475289374215,179.070781254618),
 .UNSPECIFIED.);
#3469=B_SPLINE_CURVE_WITH_KNOTS('',3,(#66555,#66556,#66557,#66558,#66559,
#66560,#66561,#66562,#66563,#66564,#66565),.UNSPECIFIED.,.F.,.F.,(4,1,1,
1,1,1,1,1,4),(166.504410640259,166.570470538961,167.570181870001,168.569893201041,
169.569604532081,170.569315863121,171.569027194161,172.568738525201,172.787595947439),
 .UNSPECIFIED.);
#3470=B_SPLINE_CURVE_WITH_KNOTS('',3,(#66566,#66567,#66568,#66569,#66570,
#66571,#66572,#66573,#66574,#66575,#66576),.UNSPECIFIED.,.F.,.F.,(4,1,1,
1,1,1,1,1,4),(166.504410640259,166.534197681278,167.529288655689,168.524379630101,
169.519470604512,170.514561578924,171.509652553335,172.504743527747,172.787595947439),
 .UNSPECIFIED.);
#3471=B_SPLINE_CURVE_WITH_KNOTS('',3,(#66581,#66582,#66583,#66584,#66585,
#66586,#66587,#66588,#66589,#66590),.UNSPECIFIED.,.F.,.F.,(4,1,1,1,1,1,
1,4),(160.22122533308,160.572202552721,161.571913883761,162.571625214801,
163.571336545841,164.571047876881,165.570759207921,166.504410640259),
 .UNSPECIFIED.);
#3472=B_SPLINE_CURVE_WITH_KNOTS('',3,(#66591,#66592,#66593,#66594,#66595,
#66596,#66597,#66598,#66599,#66600),.UNSPECIFIED.,.F.,.F.,(4,1,1,1,1,1,
1,4),(160.22122533308,160.563651834809,161.558742809221,162.553833783632,
163.548924758044,164.544015732455,165.539106706867,166.504410640259),
 .UNSPECIFIED.);
#3473=B_SPLINE_CURVE_WITH_KNOTS('',3,(#66605,#66606,#66607,#66608,#66609,
#66610,#66611,#66612,#66613,#66614),.UNSPECIFIED.,.F.,.F.,(4,1,1,1,1,1,
1,4),(153.9380400259,154.57393456648,155.57364589752,156.57335722856,157.573068559601,
158.572779890641,159.572491221681,160.22122533308),.UNSPECIFIED.);
#3474=B_SPLINE_CURVE_WITH_KNOTS('',3,(#66615,#66616,#66617,#66618,#66619,
#66620,#66621,#66622,#66623,#66624),.UNSPECIFIED.,.F.,.F.,(4,1,1,1,1,1,
1,4),(153.9380400259,154.593105988341,155.588196962752,156.583287937164,
157.578378911575,158.573469885986,159.568560860398,160.22122533308),
 .UNSPECIFIED.);
#3475=B_SPLINE_CURVE_WITH_KNOTS('',3,(#66629,#66630,#66631,#66632,#66633,
#66634,#66635,#66636,#66637,#66638),.UNSPECIFIED.,.F.,.F.,(4,1,1,1,1,1,
1,4),(147.65485471872,148.57566658024,149.57537791128,150.57508924232,151.57480057336,
152.5745119044,153.57422323544,153.9380400259),.UNSPECIFIED.);
#3476=B_SPLINE_CURVE_WITH_KNOTS('',3,(#66639,#66640,#66641,#66642,#66643,
#66644,#66645,#66646,#66647,#66648),.UNSPECIFIED.,.F.,.F.,(4,1,1,1,1,1,
1,4),(147.65485471872,148.622560141872,149.617651116283,150.612742090695,
151.607833065106,152.602924039518,153.598015013929,153.9380400259),
 .UNSPECIFIED.);
#3477=B_SPLINE_CURVE_WITH_KNOTS('',3,(#66653,#66654,#66655,#66656,#66657,
#66658,#66659,#66660,#66661,#66662,#66663),.UNSPECIFIED.,.F.,.F.,(4,1,1,
1,1,1,1,1,4),(141.371669411541,141.57768726296,142.577398594,143.57710992504,
144.57682125608,145.57653258712,146.57624391816,147.5759552492,147.65485471872),
 .UNSPECIFIED.);
#3478=B_SPLINE_CURVE_WITH_KNOTS('',3,(#66664,#66665,#66666,#66667,#66668,
#66669,#66670,#66671,#66672,#66673,#66674),.UNSPECIFIED.,.F.,.F.,(4,1,1,
1,1,1,1,1,4),(141.371669411541,141.656923320992,142.652014295403,143.647105269815,
144.642196244226,145.637287218638,146.632378193049,147.627469167461,147.65485471872),
 .UNSPECIFIED.);
#3479=B_SPLINE_CURVE_WITH_KNOTS('',3,(#66679,#66680,#66681,#66682,#66683,
#66684,#66685,#66686,#66687,#66688),.UNSPECIFIED.,.F.,.F.,(4,1,1,1,1,1,
1,4),(135.088484104361,135.57941927672,136.57913060776,137.5788419388,138.57855326984,
139.57826460088,140.57797593192,141.371669411541),.UNSPECIFIED.);
#3480=B_SPLINE_CURVE_WITH_KNOTS('',3,(#66689,#66690,#66691,#66692,#66693,
#66694,#66695,#66696,#66697,#66698),.UNSPECIFIED.,.F.,.F.,(4,1,1,1,1,1,
1,4),(135.088484104361,135.686377474523,136.681468448935,137.676559423346,
138.671650397758,139.666741372169,140.66183234658,141.371669411541),
 .UNSPECIFIED.);
#3481=B_SPLINE_CURVE_WITH_KNOTS('',3,(#66703,#66704,#66705,#66706,#66707,
#66708,#66709,#66710,#66711,#66712),.UNSPECIFIED.,.F.,.F.,(4,1,1,1,1,1,
1,4),(128.805298797182,129.581151290479,130.58086262152,131.58057395256,
132.5802852836,133.57999661464,134.57970794568,135.088484104361),
 .UNSPECIFIED.);
#3482=B_SPLINE_CURVE_WITH_KNOTS('',3,(#66713,#66714,#66715,#66716,#66717,
#66718,#66719,#66720,#66721,#66722),.UNSPECIFIED.,.F.,.F.,(4,1,1,1,1,1,
1,4),(128.805298797182,129.715831628055,130.710922602466,131.706013576877,
132.701104551289,133.6961955257,134.691286500112,135.088484104361),
 .UNSPECIFIED.);
#3483=B_SPLINE_CURVE_WITH_KNOTS('',3,(#66727,#66728,#66729,#66730,#66731,
#66732,#66733,#66734,#66735,#66736,#66737),.UNSPECIFIED.,.F.,.F.,(4,1,1,
1,1,1,1,1,4),(122.522113490002,122.583171973199,123.582883304239,124.582594635279,
125.582305966319,126.582017297359,127.581728628399,128.581439959439,128.805298797182),
 .UNSPECIFIED.);
#3484=B_SPLINE_CURVE_WITH_KNOTS('',3,(#66738,#66739,#66740,#66741,#66742,
#66743,#66744,#66745,#66746,#66747,#66748),.UNSPECIFIED.,.F.,.F.,(4,1,1,
1,1,1,1,1,4),(122.522113490002,122.750194807174,123.745285781586,124.740376755997,
125.735467730409,126.73055870482,127.725649679232,128.720740653643,128.805298797182),
 .UNSPECIFIED.);
#3485=B_SPLINE_CURVE_WITH_KNOTS('',3,(#66753,#66754,#66755,#66756,#66757,
#66758,#66759,#66760,#66761,#66762),.UNSPECIFIED.,.F.,.F.,(4,1,1,1,1,1,
1,4),(116.238928182823,116.584903986959,117.584615317999,118.584326649039,
119.584037980079,120.583749311119,121.583460642159,122.522113490002),
 .UNSPECIFIED.);
#3486=B_SPLINE_CURVE_WITH_KNOTS('',3,(#66763,#66764,#66765,#66766,#66767,
#66768,#66769,#66770,#66771,#66772),.UNSPECIFIED.,.F.,.F.,(4,1,1,1,1,1,
1,4),(116.238928182823,116.779648960706,117.774739935117,118.769830909529,
119.76492188394,120.760012858352,121.755103832763,122.522113490002),
 .UNSPECIFIED.);
#3487=B_SPLINE_CURVE_WITH_KNOTS('',3,(#66777,#66778,#66779,#66780,#66781,
#66782,#66783,#66784,#66785,#66786),.UNSPECIFIED.,.F.,.F.,(4,1,1,1,1,1,
1,4),(109.955742875643,110.586636000719,111.586347331759,112.586058662799,
113.585769993839,114.585481324879,115.585192655919,116.238928182823),
 .UNSPECIFIED.);
#3488=B_SPLINE_CURVE_WITH_KNOTS('',3,(#66787,#66788,#66789,#66790,#66791,
#66792,#66793,#66794,#66795,#66796),.UNSPECIFIED.,.F.,.F.,(4,1,1,1,1,1,
1,4),(109.955742875643,110.809103114237,111.804194088649,112.79928506306,
113.794376037471,114.789467011883,115.784557986294,116.238928182823),
 .UNSPECIFIED.);
#3489=B_SPLINE_CURVE_WITH_KNOTS('',3,(#66801,#66802,#66803,#66804,#66805,
#66806,#66807,#66808,#66809,#66810),.UNSPECIFIED.,.F.,.F.,(4,1,1,1,1,1,
1,4),(103.672557568463,104.588368014479,105.588079345519,106.587790676559,
107.587502007599,108.587213338639,109.586924669679,109.955742875643),
 .UNSPECIFIED.);
#3490=B_SPLINE_CURVE_WITH_KNOTS('',3,(#66811,#66812,#66813,#66814,#66815,
#66816,#66817,#66818,#66819,#66820,#66821),.UNSPECIFIED.,.F.,.F.,(4,1,1,
1,1,1,1,1,4),(103.672557568463,103.843466293357,104.838557267768,105.83364824218,
106.828739216591,107.823830191003,108.818921165414,109.814012139826,109.955742875643),
 .UNSPECIFIED.);
#3491=B_SPLINE_CURVE_WITH_KNOTS('',3,(#66826,#66827,#66828,#66829,#66830,
#66831,#66832,#66833,#66834,#66835,#66836),.UNSPECIFIED.,.F.,.F.,(4,1,1,
1,1,1,1,1,4),(97.3893722612838,97.5903886971983,98.5901000282383,99.5898113592783,
100.589522690318,101.589234021358,102.588945352398,103.588656683438,103.672557568463),
 .UNSPECIFIED.);
#3492=B_SPLINE_CURVE_WITH_KNOTS('',3,(#66837,#66838,#66839,#66840,#66841,
#66842,#66843,#66844,#66845,#66846),.UNSPECIFIED.,.F.,.F.,(4,1,1,1,1,1,
1,4),(97.3893722612838,97.8729204468883,98.8680114212997,99.8631023957112,
100.858193370123,101.853284344534,102.848375318946,103.672557568463),
 .UNSPECIFIED.);
#3493=B_SPLINE_CURVE_WITH_KNOTS('',3,(#66851,#66852,#66853,#66854,#66855,
#66856,#66857,#66858,#66859,#66860),.UNSPECIFIED.,.F.,.F.,(4,1,1,1,1,1,
1,4),(91.1061869541042,91.592120710958,92.5918320419981,93.5915433730381,
94.5912547040781,95.5909660351182,96.5906773661582,97.3893722612838),
 .UNSPECIFIED.);
#3494=B_SPLINE_CURVE_WITH_KNOTS('',3,(#66861,#66862,#66863,#66864,#66865,
#66866,#66867,#66868,#66869,#66870),.UNSPECIFIED.,.F.,.F.,(4,1,1,1,1,1,
1,4),(91.1061869541042,91.9023746004196,92.897465574831,93.8925565492425,
94.8876475236539,95.8827384980654,96.8778294724768,97.3893722612838),
 .UNSPECIFIED.);
#3495=B_SPLINE_CURVE_WITH_KNOTS('',3,(#66875,#66876,#66877,#66878,#66879,
#66880,#66881,#66882,#66883,#66884),.UNSPECIFIED.,.F.,.F.,(4,1,1,1,1,1,
1,4),(84.8230016469246,85.5938527247178,86.5935640557578,87.5932753867979,
88.5929867178379,89.5926980488779,90.592409379918,91.1061869541042),
 .UNSPECIFIED.);
#3496=B_SPLINE_CURVE_WITH_KNOTS('',3,(#66885,#66886,#66887,#66888,#66889,
#66890,#66891,#66892,#66893,#66894,#66895),.UNSPECIFIED.,.F.,.F.,(4,1,1,
1,1,1,1,1,4),(84.8230016469246,84.9367377795395,85.9318287539509,86.9269197283624,
87.9220107027738,88.9171016771853,89.9121926515967,90.9072836260082,91.1061869541042),
 .UNSPECIFIED.);
#3497=B_SPLINE_CURVE_WITH_KNOTS('',3,(#66900,#66901,#66902,#66903,#66904,
#66905,#66906,#66907,#66908,#66909,#66910),.UNSPECIFIED.,.F.,.F.,(4,1,1,
1,1,1,1,1,4),(78.539816339745,78.5958734074375,79.5955847384776,80.5952960695176,
81.5950074005576,82.5947187315977,83.5944300626377,84.5941413936777,84.8230016469246),
 .UNSPECIFIED.);
#3498=B_SPLINE_CURVE_WITH_KNOTS('',3,(#66911,#66912,#66913,#66914,#66915,
#66916,#66917,#66918,#66919,#66920),.UNSPECIFIED.,.F.,.F.,(4,1,1,1,1,1,
1,4),(78.539816339745,78.9661919330708,79.9612829074823,80.9563738818937,
81.9514648563052,82.9465558307166,83.941646805128,84.8230016469246),
 .UNSPECIFIED.);
#3499=B_SPLINE_CURVE_WITH_KNOTS('',3,(#66925,#66926,#66927,#66928,#66929,
#66930,#66931,#66932,#66933,#66934),.UNSPECIFIED.,.F.,.F.,(4,1,1,1,1,1,
1,4),(72.2566310325654,72.5976054211973,73.5973167522373,74.5970280832774,
75.5967394143174,76.5964507453574,77.5961620763975,78.539816339745),
 .UNSPECIFIED.);
#3500=B_SPLINE_CURVE_WITH_KNOTS('',3,(#66935,#66936,#66937,#66938,#66939,
#66940,#66941,#66942,#66943,#66944),.UNSPECIFIED.,.F.,.F.,(4,1,1,1,1,1,
1,4),(72.2566310325654,72.9956460866021,73.9907370610136,74.985828035425,
75.9809190098365,76.9760099842479,77.9711009586594,78.539816339745),
 .UNSPECIFIED.);
#3501=B_SPLINE_CURVE_WITH_KNOTS('',3,(#66949,#66950,#66951,#66952,#66953,
#66954,#66955,#66956,#66957,#66958),.UNSPECIFIED.,.F.,.F.,(4,1,1,1,1,1,
1,4),(65.9734457253858,66.5993374349571,67.5990487659971,68.5987600970371,
69.5984714280772,70.5981827591172,71.5978940901573,72.2566310325654),
 .UNSPECIFIED.);
#3502=B_SPLINE_CURVE_WITH_KNOTS('',3,(#66959,#66960,#66961,#66962,#66963,
#66964,#66965,#66966,#66967,#66968,#66969),.UNSPECIFIED.,.F.,.F.,(4,1,1,
1,1,1,1,1,4),(65.9734457253858,66.030009265722,67.0251002401335,68.0201912145449,
69.0152821889564,70.0103731633678,71.0054641377792,72.0005551121907,72.2566310325654),
 .UNSPECIFIED.);
#3503=B_SPLINE_CURVE_WITH_KNOTS('',3,(#66974,#66975,#66976,#66977,#66978,
#66979,#66980,#66981,#66982,#66983),.UNSPECIFIED.,.F.,.F.,(4,1,1,1,1,1,
1,4),(59.6902604182062,60.6010694487168,61.6007807797569,62.6004921107969,
63.6002034418369,64.599914772877,65.599626103917,65.9734457253858),
 .UNSPECIFIED.);
#3504=B_SPLINE_CURVE_WITH_KNOTS('',3,(#66984,#66985,#66986,#66987,#66988,
#66989,#66990,#66991,#66992,#66993),.UNSPECIFIED.,.F.,.F.,(4,1,1,1,1,1,
1,4),(59.6902604182063,60.0594634192534,61.0545543936648,62.0496453680762,
63.0447363424877,64.0398273168991,65.0349182913106,65.9734457253858),
 .UNSPECIFIED.);
#3505=B_SPLINE_CURVE_WITH_KNOTS('',3,(#66998,#66999,#67000,#67001,#67002,
#67003,#67004,#67005,#67006,#67007,#67008),.UNSPECIFIED.,.F.,.F.,(4,1,1,
1,1,1,1,1,4),(53.4070751110266,53.6030901314366,54.6028014624766,55.6025127935166,
56.6022241245567,57.6019354555967,58.6016467866367,59.6013581176768,59.6902604182062),
 .UNSPECIFIED.);
#3506=B_SPLINE_CURVE_WITH_KNOTS('',3,(#67009,#67010,#67011,#67012,#67013,
#67014,#67015,#67016,#67017,#67018),.UNSPECIFIED.,.F.,.F.,(4,1,1,1,1,1,
1,4),(53.4070751110267,54.0889175727847,55.0840085471961,56.0790995216076,
57.074190496019,58.0692814704305,59.0643724448419,59.6902604182063),
 .UNSPECIFIED.);
#3507=B_SPLINE_CURVE_WITH_KNOTS('',3,(#67023,#67024,#67025,#67026,#67027,
#67028,#67029,#67030,#67031,#67032),.UNSPECIFIED.,.F.,.F.,(4,1,1,1,1,1,
1,4),(47.123889803847,47.6048221451963,48.6045334762364,49.6042448072764,
50.6039561383164,51.6036674693565,52.6033788003965,53.4070751110266),
 .UNSPECIFIED.);
#3508=B_SPLINE_CURVE_WITH_KNOTS('',3,(#67033,#67034,#67035,#67036,#67037,
#67038,#67039,#67040,#67041,#67042),.UNSPECIFIED.,.F.,.F.,(4,1,1,1,1,1,
1,4),(47.1238898038471,48.118371726316,49.1134627007275,50.1085536751389,
51.1036446495503,52.0987356239618,53.0938265983732,53.4070751110267),
 .UNSPECIFIED.);
#3509=B_SPLINE_CURVE_WITH_KNOTS('',3,(#67047,#67048,#67049,#67050,#67051,
#67052,#67053,#67054,#67055,#67056),.UNSPECIFIED.,.F.,.F.,(4,1,1,1,1,1,
1,4),(40.8407044966674,41.6065541589561,42.6062654899961,43.6059768210362,
44.6056881520762,45.6053994831162,46.6051108141563,47.123889803847),
 .UNSPECIFIED.);
#3510=B_SPLINE_CURVE_WITH_KNOTS('',3,(#67057,#67058,#67059,#67060,#67061,
#67062,#67063,#67064,#67065,#67066,#67067),.UNSPECIFIED.,.F.,.F.,(4,1,1,
1,1,1,1,1,4),(40.8407044966675,41.1527349054359,42.1478258798473,43.1429168542588,
44.1380078286702,45.1330988030817,46.1281897774931,47.1232807519046,47.1238898038471),
 .UNSPECIFIED.);
#3511=B_SPLINE_CURVE_WITH_KNOTS('',3,(#67072,#67073,#67074,#67075,#67076,
#67077,#67078,#67079,#67080,#67081,#67082),.UNSPECIFIED.,.F.,.F.,(4,1,1,
1,1,1,1,1,4),(34.5575191894878,34.6085748416758,35.6082861727159,36.6079975037559,
37.6077088347959,38.607420165836,39.607131496876,40.6068428279161,40.8407044966674),
 .UNSPECIFIED.);
#3512=B_SPLINE_CURVE_WITH_KNOTS('',3,(#67083,#67084,#67085,#67086,#67087,
#67088,#67089,#67090,#67091,#67092),.UNSPECIFIED.,.F.,.F.,(4,1,1,1,1,1,
1,4),(34.5575191894879,35.1821890589672,36.1772800333787,37.1723710077901,
38.1674619822016,39.162552956613,40.1576439310244,40.8407044966675),
 .UNSPECIFIED.);
#3513=B_SPLINE_CURVE_WITH_KNOTS('',3,(#67097,#67098,#67099,#67100,#67101,
#67102,#67103,#67104,#67105,#67106),.UNSPECIFIED.,.F.,.F.,(4,1,1,1,1,1,
1,4),(28.2743338823082,28.6103068554356,29.6100181864756,30.6097295175157,
31.6094408485557,32.6091521795958,33.6088635106358,34.5575191894878),
 .UNSPECIFIED.);
#3514=B_SPLINE_CURVE_WITH_KNOTS('',3,(#67107,#67108,#67109,#67110,#67111,
#67112,#67113,#67114,#67115,#67116),.UNSPECIFIED.,.F.,.F.,(4,1,1,1,1,1,
1,4),(28.2743338823083,29.2116432124985,30.20673418691,31.2018251613214,
32.1969161357329,33.1920071101443,34.1870980845558,34.5575191894879),
 .UNSPECIFIED.);
#3515=B_SPLINE_CURVE_WITH_KNOTS('',3,(#67121,#67122,#67123,#67124,#67125,
#67126,#67127,#67128,#67129,#67130),.UNSPECIFIED.,.F.,.F.,(4,1,1,1,1,1,
1,4),(21.9911485751287,22.6120388691954,23.6117502002354,24.6114615312754,
25.6111728623155,26.6108841933555,27.6105955243956,28.2743338823082),
 .UNSPECIFIED.);
#3516=B_SPLINE_CURVE_WITH_KNOTS('',3,(#67131,#67132,#67133,#67134,#67135,
#67136,#67137,#67138,#67139,#67140,#67141),.UNSPECIFIED.,.F.,.F.,(4,1,1,
1,1,1,1,1,4),(21.9911485751287,22.2460063916184,23.2410973660299,24.2361883404413,
25.2312793148528,26.2263702892642,27.2214612636757,28.2165522380871,28.2743338823083),
 .UNSPECIFIED.);
#3517=B_SPLINE_CURVE_WITH_KNOTS('',3,(#67146,#67147,#67148,#67149,#67150,
#67151,#67152,#67153,#67154,#67155),.UNSPECIFIED.,.F.,.F.,(4,1,1,1,1,1,
1,4),(15.7079632679491,16.6137708829551,17.6134822139952,18.6131935450352,
19.6129048760753,20.6126162071153,21.6123275381553,21.9911485751287),
 .UNSPECIFIED.);
#3518=B_SPLINE_CURVE_WITH_KNOTS('',3,(#67156,#67157,#67158,#67159,#67160,
#67161,#67162,#67163,#67164,#67165),.UNSPECIFIED.,.F.,.F.,(4,1,1,1,1,1,
1,4),(15.7079632679491,16.2754605451498,17.2705515195612,18.2656424939726,
19.2607334683841,20.2558244427955,21.250915417207,21.9911485751287),
 .UNSPECIFIED.);
#3519=B_SPLINE_CURVE_WITH_KNOTS('',3,(#67171,#67172,#67173,#67174,#67175,
#67176,#67177,#67178,#67179,#67180,#67181,#67182,#67183,#67184,#67185,#67186,
#67187,#67188,#67189,#67190,#67191,#67192,#67193,#67194,#67195,#67196,#67197,
#67198,#67199,#67200,#67201,#67202,#67203,#67204,#67205,#67206,#67207,#67208,
#67209,#67210,#67211,#67212,#67213,#67214,#67215,#67216,#67217,#67218,#67219,
#67220,#67221,#67222,#67223,#67224,#67225,#67226,#67227,#67228,#67229,#67230,
#67231,#67232,#67233,#67234,#67235,#67236,#67237,#67238,#67239,#67240,#67241,
#67242,#67243,#67244,#67245,#67246,#67247,#67248,#67249,#67250,#67251,#67252,
#67253,#67254,#67255,#67256,#67257,#67258,#67259,#67260,#67261,#67262,#67263,
#67264,#67265,#67266,#67267,#67268,#67269,#67270,#67271,#67272,#67273,#67274,
#67275,#67276,#67277,#67278,#67279,#67280,#67281,#67282,#67283,#67284,#67285,
#67286,#67287,#67288,#67289,#67290,#67291,#67292,#67293,#67294,#67295,#67296,
#67297,#67298,#67299,#67300,#67301,#67302,#67303,#67304,#67305,#67306,#67307,
#67308,#67309,#67310,#67311,#67312,#67313,#67314,#67315,#67316,#67317,#67318,
#67319,#67320,#67321,#67322,#67323,#67324,#67325,#67326,#67327,#67328,#67329,
#67330,#67331,#67332,#67333,#67334,#67335,#67336,#67337,#67338,#67339,#67340,
#67341,#67342,#67343,#67344,#67345,#67346,#67347,#67348,#67349,#67350,#67351,
#67352,#67353,#67354,#67355,#67356,#67357,#67358,#67359,#67360,#67361,#67362,
#67363,#67364,#67365,#67366,#67367,#67368,#67369,#67370,#67371,#67372,#67373,
#67374,#67375,#67376,#67377,#67378,#67379,#67380,#67381,#67382,#67383,#67384,
#67385,#67386,#67387,#67388,#67389,#67390,#67391,#67392,#67393,#67394,#67395,
#67396,#67397,#67398,#67399,#67400,#67401,#67402,#67403,#67404,#67405,#67406,
#67407,#67408,#67409,#67410,#67411,#67412,#67413,#67414,#67415,#67416,#67417,
#67418,#67419,#67420,#67421,#67422,#67423,#67424,#67425,#67426,#67427,#67428,
#67429),.UNSPECIFIED.,.F.,.F.,(4,3,3,3,3,3,3,3,3,3,3,3,3,3,3,3,3,3,3,3,
3,3,3,3,3,3,3,3,3,3,3,3,3,3,3,3,3,3,3,3,3,3,3,3,3,3,3,3,3,3,3,3,3,3,3,3,
3,3,3,3,3,3,3,3,3,3,3,3,3,3,3,3,3,3,3,3,3,3,3,3,3,3,3,3,3,3,4),(-2.02747957522477,
-1.99629697890573,-1.96434882803362,-1.94770684698045,-1.93465745109861,
-1.92899323505435,-1.89637939967214,-1.86351156618679,-1.84191868086962,
-1.83643395258831,-1.80184474723693,-1.76878588804004,-1.7361915602774,
-1.71713434573009,-1.71111396618423,-1.70636535171271,-1.69807713118279,
-1.66615334411595,-1.63338107755074,-1.59870970356575,-1.58354097744731,
-1.57777243171763,-1.57288272657502,-1.53932550715147,-1.50538593530636,
-1.47155442193573,-1.45678251339105,-1.44498318417569,-1.44016588491778,
-1.40590427589964,-1.372125965904,-1.35601008567079,-1.32227811773956,-1.3110762482785,
-1.30413477324209,-1.27089096674751,-1.23651000513344,-1.20188424717791,
-1.17687285717032,-1.17117345644662,-1.16636983006357,-1.13156642853056,
-1.09668061447692,-1.06224151139586,-1.03201731925653,-1.02689100048705,
-1.00179312711721,-0.967864540839157,-0.93313532953401,-0.897918428976919,
-0.890942884625253,-0.885051901025072,-0.849845686106437,-0.814185285823995,
-0.778541242116049,-0.760617194519175,-0.745868237951496,-0.740902737283996,
-0.704880648128088,-0.669414287483829,-0.635148861341054,-0.611477896978161,
-0.602075382147568,-0.596900307049893,-0.562097694744849,-0.526417664836126,
-0.490045423902471,-0.460841424856508,-0.453624100180632,-0.448600894627828,
-0.412078836391778,-0.375321168507609,-0.339131447204507,-0.318451943287073,
-0.304419386760625,-0.299402690224966,-0.262514781947601,-0.25641343153477,
-0.220343758631792,-0.183630684098196,-0.160676848585921,-0.153063253496153,
-0.14786021524992,-0.11089516143744,-0.073565266371696,-0.0362697295661738,
0.),.UNSPECIFIED.);
#3520=B_SPLINE_CURVE_WITH_KNOTS('',3,(#67433,#67434,#67435,#67436,#67437,
#67438,#67439,#67440,#67441,#67442,#67443,#67444,#67445,#67446,#67447,#67448,
#67449,#67450,#67451,#67452,#67453,#67454,#67455,#67456,#67457,#67458,#67459,
#67460,#67461,#67462,#67463,#67464,#67465,#67466,#67467,#67468,#67469,#67470,
#67471,#67472,#67473,#67474,#67475,#67476,#67477,#67478,#67479,#67480,#67481),
 .UNSPECIFIED.,.F.,.F.,(4,3,3,3,3,3,3,3,3,3,3,3,3,3,3,3,4),(-0.379502319520043,
-0.35268354233973,-0.317392763997328,-0.282090054200831,-0.271802233255953,
-0.267093649425612,-0.233020332933001,-0.198977913737098,-0.165391137616394,
-0.144717245414345,-0.134595686290805,-0.130270172117405,-0.097702629088054,
-0.0656991121917264,-0.0328495560958632,-0.00219762996067144,0.),
 .UNSPECIFIED.);
#3521=B_SPLINE_CURVE_WITH_KNOTS('',3,(#67483,#67484,#67485,#67486,#67487,
#67488,#67489,#67490,#67491,#67492,#67493,#67494,#67495,#67496,#67497,#67498,
#67499,#67500,#67501,#67502,#67503,#67504,#67505,#67506,#67507),
 .UNSPECIFIED.,.F.,.F.,(4,3,3,3,3,3,3,3,4),(-0.549622632142038,-0.513019755170316,
-0.477082564278427,-0.4417887745146,-0.426217160765961,-0.417941853469451,
-0.412784386135711,-0.408981449436597,-0.379502319520043),.UNSPECIFIED.);
#3522=B_SPLINE_CURVE_WITH_KNOTS('',3,(#68321,#68322,#68323,#68324,#68325,
#68326,#68327,#68328),.UNSPECIFIED.,.F.,.F.,(4,1,1,1,1,4),(11.6152142277549,
12.614925558795,13.614636889835,14.6143482208751,15.6140595519151,15.7079632679491),
 .UNSPECIFIED.);
#3523=B_SPLINE_CURVE_WITH_KNOTS('',3,(#68329,#68330,#68331,#68332,#68333,
#68334,#68335,#68336,#68337,#68338,#68339,#68340,#68341,#68342,#68343,#68344,
#68345,#68346,#68347,#68348,#68349,#68350,#68351,#68352,#68353,#68354,#68355,
#68356,#68357,#68358,#68359,#68360,#68361,#68362,#68363,#68364,#68365,#68366,
#68367,#68368,#68369,#68370,#68371,#68372,#68373,#68374,#68375,#68376,#68377,
#68378,#68379,#68380,#68381,#68382,#68383,#68384,#68385,#68386,#68387,#68388,
#68389,#68390,#68391,#68392,#68393,#68394,#68395,#68396,#68397,#68398,#68399,
#68400,#68401,#68402,#68403,#68404,#68405,#68406,#68407,#68408,#68409,#68410,
#68411,#68412,#68413,#68414,#68415,#68416,#68417,#68418,#68419,#68420,#68421,
#68422,#68423,#68424,#68425),.UNSPECIFIED.,.F.,.F.,(4,3,3,3,3,3,3,3,3,3,
3,3,3,3,3,3,3,3,3,3,3,3,3,3,3,3,3,3,3,3,3,3,4),(-0.741270768406377,-0.717014623295539,
-0.680491508968579,-0.659046519725601,-0.642659659722095,-0.636144348715375,
-0.599359723630772,-0.567173176681745,-0.553071549886647,-0.544359430417001,
-0.537677536280526,-0.502275731429912,-0.467137784296744,-0.43303904778729,
-0.410246122850107,-0.399258187406409,-0.39485296865865,-0.361233284053521,
-0.341867348038558,-0.307605174602581,-0.273187750648466,-0.26292576164664,
-0.257107052763031,-0.223674627080457,-0.190212894077251,-0.15716430044683,
-0.137518762890977,-0.127951707437281,-0.12318250736928,-0.0909836130414784,
-0.0592393070967323,-0.028471589982648,0.),.UNSPECIFIED.);
#3524=B_SPLINE_CURVE_WITH_KNOTS('',3,(#68428,#68429,#68430,#68431,#68432,
#68433,#68434,#68435,#68436),.UNSPECIFIED.,.F.,.F.,(4,1,1,1,1,1,4),(10.375934347374,
11.3000056730925,12.295096647504,13.2901876219154,14.2852785963269,15.2803695707383,
15.7079632679491),.UNSPECIFIED.);
#3525=B_SPLINE_CURVE_WITH_KNOTS('',3,(#69262,#69263,#69264,#69265,#69266,
#69267,#69268),.UNSPECIFIED.,.F.,.F.,(4,3,4),(195.888789733479,196.032921959055,
196.372160316468),.UNSPECIFIED.);
#3526=B_SPLINE_CURVE_WITH_KNOTS('',3,(#69269,#69270,#69271,#69272,#69273,
#69274,#69275,#69276,#69277,#69278,#69279,#69280,#69281,#69282,#69283,#69284,
#69285,#69286,#69287,#69288,#69289,#69290,#69291,#69292,#69293,#69294,#69295,
#69296,#69297,#69298,#69299,#69300,#69301,#69302,#69303,#69304,#69305,#69306,
#69307,#69308,#69309,#69310,#69311,#69312,#69313,#69314,#69315,#69316,#69317,
#69318,#69319,#69320,#69321,#69322,#69323,#69324,#69325,#69326,#69327,#69328,
#69329,#69330,#69331,#69332,#69333,#69334,#69335,#69336,#69337,#69338,#69339,
#69340,#69341,#69342,#69343,#69344,#69345,#69346,#69347,#69348,#69349,#69350,
#69351,#69352,#69353,#69354,#69355,#69356,#69357,#69358,#69359,#69360,#69361,
#69362,#69363,#69364,#69365,#69366,#69367,#69368),.UNSPECIFIED.,.F.,.F.,
(4,3,3,3,3,3,3,3,3,3,3,3,3,3,3,3,3,3,3,3,3,3,3,3,3,3,3,3,3,3,3,3,3,4),(-0.744397949170583,
-0.721187707565161,-0.690060066224835,-0.670522596439773,-0.661245127518269,
-0.655323531675899,-0.623354149124615,-0.592617449192018,-0.579170142971507,
-0.572605591331247,-0.567933946140104,-0.534583176062334,-0.500700944806229,
-0.466885135058086,-0.444528988709526,-0.437828648817827,-0.433043709852644,
-0.398130555533214,-0.377460549663844,-0.343724507848801,-0.309355146205245,
-0.297653275947071,-0.292702465404463,-0.258301310351799,-0.222794013971477,
-0.186953470658781,-0.163584286826433,-0.155883350189299,-0.150570414508087,
-0.145643391754365,-0.108904568168204,-0.0721037270654814,-0.0359977762023965,
0.),.UNSPECIFIED.);
#3527=LINE('',#18714,#4375);
#3528=LINE('',#18723,#4376);
#3529=LINE('',#18740,#4377);
#3530=LINE('',#18791,#4378);
#3531=LINE('',#18842,#4379);
#3532=LINE('',#18890,#4380);
#3533=LINE('',#18941,#4381);
#3534=LINE('',#18992,#4382);
#3535=LINE('',#19040,#4383);
#3536=LINE('',#19091,#4384);
#3537=LINE('',#19130,#4385);
#3538=LINE('',#19154,#4386);
#3539=LINE('',#19178,#4387);
#3540=LINE('',#19203,#4388);
#3541=LINE('',#19228,#4389);
#3542=LINE('',#19252,#4390);
#3543=LINE('',#19277,#4391);
#3544=LINE('',#19302,#4392);
#3545=LINE('',#19326,#4393);
#3546=LINE('',#19343,#4394);
#3547=LINE('',#19352,#4395);
#3548=LINE('',#19369,#4396);
#3549=LINE('',#19420,#4397);
#3550=LINE('',#19471,#4398);
#3551=LINE('',#19519,#4399);
#3552=LINE('',#19570,#4400);
#3553=LINE('',#19621,#4401);
#3554=LINE('',#19669,#4402);
#3555=LINE('',#19720,#4403);
#3556=LINE('',#19759,#4404);
#3557=LINE('',#19783,#4405);
#3558=LINE('',#19807,#4406);
#3559=LINE('',#19832,#4407);
#3560=LINE('',#19857,#4408);
#3561=LINE('',#19881,#4409);
#3562=LINE('',#19906,#4410);
#3563=LINE('',#19931,#4411);
#3564=LINE('',#19955,#4412);
#3565=LINE('',#19972,#4413);
#3566=LINE('',#19981,#4414);
#3567=LINE('',#19998,#4415);
#3568=LINE('',#20049,#4416);
#3569=LINE('',#20100,#4417);
#3570=LINE('',#20148,#4418);
#3571=LINE('',#20199,#4419);
#3572=LINE('',#20250,#4420);
#3573=LINE('',#20298,#4421);
#3574=LINE('',#20349,#4422);
#3575=LINE('',#20388,#4423);
#3576=LINE('',#20412,#4424);
#3577=LINE('',#20436,#4425);
#3578=LINE('',#20461,#4426);
#3579=LINE('',#20486,#4427);
#3580=LINE('',#20510,#4428);
#3581=LINE('',#20535,#4429);
#3582=LINE('',#20560,#4430);
#3583=LINE('',#20584,#4431);
#3584=LINE('',#20601,#4432);
#3585=LINE('',#20610,#4433);
#3586=LINE('',#20627,#4434);
#3587=LINE('',#20678,#4435);
#3588=LINE('',#20729,#4436);
#3589=LINE('',#20777,#4437);
#3590=LINE('',#20828,#4438);
#3591=LINE('',#20879,#4439);
#3592=LINE('',#20927,#4440);
#3593=LINE('',#20978,#4441);
#3594=LINE('',#21017,#4442);
#3595=LINE('',#21041,#4443);
#3596=LINE('',#21065,#4444);
#3597=LINE('',#21090,#4445);
#3598=LINE('',#21115,#4446);
#3599=LINE('',#21139,#4447);
#3600=LINE('',#21164,#4448);
#3601=LINE('',#21189,#4449);
#3602=LINE('',#21213,#4450);
#3603=LINE('',#21230,#4451);
#3604=LINE('',#21239,#4452);
#3605=LINE('',#21256,#4453);
#3606=LINE('',#21307,#4454);
#3607=LINE('',#21358,#4455);
#3608=LINE('',#21406,#4456);
#3609=LINE('',#21457,#4457);
#3610=LINE('',#21508,#4458);
#3611=LINE('',#21556,#4459);
#3612=LINE('',#21607,#4460);
#3613=LINE('',#21646,#4461);
#3614=LINE('',#21670,#4462);
#3615=LINE('',#21694,#4463);
#3616=LINE('',#21719,#4464);
#3617=LINE('',#21744,#4465);
#3618=LINE('',#21768,#4466);
#3619=LINE('',#21793,#4467);
#3620=LINE('',#21818,#4468);
#3621=LINE('',#21842,#4469);
#3622=LINE('',#21859,#4470);
#3623=LINE('',#21868,#4471);
#3624=LINE('',#21885,#4472);
#3625=LINE('',#21936,#4473);
#3626=LINE('',#21987,#4474);
#3627=LINE('',#22035,#4475);
#3628=LINE('',#22086,#4476);
#3629=LINE('',#22137,#4477);
#3630=LINE('',#22185,#4478);
#3631=LINE('',#22236,#4479);
#3632=LINE('',#22275,#4480);
#3633=LINE('',#22299,#4481);
#3634=LINE('',#22323,#4482);
#3635=LINE('',#22348,#4483);
#3636=LINE('',#22373,#4484);
#3637=LINE('',#22397,#4485);
#3638=LINE('',#22422,#4486);
#3639=LINE('',#22447,#4487);
#3640=LINE('',#22471,#4488);
#3641=LINE('',#22488,#4489);
#3642=LINE('',#22497,#4490);
#3643=LINE('',#22514,#4491);
#3644=LINE('',#22565,#4492);
#3645=LINE('',#22616,#4493);
#3646=LINE('',#22664,#4494);
#3647=LINE('',#22715,#4495);
#3648=LINE('',#22766,#4496);
#3649=LINE('',#22814,#4497);
#3650=LINE('',#22865,#4498);
#3651=LINE('',#22904,#4499);
#3652=LINE('',#22928,#4500);
#3653=LINE('',#22952,#4501);
#3654=LINE('',#22977,#4502);
#3655=LINE('',#23002,#4503);
#3656=LINE('',#23026,#4504);
#3657=LINE('',#23051,#4505);
#3658=LINE('',#23076,#4506);
#3659=LINE('',#23100,#4507);
#3660=LINE('',#23117,#4508);
#3661=LINE('',#23126,#4509);
#3662=LINE('',#23143,#4510);
#3663=LINE('',#23194,#4511);
#3664=LINE('',#23245,#4512);
#3665=LINE('',#23293,#4513);
#3666=LINE('',#23344,#4514);
#3667=LINE('',#23395,#4515);
#3668=LINE('',#23443,#4516);
#3669=LINE('',#23494,#4517);
#3670=LINE('',#23533,#4518);
#3671=LINE('',#23557,#4519);
#3672=LINE('',#23581,#4520);
#3673=LINE('',#23606,#4521);
#3674=LINE('',#23631,#4522);
#3675=LINE('',#23655,#4523);
#3676=LINE('',#23680,#4524);
#3677=LINE('',#23705,#4525);
#3678=LINE('',#23729,#4526);
#3679=LINE('',#23747,#4527);
#3680=LINE('',#23756,#4528);
#3681=LINE('',#23765,#4529);
#3682=LINE('',#23774,#4530);
#3683=LINE('',#23781,#4531);
#3684=LINE('',#23785,#4532);
#3685=LINE('',#23789,#4533);
#3686=LINE('',#23793,#4534);
#3687=LINE('',#31294,#4535);
#3688=LINE('',#31296,#4536);
#3689=LINE('',#31298,#4537);
#3690=LINE('',#31299,#4538);
#3691=LINE('',#31303,#4539);
#3692=LINE('',#31304,#4540);
#3693=LINE('',#31306,#4541);
#3694=LINE('',#31308,#4542);
#3695=LINE('',#31310,#4543);
#3696=LINE('',#31312,#4544);
#3697=LINE('',#31314,#4545);
#3698=LINE('',#31316,#4546);
#3699=LINE('',#31318,#4547);
#3700=LINE('',#31320,#4548);
#3701=LINE('',#31321,#4549);
#3702=LINE('',#31325,#4550);
#3703=LINE('',#31326,#4551);
#3704=LINE('',#31327,#4552);
#3705=LINE('',#31333,#4553);
#3706=LINE('',#31335,#4554);
#3707=LINE('',#31337,#4555);
#3708=LINE('',#31339,#4556);
#3709=LINE('',#31341,#4557);
#3710=LINE('',#31343,#4558);
#3711=LINE('',#31345,#4559);
#3712=LINE('',#31347,#4560);
#3713=LINE('',#31349,#4561);
#3714=LINE('',#31351,#4562);
#3715=LINE('',#31353,#4563);
#3716=LINE('',#31354,#4564);
#3717=LINE('',#31358,#4565);
#3718=LINE('',#31359,#4566);
#3719=LINE('',#31360,#4567);
#3720=LINE('',#31364,#4568);
#3721=LINE('',#31365,#4569);
#3722=LINE('',#31366,#4570);
#3723=LINE('',#31371,#4571);
#3724=LINE('',#31373,#4572);
#3725=LINE('',#31377,#4573);
#3726=LINE('',#31378,#4574);
#3727=LINE('',#31381,#4575);
#3728=LINE('',#31382,#4576);
#3729=LINE('',#31387,#4577);
#3730=LINE('',#31389,#4578);
#3731=LINE('',#31391,#4579);
#3732=LINE('',#31393,#4580);
#3733=LINE('',#31397,#4581);
#3734=LINE('',#31398,#4582);
#3735=LINE('',#31401,#4583);
#3736=LINE('',#31403,#4584);
#3737=LINE('',#31407,#4585);
#3738=LINE('',#31409,#4586);
#3739=LINE('',#31411,#4587);
#3740=LINE('',#31413,#4588);
#3741=LINE('',#31417,#4589);
#3742=LINE('',#31418,#4590);
#3743=LINE('',#31420,#4591);
#3744=LINE('',#31423,#4592);
#3745=LINE('',#31425,#4593);
#3746=LINE('',#31429,#4594);
#3747=LINE('',#31430,#4595);
#3748=LINE('',#31433,#4596);
#3749=LINE('',#31434,#4597);
#3750=LINE('',#31437,#4598);
#3751=LINE('',#31438,#4599);
#3752=LINE('',#31441,#4600);
#3753=LINE('',#31442,#4601);
#3754=LINE('',#31447,#4602);
#3755=LINE('',#31449,#4603);
#3756=LINE('',#31451,#4604);
#3757=LINE('',#31453,#4605);
#3758=LINE('',#31456,#4606);
#3759=LINE('',#31459,#4607);
#3760=LINE('',#31460,#4608);
#3761=LINE('',#31463,#4609);
#3762=LINE('',#31464,#4610);
#3763=LINE('',#31467,#4611);
#3764=LINE('',#31469,#4612);
#3765=LINE('',#31470,#4613);
#3766=LINE('',#31472,#4614);
#3767=LINE('',#31474,#4615);
#3768=LINE('',#31475,#4616);
#3769=LINE('',#31477,#4617);
#3770=LINE('',#31481,#4618);
#3771=LINE('',#31484,#4619);
#3772=LINE('',#31485,#4620);
#3773=LINE('',#31487,#4621);
#3774=LINE('',#31491,#4622);
#3775=LINE('',#31495,#4623);
#3776=LINE('',#31497,#4624);
#3777=LINE('',#31498,#4625);
#3778=LINE('',#31500,#4626);
#3779=LINE('',#31503,#4627);
#3780=LINE('',#31506,#4628);
#3781=LINE('',#31507,#4629);
#3782=LINE('',#31508,#4630);
#3783=LINE('',#31510,#4631);
#3784=LINE('',#31513,#4632);
#3785=LINE('',#31515,#4633);
#3786=LINE('',#31516,#4634);
#3787=LINE('',#31521,#4635);
#3788=LINE('',#31523,#4636);
#3789=LINE('',#31527,#4637);
#3790=LINE('',#31529,#4638);
#3791=LINE('',#31531,#4639);
#3792=LINE('',#31533,#4640);
#3793=LINE('',#31535,#4641);
#3794=LINE('',#31537,#4642);
#3795=LINE('',#31538,#4643);
#3796=LINE('',#31539,#4644);
#3797=LINE('',#31541,#4645);
#3798=LINE('',#31544,#4646);
#3799=LINE('',#31546,#4647);
#3800=LINE('',#31547,#4648);
#3801=LINE('',#31550,#4649);
#3802=LINE('',#31552,#4650);
#3803=LINE('',#31554,#4651);
#3804=LINE('',#31556,#4652);
#3805=LINE('',#31558,#4653);
#3806=LINE('',#31560,#4654);
#3807=LINE('',#31562,#4655);
#3808=LINE('',#31564,#4656);
#3809=LINE('',#31566,#4657);
#3810=LINE('',#31567,#4658);
#3811=LINE('',#31571,#4659);
#3812=LINE('',#31572,#4660);
#3813=LINE('',#31573,#4661);
#3814=LINE('',#31577,#4662);
#3815=LINE('',#31578,#4663);
#3816=LINE('',#31581,#4664);
#3817=LINE('',#31582,#4665);
#3818=LINE('',#31584,#4666);
#3819=LINE('',#31587,#4667);
#3820=LINE('',#31592,#4668);
#3821=LINE('',#31593,#4669);
#3822=LINE('',#31595,#4670);
#3823=LINE('',#31596,#4671);
#3824=LINE('',#31599,#4672);
#3825=LINE('',#31600,#4673);
#3826=LINE('',#31602,#4674);
#3827=LINE('',#31604,#4675);
#3828=LINE('',#31605,#4676);
#3829=LINE('',#31606,#4677);
#3830=LINE('',#31608,#4678);
#3831=LINE('',#31610,#4679);
#3832=LINE('',#31611,#4680);
#3833=LINE('',#31612,#4681);
#3834=LINE('',#31614,#4682);
#3835=LINE('',#31616,#4683);
#3836=LINE('',#31617,#4684);
#3837=LINE('',#31621,#4685);
#3838=LINE('',#31622,#4686);
#3839=LINE('',#31625,#4687);
#3840=LINE('',#31629,#4688);
#3841=LINE('',#31635,#4689);
#3842=LINE('',#31643,#4690);
#3843=LINE('',#31655,#4691);
#3844=LINE('',#31675,#4692);
#3845=LINE('',#31729,#4693);
#3846=LINE('',#31777,#4694);
#3847=LINE('',#31828,#4695);
#3848=LINE('',#31879,#4696);
#3849=LINE('',#31927,#4697);
#3850=LINE('',#31966,#4698);
#3851=LINE('',#31992,#4699);
#3852=LINE('',#32017,#4700);
#3853=LINE('',#32042,#4701);
#3854=LINE('',#32066,#4702);
#3855=LINE('',#32091,#4703);
#3856=LINE('',#32116,#4704);
#3857=LINE('',#32133,#4705);
#3858=LINE('',#32145,#4706);
#3859=LINE('',#32165,#4707);
#3860=LINE('',#32219,#4708);
#3861=LINE('',#32267,#4709);
#3862=LINE('',#32318,#4710);
#3863=LINE('',#32369,#4711);
#3864=LINE('',#32417,#4712);
#3865=LINE('',#32456,#4713);
#3866=LINE('',#32482,#4714);
#3867=LINE('',#32507,#4715);
#3868=LINE('',#32532,#4716);
#3869=LINE('',#32556,#4717);
#3870=LINE('',#32581,#4718);
#3871=LINE('',#32606,#4719);
#3872=LINE('',#32623,#4720);
#3873=LINE('',#32635,#4721);
#3874=LINE('',#32655,#4722);
#3875=LINE('',#32709,#4723);
#3876=LINE('',#32757,#4724);
#3877=LINE('',#32808,#4725);
#3878=LINE('',#32859,#4726);
#3879=LINE('',#32907,#4727);
#3880=LINE('',#32946,#4728);
#3881=LINE('',#32972,#4729);
#3882=LINE('',#32997,#4730);
#3883=LINE('',#33022,#4731);
#3884=LINE('',#33046,#4732);
#3885=LINE('',#33071,#4733);
#3886=LINE('',#33096,#4734);
#3887=LINE('',#33113,#4735);
#3888=LINE('',#33125,#4736);
#3889=LINE('',#33145,#4737);
#3890=LINE('',#33199,#4738);
#3891=LINE('',#33247,#4739);
#3892=LINE('',#33298,#4740);
#3893=LINE('',#33349,#4741);
#3894=LINE('',#33397,#4742);
#3895=LINE('',#33436,#4743);
#3896=LINE('',#33462,#4744);
#3897=LINE('',#33487,#4745);
#3898=LINE('',#33512,#4746);
#3899=LINE('',#33536,#4747);
#3900=LINE('',#33561,#4748);
#3901=LINE('',#33586,#4749);
#3902=LINE('',#33603,#4750);
#3903=LINE('',#33647,#4751);
#3904=LINE('',#33695,#4752);
#3905=LINE('',#33779,#4753);
#3906=LINE('',#33854,#4754);
#3907=LINE('',#33923,#4755);
#3908=LINE('',#33948,#4756);
#3909=LINE('',#33985,#4757);
#3910=LINE('',#34019,#4758);
#3911=LINE('',#34055,#4759);
#3912=LINE('',#34075,#4760);
#3913=LINE('',#34119,#4761);
#3914=LINE('',#34167,#4762);
#3915=LINE('',#34251,#4763);
#3916=LINE('',#34326,#4764);
#3917=LINE('',#34395,#4765);
#3918=LINE('',#34420,#4766);
#3919=LINE('',#34457,#4767);
#3920=LINE('',#34491,#4768);
#3921=LINE('',#34527,#4769);
#3922=LINE('',#34547,#4770);
#3923=LINE('',#34591,#4771);
#3924=LINE('',#34639,#4772);
#3925=LINE('',#34723,#4773);
#3926=LINE('',#34798,#4774);
#3927=LINE('',#34867,#4775);
#3928=LINE('',#34892,#4776);
#3929=LINE('',#34929,#4777);
#3930=LINE('',#34963,#4778);
#3931=LINE('',#34999,#4779);
#3932=LINE('',#35019,#4780);
#3933=LINE('',#35063,#4781);
#3934=LINE('',#35111,#4782);
#3935=LINE('',#35195,#4783);
#3936=LINE('',#35270,#4784);
#3937=LINE('',#35339,#4785);
#3938=LINE('',#35364,#4786);
#3939=LINE('',#35401,#4787);
#3940=LINE('',#35435,#4788);
#3941=LINE('',#35471,#4789);
#3942=LINE('',#43248,#4790);
#3943=LINE('',#43255,#4791);
#3944=LINE('',#43261,#4792);
#3945=LINE('',#43269,#4793);
#3946=LINE('',#43344,#4794);
#3947=LINE('',#43431,#4795);
#3948=LINE('',#43518,#4796);
#3949=LINE('',#43605,#4797);
#3950=LINE('',#43695,#4798);
#3951=LINE('',#43782,#4799);
#3952=LINE('',#43869,#4800);
#3953=LINE('',#43956,#4801);
#3954=LINE('',#44043,#4802);
#3955=LINE('',#44133,#4803);
#3956=LINE('',#44220,#4804);
#3957=LINE('',#44307,#4805);
#3958=LINE('',#44394,#4806);
#3959=LINE('',#44481,#4807);
#3960=LINE('',#44568,#4808);
#3961=LINE('',#44655,#4809);
#3962=LINE('',#44742,#4810);
#3963=LINE('',#44829,#4811);
#3964=LINE('',#44916,#4812);
#3965=LINE('',#45003,#4813);
#3966=LINE('',#45093,#4814);
#3967=LINE('',#45180,#4815);
#3968=LINE('',#45267,#4816);
#3969=LINE('',#45354,#4817);
#3970=LINE('',#45441,#4818);
#3971=LINE('',#45531,#4819);
#3972=LINE('',#45618,#4820);
#3973=LINE('',#45687,#4821);
#3974=LINE('',#45709,#4822);
#3975=LINE('',#45747,#4823);
#3976=LINE('',#45783,#4824);
#3977=LINE('',#45821,#4825);
#3978=LINE('',#45858,#4826);
#3979=LINE('',#45895,#4827);
#3980=LINE('',#45933,#4828);
#3981=LINE('',#45969,#4829);
#3982=LINE('',#46007,#4830);
#3983=LINE('',#46044,#4831);
#3984=LINE('',#46081,#4832);
#3985=LINE('',#46119,#4833);
#3986=LINE('',#46155,#4834);
#3987=LINE('',#46193,#4835);
#3988=LINE('',#46230,#4836);
#3989=LINE('',#46267,#4837);
#3990=LINE('',#46305,#4838);
#3991=LINE('',#46341,#4839);
#3992=LINE('',#46379,#4840);
#3993=LINE('',#46415,#4841);
#3994=LINE('',#46453,#4842);
#3995=LINE('',#46491,#4843);
#3996=LINE('',#46527,#4844);
#3997=LINE('',#46565,#4845);
#3998=LINE('',#46601,#4846);
#3999=LINE('',#46639,#4847);
#4000=LINE('',#46677,#4848);
#4001=LINE('',#46713,#4849);
#4002=LINE('',#50235,#4850);
#4003=LINE('',#50237,#4851);
#4004=LINE('',#50239,#4852);
#4005=LINE('',#50241,#4853);
#4006=LINE('',#50243,#4854);
#4007=LINE('',#50245,#4855);
#4008=LINE('',#50247,#4856);
#4009=LINE('',#50248,#4857);
#4010=LINE('',#50253,#4858);
#4011=LINE('',#50255,#4859);
#4012=LINE('',#50257,#4860);
#4013=LINE('',#50258,#4861);
#4014=LINE('',#50262,#4862);
#4015=LINE('',#50263,#4863);
#4016=LINE('',#50264,#4864);
#4017=LINE('',#50266,#4865);
#4018=LINE('',#50267,#4866);
#4019=LINE('',#50270,#4867);
#4020=LINE('',#50271,#4868);
#4021=LINE('',#50274,#4869);
#4022=LINE('',#50275,#4870);
#4023=LINE('',#50278,#4871);
#4024=LINE('',#50279,#4872);
#4025=LINE('',#50282,#4873);
#4026=LINE('',#50283,#4874);
#4027=LINE('',#50286,#4875);
#4028=LINE('',#50287,#4876);
#4029=LINE('',#50290,#4877);
#4030=LINE('',#50291,#4878);
#4031=LINE('',#50293,#4879);
#4032=LINE('',#50300,#4880);
#4033=LINE('',#50306,#4881);
#4034=LINE('',#50311,#4882);
#4035=LINE('',#50315,#4883);
#4036=LINE('',#50320,#4884);
#4037=LINE('',#50324,#4885);
#4038=LINE('',#50328,#4886);
#4039=LINE('',#50330,#4887);
#4040=LINE('',#50332,#4888);
#4041=LINE('',#50334,#4889);
#4042=LINE('',#50336,#4890);
#4043=LINE('',#50338,#4891);
#4044=LINE('',#50340,#4892);
#4045=LINE('',#50342,#4893);
#4046=LINE('',#50343,#4894);
#4047=LINE('',#50344,#4895);
#4048=LINE('',#50349,#4896);
#4049=LINE('',#50351,#4897);
#4050=LINE('',#50353,#4898);
#4051=LINE('',#50355,#4899);
#4052=LINE('',#50357,#4900);
#4053=LINE('',#50359,#4901);
#4054=LINE('',#50360,#4902);
#4055=LINE('',#50363,#4903);
#4056=LINE('',#50365,#4904);
#4057=LINE('',#50367,#4905);
#4058=LINE('',#50369,#4906);
#4059=LINE('',#50371,#4907);
#4060=LINE('',#50373,#4908);
#4061=LINE('',#50374,#4909);
#4062=LINE('',#50376,#4910);
#4063=LINE('',#50380,#4911);
#4064=LINE('',#50386,#4912);
#4065=LINE('',#50389,#4913);
#4066=LINE('',#50392,#4914);
#4067=LINE('',#50393,#4915);
#4068=LINE('',#50395,#4916);
#4069=LINE('',#50396,#4917);
#4070=LINE('',#50398,#4918);
#4071=LINE('',#50400,#4919);
#4072=LINE('',#50401,#4920);
#4073=LINE('',#50404,#4921);
#4074=LINE('',#50405,#4922);
#4075=LINE('',#50407,#4923);
#4076=LINE('',#50410,#4924);
#4077=LINE('',#50412,#4925);
#4078=LINE('',#50415,#4926);
#4079=LINE('',#50416,#4927);
#4080=LINE('',#50419,#4928);
#4081=LINE('',#50420,#4929);
#4082=LINE('',#50422,#4930);
#4083=LINE('',#50428,#4931);
#4084=LINE('',#50461,#4932);
#4085=LINE('',#50545,#4933);
#4086=LINE('',#50635,#4934);
#4087=LINE('',#50719,#4935);
#4088=LINE('',#50809,#4936);
#4089=LINE('',#50899,#4937);
#4090=LINE('',#50983,#4938);
#4091=LINE('',#51073,#4939);
#4092=LINE('',#51157,#4940);
#4093=LINE('',#51247,#4941);
#4094=LINE('',#51331,#4942);
#4095=LINE('',#51421,#4943);
#4096=LINE('',#51511,#4944);
#4097=LINE('',#51595,#4945);
#4098=LINE('',#51685,#4946);
#4099=LINE('',#51769,#4947);
#4100=LINE('',#51859,#4948);
#4101=LINE('',#51943,#4949);
#4102=LINE('',#52030,#4950);
#4103=LINE('',#52120,#4951);
#4104=LINE('',#52204,#4952);
#4105=LINE('',#52294,#4953);
#4106=LINE('',#52378,#4954);
#4107=LINE('',#52468,#4955);
#4108=LINE('',#52555,#4956);
#4109=LINE('',#52642,#4957);
#4110=LINE('',#52732,#4958);
#4111=LINE('',#52816,#4959);
#4112=LINE('',#52906,#4960);
#4113=LINE('',#52990,#4961);
#4114=LINE('',#53080,#4962);
#4115=LINE('',#53167,#4963);
#4116=LINE('',#53254,#4964);
#4117=LINE('',#53344,#4965);
#4118=LINE('',#53428,#4966);
#4119=LINE('',#53519,#4967);
#4120=LINE('',#53537,#4968);
#4121=LINE('',#53562,#4969);
#4122=LINE('',#53597,#4970);
#4123=LINE('',#53634,#4971);
#4124=LINE('',#53671,#4972);
#4125=LINE('',#53708,#4973);
#4126=LINE('',#53746,#4974);
#4127=LINE('',#53782,#4975);
#4128=LINE('',#53820,#4976);
#4129=LINE('',#53857,#4977);
#4130=LINE('',#53894,#4978);
#4131=LINE('',#53931,#4979);
#4132=LINE('',#53968,#4980);
#4133=LINE('',#54006,#4981);
#4134=LINE('',#54042,#4982);
#4135=LINE('',#54080,#4983);
#4136=LINE('',#54117,#4984);
#4137=LINE('',#54154,#4985);
#4138=LINE('',#54191,#4986);
#4139=LINE('',#54228,#4987);
#4140=LINE('',#54266,#4988);
#4141=LINE('',#54302,#4989);
#4142=LINE('',#54340,#4990);
#4143=LINE('',#54377,#4991);
#4144=LINE('',#54414,#4992);
#4145=LINE('',#54451,#4993);
#4146=LINE('',#54488,#4994);
#4147=LINE('',#54526,#4995);
#4148=LINE('',#54563,#4996);
#4149=LINE('',#54600,#4997);
#4150=LINE('',#54637,#4998);
#4151=LINE('',#54674,#4999);
#4152=LINE('',#54711,#5000);
#4153=LINE('',#54748,#5001);
#4154=LINE('',#54786,#5002);
#4155=LINE('',#54823,#5003);
#4156=LINE('',#54860,#5004);
#4157=LINE('',#54897,#5005);
#4158=LINE('',#54899,#5006);
#4159=LINE('',#54901,#5007);
#4160=LINE('',#54902,#5008);
#4161=LINE('',#54905,#5009);
#4162=LINE('',#54907,#5010);
#4163=LINE('',#54908,#5011);
#4164=LINE('',#54911,#5012);
#4165=LINE('',#54913,#5013);
#4166=LINE('',#54914,#5014);
#4167=LINE('',#54917,#5015);
#4168=LINE('',#54919,#5016);
#4169=LINE('',#54920,#5017);
#4170=LINE('',#54923,#5018);
#4171=LINE('',#54925,#5019);
#4172=LINE('',#54926,#5020);
#4173=LINE('',#54928,#5021);
#4174=LINE('',#54929,#5022);
#4175=LINE('',#54935,#5023);
#4176=LINE('',#54944,#5024);
#4177=LINE('',#59232,#5025);
#4178=LINE('',#59239,#5026);
#4179=LINE('',#59241,#5027);
#4180=LINE('',#59243,#5028);
#4181=LINE('',#59244,#5029);
#4182=LINE('',#59248,#5030);
#4183=LINE('',#59250,#5031);
#4184=LINE('',#59252,#5032);
#4185=LINE('',#59253,#5033);
#4186=LINE('',#59267,#5034);
#4187=LINE('',#59273,#5035);
#4188=LINE('',#59282,#5036);
#4189=LINE('',#59288,#5037);
#4190=LINE('',#59296,#5038);
#4191=LINE('',#59320,#5039);
#4192=LINE('',#59368,#5040);
#4193=LINE('',#59416,#5041);
#4194=LINE('',#59467,#5042);
#4195=LINE('',#59518,#5043);
#4196=LINE('',#59566,#5044);
#4197=LINE('',#59614,#5045);
#4198=LINE('',#59668,#5046);
#4199=LINE('',#59716,#5047);
#4200=LINE('',#59764,#5048);
#4201=LINE('',#59815,#5049);
#4202=LINE('',#59866,#5050);
#4203=LINE('',#59914,#5051);
#4204=LINE('',#59965,#5052);
#4205=LINE('',#60016,#5053);
#4206=LINE('',#60064,#5054);
#4207=LINE('',#60115,#5055);
#4208=LINE('',#60163,#5056);
#4209=LINE('',#60214,#5057);
#4210=LINE('',#60262,#5058);
#4211=LINE('',#60313,#5059);
#4212=LINE('',#60364,#5060);
#4213=LINE('',#60412,#5061);
#4214=LINE('',#60463,#5062);
#4215=LINE('',#60511,#5063);
#4216=LINE('',#60562,#5064);
#4217=LINE('',#60613,#5065);
#4218=LINE('',#60661,#5066);
#4219=LINE('',#60712,#5067);
#4220=LINE('',#60763,#5068);
#4221=LINE('',#60811,#5069);
#4222=LINE('',#60859,#5070);
#4223=LINE('',#60910,#5071);
#4224=LINE('',#60961,#5072);
#4225=LINE('',#61009,#5073);
#4226=LINE('',#61060,#5074);
#4227=LINE('',#61111,#5075);
#4228=LINE('',#61159,#5076);
#4229=LINE('',#61207,#5077);
#4230=LINE('',#61232,#5078);
#4231=LINE('',#61257,#5079);
#4232=LINE('',#61281,#5080);
#4233=LINE('',#61305,#5081);
#4234=LINE('',#61331,#5082);
#4235=LINE('',#61355,#5083);
#4236=LINE('',#61379,#5084);
#4237=LINE('',#61405,#5085);
#4238=LINE('',#61429,#5086);
#4239=LINE('',#61453,#5087);
#4240=LINE('',#61477,#5088);
#4241=LINE('',#61503,#5089);
#4242=LINE('',#61527,#5090);
#4243=LINE('',#61551,#5091);
#4244=LINE('',#61577,#5092);
#4245=LINE('',#61601,#5093);
#4246=LINE('',#61625,#5094);
#4247=LINE('',#61650,#5095);
#4248=LINE('',#61675,#5096);
#4249=LINE('',#61699,#5097);
#4250=LINE('',#61724,#5098);
#4251=LINE('',#61749,#5099);
#4252=LINE('',#61773,#5100);
#4253=LINE('',#61797,#5101);
#4254=LINE('',#61822,#5102);
#4255=LINE('',#61847,#5103);
#4256=LINE('',#61871,#5104);
#4257=LINE('',#61896,#5105);
#4258=LINE('',#61921,#5106);
#4259=LINE('',#61945,#5107);
#4260=LINE('',#61970,#5108);
#4261=LINE('',#61994,#5109);
#4262=LINE('',#62019,#5110);
#4263=LINE('',#62044,#5111);
#4264=LINE('',#62068,#5112);
#4265=LINE('',#62093,#5113);
#4266=LINE('',#62117,#5114);
#4267=LINE('',#62142,#5115);
#4268=LINE('',#62490,#5116);
#4269=LINE('',#64771,#5117);
#4270=LINE('',#64773,#5118);
#4271=LINE('',#64775,#5119);
#4272=LINE('',#64776,#5120);
#4273=LINE('',#64779,#5121);
#4274=LINE('',#64781,#5122);
#4275=LINE('',#64782,#5123);
#4276=LINE('',#64785,#5124);
#4277=LINE('',#64787,#5125);
#4278=LINE('',#64788,#5126);
#4279=LINE('',#64791,#5127);
#4280=LINE('',#64793,#5128);
#4281=LINE('',#64794,#5129);
#4282=LINE('',#64797,#5130);
#4283=LINE('',#64799,#5131);
#4284=LINE('',#64800,#5132);
#4285=LINE('',#64802,#5133);
#4286=LINE('',#64803,#5134);
#4287=LINE('',#64810,#5135);
#4288=LINE('',#64819,#5136);
#4289=LINE('',#64825,#5137);
#4290=LINE('',#64833,#5138);
#4291=LINE('',#64857,#5139);
#4292=LINE('',#64905,#5140);
#4293=LINE('',#64953,#5141);
#4294=LINE('',#65004,#5142);
#4295=LINE('',#65055,#5143);
#4296=LINE('',#65103,#5144);
#4297=LINE('',#65151,#5145);
#4298=LINE('',#65202,#5146);
#4299=LINE('',#65250,#5147);
#4300=LINE('',#65298,#5148);
#4301=LINE('',#65349,#5149);
#4302=LINE('',#65400,#5150);
#4303=LINE('',#65448,#5151);
#4304=LINE('',#65499,#5152);
#4305=LINE('',#65550,#5153);
#4306=LINE('',#65598,#5154);
#4307=LINE('',#65649,#5155);
#4308=LINE('',#65697,#5156);
#4309=LINE('',#65748,#5157);
#4310=LINE('',#65799,#5158);
#4311=LINE('',#65847,#5159);
#4312=LINE('',#65898,#5160);
#4313=LINE('',#65949,#5161);
#4314=LINE('',#65997,#5162);
#4315=LINE('',#66045,#5163);
#4316=LINE('',#66096,#5164);
#4317=LINE('',#66147,#5165);
#4318=LINE('',#66195,#5166);
#4319=LINE('',#66246,#5167);
#4320=LINE('',#66297,#5168);
#4321=LINE('',#66345,#5169);
#4322=LINE('',#66395,#5170);
#4323=LINE('',#66406,#5171);
#4324=LINE('',#66432,#5172);
#4325=LINE('',#66456,#5173);
#4326=LINE('',#66480,#5174);
#4327=LINE('',#66506,#5175);
#4328=LINE('',#66530,#5176);
#4329=LINE('',#66554,#5177);
#4330=LINE('',#66580,#5178);
#4331=LINE('',#66604,#5179);
#4332=LINE('',#66628,#5180);
#4333=LINE('',#66652,#5181);
#4334=LINE('',#66678,#5182);
#4335=LINE('',#66702,#5183);
#4336=LINE('',#66726,#5184);
#4337=LINE('',#66752,#5185);
#4338=LINE('',#66776,#5186);
#4339=LINE('',#66800,#5187);
#4340=LINE('',#66825,#5188);
#4341=LINE('',#66850,#5189);
#4342=LINE('',#66874,#5190);
#4343=LINE('',#66899,#5191);
#4344=LINE('',#66924,#5192);
#4345=LINE('',#66948,#5193);
#4346=LINE('',#66973,#5194);
#4347=LINE('',#66997,#5195);
#4348=LINE('',#67022,#5196);
#4349=LINE('',#67046,#5197);
#4350=LINE('',#67071,#5198);
#4351=LINE('',#67096,#5199);
#4352=LINE('',#67120,#5200);
#4353=LINE('',#67145,#5201);
#4354=LINE('',#67168,#5202);
#4355=LINE('',#67431,#5203);
#4356=LINE('',#69373,#5204);
#4357=LINE('',#69375,#5205);
#4358=LINE('',#69377,#5206);
#4359=LINE('',#69378,#5207);
#4360=LINE('',#69381,#5208);
#4361=LINE('',#69383,#5209);
#4362=LINE('',#69384,#5210);
#4363=LINE('',#69387,#5211);
#4364=LINE('',#69389,#5212);
#4365=LINE('',#69390,#5213);
#4366=LINE('',#69393,#5214);
#4367=LINE('',#69395,#5215);
#4368=LINE('',#69396,#5216);
#4369=LINE('',#69399,#5217);
#4370=LINE('',#69401,#5218);
#4371=LINE('',#69402,#5219);
#4372=LINE('',#69404,#5220);
#4373=LINE('',#69405,#5221);
#4374=LINE('',#69412,#5222);
#4375=VECTOR('',#15869,3.);
#4376=VECTOR('',#15872,3.);
#4377=VECTOR('',#15879,3.);
#4378=VECTOR('',#15882,3.);
#4379=VECTOR('',#15885,3.);
#4380=VECTOR('',#15888,3.);
#4381=VECTOR('',#15891,3.);
#4382=VECTOR('',#15894,3.);
#4383=VECTOR('',#15897,3.);
#4384=VECTOR('',#15900,3.);
#4385=VECTOR('',#15905,3.0735);
#4386=VECTOR('',#15910,3.0735);
#4387=VECTOR('',#15913,3.0735);
#4388=VECTOR('',#15916,3.0735);
#4389=VECTOR('',#15919,3.0735);
#4390=VECTOR('',#15922,3.0735);
#4391=VECTOR('',#15925,3.0735);
#4392=VECTOR('',#15928,3.0735);
#4393=VECTOR('',#15931,3.0735);
#4394=VECTOR('',#15936,3.);
#4395=VECTOR('',#15939,3.);
#4396=VECTOR('',#15946,3.);
#4397=VECTOR('',#15949,3.);
#4398=VECTOR('',#15952,3.);
#4399=VECTOR('',#15955,3.);
#4400=VECTOR('',#15958,3.);
#4401=VECTOR('',#15961,3.);
#4402=VECTOR('',#15964,3.);
#4403=VECTOR('',#15967,3.);
#4404=VECTOR('',#15972,3.0735);
#4405=VECTOR('',#15977,3.0735);
#4406=VECTOR('',#15980,3.0735);
#4407=VECTOR('',#15983,3.0735);
#4408=VECTOR('',#15986,3.0735);
#4409=VECTOR('',#15989,3.0735);
#4410=VECTOR('',#15992,3.0735);
#4411=VECTOR('',#15995,3.0735);
#4412=VECTOR('',#15998,3.0735);
#4413=VECTOR('',#16003,3.);
#4414=VECTOR('',#16006,3.);
#4415=VECTOR('',#16013,3.);
#4416=VECTOR('',#16016,3.);
#4417=VECTOR('',#16019,3.);
#4418=VECTOR('',#16022,3.);
#4419=VECTOR('',#16025,3.);
#4420=VECTOR('',#16028,3.);
#4421=VECTOR('',#16031,3.);
#4422=VECTOR('',#16034,3.);
#4423=VECTOR('',#16039,3.0735);
#4424=VECTOR('',#16044,3.0735);
#4425=VECTOR('',#16047,3.0735);
#4426=VECTOR('',#16050,3.0735);
#4427=VECTOR('',#16053,3.0735);
#4428=VECTOR('',#16056,3.0735);
#4429=VECTOR('',#16059,3.0735);
#4430=VECTOR('',#16062,3.0735);
#4431=VECTOR('',#16065,3.0735);
#4432=VECTOR('',#16070,3.);
#4433=VECTOR('',#16073,3.);
#4434=VECTOR('',#16080,3.);
#4435=VECTOR('',#16083,3.);
#4436=VECTOR('',#16086,3.);
#4437=VECTOR('',#16089,3.);
#4438=VECTOR('',#16092,3.);
#4439=VECTOR('',#16095,3.);
#4440=VECTOR('',#16098,3.);
#4441=VECTOR('',#16101,3.);
#4442=VECTOR('',#16106,3.0735);
#4443=VECTOR('',#16111,3.0735);
#4444=VECTOR('',#16114,3.0735);
#4445=VECTOR('',#16117,3.0735);
#4446=VECTOR('',#16120,3.0735);
#4447=VECTOR('',#16123,3.0735);
#4448=VECTOR('',#16126,3.0735);
#4449=VECTOR('',#16129,3.0735);
#4450=VECTOR('',#16132,3.0735);
#4451=VECTOR('',#16137,3.);
#4452=VECTOR('',#16140,3.);
#4453=VECTOR('',#16147,3.);
#4454=VECTOR('',#16150,3.);
#4455=VECTOR('',#16153,3.);
#4456=VECTOR('',#16156,3.);
#4457=VECTOR('',#16159,3.);
#4458=VECTOR('',#16162,3.);
#4459=VECTOR('',#16165,3.);
#4460=VECTOR('',#16168,3.);
#4461=VECTOR('',#16173,3.0735);
#4462=VECTOR('',#16178,3.0735);
#4463=VECTOR('',#16181,3.0735);
#4464=VECTOR('',#16184,3.0735);
#4465=VECTOR('',#16187,3.0735);
#4466=VECTOR('',#16190,3.0735);
#4467=VECTOR('',#16193,3.0735);
#4468=VECTOR('',#16196,3.0735);
#4469=VECTOR('',#16199,3.0735);
#4470=VECTOR('',#16204,3.);
#4471=VECTOR('',#16207,3.);
#4472=VECTOR('',#16214,3.);
#4473=VECTOR('',#16217,3.);
#4474=VECTOR('',#16220,3.);
#4475=VECTOR('',#16223,3.);
#4476=VECTOR('',#16226,3.);
#4477=VECTOR('',#16229,3.);
#4478=VECTOR('',#16232,3.);
#4479=VECTOR('',#16235,3.);
#4480=VECTOR('',#16240,3.0735);
#4481=VECTOR('',#16245,3.0735);
#4482=VECTOR('',#16248,3.0735);
#4483=VECTOR('',#16251,3.0735);
#4484=VECTOR('',#16254,3.0735);
#4485=VECTOR('',#16257,3.0735);
#4486=VECTOR('',#16260,3.0735);
#4487=VECTOR('',#16263,3.0735);
#4488=VECTOR('',#16266,3.0735);
#4489=VECTOR('',#16271,3.);
#4490=VECTOR('',#16274,3.);
#4491=VECTOR('',#16281,3.);
#4492=VECTOR('',#16284,3.);
#4493=VECTOR('',#16287,3.);
#4494=VECTOR('',#16290,3.);
#4495=VECTOR('',#16293,3.);
#4496=VECTOR('',#16296,3.);
#4497=VECTOR('',#16299,3.);
#4498=VECTOR('',#16302,3.);
#4499=VECTOR('',#16307,3.0735);
#4500=VECTOR('',#16312,3.0735);
#4501=VECTOR('',#16315,3.0735);
#4502=VECTOR('',#16318,3.0735);
#4503=VECTOR('',#16321,3.0735);
#4504=VECTOR('',#16324,3.0735);
#4505=VECTOR('',#16327,3.0735);
#4506=VECTOR('',#16330,3.0735);
#4507=VECTOR('',#16333,3.0735);
#4508=VECTOR('',#16338,3.);
#4509=VECTOR('',#16341,3.);
#4510=VECTOR('',#16348,3.);
#4511=VECTOR('',#16351,3.);
#4512=VECTOR('',#16354,3.);
#4513=VECTOR('',#16357,3.);
#4514=VECTOR('',#16360,3.);
#4515=VECTOR('',#16363,3.);
#4516=VECTOR('',#16366,3.);
#4517=VECTOR('',#16369,3.);
#4518=VECTOR('',#16374,3.0735);
#4519=VECTOR('',#16379,3.0735);
#4520=VECTOR('',#16382,3.0735);
#4521=VECTOR('',#16385,3.0735);
#4522=VECTOR('',#16388,3.0735);
#4523=VECTOR('',#16391,3.0735);
#4524=VECTOR('',#16394,3.0735);
#4525=VECTOR('',#16397,3.0735);
#4526=VECTOR('',#16400,3.0735);
#4527=VECTOR('',#16407,7.);
#4528=VECTOR('',#16418,7.);
#4529=VECTOR('',#16429,7.);
#4530=VECTOR('',#16440,7.);
#4531=VECTOR('',#16449,4.5);
#4532=VECTOR('',#16454,4.5);
#4533=VECTOR('',#16459,4.5);
#4534=VECTOR('',#16464,4.5);
#4535=VECTOR('',#16517,10.);
#4536=VECTOR('',#16518,10.);
#4537=VECTOR('',#16519,10.);
#4538=VECTOR('',#16520,10.);
#4539=VECTOR('',#16523,10.);
#4540=VECTOR('',#16524,10.);
#4541=VECTOR('',#16525,10.);
#4542=VECTOR('',#16526,10.);
#4543=VECTOR('',#16527,10.);
#4544=VECTOR('',#16528,10.);
#4545=VECTOR('',#16529,10.);
#4546=VECTOR('',#16530,10.);
#4547=VECTOR('',#16531,10.);
#4548=VECTOR('',#16532,10.);
#4549=VECTOR('',#16533,10.);
#4550=VECTOR('',#16536,10.);
#4551=VECTOR('',#16537,10.);
#4552=VECTOR('',#16538,10.);
#4553=VECTOR('',#16545,10.);
#4554=VECTOR('',#16546,10.);
#4555=VECTOR('',#16547,10.);
#4556=VECTOR('',#16548,10.);
#4557=VECTOR('',#16549,10.);
#4558=VECTOR('',#16550,10.);
#4559=VECTOR('',#16551,10.);
#4560=VECTOR('',#16552,10.);
#4561=VECTOR('',#16553,10.);
#4562=VECTOR('',#16554,10.);
#4563=VECTOR('',#16555,10.);
#4564=VECTOR('',#16556,10.);
#4565=VECTOR('',#16559,10.);
#4566=VECTOR('',#16560,10.);
#4567=VECTOR('',#16561,10.);
#4568=VECTOR('',#16564,10.);
#4569=VECTOR('',#16565,10.);
#4570=VECTOR('',#16566,10.);
#4571=VECTOR('',#16573,10.);
#4572=VECTOR('',#16574,10.);
#4573=VECTOR('',#16577,10.);
#4574=VECTOR('',#16578,10.);
#4575=VECTOR('',#16581,10.);
#4576=VECTOR('',#16582,10.);
#4577=VECTOR('',#16587,10.);
#4578=VECTOR('',#16588,10.);
#4579=VECTOR('',#16589,10.);
#4580=VECTOR('',#16590,10.);
#4581=VECTOR('',#16593,10.);
#4582=VECTOR('',#16594,10.);
#4583=VECTOR('',#16597,10.);
#4584=VECTOR('',#16598,10.);
#4585=VECTOR('',#16601,10.);
#4586=VECTOR('',#16602,10.);
#4587=VECTOR('',#16603,10.);
#4588=VECTOR('',#16604,10.);
#4589=VECTOR('',#16609,10.);
#4590=VECTOR('',#16610,10.);
#4591=VECTOR('',#16613,10.);
#4592=VECTOR('',#16616,10.);
#4593=VECTOR('',#16617,10.);
#4594=VECTOR('',#16620,10.);
#4595=VECTOR('',#16621,10.);
#4596=VECTOR('',#16624,10.);
#4597=VECTOR('',#16625,10.);
#4598=VECTOR('',#16628,10.);
#4599=VECTOR('',#16629,10.);
#4600=VECTOR('',#16632,10.);
#4601=VECTOR('',#16633,10.);
#4602=VECTOR('',#16638,10.);
#4603=VECTOR('',#16639,10.);
#4604=VECTOR('',#16640,10.);
#4605=VECTOR('',#16641,10.);
#4606=VECTOR('',#16644,10.);
#4607=VECTOR('',#16647,10.);
#4608=VECTOR('',#16648,10.);
#4609=VECTOR('',#16651,10.);
#4610=VECTOR('',#16652,10.);
#4611=VECTOR('',#16655,10.);
#4612=VECTOR('',#16656,10.);
#4613=VECTOR('',#16657,10.);
#4614=VECTOR('',#16660,10.);
#4615=VECTOR('',#16663,10.);
#4616=VECTOR('',#16664,10.);
#4617=VECTOR('',#16665,10.);
#4618=VECTOR('',#16668,10.);
#4619=VECTOR('',#16671,10.);
#4620=VECTOR('',#16672,10.);
#4621=VECTOR('',#16673,10.);
#4622=VECTOR('',#16676,20.);
#4623=VECTOR('',#16681,10.);
#4624=VECTOR('',#16684,10.);
#4625=VECTOR('',#16685,10.);
#4626=VECTOR('',#16688,10.);
#4627=VECTOR('',#16693,10.);
#4628=VECTOR('',#16696,10.);
#4629=VECTOR('',#16697,10.);
#4630=VECTOR('',#16698,10.);
#4631=VECTOR('',#16701,10.);
#4632=VECTOR('',#16704,10.);
#4633=VECTOR('',#16705,10.);
#4634=VECTOR('',#16706,10.);
#4635=VECTOR('',#16711,10.);
#4636=VECTOR('',#16712,10.);
#4637=VECTOR('',#16717,10.);
#4638=VECTOR('',#16718,10.);
#4639=VECTOR('',#16719,10.);
#4640=VECTOR('',#16720,10.);
#4641=VECTOR('',#16721,10.);
#4642=VECTOR('',#16722,10.);
#4643=VECTOR('',#16723,10.);
#4644=VECTOR('',#16724,10.);
#4645=VECTOR('',#16727,10.);
#4646=VECTOR('',#16730,10.);
#4647=VECTOR('',#16731,10.);
#4648=VECTOR('',#16732,10.);
#4649=VECTOR('',#16735,10.);
#4650=VECTOR('',#16736,10.);
#4651=VECTOR('',#16737,10.);
#4652=VECTOR('',#16738,10.);
#4653=VECTOR('',#16739,10.);
#4654=VECTOR('',#16740,10.);
#4655=VECTOR('',#16741,10.);
#4656=VECTOR('',#16742,10.);
#4657=VECTOR('',#16743,10.);
#4658=VECTOR('',#16744,10.);
#4659=VECTOR('',#16747,10.);
#4660=VECTOR('',#16748,10.);
#4661=VECTOR('',#16749,10.);
#4662=VECTOR('',#16756,10.);
#4663=VECTOR('',#16757,10.);
#4664=VECTOR('',#16760,10.);
#4665=VECTOR('',#16761,10.);
#4666=VECTOR('',#16764,10.);
#4667=VECTOR('',#16767,100.);
#4668=VECTOR('',#16774,10.);
#4669=VECTOR('',#16775,10.);
#4670=VECTOR('',#16778,10.);
#4671=VECTOR('',#16779,10.);
#4672=VECTOR('',#16782,10.);
#4673=VECTOR('',#16783,10.);
#4674=VECTOR('',#16786,10.);
#4675=VECTOR('',#16789,10.);
#4676=VECTOR('',#16790,10.);
#4677=VECTOR('',#16791,10.);
#4678=VECTOR('',#16794,10.);
#4679=VECTOR('',#16797,10.);
#4680=VECTOR('',#16798,10.);
#4681=VECTOR('',#16799,10.);
#4682=VECTOR('',#16802,10.);
#4683=VECTOR('',#16803,10.);
#4684=VECTOR('',#16804,10.);
#4685=VECTOR('',#16809,10.);
#4686=VECTOR('',#16810,10.);
#4687=VECTOR('',#16815,10.);
#4688=VECTOR('',#16822,10.);
#4689=VECTOR('',#16829,40.);
#4690=VECTOR('',#16840,4.);
#4691=VECTOR('',#16843,4.);
#4692=VECTOR('',#16850,4.);
#4693=VECTOR('',#16853,4.);
#4694=VECTOR('',#16856,4.);
#4695=VECTOR('',#16859,4.);
#4696=VECTOR('',#16862,4.);
#4697=VECTOR('',#16865,4.);
#4698=VECTOR('',#16870,4.085);
#4699=VECTOR('',#16875,4.085);
#4700=VECTOR('',#16878,4.085);
#4701=VECTOR('',#16881,4.085);
#4702=VECTOR('',#16884,4.085);
#4703=VECTOR('',#16887,4.085);
#4704=VECTOR('',#16890,4.085);
#4705=VECTOR('',#16895,4.);
#4706=VECTOR('',#16898,4.);
#4707=VECTOR('',#16905,4.);
#4708=VECTOR('',#16908,4.);
#4709=VECTOR('',#16911,4.);
#4710=VECTOR('',#16914,4.);
#4711=VECTOR('',#16917,4.);
#4712=VECTOR('',#16920,4.);
#4713=VECTOR('',#16925,4.085);
#4714=VECTOR('',#16930,4.085);
#4715=VECTOR('',#16933,4.085);
#4716=VECTOR('',#16936,4.085);
#4717=VECTOR('',#16939,4.085);
#4718=VECTOR('',#16942,4.085);
#4719=VECTOR('',#16945,4.085);
#4720=VECTOR('',#16950,4.);
#4721=VECTOR('',#16953,4.);
#4722=VECTOR('',#16960,4.);
#4723=VECTOR('',#16963,4.);
#4724=VECTOR('',#16966,4.);
#4725=VECTOR('',#16969,4.);
#4726=VECTOR('',#16972,4.);
#4727=VECTOR('',#16975,4.);
#4728=VECTOR('',#16980,4.085);
#4729=VECTOR('',#16985,4.085);
#4730=VECTOR('',#16988,4.085);
#4731=VECTOR('',#16991,4.085);
#4732=VECTOR('',#16994,4.085);
#4733=VECTOR('',#16997,4.085);
#4734=VECTOR('',#17000,4.085);
#4735=VECTOR('',#17005,4.);
#4736=VECTOR('',#17008,4.);
#4737=VECTOR('',#17015,4.);
#4738=VECTOR('',#17018,4.);
#4739=VECTOR('',#17021,4.);
#4740=VECTOR('',#17024,4.);
#4741=VECTOR('',#17027,4.);
#4742=VECTOR('',#17030,4.);
#4743=VECTOR('',#17035,4.085);
#4744=VECTOR('',#17040,4.085);
#4745=VECTOR('',#17043,4.085);
#4746=VECTOR('',#17046,4.085);
#4747=VECTOR('',#17049,4.085);
#4748=VECTOR('',#17052,4.085);
#4749=VECTOR('',#17055,4.085);
#4750=VECTOR('',#17060,5.);
#4751=VECTOR('',#17063,5.);
#4752=VECTOR('',#17068,5.);
#4753=VECTOR('',#17071,5.);
#4754=VECTOR('',#17074,5.);
#4755=VECTOR('',#17079,5.099);
#4756=VECTOR('',#17084,5.099);
#4757=VECTOR('',#17087,5.099);
#4758=VECTOR('',#17090,5.099);
#4759=VECTOR('',#17093,5.099);
#4760=VECTOR('',#17098,5.);
#4761=VECTOR('',#17101,5.);
#4762=VECTOR('',#17106,5.);
#4763=VECTOR('',#17109,5.);
#4764=VECTOR('',#17112,5.);
#4765=VECTOR('',#17117,5.099);
#4766=VECTOR('',#17122,5.099);
#4767=VECTOR('',#17125,5.099);
#4768=VECTOR('',#17128,5.099);
#4769=VECTOR('',#17131,5.099);
#4770=VECTOR('',#17136,5.);
#4771=VECTOR('',#17139,5.);
#4772=VECTOR('',#17144,5.);
#4773=VECTOR('',#17147,5.);
#4774=VECTOR('',#17150,5.);
#4775=VECTOR('',#17155,5.099);
#4776=VECTOR('',#17160,5.099);
#4777=VECTOR('',#17163,5.099);
#4778=VECTOR('',#17166,5.099);
#4779=VECTOR('',#17169,5.099);
#4780=VECTOR('',#17174,5.);
#4781=VECTOR('',#17177,5.);
#4782=VECTOR('',#17182,5.);
#4783=VECTOR('',#17185,5.);
#4784=VECTOR('',#17188,5.);
#4785=VECTOR('',#17193,5.099);
#4786=VECTOR('',#17198,5.099);
#4787=VECTOR('',#17201,5.099);
#4788=VECTOR('',#17204,5.099);
#4789=VECTOR('',#17207,5.099);
#4790=VECTOR('',#17270,40.);
#4791=VECTOR('',#17279,20.);
#4792=VECTOR('',#17286,100.);
#4793=VECTOR('',#17297,6.);
#4794=VECTOR('',#17302,6.);
#4795=VECTOR('',#17305,6.);
#4796=VECTOR('',#17308,6.);
#4797=VECTOR('',#17311,6.);
#4798=VECTOR('',#17314,6.);
#4799=VECTOR('',#17317,6.);
#4800=VECTOR('',#17320,6.);
#4801=VECTOR('',#17323,6.);
#4802=VECTOR('',#17326,6.);
#4803=VECTOR('',#17329,6.);
#4804=VECTOR('',#17332,6.);
#4805=VECTOR('',#17335,6.);
#4806=VECTOR('',#17338,6.);
#4807=VECTOR('',#17341,6.);
#4808=VECTOR('',#17344,6.);
#4809=VECTOR('',#17347,6.);
#4810=VECTOR('',#17350,6.);
#4811=VECTOR('',#17353,6.);
#4812=VECTOR('',#17356,6.);
#4813=VECTOR('',#17359,6.);
#4814=VECTOR('',#17362,6.);
#4815=VECTOR('',#17365,6.);
#4816=VECTOR('',#17368,6.);
#4817=VECTOR('',#17371,6.);
#4818=VECTOR('',#17374,6.);
#4819=VECTOR('',#17377,6.);
#4820=VECTOR('',#17380,6.);
#4821=VECTOR('',#17385,6.11325);
#4822=VECTOR('',#17390,6.11325);
#4823=VECTOR('',#17393,6.11325);
#4824=VECTOR('',#17396,6.11325);
#4825=VECTOR('',#17399,6.11325);
#4826=VECTOR('',#17402,6.11325);
#4827=VECTOR('',#17405,6.11325);
#4828=VECTOR('',#17408,6.11325);
#4829=VECTOR('',#17411,6.11325);
#4830=VECTOR('',#17414,6.11325);
#4831=VECTOR('',#17417,6.11325);
#4832=VECTOR('',#17420,6.11325);
#4833=VECTOR('',#17423,6.11325);
#4834=VECTOR('',#17426,6.11325);
#4835=VECTOR('',#17429,6.11325);
#4836=VECTOR('',#17432,6.11325);
#4837=VECTOR('',#17435,6.11325);
#4838=VECTOR('',#17438,6.11325);
#4839=VECTOR('',#17441,6.11325);
#4840=VECTOR('',#17444,6.11325);
#4841=VECTOR('',#17447,6.11325);
#4842=VECTOR('',#17450,6.11325);
#4843=VECTOR('',#17453,6.11325);
#4844=VECTOR('',#17456,6.11325);
#4845=VECTOR('',#17459,6.11325);
#4846=VECTOR('',#17462,6.11325);
#4847=VECTOR('',#17465,6.11325);
#4848=VECTOR('',#17468,6.11325);
#4849=VECTOR('',#17471,6.11325);
#4850=VECTOR('',#17478,10.);
#4851=VECTOR('',#17479,10.);
#4852=VECTOR('',#17480,10.);
#4853=VECTOR('',#17481,10.);
#4854=VECTOR('',#17482,10.);
#4855=VECTOR('',#17483,10.);
#4856=VECTOR('',#17484,10.);
#4857=VECTOR('',#17485,10.);
#4858=VECTOR('',#17490,10.);
#4859=VECTOR('',#17491,10.);
#4860=VECTOR('',#17492,10.);
#4861=VECTOR('',#17493,10.);
#4862=VECTOR('',#17496,10.);
#4863=VECTOR('',#17497,10.);
#4864=VECTOR('',#17498,10.);
#4865=VECTOR('',#17501,10.);
#4866=VECTOR('',#17502,10.);
#4867=VECTOR('',#17505,10.);
#4868=VECTOR('',#17506,10.);
#4869=VECTOR('',#17509,10.);
#4870=VECTOR('',#17510,10.);
#4871=VECTOR('',#17513,10.);
#4872=VECTOR('',#17514,10.);
#4873=VECTOR('',#17517,10.);
#4874=VECTOR('',#17518,10.);
#4875=VECTOR('',#17521,10.);
#4876=VECTOR('',#17522,10.);
#4877=VECTOR('',#17525,10.);
#4878=VECTOR('',#17526,10.);
#4879=VECTOR('',#17529,10.);
#4880=VECTOR('',#17538,3.5);
#4881=VECTOR('',#17545,3.5);
#4882=VECTOR('',#17550,10.);
#4883=VECTOR('',#17553,10.);
#4884=VECTOR('',#17558,10.);
#4885=VECTOR('',#17561,10.);
#4886=VECTOR('',#17566,10.);
#4887=VECTOR('',#17567,10.);
#4888=VECTOR('',#17568,10.);
#4889=VECTOR('',#17569,10.);
#4890=VECTOR('',#17570,10.);
#4891=VECTOR('',#17571,10.);
#4892=VECTOR('',#17572,10.);
#4893=VECTOR('',#17573,10.);
#4894=VECTOR('',#17574,10.);
#4895=VECTOR('',#17575,10.);
#4896=VECTOR('',#17580,10.);
#4897=VECTOR('',#17581,10.);
#4898=VECTOR('',#17582,10.);
#4899=VECTOR('',#17583,10.);
#4900=VECTOR('',#17584,10.);
#4901=VECTOR('',#17585,10.);
#4902=VECTOR('',#17586,10.);
#4903=VECTOR('',#17589,10.);
#4904=VECTOR('',#17590,10.);
#4905=VECTOR('',#17591,10.);
#4906=VECTOR('',#17592,10.);
#4907=VECTOR('',#17593,10.);
#4908=VECTOR('',#17594,10.);
#4909=VECTOR('',#17595,10.);
#4910=VECTOR('',#17598,10.);
#4911=VECTOR('',#17601,10.);
#4912=VECTOR('',#17608,10.);
#4913=VECTOR('',#17611,10.);
#4914=VECTOR('',#17614,10.);
#4915=VECTOR('',#17615,10.);
#4916=VECTOR('',#17616,10.);
#4917=VECTOR('',#17617,10.);
#4918=VECTOR('',#17620,7.);
#4919=VECTOR('',#17623,10.);
#4920=VECTOR('',#17624,10.);
#4921=VECTOR('',#17629,10.);
#4922=VECTOR('',#17630,10.);
#4923=VECTOR('',#17633,10.);
#4924=VECTOR('',#17638,10.);
#4925=VECTOR('',#17641,10.);
#4926=VECTOR('',#17644,10.);
#4927=VECTOR('',#17645,10.);
#4928=VECTOR('',#17648,10.);
#4929=VECTOR('',#17649,10.);
#4930=VECTOR('',#17652,10.);
#4931=VECTOR('',#17659,6.);
#4932=VECTOR('',#17664,6.);
#4933=VECTOR('',#17667,6.);
#4934=VECTOR('',#17670,6.);
#4935=VECTOR('',#17673,6.);
#4936=VECTOR('',#17676,6.);
#4937=VECTOR('',#17679,6.);
#4938=VECTOR('',#17682,6.);
#4939=VECTOR('',#17685,6.);
#4940=VECTOR('',#17688,6.);
#4941=VECTOR('',#17691,6.);
#4942=VECTOR('',#17694,6.);
#4943=VECTOR('',#17697,6.);
#4944=VECTOR('',#17700,6.);
#4945=VECTOR('',#17703,6.);
#4946=VECTOR('',#17706,6.);
#4947=VECTOR('',#17709,6.);
#4948=VECTOR('',#17712,6.);
#4949=VECTOR('',#17715,6.);
#4950=VECTOR('',#17718,6.);
#4951=VECTOR('',#17721,6.);
#4952=VECTOR('',#17724,6.);
#4953=VECTOR('',#17727,6.);
#4954=VECTOR('',#17730,6.);
#4955=VECTOR('',#17733,6.);
#4956=VECTOR('',#17736,6.);
#4957=VECTOR('',#17739,6.);
#4958=VECTOR('',#17742,6.);
#4959=VECTOR('',#17745,6.);
#4960=VECTOR('',#17748,6.);
#4961=VECTOR('',#17751,6.);
#4962=VECTOR('',#17754,6.);
#4963=VECTOR('',#17757,6.);
#4964=VECTOR('',#17760,6.);
#4965=VECTOR('',#17763,6.);
#4966=VECTOR('',#17766,6.);
#4967=VECTOR('',#17771,6.);
#4968=VECTOR('',#17774,6.);
#4969=VECTOR('',#17779,4.91825);
#4970=VECTOR('',#17784,4.91825);
#4971=VECTOR('',#17787,4.91825);
#4972=VECTOR('',#17790,4.91825);
#4973=VECTOR('',#17793,4.91825);
#4974=VECTOR('',#17796,4.91825);
#4975=VECTOR('',#17799,4.91825);
#4976=VECTOR('',#17802,4.91825);
#4977=VECTOR('',#17805,4.91825);
#4978=VECTOR('',#17808,4.91825);
#4979=VECTOR('',#17811,4.91825);
#4980=VECTOR('',#17814,4.91825);
#4981=VECTOR('',#17817,4.91825);
#4982=VECTOR('',#17820,4.91825);
#4983=VECTOR('',#17823,4.91825);
#4984=VECTOR('',#17826,4.91825);
#4985=VECTOR('',#17829,4.91825);
#4986=VECTOR('',#17832,4.91825);
#4987=VECTOR('',#17835,4.91825);
#4988=VECTOR('',#17838,4.91825);
#4989=VECTOR('',#17841,4.91825);
#4990=VECTOR('',#17844,4.91825);
#4991=VECTOR('',#17847,4.91825);
#4992=VECTOR('',#17850,4.91825);
#4993=VECTOR('',#17853,4.91825);
#4994=VECTOR('',#17856,4.91825);
#4995=VECTOR('',#17859,4.91825);
#4996=VECTOR('',#17862,4.91825);
#4997=VECTOR('',#17865,4.91825);
#4998=VECTOR('',#17868,4.91825);
#4999=VECTOR('',#17871,4.91825);
#5000=VECTOR('',#17874,4.91825);
#5001=VECTOR('',#17877,4.91825);
#5002=VECTOR('',#17880,4.91825);
#5003=VECTOR('',#17883,4.91825);
#5004=VECTOR('',#17886,4.91825);
#5005=VECTOR('',#17889,10.);
#5006=VECTOR('',#17890,10.);
#5007=VECTOR('',#17891,10.);
#5008=VECTOR('',#17892,10.);
#5009=VECTOR('',#17895,10.);
#5010=VECTOR('',#17896,10.);
#5011=VECTOR('',#17897,10.);
#5012=VECTOR('',#17900,10.);
#5013=VECTOR('',#17901,10.);
#5014=VECTOR('',#17902,10.);
#5015=VECTOR('',#17905,10.);
#5016=VECTOR('',#17906,10.);
#5017=VECTOR('',#17907,10.);
#5018=VECTOR('',#17910,10.);
#5019=VECTOR('',#17911,10.);
#5020=VECTOR('',#17912,10.);
#5021=VECTOR('',#17915,10.);
#5022=VECTOR('',#17916,10.);
#5023=VECTOR('',#17923,5.);
#5024=VECTOR('',#17936,6.);
#5025=VECTOR('',#17953,10.);
#5026=VECTOR('',#17962,10.);
#5027=VECTOR('',#17963,10.);
#5028=VECTOR('',#17964,10.);
#5029=VECTOR('',#17965,10.);
#5030=VECTOR('',#17968,10.);
#5031=VECTOR('',#17969,10.);
#5032=VECTOR('',#17970,10.);
#5033=VECTOR('',#17971,10.);
#5034=VECTOR('',#17994,6.);
#5035=VECTOR('',#18001,7.);
#5036=VECTOR('',#18014,6.);
#5037=VECTOR('',#18021,10.);
#5038=VECTOR('',#18032,3.);
#5039=VECTOR('',#18037,3.);
#5040=VECTOR('',#18040,3.);
#5041=VECTOR('',#18043,3.);
#5042=VECTOR('',#18046,3.);
#5043=VECTOR('',#18049,3.);
#5044=VECTOR('',#18052,3.);
#5045=VECTOR('',#18055,3.);
#5046=VECTOR('',#18058,3.);
#5047=VECTOR('',#18061,3.);
#5048=VECTOR('',#18064,3.);
#5049=VECTOR('',#18067,3.);
#5050=VECTOR('',#18070,3.);
#5051=VECTOR('',#18073,3.);
#5052=VECTOR('',#18076,3.);
#5053=VECTOR('',#18079,3.);
#5054=VECTOR('',#18082,3.);
#5055=VECTOR('',#18085,3.);
#5056=VECTOR('',#18088,3.);
#5057=VECTOR('',#18091,3.);
#5058=VECTOR('',#18094,3.);
#5059=VECTOR('',#18097,3.);
#5060=VECTOR('',#18100,3.);
#5061=VECTOR('',#18103,3.);
#5062=VECTOR('',#18106,3.);
#5063=VECTOR('',#18109,3.);
#5064=VECTOR('',#18112,3.);
#5065=VECTOR('',#18115,3.);
#5066=VECTOR('',#18118,3.);
#5067=VECTOR('',#18121,3.);
#5068=VECTOR('',#18124,3.);
#5069=VECTOR('',#18127,3.);
#5070=VECTOR('',#18130,3.);
#5071=VECTOR('',#18133,3.);
#5072=VECTOR('',#18136,3.);
#5073=VECTOR('',#18139,3.);
#5074=VECTOR('',#18142,3.);
#5075=VECTOR('',#18145,3.);
#5076=VECTOR('',#18148,3.);
#5077=VECTOR('',#18151,2.37175);
#5078=VECTOR('',#18156,2.37175);
#5079=VECTOR('',#18159,2.37175);
#5080=VECTOR('',#18162,2.37175);
#5081=VECTOR('',#18165,2.37175);
#5082=VECTOR('',#18168,2.37175);
#5083=VECTOR('',#18171,2.37175);
#5084=VECTOR('',#18174,2.37175);
#5085=VECTOR('',#18177,2.37175);
#5086=VECTOR('',#18180,2.37175);
#5087=VECTOR('',#18183,2.37175);
#5088=VECTOR('',#18186,2.37175);
#5089=VECTOR('',#18189,2.37175);
#5090=VECTOR('',#18192,2.37175);
#5091=VECTOR('',#18195,2.37175);
#5092=VECTOR('',#18198,2.37175);
#5093=VECTOR('',#18201,2.37175);
#5094=VECTOR('',#18204,2.37175);
#5095=VECTOR('',#18207,2.37175);
#5096=VECTOR('',#18210,2.37175);
#5097=VECTOR('',#18213,2.37175);
#5098=VECTOR('',#18216,2.37175);
#5099=VECTOR('',#18219,2.37175);
#5100=VECTOR('',#18222,2.37175);
#5101=VECTOR('',#18225,2.37175);
#5102=VECTOR('',#18228,2.37175);
#5103=VECTOR('',#18231,2.37175);
#5104=VECTOR('',#18234,2.37175);
#5105=VECTOR('',#18237,2.37175);
#5106=VECTOR('',#18240,2.37175);
#5107=VECTOR('',#18243,2.37175);
#5108=VECTOR('',#18246,2.37175);
#5109=VECTOR('',#18249,2.37175);
#5110=VECTOR('',#18252,2.37175);
#5111=VECTOR('',#18255,2.37175);
#5112=VECTOR('',#18258,2.37175);
#5113=VECTOR('',#18261,2.37175);
#5114=VECTOR('',#18264,2.37175);
#5115=VECTOR('',#18267,2.37175);
#5116=VECTOR('',#18272,2.5);
#5117=VECTOR('',#18283,10.);
#5118=VECTOR('',#18284,10.);
#5119=VECTOR('',#18285,10.);
#5120=VECTOR('',#18286,10.);
#5121=VECTOR('',#18289,10.);
#5122=VECTOR('',#18290,10.);
#5123=VECTOR('',#18291,10.);
#5124=VECTOR('',#18294,10.);
#5125=VECTOR('',#18295,10.);
#5126=VECTOR('',#18296,10.);
#5127=VECTOR('',#18299,10.);
#5128=VECTOR('',#18300,10.);
#5129=VECTOR('',#18301,10.);
#5130=VECTOR('',#18304,10.);
#5131=VECTOR('',#18305,10.);
#5132=VECTOR('',#18306,10.);
#5133=VECTOR('',#18309,10.);
#5134=VECTOR('',#18310,10.);
#5135=VECTOR('',#18319,5.);
#5136=VECTOR('',#18332,3.5);
#5137=VECTOR('',#18339,7.);
#5138=VECTOR('',#18350,4.);
#5139=VECTOR('',#18355,4.);
#5140=VECTOR('',#18358,4.);
#5141=VECTOR('',#18361,4.);
#5142=VECTOR('',#18364,4.);
#5143=VECTOR('',#18367,4.);
#5144=VECTOR('',#18370,4.);
#5145=VECTOR('',#18373,4.);
#5146=VECTOR('',#18376,4.);
#5147=VECTOR('',#18379,4.);
#5148=VECTOR('',#18382,4.);
#5149=VECTOR('',#18385,4.);
#5150=VECTOR('',#18388,4.);
#5151=VECTOR('',#18391,4.);
#5152=VECTOR('',#18394,4.);
#5153=VECTOR('',#18397,4.);
#5154=VECTOR('',#18400,4.);
#5155=VECTOR('',#18403,4.);
#5156=VECTOR('',#18406,4.);
#5157=VECTOR('',#18409,4.);
#5158=VECTOR('',#18412,4.);
#5159=VECTOR('',#18415,4.);
#5160=VECTOR('',#18418,4.);
#5161=VECTOR('',#18421,4.);
#5162=VECTOR('',#18424,4.);
#5163=VECTOR('',#18427,4.);
#5164=VECTOR('',#18430,4.);
#5165=VECTOR('',#18433,4.);
#5166=VECTOR('',#18436,4.);
#5167=VECTOR('',#18439,4.);
#5168=VECTOR('',#18442,4.);
#5169=VECTOR('',#18445,4.);
#5170=VECTOR('',#18450,3.22275);
#5171=VECTOR('',#18455,3.22275);
#5172=VECTOR('',#18460,3.22275);
#5173=VECTOR('',#18463,3.22275);
#5174=VECTOR('',#18466,3.22275);
#5175=VECTOR('',#18469,3.22275);
#5176=VECTOR('',#18472,3.22275);
#5177=VECTOR('',#18475,3.22275);
#5178=VECTOR('',#18478,3.22275);
#5179=VECTOR('',#18481,3.22275);
#5180=VECTOR('',#18484,3.22275);
#5181=VECTOR('',#18487,3.22275);
#5182=VECTOR('',#18490,3.22275);
#5183=VECTOR('',#18493,3.22275);
#5184=VECTOR('',#18496,3.22275);
#5185=VECTOR('',#18499,3.22275);
#5186=VECTOR('',#18502,3.22275);
#5187=VECTOR('',#18505,3.22275);
#5188=VECTOR('',#18508,3.22275);
#5189=VECTOR('',#18511,3.22275);
#5190=VECTOR('',#18514,3.22275);
#5191=VECTOR('',#18517,3.22275);
#5192=VECTOR('',#18520,3.22275);
#5193=VECTOR('',#18523,3.22275);
#5194=VECTOR('',#18526,3.22275);
#5195=VECTOR('',#18529,3.22275);
#5196=VECTOR('',#18532,3.22275);
#5197=VECTOR('',#18535,3.22275);
#5198=VECTOR('',#18538,3.22275);
#5199=VECTOR('',#18541,3.22275);
#5200=VECTOR('',#18544,3.22275);
#5201=VECTOR('',#18547,3.22275);
#5202=VECTOR('',#18550,3.5);
#5203=VECTOR('',#18553,3.5);
#5204=VECTOR('',#18566,10.);
#5205=VECTOR('',#18567,10.);
#5206=VECTOR('',#18568,10.);
#5207=VECTOR('',#18569,10.);
#5208=VECTOR('',#18572,10.);
#5209=VECTOR('',#18573,10.);
#5210=VECTOR('',#18574,10.);
#5211=VECTOR('',#18577,10.);
#5212=VECTOR('',#18578,10.);
#5213=VECTOR('',#18579,10.);
#5214=VECTOR('',#18582,10.);
#5215=VECTOR('',#18583,10.);
#5216=VECTOR('',#18584,10.);
#5217=VECTOR('',#18587,10.);
#5218=VECTOR('',#18588,10.);
#5219=VECTOR('',#18589,10.);
#5220=VECTOR('',#18592,10.);
#5221=VECTOR('',#18593,10.);
#5222=VECTOR('',#18602,6.5);
#5223=VERTEX_POINT('',#18712);
#5224=VERTEX_POINT('',#18713);
#5225=VERTEX_POINT('',#18715);
#5226=VERTEX_POINT('',#18720);
#5227=VERTEX_POINT('',#18722);
#5228=VERTEX_POINT('',#18725);
#5229=VERTEX_POINT('',#18738);
#5230=VERTEX_POINT('',#18739);
#5231=VERTEX_POINT('',#18789);
#5232=VERTEX_POINT('',#18790);
#5233=VERTEX_POINT('',#18840);
#5234=VERTEX_POINT('',#18841);
#5235=VERTEX_POINT('',#18888);
#5236=VERTEX_POINT('',#18889);
#5237=VERTEX_POINT('',#18939);
#5238=VERTEX_POINT('',#18940);
#5239=VERTEX_POINT('',#18990);
#5240=VERTEX_POINT('',#18991);
#5241=VERTEX_POINT('',#19038);
#5242=VERTEX_POINT('',#19039);
#5243=VERTEX_POINT('',#19089);
#5244=VERTEX_POINT('',#19090);
#5245=VERTEX_POINT('',#19092);
#5246=VERTEX_POINT('',#19106);
#5247=VERTEX_POINT('',#19128);
#5248=VERTEX_POINT('',#19129);
#5249=VERTEX_POINT('',#19131);
#5250=VERTEX_POINT('',#19140);
#5251=VERTEX_POINT('',#19152);
#5252=VERTEX_POINT('',#19153);
#5253=VERTEX_POINT('',#19176);
#5254=VERTEX_POINT('',#19177);
#5255=VERTEX_POINT('',#19201);
#5256=VERTEX_POINT('',#19202);
#5257=VERTEX_POINT('',#19226);
#5258=VERTEX_POINT('',#19227);
#5259=VERTEX_POINT('',#19250);
#5260=VERTEX_POINT('',#19251);
#5261=VERTEX_POINT('',#19275);
#5262=VERTEX_POINT('',#19276);
#5263=VERTEX_POINT('',#19300);
#5264=VERTEX_POINT('',#19301);
#5265=VERTEX_POINT('',#19324);
#5266=VERTEX_POINT('',#19325);
#5267=VERTEX_POINT('',#19327);
#5268=VERTEX_POINT('',#19333);
#5269=VERTEX_POINT('',#19341);
#5270=VERTEX_POINT('',#19342);
#5271=VERTEX_POINT('',#19344);
#5272=VERTEX_POINT('',#19349);
#5273=VERTEX_POINT('',#19351);
#5274=VERTEX_POINT('',#19354);
#5275=VERTEX_POINT('',#19367);
#5276=VERTEX_POINT('',#19368);
#5277=VERTEX_POINT('',#19418);
#5278=VERTEX_POINT('',#19419);
#5279=VERTEX_POINT('',#19469);
#5280=VERTEX_POINT('',#19470);
#5281=VERTEX_POINT('',#19517);
#5282=VERTEX_POINT('',#19518);
#5283=VERTEX_POINT('',#19568);
#5284=VERTEX_POINT('',#19569);
#5285=VERTEX_POINT('',#19619);
#5286=VERTEX_POINT('',#19620);
#5287=VERTEX_POINT('',#19667);
#5288=VERTEX_POINT('',#19668);
#5289=VERTEX_POINT('',#19718);
#5290=VERTEX_POINT('',#19719);
#5291=VERTEX_POINT('',#19721);
#5292=VERTEX_POINT('',#19735);
#5293=VERTEX_POINT('',#19757);
#5294=VERTEX_POINT('',#19758);
#5295=VERTEX_POINT('',#19760);
#5296=VERTEX_POINT('',#19769);
#5297=VERTEX_POINT('',#19781);
#5298=VERTEX_POINT('',#19782);
#5299=VERTEX_POINT('',#19805);
#5300=VERTEX_POINT('',#19806);
#5301=VERTEX_POINT('',#19830);
#5302=VERTEX_POINT('',#19831);
#5303=VERTEX_POINT('',#19855);
#5304=VERTEX_POINT('',#19856);
#5305=VERTEX_POINT('',#19879);
#5306=VERTEX_POINT('',#19880);
#5307=VERTEX_POINT('',#19904);
#5308=VERTEX_POINT('',#19905);
#5309=VERTEX_POINT('',#19929);
#5310=VERTEX_POINT('',#19930);
#5311=VERTEX_POINT('',#19953);
#5312=VERTEX_POINT('',#19954);
#5313=VERTEX_POINT('',#19956);
#5314=VERTEX_POINT('',#19962);
#5315=VERTEX_POINT('',#19970);
#5316=VERTEX_POINT('',#19971);
#5317=VERTEX_POINT('',#19973);
#5318=VERTEX_POINT('',#19978);
#5319=VERTEX_POINT('',#19980);
#5320=VERTEX_POINT('',#19983);
#5321=VERTEX_POINT('',#19996);
#5322=VERTEX_POINT('',#19997);
#5323=VERTEX_POINT('',#20047);
#5324=VERTEX_POINT('',#20048);
#5325=VERTEX_POINT('',#20098);
#5326=VERTEX_POINT('',#20099);
#5327=VERTEX_POINT('',#20146);
#5328=VERTEX_POINT('',#20147);
#5329=VERTEX_POINT('',#20197);
#5330=VERTEX_POINT('',#20198);
#5331=VERTEX_POINT('',#20248);
#5332=VERTEX_POINT('',#20249);
#5333=VERTEX_POINT('',#20296);
#5334=VERTEX_POINT('',#20297);
#5335=VERTEX_POINT('',#20347);
#5336=VERTEX_POINT('',#20348);
#5337=VERTEX_POINT('',#20350);
#5338=VERTEX_POINT('',#20364);
#5339=VERTEX_POINT('',#20386);
#5340=VERTEX_POINT('',#20387);
#5341=VERTEX_POINT('',#20389);
#5342=VERTEX_POINT('',#20398);
#5343=VERTEX_POINT('',#20410);
#5344=VERTEX_POINT('',#20411);
#5345=VERTEX_POINT('',#20434);
#5346=VERTEX_POINT('',#20435);
#5347=VERTEX_POINT('',#20459);
#5348=VERTEX_POINT('',#20460);
#5349=VERTEX_POINT('',#20484);
#5350=VERTEX_POINT('',#20485);
#5351=VERTEX_POINT('',#20508);
#5352=VERTEX_POINT('',#20509);
#5353=VERTEX_POINT('',#20533);
#5354=VERTEX_POINT('',#20534);
#5355=VERTEX_POINT('',#20558);
#5356=VERTEX_POINT('',#20559);
#5357=VERTEX_POINT('',#20582);
#5358=VERTEX_POINT('',#20583);
#5359=VERTEX_POINT('',#20585);
#5360=VERTEX_POINT('',#20591);
#5361=VERTEX_POINT('',#20599);
#5362=VERTEX_POINT('',#20600);
#5363=VERTEX_POINT('',#20602);
#5364=VERTEX_POINT('',#20607);
#5365=VERTEX_POINT('',#20609);
#5366=VERTEX_POINT('',#20612);
#5367=VERTEX_POINT('',#20625);
#5368=VERTEX_POINT('',#20626);
#5369=VERTEX_POINT('',#20676);
#5370=VERTEX_POINT('',#20677);
#5371=VERTEX_POINT('',#20727);
#5372=VERTEX_POINT('',#20728);
#5373=VERTEX_POINT('',#20775);
#5374=VERTEX_POINT('',#20776);
#5375=VERTEX_POINT('',#20826);
#5376=VERTEX_POINT('',#20827);
#5377=VERTEX_POINT('',#20877);
#5378=VERTEX_POINT('',#20878);
#5379=VERTEX_POINT('',#20925);
#5380=VERTEX_POINT('',#20926);
#5381=VERTEX_POINT('',#20976);
#5382=VERTEX_POINT('',#20977);
#5383=VERTEX_POINT('',#20979);
#5384=VERTEX_POINT('',#20993);
#5385=VERTEX_POINT('',#21015);
#5386=VERTEX_POINT('',#21016);
#5387=VERTEX_POINT('',#21018);
#5388=VERTEX_POINT('',#21027);
#5389=VERTEX_POINT('',#21039);
#5390=VERTEX_POINT('',#21040);
#5391=VERTEX_POINT('',#21063);
#5392=VERTEX_POINT('',#21064);
#5393=VERTEX_POINT('',#21088);
#5394=VERTEX_POINT('',#21089);
#5395=VERTEX_POINT('',#21113);
#5396=VERTEX_POINT('',#21114);
#5397=VERTEX_POINT('',#21137);
#5398=VERTEX_POINT('',#21138);
#5399=VERTEX_POINT('',#21162);
#5400=VERTEX_POINT('',#21163);
#5401=VERTEX_POINT('',#21187);
#5402=VERTEX_POINT('',#21188);
#5403=VERTEX_POINT('',#21211);
#5404=VERTEX_POINT('',#21212);
#5405=VERTEX_POINT('',#21214);
#5406=VERTEX_POINT('',#21220);
#5407=VERTEX_POINT('',#21228);
#5408=VERTEX_POINT('',#21229);
#5409=VERTEX_POINT('',#21231);
#5410=VERTEX_POINT('',#21236);
#5411=VERTEX_POINT('',#21238);
#5412=VERTEX_POINT('',#21241);
#5413=VERTEX_POINT('',#21254);
#5414=VERTEX_POINT('',#21255);
#5415=VERTEX_POINT('',#21305);
#5416=VERTEX_POINT('',#21306);
#5417=VERTEX_POINT('',#21356);
#5418=VERTEX_POINT('',#21357);
#5419=VERTEX_POINT('',#21404);
#5420=VERTEX_POINT('',#21405);
#5421=VERTEX_POINT('',#21455);
#5422=VERTEX_POINT('',#21456);
#5423=VERTEX_POINT('',#21506);
#5424=VERTEX_POINT('',#21507);
#5425=VERTEX_POINT('',#21554);
#5426=VERTEX_POINT('',#21555);
#5427=VERTEX_POINT('',#21605);
#5428=VERTEX_POINT('',#21606);
#5429=VERTEX_POINT('',#21608);
#5430=VERTEX_POINT('',#21622);
#5431=VERTEX_POINT('',#21644);
#5432=VERTEX_POINT('',#21645);
#5433=VERTEX_POINT('',#21647);
#5434=VERTEX_POINT('',#21656);
#5435=VERTEX_POINT('',#21668);
#5436=VERTEX_POINT('',#21669);
#5437=VERTEX_POINT('',#21692);
#5438=VERTEX_POINT('',#21693);
#5439=VERTEX_POINT('',#21717);
#5440=VERTEX_POINT('',#21718);
#5441=VERTEX_POINT('',#21742);
#5442=VERTEX_POINT('',#21743);
#5443=VERTEX_POINT('',#21766);
#5444=VERTEX_POINT('',#21767);
#5445=VERTEX_POINT('',#21791);
#5446=VERTEX_POINT('',#21792);
#5447=VERTEX_POINT('',#21816);
#5448=VERTEX_POINT('',#21817);
#5449=VERTEX_POINT('',#21840);
#5450=VERTEX_POINT('',#21841);
#5451=VERTEX_POINT('',#21843);
#5452=VERTEX_POINT('',#21849);
#5453=VERTEX_POINT('',#21857);
#5454=VERTEX_POINT('',#21858);
#5455=VERTEX_POINT('',#21860);
#5456=VERTEX_POINT('',#21865);
#5457=VERTEX_POINT('',#21867);
#5458=VERTEX_POINT('',#21870);
#5459=VERTEX_POINT('',#21883);
#5460=VERTEX_POINT('',#21884);
#5461=VERTEX_POINT('',#21934);
#5462=VERTEX_POINT('',#21935);
#5463=VERTEX_POINT('',#21985);
#5464=VERTEX_POINT('',#21986);
#5465=VERTEX_POINT('',#22033);
#5466=VERTEX_POINT('',#22034);
#5467=VERTEX_POINT('',#22084);
#5468=VERTEX_POINT('',#22085);
#5469=VERTEX_POINT('',#22135);
#5470=VERTEX_POINT('',#22136);
#5471=VERTEX_POINT('',#22183);
#5472=VERTEX_POINT('',#22184);
#5473=VERTEX_POINT('',#22234);
#5474=VERTEX_POINT('',#22235);
#5475=VERTEX_POINT('',#22237);
#5476=VERTEX_POINT('',#22251);
#5477=VERTEX_POINT('',#22273);
#5478=VERTEX_POINT('',#22274);
#5479=VERTEX_POINT('',#22276);
#5480=VERTEX_POINT('',#22285);
#5481=VERTEX_POINT('',#22297);
#5482=VERTEX_POINT('',#22298);
#5483=VERTEX_POINT('',#22321);
#5484=VERTEX_POINT('',#22322);
#5485=VERTEX_POINT('',#22346);
#5486=VERTEX_POINT('',#22347);
#5487=VERTEX_POINT('',#22371);
#5488=VERTEX_POINT('',#22372);
#5489=VERTEX_POINT('',#22395);
#5490=VERTEX_POINT('',#22396);
#5491=VERTEX_POINT('',#22420);
#5492=VERTEX_POINT('',#22421);
#5493=VERTEX_POINT('',#22445);
#5494=VERTEX_POINT('',#22446);
#5495=VERTEX_POINT('',#22469);
#5496=VERTEX_POINT('',#22470);
#5497=VERTEX_POINT('',#22472);
#5498=VERTEX_POINT('',#22478);
#5499=VERTEX_POINT('',#22486);
#5500=VERTEX_POINT('',#22487);
#5501=VERTEX_POINT('',#22489);
#5502=VERTEX_POINT('',#22494);
#5503=VERTEX_POINT('',#22496);
#5504=VERTEX_POINT('',#22499);
#5505=VERTEX_POINT('',#22512);
#5506=VERTEX_POINT('',#22513);
#5507=VERTEX_POINT('',#22563);
#5508=VERTEX_POINT('',#22564);
#5509=VERTEX_POINT('',#22614);
#5510=VERTEX_POINT('',#22615);
#5511=VERTEX_POINT('',#22662);
#5512=VERTEX_POINT('',#22663);
#5513=VERTEX_POINT('',#22713);
#5514=VERTEX_POINT('',#22714);
#5515=VERTEX_POINT('',#22764);
#5516=VERTEX_POINT('',#22765);
#5517=VERTEX_POINT('',#22812);
#5518=VERTEX_POINT('',#22813);
#5519=VERTEX_POINT('',#22863);
#5520=VERTEX_POINT('',#22864);
#5521=VERTEX_POINT('',#22866);
#5522=VERTEX_POINT('',#22880);
#5523=VERTEX_POINT('',#22902);
#5524=VERTEX_POINT('',#22903);
#5525=VERTEX_POINT('',#22905);
#5526=VERTEX_POINT('',#22914);
#5527=VERTEX_POINT('',#22926);
#5528=VERTEX_POINT('',#22927);
#5529=VERTEX_POINT('',#22950);
#5530=VERTEX_POINT('',#22951);
#5531=VERTEX_POINT('',#22975);
#5532=VERTEX_POINT('',#22976);
#5533=VERTEX_POINT('',#23000);
#5534=VERTEX_POINT('',#23001);
#5535=VERTEX_POINT('',#23024);
#5536=VERTEX_POINT('',#23025);
#5537=VERTEX_POINT('',#23049);
#5538=VERTEX_POINT('',#23050);
#5539=VERTEX_POINT('',#23074);
#5540=VERTEX_POINT('',#23075);
#5541=VERTEX_POINT('',#23098);
#5542=VERTEX_POINT('',#23099);
#5543=VERTEX_POINT('',#23101);
#5544=VERTEX_POINT('',#23107);
#5545=VERTEX_POINT('',#23115);
#5546=VERTEX_POINT('',#23116);
#5547=VERTEX_POINT('',#23118);
#5548=VERTEX_POINT('',#23123);
#5549=VERTEX_POINT('',#23125);
#5550=VERTEX_POINT('',#23128);
#5551=VERTEX_POINT('',#23141);
#5552=VERTEX_POINT('',#23142);
#5553=VERTEX_POINT('',#23192);
#5554=VERTEX_POINT('',#23193);
#5555=VERTEX_POINT('',#23243);
#5556=VERTEX_POINT('',#23244);
#5557=VERTEX_POINT('',#23291);
#5558=VERTEX_POINT('',#23292);
#5559=VERTEX_POINT('',#23342);
#5560=VERTEX_POINT('',#23343);
#5561=VERTEX_POINT('',#23393);
#5562=VERTEX_POINT('',#23394);
#5563=VERTEX_POINT('',#23441);
#5564=VERTEX_POINT('',#23442);
#5565=VERTEX_POINT('',#23492);
#5566=VERTEX_POINT('',#23493);
#5567=VERTEX_POINT('',#23495);
#5568=VERTEX_POINT('',#23509);
#5569=VERTEX_POINT('',#23531);
#5570=VERTEX_POINT('',#23532);
#5571=VERTEX_POINT('',#23534);
#5572=VERTEX_POINT('',#23543);
#5573=VERTEX_POINT('',#23555);
#5574=VERTEX_POINT('',#23556);
#5575=VERTEX_POINT('',#23579);
#5576=VERTEX_POINT('',#23580);
#5577=VERTEX_POINT('',#23604);
#5578=VERTEX_POINT('',#23605);
#5579=VERTEX_POINT('',#23629);
#5580=VERTEX_POINT('',#23630);
#5581=VERTEX_POINT('',#23653);
#5582=VERTEX_POINT('',#23654);
#5583=VERTEX_POINT('',#23678);
#5584=VERTEX_POINT('',#23679);
#5585=VERTEX_POINT('',#23703);
#5586=VERTEX_POINT('',#23704);
#5587=VERTEX_POINT('',#23727);
#5588=VERTEX_POINT('',#23728);
#5589=VERTEX_POINT('',#23730);
#5590=VERTEX_POINT('',#23736);
#5591=VERTEX_POINT('',#23744);
#5592=VERTEX_POINT('',#23746);
#5593=VERTEX_POINT('',#23750);
#5594=VERTEX_POINT('',#23753);
#5595=VERTEX_POINT('',#23755);
#5596=VERTEX_POINT('',#23759);
#5597=VERTEX_POINT('',#23762);
#5598=VERTEX_POINT('',#23764);
#5599=VERTEX_POINT('',#23768);
#5600=VERTEX_POINT('',#23771);
#5601=VERTEX_POINT('',#23773);
#5602=VERTEX_POINT('',#23777);
#5603=VERTEX_POINT('',#23780);
#5604=VERTEX_POINT('',#23784);
#5605=VERTEX_POINT('',#23788);
#5606=VERTEX_POINT('',#23792);
#5607=VERTEX_POINT('',#31292);
#5608=VERTEX_POINT('',#31293);
#5609=VERTEX_POINT('',#31295);
#5610=VERTEX_POINT('',#31297);
#5611=VERTEX_POINT('',#31301);
#5612=VERTEX_POINT('',#31302);
#5613=VERTEX_POINT('',#31305);
#5614=VERTEX_POINT('',#31307);
#5615=VERTEX_POINT('',#31309);
#5616=VERTEX_POINT('',#31311);
#5617=VERTEX_POINT('',#31313);
#5618=VERTEX_POINT('',#31315);
#5619=VERTEX_POINT('',#31317);
#5620=VERTEX_POINT('',#31319);
#5621=VERTEX_POINT('',#31323);
#5622=VERTEX_POINT('',#31324);
#5623=VERTEX_POINT('',#31331);
#5624=VERTEX_POINT('',#31332);
#5625=VERTEX_POINT('',#31334);
#5626=VERTEX_POINT('',#31336);
#5627=VERTEX_POINT('',#31338);
#5628=VERTEX_POINT('',#31340);
#5629=VERTEX_POINT('',#31342);
#5630=VERTEX_POINT('',#31344);
#5631=VERTEX_POINT('',#31346);
#5632=VERTEX_POINT('',#31348);
#5633=VERTEX_POINT('',#31350);
#5634=VERTEX_POINT('',#31352);
#5635=VERTEX_POINT('',#31356);
#5636=VERTEX_POINT('',#31357);
#5637=VERTEX_POINT('',#31362);
#5638=VERTEX_POINT('',#31363);
#5639=VERTEX_POINT('',#31370);
#5640=VERTEX_POINT('',#31372);
#5641=VERTEX_POINT('',#31374);
#5642=VERTEX_POINT('',#31376);
#5643=VERTEX_POINT('',#31380);
#5644=VERTEX_POINT('',#31384);
#5645=VERTEX_POINT('',#31386);
#5646=VERTEX_POINT('',#31388);
#5647=VERTEX_POINT('',#31390);
#5648=VERTEX_POINT('',#31392);
#5649=VERTEX_POINT('',#31394);
#5650=VERTEX_POINT('',#31396);
#5651=VERTEX_POINT('',#31400);
#5652=VERTEX_POINT('',#31402);
#5653=VERTEX_POINT('',#31404);
#5654=VERTEX_POINT('',#31406);
#5655=VERTEX_POINT('',#31408);
#5656=VERTEX_POINT('',#31410);
#5657=VERTEX_POINT('',#31412);
#5658=VERTEX_POINT('',#31416);
#5659=VERTEX_POINT('',#31422);
#5660=VERTEX_POINT('',#31424);
#5661=VERTEX_POINT('',#31426);
#5662=VERTEX_POINT('',#31428);
#5663=VERTEX_POINT('',#31432);
#5664=VERTEX_POINT('',#31436);
#5665=VERTEX_POINT('',#31440);
#5666=VERTEX_POINT('',#31444);
#5667=VERTEX_POINT('',#31446);
#5668=VERTEX_POINT('',#31448);
#5669=VERTEX_POINT('',#31450);
#5670=VERTEX_POINT('',#31452);
#5671=VERTEX_POINT('',#31454);
#5672=VERTEX_POINT('',#31458);
#5673=VERTEX_POINT('',#31462);
#5674=VERTEX_POINT('',#31466);
#5675=VERTEX_POINT('',#31468);
#5676=VERTEX_POINT('',#31476);
#5677=VERTEX_POINT('',#31478);
#5678=VERTEX_POINT('',#31480);
#5679=VERTEX_POINT('',#31482);
#5680=VERTEX_POINT('',#31486);
#5681=VERTEX_POINT('',#31488);
#5682=VERTEX_POINT('',#31490);
#5683=VERTEX_POINT('',#31493);
#5684=VERTEX_POINT('',#31505);
#5685=VERTEX_POINT('',#31512);
#5686=VERTEX_POINT('',#31514);
#5687=VERTEX_POINT('',#31518);
#5688=VERTEX_POINT('',#31520);
#5689=VERTEX_POINT('',#31522);
#5690=VERTEX_POINT('',#31526);
#5691=VERTEX_POINT('',#31528);
#5692=VERTEX_POINT('',#31530);
#5693=VERTEX_POINT('',#31532);
#5694=VERTEX_POINT('',#31534);
#5695=VERTEX_POINT('',#31536);
#5696=VERTEX_POINT('',#31543);
#5697=VERTEX_POINT('',#31545);
#5698=VERTEX_POINT('',#31549);
#5699=VERTEX_POINT('',#31551);
#5700=VERTEX_POINT('',#31553);
#5701=VERTEX_POINT('',#31555);
#5702=VERTEX_POINT('',#31557);
#5703=VERTEX_POINT('',#31559);
#5704=VERTEX_POINT('',#31561);
#5705=VERTEX_POINT('',#31563);
#5706=VERTEX_POINT('',#31565);
#5707=VERTEX_POINT('',#31569);
#5708=VERTEX_POINT('',#31570);
#5709=VERTEX_POINT('',#31580);
#5710=VERTEX_POINT('',#31586);
#5711=VERTEX_POINT('',#31591);
#5712=VERTEX_POINT('',#31598);
#5713=VERTEX_POINT('',#31615);
#5714=VERTEX_POINT('',#31620);
#5715=VERTEX_POINT('',#31632);
#5716=VERTEX_POINT('',#31634);
#5717=VERTEX_POINT('',#31641);
#5718=VERTEX_POINT('',#31642);
#5719=VERTEX_POINT('',#31644);
#5720=VERTEX_POINT('',#31652);
#5721=VERTEX_POINT('',#31654);
#5722=VERTEX_POINT('',#31657);
#5723=VERTEX_POINT('',#31673);
#5724=VERTEX_POINT('',#31674);
#5725=VERTEX_POINT('',#31727);
#5726=VERTEX_POINT('',#31728);
#5727=VERTEX_POINT('',#31775);
#5728=VERTEX_POINT('',#31776);
#5729=VERTEX_POINT('',#31826);
#5730=VERTEX_POINT('',#31827);
#5731=VERTEX_POINT('',#31877);
#5732=VERTEX_POINT('',#31878);
#5733=VERTEX_POINT('',#31925);
#5734=VERTEX_POINT('',#31926);
#5735=VERTEX_POINT('',#31928);
#5736=VERTEX_POINT('',#31942);
#5737=VERTEX_POINT('',#31964);
#5738=VERTEX_POINT('',#31965);
#5739=VERTEX_POINT('',#31967);
#5740=VERTEX_POINT('',#31977);
#5741=VERTEX_POINT('',#31990);
#5742=VERTEX_POINT('',#31991);
#5743=VERTEX_POINT('',#32015);
#5744=VERTEX_POINT('',#32016);
#5745=VERTEX_POINT('',#32040);
#5746=VERTEX_POINT('',#32041);
#5747=VERTEX_POINT('',#32064);
#5748=VERTEX_POINT('',#32065);
#5749=VERTEX_POINT('',#32089);
#5750=VERTEX_POINT('',#32090);
#5751=VERTEX_POINT('',#32114);
#5752=VERTEX_POINT('',#32115);
#5753=VERTEX_POINT('',#32117);
#5754=VERTEX_POINT('',#32123);
#5755=VERTEX_POINT('',#32131);
#5756=VERTEX_POINT('',#32132);
#5757=VERTEX_POINT('',#32134);
#5758=VERTEX_POINT('',#32142);
#5759=VERTEX_POINT('',#32144);
#5760=VERTEX_POINT('',#32147);
#5761=VERTEX_POINT('',#32163);
#5762=VERTEX_POINT('',#32164);
#5763=VERTEX_POINT('',#32217);
#5764=VERTEX_POINT('',#32218);
#5765=VERTEX_POINT('',#32265);
#5766=VERTEX_POINT('',#32266);
#5767=VERTEX_POINT('',#32316);
#5768=VERTEX_POINT('',#32317);
#5769=VERTEX_POINT('',#32367);
#5770=VERTEX_POINT('',#32368);
#5771=VERTEX_POINT('',#32415);
#5772=VERTEX_POINT('',#32416);
#5773=VERTEX_POINT('',#32418);
#5774=VERTEX_POINT('',#32432);
#5775=VERTEX_POINT('',#32454);
#5776=VERTEX_POINT('',#32455);
#5777=VERTEX_POINT('',#32457);
#5778=VERTEX_POINT('',#32467);
#5779=VERTEX_POINT('',#32480);
#5780=VERTEX_POINT('',#32481);
#5781=VERTEX_POINT('',#32505);
#5782=VERTEX_POINT('',#32506);
#5783=VERTEX_POINT('',#32530);
#5784=VERTEX_POINT('',#32531);
#5785=VERTEX_POINT('',#32554);
#5786=VERTEX_POINT('',#32555);
#5787=VERTEX_POINT('',#32579);
#5788=VERTEX_POINT('',#32580);
#5789=VERTEX_POINT('',#32604);
#5790=VERTEX_POINT('',#32605);
#5791=VERTEX_POINT('',#32607);
#5792=VERTEX_POINT('',#32613);
#5793=VERTEX_POINT('',#32621);
#5794=VERTEX_POINT('',#32622);
#5795=VERTEX_POINT('',#32624);
#5796=VERTEX_POINT('',#32632);
#5797=VERTEX_POINT('',#32634);
#5798=VERTEX_POINT('',#32637);
#5799=VERTEX_POINT('',#32653);
#5800=VERTEX_POINT('',#32654);
#5801=VERTEX_POINT('',#32707);
#5802=VERTEX_POINT('',#32708);
#5803=VERTEX_POINT('',#32755);
#5804=VERTEX_POINT('',#32756);
#5805=VERTEX_POINT('',#32806);
#5806=VERTEX_POINT('',#32807);
#5807=VERTEX_POINT('',#32857);
#5808=VERTEX_POINT('',#32858);
#5809=VERTEX_POINT('',#32905);
#5810=VERTEX_POINT('',#32906);
#5811=VERTEX_POINT('',#32908);
#5812=VERTEX_POINT('',#32922);
#5813=VERTEX_POINT('',#32944);
#5814=VERTEX_POINT('',#32945);
#5815=VERTEX_POINT('',#32947);
#5816=VERTEX_POINT('',#32957);
#5817=VERTEX_POINT('',#32970);
#5818=VERTEX_POINT('',#32971);
#5819=VERTEX_POINT('',#32995);
#5820=VERTEX_POINT('',#32996);
#5821=VERTEX_POINT('',#33020);
#5822=VERTEX_POINT('',#33021);
#5823=VERTEX_POINT('',#33044);
#5824=VERTEX_POINT('',#33045);
#5825=VERTEX_POINT('',#33069);
#5826=VERTEX_POINT('',#33070);
#5827=VERTEX_POINT('',#33094);
#5828=VERTEX_POINT('',#33095);
#5829=VERTEX_POINT('',#33097);
#5830=VERTEX_POINT('',#33103);
#5831=VERTEX_POINT('',#33111);
#5832=VERTEX_POINT('',#33112);
#5833=VERTEX_POINT('',#33114);
#5834=VERTEX_POINT('',#33122);
#5835=VERTEX_POINT('',#33124);
#5836=VERTEX_POINT('',#33127);
#5837=VERTEX_POINT('',#33143);
#5838=VERTEX_POINT('',#33144);
#5839=VERTEX_POINT('',#33197);
#5840=VERTEX_POINT('',#33198);
#5841=VERTEX_POINT('',#33245);
#5842=VERTEX_POINT('',#33246);
#5843=VERTEX_POINT('',#33296);
#5844=VERTEX_POINT('',#33297);
#5845=VERTEX_POINT('',#33347);
#5846=VERTEX_POINT('',#33348);
#5847=VERTEX_POINT('',#33395);
#5848=VERTEX_POINT('',#33396);
#5849=VERTEX_POINT('',#33398);
#5850=VERTEX_POINT('',#33412);
#5851=VERTEX_POINT('',#33434);
#5852=VERTEX_POINT('',#33435);
#5853=VERTEX_POINT('',#33437);
#5854=VERTEX_POINT('',#33447);
#5855=VERTEX_POINT('',#33460);
#5856=VERTEX_POINT('',#33461);
#5857=VERTEX_POINT('',#33485);
#5858=VERTEX_POINT('',#33486);
#5859=VERTEX_POINT('',#33510);
#5860=VERTEX_POINT('',#33511);
#5861=VERTEX_POINT('',#33534);
#5862=VERTEX_POINT('',#33535);
#5863=VERTEX_POINT('',#33559);
#5864=VERTEX_POINT('',#33560);
#5865=VERTEX_POINT('',#33584);
#5866=VERTEX_POINT('',#33585);
#5867=VERTEX_POINT('',#33587);
#5868=VERTEX_POINT('',#33593);
#5869=VERTEX_POINT('',#33601);
#5870=VERTEX_POINT('',#33602);
#5871=VERTEX_POINT('',#33604);
#5872=VERTEX_POINT('',#33639);
#5873=VERTEX_POINT('',#33641);
#5874=VERTEX_POINT('',#33646);
#5875=VERTEX_POINT('',#33693);
#5876=VERTEX_POINT('',#33694);
#5877=VERTEX_POINT('',#33777);
#5878=VERTEX_POINT('',#33778);
#5879=VERTEX_POINT('',#33852);
#5880=VERTEX_POINT('',#33853);
#5881=VERTEX_POINT('',#33855);
#5882=VERTEX_POINT('',#33881);
#5883=VERTEX_POINT('',#33921);
#5884=VERTEX_POINT('',#33922);
#5885=VERTEX_POINT('',#33924);
#5886=VERTEX_POINT('',#33933);
#5887=VERTEX_POINT('',#33946);
#5888=VERTEX_POINT('',#33947);
#5889=VERTEX_POINT('',#33983);
#5890=VERTEX_POINT('',#33984);
#5891=VERTEX_POINT('',#34017);
#5892=VERTEX_POINT('',#34018);
#5893=VERTEX_POINT('',#34053);
#5894=VERTEX_POINT('',#34054);
#5895=VERTEX_POINT('',#34056);
#5896=VERTEX_POINT('',#34063);
#5897=VERTEX_POINT('',#34073);
#5898=VERTEX_POINT('',#34074);
#5899=VERTEX_POINT('',#34076);
#5900=VERTEX_POINT('',#34111);
#5901=VERTEX_POINT('',#34113);
#5902=VERTEX_POINT('',#34118);
#5903=VERTEX_POINT('',#34165);
#5904=VERTEX_POINT('',#34166);
#5905=VERTEX_POINT('',#34249);
#5906=VERTEX_POINT('',#34250);
#5907=VERTEX_POINT('',#34324);
#5908=VERTEX_POINT('',#34325);
#5909=VERTEX_POINT('',#34327);
#5910=VERTEX_POINT('',#34353);
#5911=VERTEX_POINT('',#34393);
#5912=VERTEX_POINT('',#34394);
#5913=VERTEX_POINT('',#34396);
#5914=VERTEX_POINT('',#34405);
#5915=VERTEX_POINT('',#34418);
#5916=VERTEX_POINT('',#34419);
#5917=VERTEX_POINT('',#34455);
#5918=VERTEX_POINT('',#34456);
#5919=VERTEX_POINT('',#34489);
#5920=VERTEX_POINT('',#34490);
#5921=VERTEX_POINT('',#34525);
#5922=VERTEX_POINT('',#34526);
#5923=VERTEX_POINT('',#34528);
#5924=VERTEX_POINT('',#34535);
#5925=VERTEX_POINT('',#34545);
#5926=VERTEX_POINT('',#34546);
#5927=VERTEX_POINT('',#34548);
#5928=VERTEX_POINT('',#34583);
#5929=VERTEX_POINT('',#34585);
#5930=VERTEX_POINT('',#34590);
#5931=VERTEX_POINT('',#34637);
#5932=VERTEX_POINT('',#34638);
#5933=VERTEX_POINT('',#34721);
#5934=VERTEX_POINT('',#34722);
#5935=VERTEX_POINT('',#34796);
#5936=VERTEX_POINT('',#34797);
#5937=VERTEX_POINT('',#34799);
#5938=VERTEX_POINT('',#34825);
#5939=VERTEX_POINT('',#34865);
#5940=VERTEX_POINT('',#34866);
#5941=VERTEX_POINT('',#34868);
#5942=VERTEX_POINT('',#34877);
#5943=VERTEX_POINT('',#34890);
#5944=VERTEX_POINT('',#34891);
#5945=VERTEX_POINT('',#34927);
#5946=VERTEX_POINT('',#34928);
#5947=VERTEX_POINT('',#34961);
#5948=VERTEX_POINT('',#34962);
#5949=VERTEX_POINT('',#34997);
#5950=VERTEX_POINT('',#34998);
#5951=VERTEX_POINT('',#35000);
#5952=VERTEX_POINT('',#35007);
#5953=VERTEX_POINT('',#35017);
#5954=VERTEX_POINT('',#35018);
#5955=VERTEX_POINT('',#35020);
#5956=VERTEX_POINT('',#35055);
#5957=VERTEX_POINT('',#35057);
#5958=VERTEX_POINT('',#35062);
#5959=VERTEX_POINT('',#35109);
#5960=VERTEX_POINT('',#35110);
#5961=VERTEX_POINT('',#35193);
#5962=VERTEX_POINT('',#35194);
#5963=VERTEX_POINT('',#35268);
#5964=VERTEX_POINT('',#35269);
#5965=VERTEX_POINT('',#35271);
#5966=VERTEX_POINT('',#35297);
#5967=VERTEX_POINT('',#35337);
#5968=VERTEX_POINT('',#35338);
#5969=VERTEX_POINT('',#35340);
#5970=VERTEX_POINT('',#35349);
#5971=VERTEX_POINT('',#35362);
#5972=VERTEX_POINT('',#35363);
#5973=VERTEX_POINT('',#35399);
#5974=VERTEX_POINT('',#35400);
#5975=VERTEX_POINT('',#35433);
#5976=VERTEX_POINT('',#35434);
#5977=VERTEX_POINT('',#35469);
#5978=VERTEX_POINT('',#35470);
#5979=VERTEX_POINT('',#35472);
#5980=VERTEX_POINT('',#35479);
#5981=VERTEX_POINT('',#43245);
#5982=VERTEX_POINT('',#43247);
#5983=VERTEX_POINT('',#43251);
#5984=VERTEX_POINT('',#43254);
#5985=VERTEX_POINT('',#43258);
#5986=VERTEX_POINT('',#43260);
#5987=VERTEX_POINT('',#43267);
#5988=VERTEX_POINT('',#43268);
#5989=VERTEX_POINT('',#43270);
#5990=VERTEX_POINT('',#43299);
#5991=VERTEX_POINT('',#43342);
#5992=VERTEX_POINT('',#43343);
#5993=VERTEX_POINT('',#43429);
#5994=VERTEX_POINT('',#43430);
#5995=VERTEX_POINT('',#43516);
#5996=VERTEX_POINT('',#43517);
#5997=VERTEX_POINT('',#43603);
#5998=VERTEX_POINT('',#43604);
#5999=VERTEX_POINT('',#43693);
#6000=VERTEX_POINT('',#43694);
#6001=VERTEX_POINT('',#43780);
#6002=VERTEX_POINT('',#43781);
#6003=VERTEX_POINT('',#43867);
#6004=VERTEX_POINT('',#43868);
#6005=VERTEX_POINT('',#43954);
#6006=VERTEX_POINT('',#43955);
#6007=VERTEX_POINT('',#44041);
#6008=VERTEX_POINT('',#44042);
#6009=VERTEX_POINT('',#44131);
#6010=VERTEX_POINT('',#44132);
#6011=VERTEX_POINT('',#44218);
#6012=VERTEX_POINT('',#44219);
#6013=VERTEX_POINT('',#44305);
#6014=VERTEX_POINT('',#44306);
#6015=VERTEX_POINT('',#44392);
#6016=VERTEX_POINT('',#44393);
#6017=VERTEX_POINT('',#44479);
#6018=VERTEX_POINT('',#44480);
#6019=VERTEX_POINT('',#44566);
#6020=VERTEX_POINT('',#44567);
#6021=VERTEX_POINT('',#44653);
#6022=VERTEX_POINT('',#44654);
#6023=VERTEX_POINT('',#44740);
#6024=VERTEX_POINT('',#44741);
#6025=VERTEX_POINT('',#44827);
#6026=VERTEX_POINT('',#44828);
#6027=VERTEX_POINT('',#44914);
#6028=VERTEX_POINT('',#44915);
#6029=VERTEX_POINT('',#45001);
#6030=VERTEX_POINT('',#45002);
#6031=VERTEX_POINT('',#45091);
#6032=VERTEX_POINT('',#45092);
#6033=VERTEX_POINT('',#45178);
#6034=VERTEX_POINT('',#45179);
#6035=VERTEX_POINT('',#45265);
#6036=VERTEX_POINT('',#45266);
#6037=VERTEX_POINT('',#45352);
#6038=VERTEX_POINT('',#45353);
#6039=VERTEX_POINT('',#45439);
#6040=VERTEX_POINT('',#45440);
#6041=VERTEX_POINT('',#45529);
#6042=VERTEX_POINT('',#45530);
#6043=VERTEX_POINT('',#45616);
#6044=VERTEX_POINT('',#45617);
#6045=VERTEX_POINT('',#45619);
#6046=VERTEX_POINT('',#45645);
#6047=VERTEX_POINT('',#45685);
#6048=VERTEX_POINT('',#45686);
#6049=VERTEX_POINT('',#45688);
#6050=VERTEX_POINT('',#45696);
#6051=VERTEX_POINT('',#45707);
#6052=VERTEX_POINT('',#45708);
#6053=VERTEX_POINT('',#45745);
#6054=VERTEX_POINT('',#45746);
#6055=VERTEX_POINT('',#45781);
#6056=VERTEX_POINT('',#45782);
#6057=VERTEX_POINT('',#45819);
#6058=VERTEX_POINT('',#45820);
#6059=VERTEX_POINT('',#45856);
#6060=VERTEX_POINT('',#45857);
#6061=VERTEX_POINT('',#45893);
#6062=VERTEX_POINT('',#45894);
#6063=VERTEX_POINT('',#45931);
#6064=VERTEX_POINT('',#45932);
#6065=VERTEX_POINT('',#45967);
#6066=VERTEX_POINT('',#45968);
#6067=VERTEX_POINT('',#46005);
#6068=VERTEX_POINT('',#46006);
#6069=VERTEX_POINT('',#46042);
#6070=VERTEX_POINT('',#46043);
#6071=VERTEX_POINT('',#46079);
#6072=VERTEX_POINT('',#46080);
#6073=VERTEX_POINT('',#46117);
#6074=VERTEX_POINT('',#46118);
#6075=VERTEX_POINT('',#46153);
#6076=VERTEX_POINT('',#46154);
#6077=VERTEX_POINT('',#46191);
#6078=VERTEX_POINT('',#46192);
#6079=VERTEX_POINT('',#46228);
#6080=VERTEX_POINT('',#46229);
#6081=VERTEX_POINT('',#46265);
#6082=VERTEX_POINT('',#46266);
#6083=VERTEX_POINT('',#46303);
#6084=VERTEX_POINT('',#46304);
#6085=VERTEX_POINT('',#46339);
#6086=VERTEX_POINT('',#46340);
#6087=VERTEX_POINT('',#46377);
#6088=VERTEX_POINT('',#46378);
#6089=VERTEX_POINT('',#46413);
#6090=VERTEX_POINT('',#46414);
#6091=VERTEX_POINT('',#46451);
#6092=VERTEX_POINT('',#46452);
#6093=VERTEX_POINT('',#46489);
#6094=VERTEX_POINT('',#46490);
#6095=VERTEX_POINT('',#46525);
#6096=VERTEX_POINT('',#46526);
#6097=VERTEX_POINT('',#46563);
#6098=VERTEX_POINT('',#46564);
#6099=VERTEX_POINT('',#46599);
#6100=VERTEX_POINT('',#46600);
#6101=VERTEX_POINT('',#46637);
#6102=VERTEX_POINT('',#46638);
#6103=VERTEX_POINT('',#46675);
#6104=VERTEX_POINT('',#46676);
#6105=VERTEX_POINT('',#46711);
#6106=VERTEX_POINT('',#46712);
#6107=VERTEX_POINT('',#46714);
#6108=VERTEX_POINT('',#46721);
#6109=VERTEX_POINT('',#50233);
#6110=VERTEX_POINT('',#50234);
#6111=VERTEX_POINT('',#50236);
#6112=VERTEX_POINT('',#50238);
#6113=VERTEX_POINT('',#50240);
#6114=VERTEX_POINT('',#50242);
#6115=VERTEX_POINT('',#50244);
#6116=VERTEX_POINT('',#50246);
#6117=VERTEX_POINT('',#50251);
#6118=VERTEX_POINT('',#50252);
#6119=VERTEX_POINT('',#50254);
#6120=VERTEX_POINT('',#50256);
#6121=VERTEX_POINT('',#50260);
#6122=VERTEX_POINT('',#50261);
#6123=VERTEX_POINT('',#50269);
#6124=VERTEX_POINT('',#50273);
#6125=VERTEX_POINT('',#50277);
#6126=VERTEX_POINT('',#50281);
#6127=VERTEX_POINT('',#50285);
#6128=VERTEX_POINT('',#50289);
#6129=VERTEX_POINT('',#50297);
#6130=VERTEX_POINT('',#50299);
#6131=VERTEX_POINT('',#50303);
#6132=VERTEX_POINT('',#50305);
#6133=VERTEX_POINT('',#50309);
#6134=VERTEX_POINT('',#50310);
#6135=VERTEX_POINT('',#50312);
#6136=VERTEX_POINT('',#50314);
#6137=VERTEX_POINT('',#50318);
#6138=VERTEX_POINT('',#50319);
#6139=VERTEX_POINT('',#50321);
#6140=VERTEX_POINT('',#50323);
#6141=VERTEX_POINT('',#50327);
#6142=VERTEX_POINT('',#50329);
#6143=VERTEX_POINT('',#50331);
#6144=VERTEX_POINT('',#50333);
#6145=VERTEX_POINT('',#50335);
#6146=VERTEX_POINT('',#50337);
#6147=VERTEX_POINT('',#50339);
#6148=VERTEX_POINT('',#50341);
#6149=VERTEX_POINT('',#50345);
#6150=VERTEX_POINT('',#50348);
#6151=VERTEX_POINT('',#50350);
#6152=VERTEX_POINT('',#50352);
#6153=VERTEX_POINT('',#50354);
#6154=VERTEX_POINT('',#50356);
#6155=VERTEX_POINT('',#50358);
#6156=VERTEX_POINT('',#50362);
#6157=VERTEX_POINT('',#50364);
#6158=VERTEX_POINT('',#50366);
#6159=VERTEX_POINT('',#50368);
#6160=VERTEX_POINT('',#50370);
#6161=VERTEX_POINT('',#50372);
#6162=VERTEX_POINT('',#50378);
#6163=VERTEX_POINT('',#50379);
#6164=VERTEX_POINT('',#50382);
#6165=VERTEX_POINT('',#50385);
#6166=VERTEX_POINT('',#50387);
#6167=VERTEX_POINT('',#50391);
#6168=VERTEX_POINT('',#50394);
#6169=VERTEX_POINT('',#50414);
#6170=VERTEX_POINT('',#50418);
#6171=VERTEX_POINT('',#50426);
#6172=VERTEX_POINT('',#50427);
#6173=VERTEX_POINT('',#50429);
#6174=VERTEX_POINT('',#50446);
#6175=VERTEX_POINT('',#50459);
#6176=VERTEX_POINT('',#50460);
#6177=VERTEX_POINT('',#50543);
#6178=VERTEX_POINT('',#50544);
#6179=VERTEX_POINT('',#50633);
#6180=VERTEX_POINT('',#50634);
#6181=VERTEX_POINT('',#50717);
#6182=VERTEX_POINT('',#50718);
#6183=VERTEX_POINT('',#50807);
#6184=VERTEX_POINT('',#50808);
#6185=VERTEX_POINT('',#50897);
#6186=VERTEX_POINT('',#50898);
#6187=VERTEX_POINT('',#50981);
#6188=VERTEX_POINT('',#50982);
#6189=VERTEX_POINT('',#51071);
#6190=VERTEX_POINT('',#51072);
#6191=VERTEX_POINT('',#51155);
#6192=VERTEX_POINT('',#51156);
#6193=VERTEX_POINT('',#51245);
#6194=VERTEX_POINT('',#51246);
#6195=VERTEX_POINT('',#51329);
#6196=VERTEX_POINT('',#51330);
#6197=VERTEX_POINT('',#51419);
#6198=VERTEX_POINT('',#51420);
#6199=VERTEX_POINT('',#51509);
#6200=VERTEX_POINT('',#51510);
#6201=VERTEX_POINT('',#51593);
#6202=VERTEX_POINT('',#51594);
#6203=VERTEX_POINT('',#51683);
#6204=VERTEX_POINT('',#51684);
#6205=VERTEX_POINT('',#51767);
#6206=VERTEX_POINT('',#51768);
#6207=VERTEX_POINT('',#51857);
#6208=VERTEX_POINT('',#51858);
#6209=VERTEX_POINT('',#51941);
#6210=VERTEX_POINT('',#51942);
#6211=VERTEX_POINT('',#52028);
#6212=VERTEX_POINT('',#52029);
#6213=VERTEX_POINT('',#52118);
#6214=VERTEX_POINT('',#52119);
#6215=VERTEX_POINT('',#52202);
#6216=VERTEX_POINT('',#52203);
#6217=VERTEX_POINT('',#52292);
#6218=VERTEX_POINT('',#52293);
#6219=VERTEX_POINT('',#52376);
#6220=VERTEX_POINT('',#52377);
#6221=VERTEX_POINT('',#52466);
#6222=VERTEX_POINT('',#52467);
#6223=VERTEX_POINT('',#52553);
#6224=VERTEX_POINT('',#52554);
#6225=VERTEX_POINT('',#52640);
#6226=VERTEX_POINT('',#52641);
#6227=VERTEX_POINT('',#52730);
#6228=VERTEX_POINT('',#52731);
#6229=VERTEX_POINT('',#52814);
#6230=VERTEX_POINT('',#52815);
#6231=VERTEX_POINT('',#52904);
#6232=VERTEX_POINT('',#52905);
#6233=VERTEX_POINT('',#52988);
#6234=VERTEX_POINT('',#52989);
#6235=VERTEX_POINT('',#53078);
#6236=VERTEX_POINT('',#53079);
#6237=VERTEX_POINT('',#53165);
#6238=VERTEX_POINT('',#53166);
#6239=VERTEX_POINT('',#53252);
#6240=VERTEX_POINT('',#53253);
#6241=VERTEX_POINT('',#53342);
#6242=VERTEX_POINT('',#53343);
#6243=VERTEX_POINT('',#53426);
#6244=VERTEX_POINT('',#53427);
#6245=VERTEX_POINT('',#53516);
#6246=VERTEX_POINT('',#53518);
#6247=VERTEX_POINT('',#53520);
#6248=VERTEX_POINT('',#53522);
#6249=VERTEX_POINT('',#53536);
#6250=VERTEX_POINT('',#53538);
#6251=VERTEX_POINT('',#53560);
#6252=VERTEX_POINT('',#53561);
#6253=VERTEX_POINT('',#53563);
#6254=VERTEX_POINT('',#53579);
#6255=VERTEX_POINT('',#53595);
#6256=VERTEX_POINT('',#53596);
#6257=VERTEX_POINT('',#53632);
#6258=VERTEX_POINT('',#53633);
#6259=VERTEX_POINT('',#53669);
#6260=VERTEX_POINT('',#53670);
#6261=VERTEX_POINT('',#53706);
#6262=VERTEX_POINT('',#53707);
#6263=VERTEX_POINT('',#53744);
#6264=VERTEX_POINT('',#53745);
#6265=VERTEX_POINT('',#53780);
#6266=VERTEX_POINT('',#53781);
#6267=VERTEX_POINT('',#53818);
#6268=VERTEX_POINT('',#53819);
#6269=VERTEX_POINT('',#53855);
#6270=VERTEX_POINT('',#53856);
#6271=VERTEX_POINT('',#53892);
#6272=VERTEX_POINT('',#53893);
#6273=VERTEX_POINT('',#53929);
#6274=VERTEX_POINT('',#53930);
#6275=VERTEX_POINT('',#53966);
#6276=VERTEX_POINT('',#53967);
#6277=VERTEX_POINT('',#54004);
#6278=VERTEX_POINT('',#54005);
#6279=VERTEX_POINT('',#54040);
#6280=VERTEX_POINT('',#54041);
#6281=VERTEX_POINT('',#54078);
#6282=VERTEX_POINT('',#54079);
#6283=VERTEX_POINT('',#54115);
#6284=VERTEX_POINT('',#54116);
#6285=VERTEX_POINT('',#54152);
#6286=VERTEX_POINT('',#54153);
#6287=VERTEX_POINT('',#54189);
#6288=VERTEX_POINT('',#54190);
#6289=VERTEX_POINT('',#54226);
#6290=VERTEX_POINT('',#54227);
#6291=VERTEX_POINT('',#54264);
#6292=VERTEX_POINT('',#54265);
#6293=VERTEX_POINT('',#54300);
#6294=VERTEX_POINT('',#54301);
#6295=VERTEX_POINT('',#54338);
#6296=VERTEX_POINT('',#54339);
#6297=VERTEX_POINT('',#54375);
#6298=VERTEX_POINT('',#54376);
#6299=VERTEX_POINT('',#54412);
#6300=VERTEX_POINT('',#54413);
#6301=VERTEX_POINT('',#54449);
#6302=VERTEX_POINT('',#54450);
#6303=VERTEX_POINT('',#54486);
#6304=VERTEX_POINT('',#54487);
#6305=VERTEX_POINT('',#54524);
#6306=VERTEX_POINT('',#54525);
#6307=VERTEX_POINT('',#54561);
#6308=VERTEX_POINT('',#54562);
#6309=VERTEX_POINT('',#54598);
#6310=VERTEX_POINT('',#54599);
#6311=VERTEX_POINT('',#54635);
#6312=VERTEX_POINT('',#54636);
#6313=VERTEX_POINT('',#54672);
#6314=VERTEX_POINT('',#54673);
#6315=VERTEX_POINT('',#54709);
#6316=VERTEX_POINT('',#54710);
#6317=VERTEX_POINT('',#54746);
#6318=VERTEX_POINT('',#54747);
#6319=VERTEX_POINT('',#54784);
#6320=VERTEX_POINT('',#54785);
#6321=VERTEX_POINT('',#54821);
#6322=VERTEX_POINT('',#54822);
#6323=VERTEX_POINT('',#54858);
#6324=VERTEX_POINT('',#54859);
#6325=VERTEX_POINT('',#54895);
#6326=VERTEX_POINT('',#54896);
#6327=VERTEX_POINT('',#54898);
#6328=VERTEX_POINT('',#54900);
#6329=VERTEX_POINT('',#54904);
#6330=VERTEX_POINT('',#54906);
#6331=VERTEX_POINT('',#54910);
#6332=VERTEX_POINT('',#54912);
#6333=VERTEX_POINT('',#54916);
#6334=VERTEX_POINT('',#54918);
#6335=VERTEX_POINT('',#54922);
#6336=VERTEX_POINT('',#54924);
#6337=VERTEX_POINT('',#54932);
#6338=VERTEX_POINT('',#54934);
#6339=VERTEX_POINT('',#54939);
#6340=VERTEX_POINT('',#54942);
#6341=VERTEX_POINT('',#57075);
#6342=VERTEX_POINT('',#57197);
#6343=VERTEX_POINT('',#59227);
#6344=VERTEX_POINT('',#59230);
#6345=VERTEX_POINT('',#59237);
#6346=VERTEX_POINT('',#59238);
#6347=VERTEX_POINT('',#59240);
#6348=VERTEX_POINT('',#59242);
#6349=VERTEX_POINT('',#59246);
#6350=VERTEX_POINT('',#59247);
#6351=VERTEX_POINT('',#59249);
#6352=VERTEX_POINT('',#59251);
#6353=VERTEX_POINT('',#59264);
#6354=VERTEX_POINT('',#59266);
#6355=VERTEX_POINT('',#59270);
#6356=VERTEX_POINT('',#59272);
#6357=VERTEX_POINT('',#59279);
#6358=VERTEX_POINT('',#59281);
#6359=VERTEX_POINT('',#59285);
#6360=VERTEX_POINT('',#59287);
#6361=VERTEX_POINT('',#59294);
#6362=VERTEX_POINT('',#59295);
#6363=VERTEX_POINT('',#59297);
#6364=VERTEX_POINT('',#59308);
#6365=VERTEX_POINT('',#59318);
#6366=VERTEX_POINT('',#59319);
#6367=VERTEX_POINT('',#59366);
#6368=VERTEX_POINT('',#59367);
#6369=VERTEX_POINT('',#59414);
#6370=VERTEX_POINT('',#59415);
#6371=VERTEX_POINT('',#59465);
#6372=VERTEX_POINT('',#59466);
#6373=VERTEX_POINT('',#59516);
#6374=VERTEX_POINT('',#59517);
#6375=VERTEX_POINT('',#59564);
#6376=VERTEX_POINT('',#59565);
#6377=VERTEX_POINT('',#59612);
#6378=VERTEX_POINT('',#59613);
#6379=VERTEX_POINT('',#59666);
#6380=VERTEX_POINT('',#59667);
#6381=VERTEX_POINT('',#59714);
#6382=VERTEX_POINT('',#59715);
#6383=VERTEX_POINT('',#59762);
#6384=VERTEX_POINT('',#59763);
#6385=VERTEX_POINT('',#59813);
#6386=VERTEX_POINT('',#59814);
#6387=VERTEX_POINT('',#59864);
#6388=VERTEX_POINT('',#59865);
#6389=VERTEX_POINT('',#59912);
#6390=VERTEX_POINT('',#59913);
#6391=VERTEX_POINT('',#59963);
#6392=VERTEX_POINT('',#59964);
#6393=VERTEX_POINT('',#60014);
#6394=VERTEX_POINT('',#60015);
#6395=VERTEX_POINT('',#60062);
#6396=VERTEX_POINT('',#60063);
#6397=VERTEX_POINT('',#60113);
#6398=VERTEX_POINT('',#60114);
#6399=VERTEX_POINT('',#60161);
#6400=VERTEX_POINT('',#60162);
#6401=VERTEX_POINT('',#60212);
#6402=VERTEX_POINT('',#60213);
#6403=VERTEX_POINT('',#60260);
#6404=VERTEX_POINT('',#60261);
#6405=VERTEX_POINT('',#60311);
#6406=VERTEX_POINT('',#60312);
#6407=VERTEX_POINT('',#60362);
#6408=VERTEX_POINT('',#60363);
#6409=VERTEX_POINT('',#60410);
#6410=VERTEX_POINT('',#60411);
#6411=VERTEX_POINT('',#60461);
#6412=VERTEX_POINT('',#60462);
#6413=VERTEX_POINT('',#60509);
#6414=VERTEX_POINT('',#60510);
#6415=VERTEX_POINT('',#60560);
#6416=VERTEX_POINT('',#60561);
#6417=VERTEX_POINT('',#60611);
#6418=VERTEX_POINT('',#60612);
#6419=VERTEX_POINT('',#60659);
#6420=VERTEX_POINT('',#60660);
#6421=VERTEX_POINT('',#60710);
#6422=VERTEX_POINT('',#60711);
#6423=VERTEX_POINT('',#60761);
#6424=VERTEX_POINT('',#60762);
#6425=VERTEX_POINT('',#60809);
#6426=VERTEX_POINT('',#60810);
#6427=VERTEX_POINT('',#60857);
#6428=VERTEX_POINT('',#60858);
#6429=VERTEX_POINT('',#60908);
#6430=VERTEX_POINT('',#60909);
#6431=VERTEX_POINT('',#60959);
#6432=VERTEX_POINT('',#60960);
#6433=VERTEX_POINT('',#61007);
#6434=VERTEX_POINT('',#61008);
#6435=VERTEX_POINT('',#61058);
#6436=VERTEX_POINT('',#61059);
#6437=VERTEX_POINT('',#61109);
#6438=VERTEX_POINT('',#61110);
#6439=VERTEX_POINT('',#61157);
#6440=VERTEX_POINT('',#61158);
#6441=VERTEX_POINT('',#61205);
#6442=VERTEX_POINT('',#61206);
#6443=VERTEX_POINT('',#61208);
#6444=VERTEX_POINT('',#61219);
#6445=VERTEX_POINT('',#61230);
#6446=VERTEX_POINT('',#61231);
#6447=VERTEX_POINT('',#61255);
#6448=VERTEX_POINT('',#61256);
#6449=VERTEX_POINT('',#61279);
#6450=VERTEX_POINT('',#61280);
#6451=VERTEX_POINT('',#61303);
#6452=VERTEX_POINT('',#61304);
#6453=VERTEX_POINT('',#61329);
#6454=VERTEX_POINT('',#61330);
#6455=VERTEX_POINT('',#61353);
#6456=VERTEX_POINT('',#61354);
#6457=VERTEX_POINT('',#61377);
#6458=VERTEX_POINT('',#61378);
#6459=VERTEX_POINT('',#61403);
#6460=VERTEX_POINT('',#61404);
#6461=VERTEX_POINT('',#61427);
#6462=VERTEX_POINT('',#61428);
#6463=VERTEX_POINT('',#61451);
#6464=VERTEX_POINT('',#61452);
#6465=VERTEX_POINT('',#61475);
#6466=VERTEX_POINT('',#61476);
#6467=VERTEX_POINT('',#61501);
#6468=VERTEX_POINT('',#61502);
#6469=VERTEX_POINT('',#61525);
#6470=VERTEX_POINT('',#61526);
#6471=VERTEX_POINT('',#61549);
#6472=VERTEX_POINT('',#61550);
#6473=VERTEX_POINT('',#61575);
#6474=VERTEX_POINT('',#61576);
#6475=VERTEX_POINT('',#61599);
#6476=VERTEX_POINT('',#61600);
#6477=VERTEX_POINT('',#61623);
#6478=VERTEX_POINT('',#61624);
#6479=VERTEX_POINT('',#61648);
#6480=VERTEX_POINT('',#61649);
#6481=VERTEX_POINT('',#61673);
#6482=VERTEX_POINT('',#61674);
#6483=VERTEX_POINT('',#61697);
#6484=VERTEX_POINT('',#61698);
#6485=VERTEX_POINT('',#61722);
#6486=VERTEX_POINT('',#61723);
#6487=VERTEX_POINT('',#61747);
#6488=VERTEX_POINT('',#61748);
#6489=VERTEX_POINT('',#61771);
#6490=VERTEX_POINT('',#61772);
#6491=VERTEX_POINT('',#61795);
#6492=VERTEX_POINT('',#61796);
#6493=VERTEX_POINT('',#61820);
#6494=VERTEX_POINT('',#61821);
#6495=VERTEX_POINT('',#61845);
#6496=VERTEX_POINT('',#61846);
#6497=VERTEX_POINT('',#61869);
#6498=VERTEX_POINT('',#61870);
#6499=VERTEX_POINT('',#61894);
#6500=VERTEX_POINT('',#61895);
#6501=VERTEX_POINT('',#61919);
#6502=VERTEX_POINT('',#61920);
#6503=VERTEX_POINT('',#61943);
#6504=VERTEX_POINT('',#61944);
#6505=VERTEX_POINT('',#61968);
#6506=VERTEX_POINT('',#61969);
#6507=VERTEX_POINT('',#61992);
#6508=VERTEX_POINT('',#61993);
#6509=VERTEX_POINT('',#62017);
#6510=VERTEX_POINT('',#62018);
#6511=VERTEX_POINT('',#62042);
#6512=VERTEX_POINT('',#62043);
#6513=VERTEX_POINT('',#62066);
#6514=VERTEX_POINT('',#62067);
#6515=VERTEX_POINT('',#62091);
#6516=VERTEX_POINT('',#62092);
#6517=VERTEX_POINT('',#62115);
#6518=VERTEX_POINT('',#62116);
#6519=VERTEX_POINT('',#62140);
#6520=VERTEX_POINT('',#62141);
#6521=VERTEX_POINT('',#62164);
#6522=VERTEX_POINT('',#62391);
#6523=VERTEX_POINT('',#62456);
#6524=VERTEX_POINT('',#62489);
#6525=VERTEX_POINT('',#63500);
#6526=VERTEX_POINT('',#63623);
#6527=VERTEX_POINT('',#64769);
#6528=VERTEX_POINT('',#64770);
#6529=VERTEX_POINT('',#64772);
#6530=VERTEX_POINT('',#64774);
#6531=VERTEX_POINT('',#64778);
#6532=VERTEX_POINT('',#64780);
#6533=VERTEX_POINT('',#64784);
#6534=VERTEX_POINT('',#64786);
#6535=VERTEX_POINT('',#64790);
#6536=VERTEX_POINT('',#64792);
#6537=VERTEX_POINT('',#64796);
#6538=VERTEX_POINT('',#64798);
#6539=VERTEX_POINT('',#64806);
#6540=VERTEX_POINT('',#64809);
#6541=VERTEX_POINT('',#64816);
#6542=VERTEX_POINT('',#64818);
#6543=VERTEX_POINT('',#64822);
#6544=VERTEX_POINT('',#64824);
#6545=VERTEX_POINT('',#64831);
#6546=VERTEX_POINT('',#64832);
#6547=VERTEX_POINT('',#64834);
#6548=VERTEX_POINT('',#64845);
#6549=VERTEX_POINT('',#64855);
#6550=VERTEX_POINT('',#64856);
#6551=VERTEX_POINT('',#64903);
#6552=VERTEX_POINT('',#64904);
#6553=VERTEX_POINT('',#64951);
#6554=VERTEX_POINT('',#64952);
#6555=VERTEX_POINT('',#65002);
#6556=VERTEX_POINT('',#65003);
#6557=VERTEX_POINT('',#65053);
#6558=VERTEX_POINT('',#65054);
#6559=VERTEX_POINT('',#65101);
#6560=VERTEX_POINT('',#65102);
#6561=VERTEX_POINT('',#65149);
#6562=VERTEX_POINT('',#65150);
#6563=VERTEX_POINT('',#65200);
#6564=VERTEX_POINT('',#65201);
#6565=VERTEX_POINT('',#65248);
#6566=VERTEX_POINT('',#65249);
#6567=VERTEX_POINT('',#65296);
#6568=VERTEX_POINT('',#65297);
#6569=VERTEX_POINT('',#65347);
#6570=VERTEX_POINT('',#65348);
#6571=VERTEX_POINT('',#65398);
#6572=VERTEX_POINT('',#65399);
#6573=VERTEX_POINT('',#65446);
#6574=VERTEX_POINT('',#65447);
#6575=VERTEX_POINT('',#65497);
#6576=VERTEX_POINT('',#65498);
#6577=VERTEX_POINT('',#65548);
#6578=VERTEX_POINT('',#65549);
#6579=VERTEX_POINT('',#65596);
#6580=VERTEX_POINT('',#65597);
#6581=VERTEX_POINT('',#65647);
#6582=VERTEX_POINT('',#65648);
#6583=VERTEX_POINT('',#65695);
#6584=VERTEX_POINT('',#65696);
#6585=VERTEX_POINT('',#65746);
#6586=VERTEX_POINT('',#65747);
#6587=VERTEX_POINT('',#65797);
#6588=VERTEX_POINT('',#65798);
#6589=VERTEX_POINT('',#65845);
#6590=VERTEX_POINT('',#65846);
#6591=VERTEX_POINT('',#65896);
#6592=VERTEX_POINT('',#65897);
#6593=VERTEX_POINT('',#65947);
#6594=VERTEX_POINT('',#65948);
#6595=VERTEX_POINT('',#65995);
#6596=VERTEX_POINT('',#65996);
#6597=VERTEX_POINT('',#66043);
#6598=VERTEX_POINT('',#66044);
#6599=VERTEX_POINT('',#66094);
#6600=VERTEX_POINT('',#66095);
#6601=VERTEX_POINT('',#66145);
#6602=VERTEX_POINT('',#66146);
#6603=VERTEX_POINT('',#66193);
#6604=VERTEX_POINT('',#66194);
#6605=VERTEX_POINT('',#66244);
#6606=VERTEX_POINT('',#66245);
#6607=VERTEX_POINT('',#66295);
#6608=VERTEX_POINT('',#66296);
#6609=VERTEX_POINT('',#66343);
#6610=VERTEX_POINT('',#66344);
#6611=VERTEX_POINT('',#66346);
#6612=VERTEX_POINT('',#66393);
#6613=VERTEX_POINT('',#66394);
#6614=VERTEX_POINT('',#66396);
#6615=VERTEX_POINT('',#66404);
#6616=VERTEX_POINT('',#66405);
#6617=VERTEX_POINT('',#66417);
#6618=VERTEX_POINT('',#66430);
#6619=VERTEX_POINT('',#66431);
#6620=VERTEX_POINT('',#66454);
#6621=VERTEX_POINT('',#66455);
#6622=VERTEX_POINT('',#66478);
#6623=VERTEX_POINT('',#66479);
#6624=VERTEX_POINT('',#66504);
#6625=VERTEX_POINT('',#66505);
#6626=VERTEX_POINT('',#66528);
#6627=VERTEX_POINT('',#66529);
#6628=VERTEX_POINT('',#66552);
#6629=VERTEX_POINT('',#66553);
#6630=VERTEX_POINT('',#66578);
#6631=VERTEX_POINT('',#66579);
#6632=VERTEX_POINT('',#66602);
#6633=VERTEX_POINT('',#66603);
#6634=VERTEX_POINT('',#66626);
#6635=VERTEX_POINT('',#66627);
#6636=VERTEX_POINT('',#66650);
#6637=VERTEX_POINT('',#66651);
#6638=VERTEX_POINT('',#66676);
#6639=VERTEX_POINT('',#66677);
#6640=VERTEX_POINT('',#66700);
#6641=VERTEX_POINT('',#66701);
#6642=VERTEX_POINT('',#66724);
#6643=VERTEX_POINT('',#66725);
#6644=VERTEX_POINT('',#66750);
#6645=VERTEX_POINT('',#66751);
#6646=VERTEX_POINT('',#66774);
#6647=VERTEX_POINT('',#66775);
#6648=VERTEX_POINT('',#66798);
#6649=VERTEX_POINT('',#66799);
#6650=VERTEX_POINT('',#66823);
#6651=VERTEX_POINT('',#66824);
#6652=VERTEX_POINT('',#66848);
#6653=VERTEX_POINT('',#66849);
#6654=VERTEX_POINT('',#66872);
#6655=VERTEX_POINT('',#66873);
#6656=VERTEX_POINT('',#66897);
#6657=VERTEX_POINT('',#66898);
#6658=VERTEX_POINT('',#66922);
#6659=VERTEX_POINT('',#66923);
#6660=VERTEX_POINT('',#66946);
#6661=VERTEX_POINT('',#66947);
#6662=VERTEX_POINT('',#66971);
#6663=VERTEX_POINT('',#66972);
#6664=VERTEX_POINT('',#66995);
#6665=VERTEX_POINT('',#66996);
#6666=VERTEX_POINT('',#67020);
#6667=VERTEX_POINT('',#67021);
#6668=VERTEX_POINT('',#67044);
#6669=VERTEX_POINT('',#67045);
#6670=VERTEX_POINT('',#67069);
#6671=VERTEX_POINT('',#67070);
#6672=VERTEX_POINT('',#67094);
#6673=VERTEX_POINT('',#67095);
#6674=VERTEX_POINT('',#67118);
#6675=VERTEX_POINT('',#67119);
#6676=VERTEX_POINT('',#67143);
#6677=VERTEX_POINT('',#67144);
#6678=VERTEX_POINT('',#67167);
#6679=VERTEX_POINT('',#67169);
#6680=VERTEX_POINT('',#67430);
#6681=VERTEX_POINT('',#68320);
#6682=VERTEX_POINT('',#68427);
#6683=VERTEX_POINT('',#69371);
#6684=VERTEX_POINT('',#69372);
#6685=VERTEX_POINT('',#69374);
#6686=VERTEX_POINT('',#69376);
#6687=VERTEX_POINT('',#69380);
#6688=VERTEX_POINT('',#69382);
#6689=VERTEX_POINT('',#69386);
#6690=VERTEX_POINT('',#69388);
#6691=VERTEX_POINT('',#69392);
#6692=VERTEX_POINT('',#69394);
#6693=VERTEX_POINT('',#69398);
#6694=VERTEX_POINT('',#69400);
#6695=VERTEX_POINT('',#69408);
#6696=VERTEX_POINT('',#69411);
#6697=EDGE_CURVE('',#5223,#5224,#3527,.T.);
#6698=EDGE_CURVE('',#5224,#5225,#2347,.T.);
#6699=EDGE_CURVE('',#5225,#5226,#2151,.T.);
#6700=EDGE_CURVE('',#5226,#5227,#3528,.T.);
#6701=EDGE_CURVE('',#5227,#5227,#2152,.F.);
#6702=EDGE_CURVE('',#5226,#5228,#2153,.T.);
#6703=EDGE_CURVE('',#5228,#5223,#2348,.T.);
#6704=EDGE_CURVE('',#5229,#5230,#3529,.T.);
#6705=EDGE_CURVE('',#5230,#5224,#2349,.T.);
#6706=EDGE_CURVE('',#5223,#5229,#2350,.T.);
#6707=EDGE_CURVE('',#5231,#5232,#3530,.T.);
#6708=EDGE_CURVE('',#5232,#5230,#2351,.T.);
#6709=EDGE_CURVE('',#5229,#5231,#2352,.T.);
#6710=EDGE_CURVE('',#5233,#5234,#3531,.T.);
#6711=EDGE_CURVE('',#5234,#5232,#2353,.T.);
#6712=EDGE_CURVE('',#5231,#5233,#2354,.T.);
#6713=EDGE_CURVE('',#5235,#5236,#3532,.T.);
#6714=EDGE_CURVE('',#5236,#5234,#2355,.T.);
#6715=EDGE_CURVE('',#5233,#5235,#2356,.T.);
#6716=EDGE_CURVE('',#5237,#5238,#3533,.T.);
#6717=EDGE_CURVE('',#5238,#5236,#2357,.T.);
#6718=EDGE_CURVE('',#5235,#5237,#2358,.T.);
#6719=EDGE_CURVE('',#5239,#5240,#3534,.T.);
#6720=EDGE_CURVE('',#5240,#5238,#2359,.T.);
#6721=EDGE_CURVE('',#5237,#5239,#2360,.T.);
#6722=EDGE_CURVE('',#5241,#5242,#3535,.T.);
#6723=EDGE_CURVE('',#5242,#5240,#2361,.T.);
#6724=EDGE_CURVE('',#5239,#5241,#2362,.T.);
#6725=EDGE_CURVE('',#5243,#5244,#3536,.T.);
#6726=EDGE_CURVE('',#5243,#5245,#2363,.T.);
#6727=EDGE_CURVE('',#5246,#5245,#2154,.F.);
#6728=EDGE_CURVE('',#5246,#5244,#2364,.T.);
#6729=EDGE_CURVE('',#5247,#5248,#3537,.T.);
#6730=EDGE_CURVE('',#5248,#5249,#2365,.T.);
#6731=EDGE_CURVE('',#5250,#5249,#2155,.T.);
#6732=EDGE_CURVE('',#5247,#5250,#2366,.T.);
#6733=EDGE_CURVE('',#5251,#5252,#3538,.T.);
#6734=EDGE_CURVE('',#5252,#5248,#2367,.T.);
#6735=EDGE_CURVE('',#5251,#5247,#2368,.T.);
#6736=EDGE_CURVE('',#5253,#5254,#3539,.T.);
#6737=EDGE_CURVE('',#5254,#5252,#2369,.T.);
#6738=EDGE_CURVE('',#5253,#5251,#2370,.T.);
#6739=EDGE_CURVE('',#5255,#5256,#3540,.T.);
#6740=EDGE_CURVE('',#5256,#5254,#2371,.T.);
#6741=EDGE_CURVE('',#5255,#5253,#2372,.T.);
#6742=EDGE_CURVE('',#5257,#5258,#3541,.T.);
#6743=EDGE_CURVE('',#5258,#5256,#2373,.T.);
#6744=EDGE_CURVE('',#5257,#5255,#2374,.T.);
#6745=EDGE_CURVE('',#5259,#5260,#3542,.T.);
#6746=EDGE_CURVE('',#5260,#5258,#2375,.T.);
#6747=EDGE_CURVE('',#5259,#5257,#2376,.T.);
#6748=EDGE_CURVE('',#5261,#5262,#3543,.T.);
#6749=EDGE_CURVE('',#5262,#5260,#2377,.T.);
#6750=EDGE_CURVE('',#5261,#5259,#2378,.T.);
#6751=EDGE_CURVE('',#5263,#5264,#3544,.T.);
#6752=EDGE_CURVE('',#5264,#5262,#2379,.T.);
#6753=EDGE_CURVE('',#5263,#5261,#2380,.T.);
#6754=EDGE_CURVE('',#5265,#5266,#3545,.T.);
#6755=EDGE_CURVE('',#5267,#5265,#2381,.T.);
#6756=EDGE_CURVE('',#5268,#5267,#2156,.T.);
#6757=EDGE_CURVE('',#5268,#5266,#2382,.T.);
#6758=EDGE_CURVE('',#5269,#5270,#3546,.T.);
#6759=EDGE_CURVE('',#5270,#5271,#2383,.T.);
#6760=EDGE_CURVE('',#5271,#5272,#2157,.T.);
#6761=EDGE_CURVE('',#5272,#5273,#3547,.T.);
#6762=EDGE_CURVE('',#5273,#5273,#2158,.F.);
#6763=EDGE_CURVE('',#5272,#5274,#2159,.T.);
#6764=EDGE_CURVE('',#5274,#5269,#2384,.T.);
#6765=EDGE_CURVE('',#5275,#5276,#3548,.T.);
#6766=EDGE_CURVE('',#5276,#5270,#2385,.T.);
#6767=EDGE_CURVE('',#5269,#5275,#2386,.T.);
#6768=EDGE_CURVE('',#5277,#5278,#3549,.T.);
#6769=EDGE_CURVE('',#5278,#5276,#2387,.T.);
#6770=EDGE_CURVE('',#5275,#5277,#2388,.T.);
#6771=EDGE_CURVE('',#5279,#5280,#3550,.T.);
#6772=EDGE_CURVE('',#5280,#5278,#2389,.T.);
#6773=EDGE_CURVE('',#5277,#5279,#2390,.T.);
#6774=EDGE_CURVE('',#5281,#5282,#3551,.T.);
#6775=EDGE_CURVE('',#5282,#5280,#2391,.T.);
#6776=EDGE_CURVE('',#5279,#5281,#2392,.T.);
#6777=EDGE_CURVE('',#5283,#5284,#3552,.T.);
#6778=EDGE_CURVE('',#5284,#5282,#2393,.T.);
#6779=EDGE_CURVE('',#5281,#5283,#2394,.T.);
#6780=EDGE_CURVE('',#5285,#5286,#3553,.T.);
#6781=EDGE_CURVE('',#5286,#5284,#2395,.T.);
#6782=EDGE_CURVE('',#5283,#5285,#2396,.T.);
#6783=EDGE_CURVE('',#5287,#5288,#3554,.T.);
#6784=EDGE_CURVE('',#5288,#5286,#2397,.T.);
#6785=EDGE_CURVE('',#5285,#5287,#2398,.T.);
#6786=EDGE_CURVE('',#5289,#5290,#3555,.T.);
#6787=EDGE_CURVE('',#5289,#5291,#2399,.T.);
#6788=EDGE_CURVE('',#5292,#5291,#2160,.F.);
#6789=EDGE_CURVE('',#5292,#5290,#2400,.T.);
#6790=EDGE_CURVE('',#5293,#5294,#3556,.T.);
#6791=EDGE_CURVE('',#5294,#5295,#2401,.T.);
#6792=EDGE_CURVE('',#5296,#5295,#2161,.T.);
#6793=EDGE_CURVE('',#5293,#5296,#2402,.T.);
#6794=EDGE_CURVE('',#5297,#5298,#3557,.T.);
#6795=EDGE_CURVE('',#5298,#5294,#2403,.T.);
#6796=EDGE_CURVE('',#5297,#5293,#2404,.T.);
#6797=EDGE_CURVE('',#5299,#5300,#3558,.T.);
#6798=EDGE_CURVE('',#5300,#5298,#2405,.T.);
#6799=EDGE_CURVE('',#5299,#5297,#2406,.T.);
#6800=EDGE_CURVE('',#5301,#5302,#3559,.T.);
#6801=EDGE_CURVE('',#5302,#5300,#2407,.T.);
#6802=EDGE_CURVE('',#5301,#5299,#2408,.T.);
#6803=EDGE_CURVE('',#5303,#5304,#3560,.T.);
#6804=EDGE_CURVE('',#5304,#5302,#2409,.T.);
#6805=EDGE_CURVE('',#5303,#5301,#2410,.T.);
#6806=EDGE_CURVE('',#5305,#5306,#3561,.T.);
#6807=EDGE_CURVE('',#5306,#5304,#2411,.T.);
#6808=EDGE_CURVE('',#5305,#5303,#2412,.T.);
#6809=EDGE_CURVE('',#5307,#5308,#3562,.T.);
#6810=EDGE_CURVE('',#5308,#5306,#2413,.T.);
#6811=EDGE_CURVE('',#5307,#5305,#2414,.T.);
#6812=EDGE_CURVE('',#5309,#5310,#3563,.T.);
#6813=EDGE_CURVE('',#5310,#5308,#2415,.T.);
#6814=EDGE_CURVE('',#5309,#5307,#2416,.T.);
#6815=EDGE_CURVE('',#5311,#5312,#3564,.T.);
#6816=EDGE_CURVE('',#5313,#5311,#2417,.T.);
#6817=EDGE_CURVE('',#5314,#5313,#2162,.T.);
#6818=EDGE_CURVE('',#5314,#5312,#2418,.T.);
#6819=EDGE_CURVE('',#5315,#5316,#3565,.T.);
#6820=EDGE_CURVE('',#5316,#5317,#2419,.T.);
#6821=EDGE_CURVE('',#5317,#5318,#2163,.T.);
#6822=EDGE_CURVE('',#5318,#5319,#3566,.T.);
#6823=EDGE_CURVE('',#5319,#5319,#2164,.F.);
#6824=EDGE_CURVE('',#5318,#5320,#2165,.T.);
#6825=EDGE_CURVE('',#5320,#5315,#2420,.T.);
#6826=EDGE_CURVE('',#5321,#5322,#3567,.T.);
#6827=EDGE_CURVE('',#5322,#5316,#2421,.T.);
#6828=EDGE_CURVE('',#5315,#5321,#2422,.T.);
#6829=EDGE_CURVE('',#5323,#5324,#3568,.T.);
#6830=EDGE_CURVE('',#5324,#5322,#2423,.T.);
#6831=EDGE_CURVE('',#5321,#5323,#2424,.T.);
#6832=EDGE_CURVE('',#5325,#5326,#3569,.T.);
#6833=EDGE_CURVE('',#5326,#5324,#2425,.T.);
#6834=EDGE_CURVE('',#5323,#5325,#2426,.T.);
#6835=EDGE_CURVE('',#5327,#5328,#3570,.T.);
#6836=EDGE_CURVE('',#5328,#5326,#2427,.T.);
#6837=EDGE_CURVE('',#5325,#5327,#2428,.T.);
#6838=EDGE_CURVE('',#5329,#5330,#3571,.T.);
#6839=EDGE_CURVE('',#5330,#5328,#2429,.T.);
#6840=EDGE_CURVE('',#5327,#5329,#2430,.T.);
#6841=EDGE_CURVE('',#5331,#5332,#3572,.T.);
#6842=EDGE_CURVE('',#5332,#5330,#2431,.T.);
#6843=EDGE_CURVE('',#5329,#5331,#2432,.T.);
#6844=EDGE_CURVE('',#5333,#5334,#3573,.T.);
#6845=EDGE_CURVE('',#5334,#5332,#2433,.T.);
#6846=EDGE_CURVE('',#5331,#5333,#2434,.T.);
#6847=EDGE_CURVE('',#5335,#5336,#3574,.T.);
#6848=EDGE_CURVE('',#5335,#5337,#2435,.T.);
#6849=EDGE_CURVE('',#5338,#5337,#2166,.F.);
#6850=EDGE_CURVE('',#5338,#5336,#2436,.T.);
#6851=EDGE_CURVE('',#5339,#5340,#3575,.T.);
#6852=EDGE_CURVE('',#5340,#5341,#2437,.T.);
#6853=EDGE_CURVE('',#5342,#5341,#2167,.T.);
#6854=EDGE_CURVE('',#5339,#5342,#2438,.T.);
#6855=EDGE_CURVE('',#5343,#5344,#3576,.T.);
#6856=EDGE_CURVE('',#5344,#5340,#2439,.T.);
#6857=EDGE_CURVE('',#5343,#5339,#2440,.T.);
#6858=EDGE_CURVE('',#5345,#5346,#3577,.T.);
#6859=EDGE_CURVE('',#5346,#5344,#2441,.T.);
#6860=EDGE_CURVE('',#5345,#5343,#2442,.T.);
#6861=EDGE_CURVE('',#5347,#5348,#3578,.T.);
#6862=EDGE_CURVE('',#5348,#5346,#2443,.T.);
#6863=EDGE_CURVE('',#5347,#5345,#2444,.T.);
#6864=EDGE_CURVE('',#5349,#5350,#3579,.T.);
#6865=EDGE_CURVE('',#5350,#5348,#2445,.T.);
#6866=EDGE_CURVE('',#5349,#5347,#2446,.T.);
#6867=EDGE_CURVE('',#5351,#5352,#3580,.T.);
#6868=EDGE_CURVE('',#5352,#5350,#2447,.T.);
#6869=EDGE_CURVE('',#5351,#5349,#2448,.T.);
#6870=EDGE_CURVE('',#5353,#5354,#3581,.T.);
#6871=EDGE_CURVE('',#5354,#5352,#2449,.T.);
#6872=EDGE_CURVE('',#5353,#5351,#2450,.T.);
#6873=EDGE_CURVE('',#5355,#5356,#3582,.T.);
#6874=EDGE_CURVE('',#5356,#5354,#2451,.T.);
#6875=EDGE_CURVE('',#5355,#5353,#2452,.T.);
#6876=EDGE_CURVE('',#5357,#5358,#3583,.T.);
#6877=EDGE_CURVE('',#5359,#5357,#2453,.T.);
#6878=EDGE_CURVE('',#5360,#5359,#2168,.T.);
#6879=EDGE_CURVE('',#5360,#5358,#2454,.T.);
#6880=EDGE_CURVE('',#5361,#5362,#3584,.T.);
#6881=EDGE_CURVE('',#5362,#5363,#2455,.T.);
#6882=EDGE_CURVE('',#5363,#5364,#2169,.T.);
#6883=EDGE_CURVE('',#5364,#5365,#3585,.T.);
#6884=EDGE_CURVE('',#5365,#5365,#2170,.F.);
#6885=EDGE_CURVE('',#5364,#5366,#2171,.T.);
#6886=EDGE_CURVE('',#5366,#5361,#2456,.T.);
#6887=EDGE_CURVE('',#5367,#5368,#3586,.T.);
#6888=EDGE_CURVE('',#5368,#5362,#2457,.T.);
#6889=EDGE_CURVE('',#5361,#5367,#2458,.T.);
#6890=EDGE_CURVE('',#5369,#5370,#3587,.T.);
#6891=EDGE_CURVE('',#5370,#5368,#2459,.T.);
#6892=EDGE_CURVE('',#5367,#5369,#2460,.T.);
#6893=EDGE_CURVE('',#5371,#5372,#3588,.T.);
#6894=EDGE_CURVE('',#5372,#5370,#2461,.T.);
#6895=EDGE_CURVE('',#5369,#5371,#2462,.T.);
#6896=EDGE_CURVE('',#5373,#5374,#3589,.T.);
#6897=EDGE_CURVE('',#5374,#5372,#2463,.T.);
#6898=EDGE_CURVE('',#5371,#5373,#2464,.T.);
#6899=EDGE_CURVE('',#5375,#5376,#3590,.T.);
#6900=EDGE_CURVE('',#5376,#5374,#2465,.T.);
#6901=EDGE_CURVE('',#5373,#5375,#2466,.T.);
#6902=EDGE_CURVE('',#5377,#5378,#3591,.T.);
#6903=EDGE_CURVE('',#5378,#5376,#2467,.T.);
#6904=EDGE_CURVE('',#5375,#5377,#2468,.T.);
#6905=EDGE_CURVE('',#5379,#5380,#3592,.T.);
#6906=EDGE_CURVE('',#5380,#5378,#2469,.T.);
#6907=EDGE_CURVE('',#5377,#5379,#2470,.T.);
#6908=EDGE_CURVE('',#5381,#5382,#3593,.T.);
#6909=EDGE_CURVE('',#5381,#5383,#2471,.T.);
#6910=EDGE_CURVE('',#5384,#5383,#2172,.F.);
#6911=EDGE_CURVE('',#5384,#5382,#2472,.T.);
#6912=EDGE_CURVE('',#5385,#5386,#3594,.T.);
#6913=EDGE_CURVE('',#5386,#5387,#2473,.T.);
#6914=EDGE_CURVE('',#5388,#5387,#2173,.T.);
#6915=EDGE_CURVE('',#5385,#5388,#2474,.T.);
#6916=EDGE_CURVE('',#5389,#5390,#3595,.T.);
#6917=EDGE_CURVE('',#5390,#5386,#2475,.T.);
#6918=EDGE_CURVE('',#5389,#5385,#2476,.T.);
#6919=EDGE_CURVE('',#5391,#5392,#3596,.T.);
#6920=EDGE_CURVE('',#5392,#5390,#2477,.T.);
#6921=EDGE_CURVE('',#5391,#5389,#2478,.T.);
#6922=EDGE_CURVE('',#5393,#5394,#3597,.T.);
#6923=EDGE_CURVE('',#5394,#5392,#2479,.T.);
#6924=EDGE_CURVE('',#5393,#5391,#2480,.T.);
#6925=EDGE_CURVE('',#5395,#5396,#3598,.T.);
#6926=EDGE_CURVE('',#5396,#5394,#2481,.T.);
#6927=EDGE_CURVE('',#5395,#5393,#2482,.T.);
#6928=EDGE_CURVE('',#5397,#5398,#3599,.T.);
#6929=EDGE_CURVE('',#5398,#5396,#2483,.T.);
#6930=EDGE_CURVE('',#5397,#5395,#2484,.T.);
#6931=EDGE_CURVE('',#5399,#5400,#3600,.T.);
#6932=EDGE_CURVE('',#5400,#5398,#2485,.T.);
#6933=EDGE_CURVE('',#5399,#5397,#2486,.T.);
#6934=EDGE_CURVE('',#5401,#5402,#3601,.T.);
#6935=EDGE_CURVE('',#5402,#5400,#2487,.T.);
#6936=EDGE_CURVE('',#5401,#5399,#2488,.T.);
#6937=EDGE_CURVE('',#5403,#5404,#3602,.T.);
#6938=EDGE_CURVE('',#5405,#5403,#2489,.T.);
#6939=EDGE_CURVE('',#5406,#5405,#2174,.T.);
#6940=EDGE_CURVE('',#5406,#5404,#2490,.T.);
#6941=EDGE_CURVE('',#5407,#5408,#3603,.T.);
#6942=EDGE_CURVE('',#5408,#5409,#2491,.T.);
#6943=EDGE_CURVE('',#5409,#5410,#2175,.T.);
#6944=EDGE_CURVE('',#5410,#5411,#3604,.T.);
#6945=EDGE_CURVE('',#5411,#5411,#2176,.F.);
#6946=EDGE_CURVE('',#5410,#5412,#2177,.T.);
#6947=EDGE_CURVE('',#5412,#5407,#2492,.T.);
#6948=EDGE_CURVE('',#5413,#5414,#3605,.T.);
#6949=EDGE_CURVE('',#5414,#5408,#2493,.T.);
#6950=EDGE_CURVE('',#5407,#5413,#2494,.T.);
#6951=EDGE_CURVE('',#5415,#5416,#3606,.T.);
#6952=EDGE_CURVE('',#5416,#5414,#2495,.T.);
#6953=EDGE_CURVE('',#5413,#5415,#2496,.T.);
#6954=EDGE_CURVE('',#5417,#5418,#3607,.T.);
#6955=EDGE_CURVE('',#5418,#5416,#2497,.T.);
#6956=EDGE_CURVE('',#5415,#5417,#2498,.T.);
#6957=EDGE_CURVE('',#5419,#5420,#3608,.T.);
#6958=EDGE_CURVE('',#5420,#5418,#2499,.T.);
#6959=EDGE_CURVE('',#5417,#5419,#2500,.T.);
#6960=EDGE_CURVE('',#5421,#5422,#3609,.T.);
#6961=EDGE_CURVE('',#5422,#5420,#2501,.T.);
#6962=EDGE_CURVE('',#5419,#5421,#2502,.T.);
#6963=EDGE_CURVE('',#5423,#5424,#3610,.T.);
#6964=EDGE_CURVE('',#5424,#5422,#2503,.T.);
#6965=EDGE_CURVE('',#5421,#5423,#2504,.T.);
#6966=EDGE_CURVE('',#5425,#5426,#3611,.T.);
#6967=EDGE_CURVE('',#5426,#5424,#2505,.T.);
#6968=EDGE_CURVE('',#5423,#5425,#2506,.T.);
#6969=EDGE_CURVE('',#5427,#5428,#3612,.T.);
#6970=EDGE_CURVE('',#5427,#5429,#2507,.T.);
#6971=EDGE_CURVE('',#5430,#5429,#2178,.F.);
#6972=EDGE_CURVE('',#5430,#5428,#2508,.T.);
#6973=EDGE_CURVE('',#5431,#5432,#3613,.T.);
#6974=EDGE_CURVE('',#5432,#5433,#2509,.T.);
#6975=EDGE_CURVE('',#5434,#5433,#2179,.T.);
#6976=EDGE_CURVE('',#5431,#5434,#2510,.T.);
#6977=EDGE_CURVE('',#5435,#5436,#3614,.T.);
#6978=EDGE_CURVE('',#5436,#5432,#2511,.T.);
#6979=EDGE_CURVE('',#5435,#5431,#2512,.T.);
#6980=EDGE_CURVE('',#5437,#5438,#3615,.T.);
#6981=EDGE_CURVE('',#5438,#5436,#2513,.T.);
#6982=EDGE_CURVE('',#5437,#5435,#2514,.T.);
#6983=EDGE_CURVE('',#5439,#5440,#3616,.T.);
#6984=EDGE_CURVE('',#5440,#5438,#2515,.T.);
#6985=EDGE_CURVE('',#5439,#5437,#2516,.T.);
#6986=EDGE_CURVE('',#5441,#5442,#3617,.T.);
#6987=EDGE_CURVE('',#5442,#5440,#2517,.T.);
#6988=EDGE_CURVE('',#5441,#5439,#2518,.T.);
#6989=EDGE_CURVE('',#5443,#5444,#3618,.T.);
#6990=EDGE_CURVE('',#5444,#5442,#2519,.T.);
#6991=EDGE_CURVE('',#5443,#5441,#2520,.T.);
#6992=EDGE_CURVE('',#5445,#5446,#3619,.T.);
#6993=EDGE_CURVE('',#5446,#5444,#2521,.T.);
#6994=EDGE_CURVE('',#5445,#5443,#2522,.T.);
#6995=EDGE_CURVE('',#5447,#5448,#3620,.T.);
#6996=EDGE_CURVE('',#5448,#5446,#2523,.T.);
#6997=EDGE_CURVE('',#5447,#5445,#2524,.T.);
#6998=EDGE_CURVE('',#5449,#5450,#3621,.T.);
#6999=EDGE_CURVE('',#5451,#5449,#2525,.T.);
#7000=EDGE_CURVE('',#5452,#5451,#2180,.T.);
#7001=EDGE_CURVE('',#5452,#5450,#2526,.T.);
#7002=EDGE_CURVE('',#5453,#5454,#3622,.T.);
#7003=EDGE_CURVE('',#5454,#5455,#2527,.T.);
#7004=EDGE_CURVE('',#5455,#5456,#2181,.T.);
#7005=EDGE_CURVE('',#5456,#5457,#3623,.T.);
#7006=EDGE_CURVE('',#5457,#5457,#2182,.F.);
#7007=EDGE_CURVE('',#5456,#5458,#2183,.T.);
#7008=EDGE_CURVE('',#5458,#5453,#2528,.T.);
#7009=EDGE_CURVE('',#5459,#5460,#3624,.T.);
#7010=EDGE_CURVE('',#5460,#5454,#2529,.T.);
#7011=EDGE_CURVE('',#5453,#5459,#2530,.T.);
#7012=EDGE_CURVE('',#5461,#5462,#3625,.T.);
#7013=EDGE_CURVE('',#5462,#5460,#2531,.T.);
#7014=EDGE_CURVE('',#5459,#5461,#2532,.T.);
#7015=EDGE_CURVE('',#5463,#5464,#3626,.T.);
#7016=EDGE_CURVE('',#5464,#5462,#2533,.T.);
#7017=EDGE_CURVE('',#5461,#5463,#2534,.T.);
#7018=EDGE_CURVE('',#5465,#5466,#3627,.T.);
#7019=EDGE_CURVE('',#5466,#5464,#2535,.T.);
#7020=EDGE_CURVE('',#5463,#5465,#2536,.T.);
#7021=EDGE_CURVE('',#5467,#5468,#3628,.T.);
#7022=EDGE_CURVE('',#5468,#5466,#2537,.T.);
#7023=EDGE_CURVE('',#5465,#5467,#2538,.T.);
#7024=EDGE_CURVE('',#5469,#5470,#3629,.T.);
#7025=EDGE_CURVE('',#5470,#5468,#2539,.T.);
#7026=EDGE_CURVE('',#5467,#5469,#2540,.T.);
#7027=EDGE_CURVE('',#5471,#5472,#3630,.T.);
#7028=EDGE_CURVE('',#5472,#5470,#2541,.T.);
#7029=EDGE_CURVE('',#5469,#5471,#2542,.T.);
#7030=EDGE_CURVE('',#5473,#5474,#3631,.T.);
#7031=EDGE_CURVE('',#5473,#5475,#2543,.T.);
#7032=EDGE_CURVE('',#5476,#5475,#2184,.F.);
#7033=EDGE_CURVE('',#5476,#5474,#2544,.T.);
#7034=EDGE_CURVE('',#5477,#5478,#3632,.T.);
#7035=EDGE_CURVE('',#5478,#5479,#2545,.T.);
#7036=EDGE_CURVE('',#5480,#5479,#2185,.T.);
#7037=EDGE_CURVE('',#5477,#5480,#2546,.T.);
#7038=EDGE_CURVE('',#5481,#5482,#3633,.T.);
#7039=EDGE_CURVE('',#5482,#5478,#2547,.T.);
#7040=EDGE_CURVE('',#5481,#5477,#2548,.T.);
#7041=EDGE_CURVE('',#5483,#5484,#3634,.T.);
#7042=EDGE_CURVE('',#5484,#5482,#2549,.T.);
#7043=EDGE_CURVE('',#5483,#5481,#2550,.T.);
#7044=EDGE_CURVE('',#5485,#5486,#3635,.T.);
#7045=EDGE_CURVE('',#5486,#5484,#2551,.T.);
#7046=EDGE_CURVE('',#5485,#5483,#2552,.T.);
#7047=EDGE_CURVE('',#5487,#5488,#3636,.T.);
#7048=EDGE_CURVE('',#5488,#5486,#2553,.T.);
#7049=EDGE_CURVE('',#5487,#5485,#2554,.T.);
#7050=EDGE_CURVE('',#5489,#5490,#3637,.T.);
#7051=EDGE_CURVE('',#5490,#5488,#2555,.T.);
#7052=EDGE_CURVE('',#5489,#5487,#2556,.T.);
#7053=EDGE_CURVE('',#5491,#5492,#3638,.T.);
#7054=EDGE_CURVE('',#5492,#5490,#2557,.T.);
#7055=EDGE_CURVE('',#5491,#5489,#2558,.T.);
#7056=EDGE_CURVE('',#5493,#5494,#3639,.T.);
#7057=EDGE_CURVE('',#5494,#5492,#2559,.T.);
#7058=EDGE_CURVE('',#5493,#5491,#2560,.T.);
#7059=EDGE_CURVE('',#5495,#5496,#3640,.T.);
#7060=EDGE_CURVE('',#5497,#5495,#2561,.T.);
#7061=EDGE_CURVE('',#5498,#5497,#2186,.T.);
#7062=EDGE_CURVE('',#5498,#5496,#2562,.T.);
#7063=EDGE_CURVE('',#5499,#5500,#3641,.T.);
#7064=EDGE_CURVE('',#5500,#5501,#2563,.T.);
#7065=EDGE_CURVE('',#5501,#5502,#2187,.T.);
#7066=EDGE_CURVE('',#5502,#5503,#3642,.T.);
#7067=EDGE_CURVE('',#5503,#5503,#2188,.F.);
#7068=EDGE_CURVE('',#5502,#5504,#2189,.T.);
#7069=EDGE_CURVE('',#5504,#5499,#2564,.T.);
#7070=EDGE_CURVE('',#5505,#5506,#3643,.T.);
#7071=EDGE_CURVE('',#5506,#5500,#2565,.T.);
#7072=EDGE_CURVE('',#5499,#5505,#2566,.T.);
#7073=EDGE_CURVE('',#5507,#5508,#3644,.T.);
#7074=EDGE_CURVE('',#5508,#5506,#2567,.T.);
#7075=EDGE_CURVE('',#5505,#5507,#2568,.T.);
#7076=EDGE_CURVE('',#5509,#5510,#3645,.T.);
#7077=EDGE_CURVE('',#5510,#5508,#2569,.T.);
#7078=EDGE_CURVE('',#5507,#5509,#2570,.T.);
#7079=EDGE_CURVE('',#5511,#5512,#3646,.T.);
#7080=EDGE_CURVE('',#5512,#5510,#2571,.T.);
#7081=EDGE_CURVE('',#5509,#5511,#2572,.T.);
#7082=EDGE_CURVE('',#5513,#5514,#3647,.T.);
#7083=EDGE_CURVE('',#5514,#5512,#2573,.T.);
#7084=EDGE_CURVE('',#5511,#5513,#2574,.T.);
#7085=EDGE_CURVE('',#5515,#5516,#3648,.T.);
#7086=EDGE_CURVE('',#5516,#5514,#2575,.T.);
#7087=EDGE_CURVE('',#5513,#5515,#2576,.T.);
#7088=EDGE_CURVE('',#5517,#5518,#3649,.T.);
#7089=EDGE_CURVE('',#5518,#5516,#2577,.T.);
#7090=EDGE_CURVE('',#5515,#5517,#2578,.T.);
#7091=EDGE_CURVE('',#5519,#5520,#3650,.T.);
#7092=EDGE_CURVE('',#5519,#5521,#2579,.T.);
#7093=EDGE_CURVE('',#5522,#5521,#2190,.F.);
#7094=EDGE_CURVE('',#5522,#5520,#2580,.T.);
#7095=EDGE_CURVE('',#5523,#5524,#3651,.T.);
#7096=EDGE_CURVE('',#5524,#5525,#2581,.T.);
#7097=EDGE_CURVE('',#5526,#5525,#2191,.T.);
#7098=EDGE_CURVE('',#5523,#5526,#2582,.T.);
#7099=EDGE_CURVE('',#5527,#5528,#3652,.T.);
#7100=EDGE_CURVE('',#5528,#5524,#2583,.T.);
#7101=EDGE_CURVE('',#5527,#5523,#2584,.T.);
#7102=EDGE_CURVE('',#5529,#5530,#3653,.T.);
#7103=EDGE_CURVE('',#5530,#5528,#2585,.T.);
#7104=EDGE_CURVE('',#5529,#5527,#2586,.T.);
#7105=EDGE_CURVE('',#5531,#5532,#3654,.T.);
#7106=EDGE_CURVE('',#5532,#5530,#2587,.T.);
#7107=EDGE_CURVE('',#5531,#5529,#2588,.T.);
#7108=EDGE_CURVE('',#5533,#5534,#3655,.T.);
#7109=EDGE_CURVE('',#5534,#5532,#2589,.T.);
#7110=EDGE_CURVE('',#5533,#5531,#2590,.T.);
#7111=EDGE_CURVE('',#5535,#5536,#3656,.T.);
#7112=EDGE_CURVE('',#5536,#5534,#2591,.T.);
#7113=EDGE_CURVE('',#5535,#5533,#2592,.T.);
#7114=EDGE_CURVE('',#5537,#5538,#3657,.T.);
#7115=EDGE_CURVE('',#5538,#5536,#2593,.T.);
#7116=EDGE_CURVE('',#5537,#5535,#2594,.T.);
#7117=EDGE_CURVE('',#5539,#5540,#3658,.T.);
#7118=EDGE_CURVE('',#5540,#5538,#2595,.T.);
#7119=EDGE_CURVE('',#5539,#5537,#2596,.T.);
#7120=EDGE_CURVE('',#5541,#5542,#3659,.T.);
#7121=EDGE_CURVE('',#5543,#5541,#2597,.T.);
#7122=EDGE_CURVE('',#5544,#5543,#2192,.T.);
#7123=EDGE_CURVE('',#5544,#5542,#2598,.T.);
#7124=EDGE_CURVE('',#5545,#5546,#3660,.T.);
#7125=EDGE_CURVE('',#5546,#5547,#2599,.T.);
#7126=EDGE_CURVE('',#5547,#5548,#2193,.T.);
#7127=EDGE_CURVE('',#5548,#5549,#3661,.T.);
#7128=EDGE_CURVE('',#5549,#5549,#2194,.F.);
#7129=EDGE_CURVE('',#5548,#5550,#2195,.T.);
#7130=EDGE_CURVE('',#5550,#5545,#2600,.T.);
#7131=EDGE_CURVE('',#5551,#5552,#3662,.T.);
#7132=EDGE_CURVE('',#5552,#5546,#2601,.T.);
#7133=EDGE_CURVE('',#5545,#5551,#2602,.T.);
#7134=EDGE_CURVE('',#5553,#5554,#3663,.T.);
#7135=EDGE_CURVE('',#5554,#5552,#2603,.T.);
#7136=EDGE_CURVE('',#5551,#5553,#2604,.T.);
#7137=EDGE_CURVE('',#5555,#5556,#3664,.T.);
#7138=EDGE_CURVE('',#5556,#5554,#2605,.T.);
#7139=EDGE_CURVE('',#5553,#5555,#2606,.T.);
#7140=EDGE_CURVE('',#5557,#5558,#3665,.T.);
#7141=EDGE_CURVE('',#5558,#5556,#2607,.T.);
#7142=EDGE_CURVE('',#5555,#5557,#2608,.T.);
#7143=EDGE_CURVE('',#5559,#5560,#3666,.T.);
#7144=EDGE_CURVE('',#5560,#5558,#2609,.T.);
#7145=EDGE_CURVE('',#5557,#5559,#2610,.T.);
#7146=EDGE_CURVE('',#5561,#5562,#3667,.T.);
#7147=EDGE_CURVE('',#5562,#5560,#2611,.T.);
#7148=EDGE_CURVE('',#5559,#5561,#2612,.T.);
#7149=EDGE_CURVE('',#5563,#5564,#3668,.T.);
#7150=EDGE_CURVE('',#5564,#5562,#2613,.T.);
#7151=EDGE_CURVE('',#5561,#5563,#2614,.T.);
#7152=EDGE_CURVE('',#5565,#5566,#3669,.T.);
#7153=EDGE_CURVE('',#5565,#5567,#2615,.T.);
#7154=EDGE_CURVE('',#5568,#5567,#2196,.F.);
#7155=EDGE_CURVE('',#5568,#5566,#2616,.T.);
#7156=EDGE_CURVE('',#5569,#5570,#3670,.T.);
#7157=EDGE_CURVE('',#5570,#5571,#2617,.T.);
#7158=EDGE_CURVE('',#5572,#5571,#2197,.T.);
#7159=EDGE_CURVE('',#5569,#5572,#2618,.T.);
#7160=EDGE_CURVE('',#5573,#5574,#3671,.T.);
#7161=EDGE_CURVE('',#5574,#5570,#2619,.T.);
#7162=EDGE_CURVE('',#5573,#5569,#2620,.T.);
#7163=EDGE_CURVE('',#5575,#5576,#3672,.T.);
#7164=EDGE_CURVE('',#5576,#5574,#2621,.T.);
#7165=EDGE_CURVE('',#5575,#5573,#2622,.T.);
#7166=EDGE_CURVE('',#5577,#5578,#3673,.T.);
#7167=EDGE_CURVE('',#5578,#5576,#2623,.T.);
#7168=EDGE_CURVE('',#5577,#5575,#2624,.T.);
#7169=EDGE_CURVE('',#5579,#5580,#3674,.T.);
#7170=EDGE_CURVE('',#5580,#5578,#2625,.T.);
#7171=EDGE_CURVE('',#5579,#5577,#2626,.T.);
#7172=EDGE_CURVE('',#5581,#5582,#3675,.T.);
#7173=EDGE_CURVE('',#5582,#5580,#2627,.T.);
#7174=EDGE_CURVE('',#5581,#5579,#2628,.T.);
#7175=EDGE_CURVE('',#5583,#5584,#3676,.T.);
#7176=EDGE_CURVE('',#5584,#5582,#2629,.T.);
#7177=EDGE_CURVE('',#5583,#5581,#2630,.T.);
#7178=EDGE_CURVE('',#5585,#5586,#3677,.T.);
#7179=EDGE_CURVE('',#5586,#5584,#2631,.T.);
#7180=EDGE_CURVE('',#5585,#5583,#2632,.T.);
#7181=EDGE_CURVE('',#5587,#5588,#3678,.T.);
#7182=EDGE_CURVE('',#5589,#5587,#2633,.T.);
#7183=EDGE_CURVE('',#5590,#5589,#2198,.T.);
#7184=EDGE_CURVE('',#5590,#5588,#2634,.T.);
#7185=EDGE_CURVE('',#5591,#5591,#2199,.T.);
#7186=EDGE_CURVE('',#5591,#5592,#3679,.T.);
#7187=EDGE_CURVE('',#5592,#5592,#2200,.T.);
#7188=EDGE_CURVE('',#5593,#5593,#2201,.T.);
#7189=EDGE_CURVE('',#5594,#5594,#2202,.T.);
#7190=EDGE_CURVE('',#5594,#5595,#3680,.T.);
#7191=EDGE_CURVE('',#5595,#5595,#2203,.T.);
#7192=EDGE_CURVE('',#5596,#5596,#2204,.T.);
#7193=EDGE_CURVE('',#5597,#5597,#2205,.T.);
#7194=EDGE_CURVE('',#5597,#5598,#3681,.T.);
#7195=EDGE_CURVE('',#5598,#5598,#2206,.T.);
#7196=EDGE_CURVE('',#5599,#5599,#2207,.T.);
#7197=EDGE_CURVE('',#5600,#5600,#2208,.T.);
#7198=EDGE_CURVE('',#5600,#5601,#3682,.T.);
#7199=EDGE_CURVE('',#5601,#5601,#2209,.T.);
#7200=EDGE_CURVE('',#5602,#5602,#2210,.T.);
#7201=EDGE_CURVE('',#5593,#5603,#3683,.T.);
#7202=EDGE_CURVE('',#5603,#5603,#2211,.T.);
#7203=EDGE_CURVE('',#5596,#5604,#3684,.T.);
#7204=EDGE_CURVE('',#5604,#5604,#2212,.T.);
#7205=EDGE_CURVE('',#5599,#5605,#3685,.T.);
#7206=EDGE_CURVE('',#5605,#5605,#2213,.T.);
#7207=EDGE_CURVE('',#5602,#5606,#3686,.T.);
#7208=EDGE_CURVE('',#5606,#5606,#2214,.T.);
#7209=EDGE_CURVE('',#5547,#5572,#2635,.T.);
#7210=EDGE_CURVE('',#5571,#5550,#2636,.T.);
#7211=EDGE_CURVE('',#5588,#5586,#2637,.T.);
#7212=EDGE_CURVE('',#5587,#5585,#2638,.T.);
#7213=EDGE_CURVE('',#5567,#5590,#2639,.T.);
#7214=EDGE_CURVE('',#5563,#5565,#2640,.T.);
#7215=EDGE_CURVE('',#5566,#5564,#2641,.T.);
#7216=EDGE_CURVE('',#5589,#5568,#2642,.T.);
#7217=EDGE_CURVE('',#5501,#5526,#2643,.T.);
#7218=EDGE_CURVE('',#5525,#5504,#2644,.T.);
#7219=EDGE_CURVE('',#5542,#5540,#2645,.T.);
#7220=EDGE_CURVE('',#5541,#5539,#2646,.T.);
#7221=EDGE_CURVE('',#5521,#5544,#2647,.T.);
#7222=EDGE_CURVE('',#5517,#5519,#2648,.T.);
#7223=EDGE_CURVE('',#5520,#5518,#2649,.T.);
#7224=EDGE_CURVE('',#5543,#5522,#2650,.T.);
#7225=EDGE_CURVE('',#5455,#5480,#2651,.T.);
#7226=EDGE_CURVE('',#5479,#5458,#2652,.T.);
#7227=EDGE_CURVE('',#5496,#5494,#2653,.T.);
#7228=EDGE_CURVE('',#5495,#5493,#2654,.T.);
#7229=EDGE_CURVE('',#5475,#5498,#2655,.T.);
#7230=EDGE_CURVE('',#5471,#5473,#2656,.T.);
#7231=EDGE_CURVE('',#5474,#5472,#2657,.T.);
#7232=EDGE_CURVE('',#5497,#5476,#2658,.T.);
#7233=EDGE_CURVE('',#5409,#5434,#2659,.T.);
#7234=EDGE_CURVE('',#5433,#5412,#2660,.T.);
#7235=EDGE_CURVE('',#5450,#5448,#2661,.T.);
#7236=EDGE_CURVE('',#5449,#5447,#2662,.T.);
#7237=EDGE_CURVE('',#5429,#5452,#2663,.T.);
#7238=EDGE_CURVE('',#5425,#5427,#2664,.T.);
#7239=EDGE_CURVE('',#5428,#5426,#2665,.T.);
#7240=EDGE_CURVE('',#5451,#5430,#2666,.T.);
#7241=EDGE_CURVE('',#5363,#5388,#2667,.T.);
#7242=EDGE_CURVE('',#5387,#5366,#2668,.T.);
#7243=EDGE_CURVE('',#5404,#5402,#2669,.T.);
#7244=EDGE_CURVE('',#5403,#5401,#2670,.T.);
#7245=EDGE_CURVE('',#5383,#5406,#2671,.T.);
#7246=EDGE_CURVE('',#5379,#5381,#2672,.T.);
#7247=EDGE_CURVE('',#5382,#5380,#2673,.T.);
#7248=EDGE_CURVE('',#5405,#5384,#2674,.T.);
#7249=EDGE_CURVE('',#5317,#5342,#2675,.T.);
#7250=EDGE_CURVE('',#5341,#5320,#2676,.T.);
#7251=EDGE_CURVE('',#5358,#5356,#2677,.T.);
#7252=EDGE_CURVE('',#5357,#5355,#2678,.T.);
#7253=EDGE_CURVE('',#5337,#5360,#2679,.T.);
#7254=EDGE_CURVE('',#5333,#5335,#2680,.T.);
#7255=EDGE_CURVE('',#5336,#5334,#2681,.T.);
#7256=EDGE_CURVE('',#5359,#5338,#2682,.T.);
#7257=EDGE_CURVE('',#5271,#5296,#2683,.T.);
#7258=EDGE_CURVE('',#5295,#5274,#2684,.T.);
#7259=EDGE_CURVE('',#5312,#5310,#2685,.T.);
#7260=EDGE_CURVE('',#5311,#5309,#2686,.T.);
#7261=EDGE_CURVE('',#5291,#5314,#2687,.T.);
#7262=EDGE_CURVE('',#5287,#5289,#2688,.T.);
#7263=EDGE_CURVE('',#5290,#5288,#2689,.T.);
#7264=EDGE_CURVE('',#5313,#5292,#2690,.T.);
#7265=EDGE_CURVE('',#5225,#5250,#2691,.T.);
#7266=EDGE_CURVE('',#5249,#5228,#2692,.T.);
#7267=EDGE_CURVE('',#5266,#5264,#2693,.T.);
#7268=EDGE_CURVE('',#5265,#5263,#2694,.T.);
#7269=EDGE_CURVE('',#5245,#5268,#2695,.T.);
#7270=EDGE_CURVE('',#5241,#5243,#2696,.T.);
#7271=EDGE_CURVE('',#5244,#5242,#2697,.T.);
#7272=EDGE_CURVE('',#5267,#5246,#2698,.T.);
#7273=EDGE_CURVE('',#5607,#5608,#3687,.T.);
#7274=EDGE_CURVE('',#5607,#5609,#3688,.T.);
#7275=EDGE_CURVE('',#5610,#5609,#3689,.T.);
#7276=EDGE_CURVE('',#5608,#5610,#3690,.T.);
#7277=EDGE_CURVE('',#5611,#5612,#3691,.T.);
#7278=EDGE_CURVE('',#5610,#5611,#3692,.T.);
#7279=EDGE_CURVE('',#5609,#5613,#3693,.T.);
#7280=EDGE_CURVE('',#5614,#5613,#3694,.T.);
#7281=EDGE_CURVE('',#5615,#5614,#3695,.T.);
#7282=EDGE_CURVE('',#5616,#5615,#3696,.T.);
#7283=EDGE_CURVE('',#5617,#5616,#3697,.T.);
#7284=EDGE_CURVE('',#5618,#5617,#3698,.T.);
#7285=EDGE_CURVE('',#5619,#5618,#3699,.T.);
#7286=EDGE_CURVE('',#5620,#5619,#3700,.T.);
#7287=EDGE_CURVE('',#5612,#5620,#3701,.T.);
#7288=EDGE_CURVE('',#5621,#5622,#3702,.T.);
#7289=EDGE_CURVE('',#5614,#5621,#3703,.T.);
#7290=EDGE_CURVE('',#5613,#5622,#3704,.T.);
#7291=EDGE_CURVE('',#5622,#5607,#2215,.T.);
#7292=EDGE_CURVE('',#5623,#5624,#3705,.T.);
#7293=EDGE_CURVE('',#5625,#5623,#3706,.T.);
#7294=EDGE_CURVE('',#5625,#5626,#3707,.T.);
#7295=EDGE_CURVE('',#5626,#5627,#3708,.T.);
#7296=EDGE_CURVE('',#5628,#5627,#3709,.T.);
#7297=EDGE_CURVE('',#5629,#5628,#3710,.T.);
#7298=EDGE_CURVE('',#5630,#5629,#3711,.T.);
#7299=EDGE_CURVE('',#5631,#5630,#3712,.T.);
#7300=EDGE_CURVE('',#5632,#5631,#3713,.T.);
#7301=EDGE_CURVE('',#5633,#5632,#3714,.T.);
#7302=EDGE_CURVE('',#5634,#5633,#3715,.T.);
#7303=EDGE_CURVE('',#5624,#5634,#3716,.T.);
#7304=EDGE_CURVE('',#5635,#5636,#3717,.T.);
#7305=EDGE_CURVE('',#5635,#5626,#3718,.T.);
#7306=EDGE_CURVE('',#5636,#5625,#3719,.T.);
#7307=EDGE_CURVE('',#5637,#5638,#3720,.T.);
#7308=EDGE_CURVE('',#5628,#5637,#3721,.T.);
#7309=EDGE_CURVE('',#5627,#5638,#3722,.T.);
#7310=EDGE_CURVE('',#5638,#5635,#2216,.T.);
#7311=EDGE_CURVE('',#5639,#5618,#3723,.T.);
#7312=EDGE_CURVE('',#5640,#5639,#3724,.T.);
#7313=EDGE_CURVE('',#5641,#5640,#2217,.T.);
#7314=EDGE_CURVE('',#5642,#5641,#3725,.T.);
#7315=EDGE_CURVE('',#5619,#5642,#3726,.T.);
#7316=EDGE_CURVE('',#5617,#5643,#3727,.T.);
#7317=EDGE_CURVE('',#5643,#5639,#3728,.T.);
#7318=EDGE_CURVE('',#5621,#5644,#2218,.T.);
#7319=EDGE_CURVE('',#5644,#5645,#3729,.T.);
#7320=EDGE_CURVE('',#5645,#5646,#3730,.T.);
#7321=EDGE_CURVE('',#5646,#5647,#3731,.T.);
#7322=EDGE_CURVE('',#5647,#5648,#3732,.T.);
#7323=EDGE_CURVE('',#5648,#5649,#2219,.T.);
#7324=EDGE_CURVE('',#5649,#5650,#3733,.T.);
#7325=EDGE_CURVE('',#5650,#5615,#3734,.T.);
#7326=EDGE_CURVE('',#5611,#5651,#3735,.T.);
#7327=EDGE_CURVE('',#5651,#5652,#3736,.T.);
#7328=EDGE_CURVE('',#5652,#5653,#2220,.T.);
#7329=EDGE_CURVE('',#5653,#5654,#3737,.T.);
#7330=EDGE_CURVE('',#5654,#5655,#3738,.T.);
#7331=EDGE_CURVE('',#5655,#5656,#3739,.T.);
#7332=EDGE_CURVE('',#5656,#5657,#3740,.T.);
#7333=EDGE_CURVE('',#5657,#5608,#2221,.T.);
#7334=EDGE_CURVE('',#5658,#5616,#3741,.T.);
#7335=EDGE_CURVE('',#5643,#5658,#3742,.T.);
#7336=EDGE_CURVE('',#5650,#5658,#3743,.T.);
#7337=EDGE_CURVE('',#5659,#5632,#3744,.T.);
#7338=EDGE_CURVE('',#5660,#5659,#3745,.T.);
#7339=EDGE_CURVE('',#5661,#5660,#2222,.T.);
#7340=EDGE_CURVE('',#5662,#5661,#3746,.T.);
#7341=EDGE_CURVE('',#5633,#5662,#3747,.T.);
#7342=EDGE_CURVE('',#5631,#5663,#3748,.T.);
#7343=EDGE_CURVE('',#5663,#5659,#3749,.T.);
#7344=EDGE_CURVE('',#5664,#5630,#3750,.T.);
#7345=EDGE_CURVE('',#5663,#5664,#3751,.T.);
#7346=EDGE_CURVE('',#5665,#5629,#3752,.T.);
#7347=EDGE_CURVE('',#5665,#5664,#3753,.T.);
#7348=EDGE_CURVE('',#5637,#5666,#2223,.T.);
#7349=EDGE_CURVE('',#5666,#5667,#3754,.T.);
#7350=EDGE_CURVE('',#5667,#5668,#3755,.T.);
#7351=EDGE_CURVE('',#5668,#5669,#3756,.T.);
#7352=EDGE_CURVE('',#5669,#5670,#3757,.T.);
#7353=EDGE_CURVE('',#5670,#5671,#2224,.T.);
#7354=EDGE_CURVE('',#5671,#5665,#3758,.T.);
#7355=EDGE_CURVE('',#5672,#5642,#3759,.T.);
#7356=EDGE_CURVE('',#5672,#5620,#3760,.T.);
#7357=EDGE_CURVE('',#5673,#5672,#3761,.T.);
#7358=EDGE_CURVE('',#5612,#5673,#3762,.T.);
#7359=EDGE_CURVE('',#5674,#5634,#3763,.T.);
#7360=EDGE_CURVE('',#5675,#5674,#3764,.T.);
#7361=EDGE_CURVE('',#5624,#5675,#3765,.T.);
#7362=EDGE_CURVE('',#5674,#5662,#3766,.T.);
#7363=EDGE_CURVE('',#5652,#5641,#3767,.T.);
#7364=EDGE_CURVE('',#5640,#5649,#3768,.T.);
#7365=EDGE_CURVE('',#5648,#5676,#3769,.T.);
#7366=EDGE_CURVE('',#5676,#5677,#2225,.T.);
#7367=EDGE_CURVE('',#5677,#5678,#3770,.T.);
#7368=EDGE_CURVE('',#5679,#5678,#2226,.T.);
#7369=EDGE_CURVE('',#5679,#5661,#3771,.T.);
#7370=EDGE_CURVE('',#5660,#5671,#3772,.T.);
#7371=EDGE_CURVE('',#5670,#5680,#3773,.T.);
#7372=EDGE_CURVE('',#5680,#5681,#2227,.T.);
#7373=EDGE_CURVE('',#5681,#5682,#3774,.T.);
#7374=EDGE_CURVE('',#5682,#5682,#2228,.T.);
#7375=EDGE_CURVE('',#5681,#5683,#2229,.T.);
#7376=EDGE_CURVE('',#5683,#5653,#3775,.T.);
#7377=EDGE_CURVE('',#5651,#5673,#3776,.T.);
#7378=EDGE_CURVE('',#5672,#5642,#3777,.T.);
#7379=EDGE_CURVE('',#5643,#5639,#3778,.T.);
#7380=EDGE_CURVE('',#5663,#5659,#3779,.T.);
#7381=EDGE_CURVE('',#5684,#5679,#3780,.T.);
#7382=EDGE_CURVE('',#5684,#5675,#3781,.T.);
#7383=EDGE_CURVE('',#5674,#5662,#3782,.T.);
#7384=EDGE_CURVE('',#5623,#5684,#3783,.T.);
#7385=EDGE_CURVE('',#5657,#5685,#3784,.T.);
#7386=EDGE_CURVE('',#5656,#5686,#3785,.T.);
#7387=EDGE_CURVE('',#5686,#5685,#3786,.T.);
#7388=EDGE_CURVE('',#5685,#5687,#2230,.T.);
#7389=EDGE_CURVE('',#5688,#5686,#3787,.T.);
#7390=EDGE_CURVE('',#5689,#5688,#3788,.T.);
#7391=EDGE_CURVE('',#5687,#5689,#2231,.T.);
#7392=EDGE_CURVE('',#5690,#5655,#3789,.T.);
#7393=EDGE_CURVE('',#5691,#5690,#3790,.T.);
#7394=EDGE_CURVE('',#5692,#5691,#3791,.T.);
#7395=EDGE_CURVE('',#5693,#5692,#3792,.T.);
#7396=EDGE_CURVE('',#5694,#5693,#3793,.T.);
#7397=EDGE_CURVE('',#5695,#5694,#3794,.T.);
#7398=EDGE_CURVE('',#5668,#5695,#3795,.T.);
#7399=EDGE_CURVE('',#5667,#5688,#3796,.T.);
#7400=EDGE_CURVE('',#5689,#5666,#3797,.T.);
#7401=EDGE_CURVE('',#5696,#5644,#3798,.T.);
#7402=EDGE_CURVE('',#5696,#5697,#3799,.T.);
#7403=EDGE_CURVE('',#5645,#5697,#3800,.T.);
#7404=EDGE_CURVE('',#5646,#5698,#3801,.T.);
#7405=EDGE_CURVE('',#5697,#5699,#3802,.T.);
#7406=EDGE_CURVE('',#5700,#5699,#3803,.T.);
#7407=EDGE_CURVE('',#5701,#5700,#3804,.T.);
#7408=EDGE_CURVE('',#5702,#5701,#3805,.T.);
#7409=EDGE_CURVE('',#5703,#5702,#3806,.T.);
#7410=EDGE_CURVE('',#5704,#5703,#3807,.T.);
#7411=EDGE_CURVE('',#5705,#5704,#3808,.T.);
#7412=EDGE_CURVE('',#5706,#5705,#3809,.T.);
#7413=EDGE_CURVE('',#5698,#5706,#3810,.T.);
#7414=EDGE_CURVE('',#5707,#5708,#3811,.T.);
#7415=EDGE_CURVE('',#5700,#5707,#3812,.T.);
#7416=EDGE_CURVE('',#5699,#5708,#3813,.T.);
#7417=EDGE_CURVE('',#5708,#5696,#2232,.T.);
#7418=EDGE_CURVE('',#5691,#5672,#3814,.T.);
#7419=EDGE_CURVE('',#5642,#5692,#3815,.T.);
#7420=EDGE_CURVE('',#5709,#5690,#3816,.T.);
#7421=EDGE_CURVE('',#5672,#5709,#3817,.T.);
#7422=EDGE_CURVE('',#5654,#5709,#3818,.T.);
#7423=EDGE_CURVE('',#5687,#5710,#3819,.T.);
#7424=EDGE_CURVE('',#5710,#5710,#2233,.T.);
#7425=EDGE_CURVE('',#5707,#5636,#2234,.T.);
#7426=EDGE_CURVE('',#5698,#5711,#3820,.T.);
#7427=EDGE_CURVE('',#5647,#5711,#3821,.T.);
#7428=EDGE_CURVE('',#5643,#5706,#3822,.T.);
#7429=EDGE_CURVE('',#5711,#5643,#3823,.T.);
#7430=EDGE_CURVE('',#5678,#5712,#3824,.T.);
#7431=EDGE_CURVE('',#5712,#5701,#3825,.T.);
#7432=EDGE_CURVE('',#5705,#5639,#3826,.T.);
#7433=EDGE_CURVE('',#5662,#5704,#3827,.T.);
#7434=EDGE_CURVE('',#5677,#5662,#3828,.T.);
#7435=EDGE_CURVE('',#5639,#5676,#3829,.T.);
#7436=EDGE_CURVE('',#5703,#5674,#3830,.T.);
#7437=EDGE_CURVE('',#5683,#5642,#3831,.T.);
#7438=EDGE_CURVE('',#5659,#5680,#3832,.T.);
#7439=EDGE_CURVE('',#5693,#5659,#3833,.T.);
#7440=EDGE_CURVE('',#5663,#5694,#3834,.T.);
#7441=EDGE_CURVE('',#5713,#5663,#3835,.T.);
#7442=EDGE_CURVE('',#5695,#5713,#3836,.T.);
#7443=EDGE_CURVE('',#5714,#5702,#3837,.T.);
#7444=EDGE_CURVE('',#5674,#5714,#3838,.T.);
#7445=EDGE_CURVE('',#5669,#5713,#3839,.T.);
#7446=EDGE_CURVE('',#5712,#5714,#3840,.T.);
#7447=EDGE_CURVE('',#5715,#5715,#2235,.T.);
#7448=EDGE_CURVE('',#5715,#5716,#3841,.T.);
#7449=EDGE_CURVE('',#5716,#5716,#2236,.T.);
#7450=EDGE_CURVE('',#5717,#5718,#3842,.T.);
#7451=EDGE_CURVE('',#5718,#5719,#2699,.T.);
#7452=EDGE_CURVE('',#5719,#5720,#2237,.T.);
#7453=EDGE_CURVE('',#5720,#5721,#3843,.T.);
#7454=EDGE_CURVE('',#5721,#5721,#2238,.F.);
#7455=EDGE_CURVE('',#5720,#5722,#2239,.T.);
#7456=EDGE_CURVE('',#5722,#5717,#2700,.T.);
#7457=EDGE_CURVE('',#5723,#5724,#3844,.T.);
#7458=EDGE_CURVE('',#5724,#5718,#2701,.T.);
#7459=EDGE_CURVE('',#5717,#5723,#2702,.T.);
#7460=EDGE_CURVE('',#5725,#5726,#3845,.T.);
#7461=EDGE_CURVE('',#5726,#5724,#2703,.T.);
#7462=EDGE_CURVE('',#5723,#5725,#2704,.T.);
#7463=EDGE_CURVE('',#5727,#5728,#3846,.T.);
#7464=EDGE_CURVE('',#5728,#5726,#2705,.T.);
#7465=EDGE_CURVE('',#5725,#5727,#2706,.T.);
#7466=EDGE_CURVE('',#5729,#5730,#3847,.T.);
#7467=EDGE_CURVE('',#5730,#5728,#2707,.T.);
#7468=EDGE_CURVE('',#5727,#5729,#2708,.T.);
#7469=EDGE_CURVE('',#5731,#5732,#3848,.T.);
#7470=EDGE_CURVE('',#5732,#5730,#2709,.T.);
#7471=EDGE_CURVE('',#5729,#5731,#2710,.T.);
#7472=EDGE_CURVE('',#5733,#5734,#3849,.T.);
#7473=EDGE_CURVE('',#5733,#5735,#2711,.T.);
#7474=EDGE_CURVE('',#5736,#5735,#2240,.T.);
#7475=EDGE_CURVE('',#5736,#5734,#2712,.T.);
#7476=EDGE_CURVE('',#5737,#5738,#3850,.T.);
#7477=EDGE_CURVE('',#5738,#5739,#2713,.T.);
#7478=EDGE_CURVE('',#5740,#5739,#2241,.T.);
#7479=EDGE_CURVE('',#5737,#5740,#2714,.T.);
#7480=EDGE_CURVE('',#5741,#5742,#3851,.T.);
#7481=EDGE_CURVE('',#5742,#5738,#2715,.T.);
#7482=EDGE_CURVE('',#5741,#5737,#2716,.T.);
#7483=EDGE_CURVE('',#5743,#5744,#3852,.T.);
#7484=EDGE_CURVE('',#5744,#5742,#2717,.T.);
#7485=EDGE_CURVE('',#5743,#5741,#2718,.T.);
#7486=EDGE_CURVE('',#5745,#5746,#3853,.T.);
#7487=EDGE_CURVE('',#5746,#5744,#2719,.T.);
#7488=EDGE_CURVE('',#5745,#5743,#2720,.T.);
#7489=EDGE_CURVE('',#5747,#5748,#3854,.T.);
#7490=EDGE_CURVE('',#5748,#5746,#2721,.T.);
#7491=EDGE_CURVE('',#5747,#5745,#2722,.T.);
#7492=EDGE_CURVE('',#5749,#5750,#3855,.T.);
#7493=EDGE_CURVE('',#5750,#5748,#2723,.T.);
#7494=EDGE_CURVE('',#5749,#5747,#2724,.T.);
#7495=EDGE_CURVE('',#5751,#5752,#3856,.T.);
#7496=EDGE_CURVE('',#5753,#5751,#2725,.T.);
#7497=EDGE_CURVE('',#5754,#5753,#2242,.T.);
#7498=EDGE_CURVE('',#5754,#5752,#2726,.T.);
#7499=EDGE_CURVE('',#5755,#5756,#3857,.T.);
#7500=EDGE_CURVE('',#5756,#5757,#2727,.T.);
#7501=EDGE_CURVE('',#5757,#5758,#2243,.T.);
#7502=EDGE_CURVE('',#5758,#5759,#3858,.T.);
#7503=EDGE_CURVE('',#5759,#5759,#2244,.F.);
#7504=EDGE_CURVE('',#5758,#5760,#2245,.T.);
#7505=EDGE_CURVE('',#5760,#5755,#2728,.T.);
#7506=EDGE_CURVE('',#5761,#5762,#3859,.T.);
#7507=EDGE_CURVE('',#5762,#5756,#2729,.T.);
#7508=EDGE_CURVE('',#5755,#5761,#2730,.T.);
#7509=EDGE_CURVE('',#5763,#5764,#3860,.T.);
#7510=EDGE_CURVE('',#5764,#5762,#2731,.T.);
#7511=EDGE_CURVE('',#5761,#5763,#2732,.T.);
#7512=EDGE_CURVE('',#5765,#5766,#3861,.T.);
#7513=EDGE_CURVE('',#5766,#5764,#2733,.T.);
#7514=EDGE_CURVE('',#5763,#5765,#2734,.T.);
#7515=EDGE_CURVE('',#5767,#5768,#3862,.T.);
#7516=EDGE_CURVE('',#5768,#5766,#2735,.T.);
#7517=EDGE_CURVE('',#5765,#5767,#2736,.T.);
#7518=EDGE_CURVE('',#5769,#5770,#3863,.T.);
#7519=EDGE_CURVE('',#5770,#5768,#2737,.T.);
#7520=EDGE_CURVE('',#5767,#5769,#2738,.T.);
#7521=EDGE_CURVE('',#5771,#5772,#3864,.T.);
#7522=EDGE_CURVE('',#5771,#5773,#2739,.T.);
#7523=EDGE_CURVE('',#5774,#5773,#2246,.T.);
#7524=EDGE_CURVE('',#5774,#5772,#2740,.T.);
#7525=EDGE_CURVE('',#5775,#5776,#3865,.T.);
#7526=EDGE_CURVE('',#5776,#5777,#2741,.T.);
#7527=EDGE_CURVE('',#5778,#5777,#2247,.T.);
#7528=EDGE_CURVE('',#5775,#5778,#2742,.T.);
#7529=EDGE_CURVE('',#5779,#5780,#3866,.T.);
#7530=EDGE_CURVE('',#5780,#5776,#2743,.T.);
#7531=EDGE_CURVE('',#5779,#5775,#2744,.T.);
#7532=EDGE_CURVE('',#5781,#5782,#3867,.T.);
#7533=EDGE_CURVE('',#5782,#5780,#2745,.T.);
#7534=EDGE_CURVE('',#5781,#5779,#2746,.T.);
#7535=EDGE_CURVE('',#5783,#5784,#3868,.T.);
#7536=EDGE_CURVE('',#5784,#5782,#2747,.T.);
#7537=EDGE_CURVE('',#5783,#5781,#2748,.T.);
#7538=EDGE_CURVE('',#5785,#5786,#3869,.T.);
#7539=EDGE_CURVE('',#5786,#5784,#2749,.T.);
#7540=EDGE_CURVE('',#5785,#5783,#2750,.T.);
#7541=EDGE_CURVE('',#5787,#5788,#3870,.T.);
#7542=EDGE_CURVE('',#5788,#5786,#2751,.T.);
#7543=EDGE_CURVE('',#5787,#5785,#2752,.T.);
#7544=EDGE_CURVE('',#5789,#5790,#3871,.T.);
#7545=EDGE_CURVE('',#5791,#5789,#2753,.T.);
#7546=EDGE_CURVE('',#5792,#5791,#2248,.T.);
#7547=EDGE_CURVE('',#5792,#5790,#2754,.T.);
#7548=EDGE_CURVE('',#5793,#5794,#3872,.T.);
#7549=EDGE_CURVE('',#5794,#5795,#2755,.T.);
#7550=EDGE_CURVE('',#5795,#5796,#2249,.T.);
#7551=EDGE_CURVE('',#5796,#5797,#3873,.T.);
#7552=EDGE_CURVE('',#5797,#5797,#2250,.F.);
#7553=EDGE_CURVE('',#5796,#5798,#2251,.T.);
#7554=EDGE_CURVE('',#5798,#5793,#2756,.T.);
#7555=EDGE_CURVE('',#5799,#5800,#3874,.T.);
#7556=EDGE_CURVE('',#5800,#5794,#2757,.T.);
#7557=EDGE_CURVE('',#5793,#5799,#2758,.T.);
#7558=EDGE_CURVE('',#5801,#5802,#3875,.T.);
#7559=EDGE_CURVE('',#5802,#5800,#2759,.T.);
#7560=EDGE_CURVE('',#5799,#5801,#2760,.T.);
#7561=EDGE_CURVE('',#5803,#5804,#3876,.T.);
#7562=EDGE_CURVE('',#5804,#5802,#2761,.T.);
#7563=EDGE_CURVE('',#5801,#5803,#2762,.T.);
#7564=EDGE_CURVE('',#5805,#5806,#3877,.T.);
#7565=EDGE_CURVE('',#5806,#5804,#2763,.T.);
#7566=EDGE_CURVE('',#5803,#5805,#2764,.T.);
#7567=EDGE_CURVE('',#5807,#5808,#3878,.T.);
#7568=EDGE_CURVE('',#5808,#5806,#2765,.T.);
#7569=EDGE_CURVE('',#5805,#5807,#2766,.T.);
#7570=EDGE_CURVE('',#5809,#5810,#3879,.T.);
#7571=EDGE_CURVE('',#5809,#5811,#2767,.T.);
#7572=EDGE_CURVE('',#5812,#5811,#2252,.T.);
#7573=EDGE_CURVE('',#5812,#5810,#2768,.T.);
#7574=EDGE_CURVE('',#5813,#5814,#3880,.T.);
#7575=EDGE_CURVE('',#5814,#5815,#2769,.T.);
#7576=EDGE_CURVE('',#5816,#5815,#2253,.T.);
#7577=EDGE_CURVE('',#5813,#5816,#2770,.T.);
#7578=EDGE_CURVE('',#5817,#5818,#3881,.T.);
#7579=EDGE_CURVE('',#5818,#5814,#2771,.T.);
#7580=EDGE_CURVE('',#5817,#5813,#2772,.T.);
#7581=EDGE_CURVE('',#5819,#5820,#3882,.T.);
#7582=EDGE_CURVE('',#5820,#5818,#2773,.T.);
#7583=EDGE_CURVE('',#5819,#5817,#2774,.T.);
#7584=EDGE_CURVE('',#5821,#5822,#3883,.T.);
#7585=EDGE_CURVE('',#5822,#5820,#2775,.T.);
#7586=EDGE_CURVE('',#5821,#5819,#2776,.T.);
#7587=EDGE_CURVE('',#5823,#5824,#3884,.T.);
#7588=EDGE_CURVE('',#5824,#5822,#2777,.T.);
#7589=EDGE_CURVE('',#5823,#5821,#2778,.T.);
#7590=EDGE_CURVE('',#5825,#5826,#3885,.T.);
#7591=EDGE_CURVE('',#5826,#5824,#2779,.T.);
#7592=EDGE_CURVE('',#5825,#5823,#2780,.T.);
#7593=EDGE_CURVE('',#5827,#5828,#3886,.T.);
#7594=EDGE_CURVE('',#5829,#5827,#2781,.T.);
#7595=EDGE_CURVE('',#5830,#5829,#2254,.T.);
#7596=EDGE_CURVE('',#5830,#5828,#2782,.T.);
#7597=EDGE_CURVE('',#5831,#5832,#3887,.T.);
#7598=EDGE_CURVE('',#5832,#5833,#2783,.T.);
#7599=EDGE_CURVE('',#5833,#5834,#2255,.T.);
#7600=EDGE_CURVE('',#5834,#5835,#3888,.T.);
#7601=EDGE_CURVE('',#5835,#5835,#2256,.F.);
#7602=EDGE_CURVE('',#5834,#5836,#2257,.T.);
#7603=EDGE_CURVE('',#5836,#5831,#2784,.T.);
#7604=EDGE_CURVE('',#5837,#5838,#3889,.T.);
#7605=EDGE_CURVE('',#5838,#5832,#2785,.T.);
#7606=EDGE_CURVE('',#5831,#5837,#2786,.T.);
#7607=EDGE_CURVE('',#5839,#5840,#3890,.T.);
#7608=EDGE_CURVE('',#5840,#5838,#2787,.T.);
#7609=EDGE_CURVE('',#5837,#5839,#2788,.T.);
#7610=EDGE_CURVE('',#5841,#5842,#3891,.T.);
#7611=EDGE_CURVE('',#5842,#5840,#2789,.T.);
#7612=EDGE_CURVE('',#5839,#5841,#2790,.T.);
#7613=EDGE_CURVE('',#5843,#5844,#3892,.T.);
#7614=EDGE_CURVE('',#5844,#5842,#2791,.T.);
#7615=EDGE_CURVE('',#5841,#5843,#2792,.T.);
#7616=EDGE_CURVE('',#5845,#5846,#3893,.T.);
#7617=EDGE_CURVE('',#5846,#5844,#2793,.T.);
#7618=EDGE_CURVE('',#5843,#5845,#2794,.T.);
#7619=EDGE_CURVE('',#5847,#5848,#3894,.T.);
#7620=EDGE_CURVE('',#5847,#5849,#2795,.T.);
#7621=EDGE_CURVE('',#5850,#5849,#2258,.T.);
#7622=EDGE_CURVE('',#5850,#5848,#2796,.T.);
#7623=EDGE_CURVE('',#5851,#5852,#3895,.T.);
#7624=EDGE_CURVE('',#5852,#5853,#2797,.T.);
#7625=EDGE_CURVE('',#5854,#5853,#2259,.T.);
#7626=EDGE_CURVE('',#5851,#5854,#2798,.T.);
#7627=EDGE_CURVE('',#5855,#5856,#3896,.T.);
#7628=EDGE_CURVE('',#5856,#5852,#2799,.T.);
#7629=EDGE_CURVE('',#5855,#5851,#2800,.T.);
#7630=EDGE_CURVE('',#5857,#5858,#3897,.T.);
#7631=EDGE_CURVE('',#5858,#5856,#2801,.T.);
#7632=EDGE_CURVE('',#5857,#5855,#2802,.T.);
#7633=EDGE_CURVE('',#5859,#5860,#3898,.T.);
#7634=EDGE_CURVE('',#5860,#5858,#2803,.T.);
#7635=EDGE_CURVE('',#5859,#5857,#2804,.T.);
#7636=EDGE_CURVE('',#5861,#5862,#3899,.T.);
#7637=EDGE_CURVE('',#5862,#5860,#2805,.T.);
#7638=EDGE_CURVE('',#5861,#5859,#2806,.T.);
#7639=EDGE_CURVE('',#5863,#5864,#3900,.T.);
#7640=EDGE_CURVE('',#5864,#5862,#2807,.T.);
#7641=EDGE_CURVE('',#5863,#5861,#2808,.T.);
#7642=EDGE_CURVE('',#5865,#5866,#3901,.T.);
#7643=EDGE_CURVE('',#5867,#5865,#2809,.T.);
#7644=EDGE_CURVE('',#5868,#5867,#2260,.T.);
#7645=EDGE_CURVE('',#5868,#5866,#2810,.T.);
#7646=EDGE_CURVE('',#5869,#5870,#3902,.T.);
#7647=EDGE_CURVE('',#5870,#5871,#2811,.T.);
#7648=EDGE_CURVE('',#5871,#5872,#2261,.T.);
#7649=EDGE_CURVE('',#5872,#5873,#2812,.T.);
#7650=EDGE_CURVE('',#5873,#5874,#3903,.T.);
#7651=EDGE_CURVE('',#5874,#5874,#2262,.F.);
#7652=EDGE_CURVE('',#5873,#5869,#2813,.T.);
#7653=EDGE_CURVE('',#5875,#5876,#3904,.T.);
#7654=EDGE_CURVE('',#5876,#5870,#2814,.T.);
#7655=EDGE_CURVE('',#5869,#5875,#2815,.T.);
#7656=EDGE_CURVE('',#5877,#5878,#3905,.T.);
#7657=EDGE_CURVE('',#5878,#5876,#2816,.T.);
#7658=EDGE_CURVE('',#5875,#5877,#2817,.T.);
#7659=EDGE_CURVE('',#5879,#5880,#3906,.T.);
#7660=EDGE_CURVE('',#5879,#5881,#2818,.T.);
#7661=EDGE_CURVE('',#5882,#5881,#2263,.F.);
#7662=EDGE_CURVE('',#5882,#5880,#2819,.T.);
#7663=EDGE_CURVE('',#5883,#5884,#3907,.T.);
#7664=EDGE_CURVE('',#5884,#5885,#2820,.T.);
#7665=EDGE_CURVE('',#5886,#5885,#2264,.T.);
#7666=EDGE_CURVE('',#5883,#5886,#2821,.T.);
#7667=EDGE_CURVE('',#5887,#5888,#3908,.T.);
#7668=EDGE_CURVE('',#5888,#5884,#2822,.T.);
#7669=EDGE_CURVE('',#5887,#5883,#2823,.T.);
#7670=EDGE_CURVE('',#5889,#5890,#3909,.T.);
#7671=EDGE_CURVE('',#5890,#5888,#2824,.T.);
#7672=EDGE_CURVE('',#5889,#5887,#2825,.T.);
#7673=EDGE_CURVE('',#5891,#5892,#3910,.T.);
#7674=EDGE_CURVE('',#5892,#5890,#2826,.T.);
#7675=EDGE_CURVE('',#5891,#5889,#2827,.T.);
#7676=EDGE_CURVE('',#5893,#5894,#3911,.T.);
#7677=EDGE_CURVE('',#5895,#5893,#2828,.T.);
#7678=EDGE_CURVE('',#5896,#5895,#2265,.T.);
#7679=EDGE_CURVE('',#5896,#5894,#2829,.T.);
#7680=EDGE_CURVE('',#5897,#5898,#3912,.T.);
#7681=EDGE_CURVE('',#5898,#5899,#2830,.T.);
#7682=EDGE_CURVE('',#5899,#5900,#2266,.T.);
#7683=EDGE_CURVE('',#5900,#5901,#2831,.T.);
#7684=EDGE_CURVE('',#5901,#5902,#3913,.T.);
#7685=EDGE_CURVE('',#5902,#5902,#2267,.F.);
#7686=EDGE_CURVE('',#5901,#5897,#2832,.T.);
#7687=EDGE_CURVE('',#5903,#5904,#3914,.T.);
#7688=EDGE_CURVE('',#5904,#5898,#2833,.T.);
#7689=EDGE_CURVE('',#5897,#5903,#2834,.T.);
#7690=EDGE_CURVE('',#5905,#5906,#3915,.T.);
#7691=EDGE_CURVE('',#5906,#5904,#2835,.T.);
#7692=EDGE_CURVE('',#5903,#5905,#2836,.T.);
#7693=EDGE_CURVE('',#5907,#5908,#3916,.T.);
#7694=EDGE_CURVE('',#5907,#5909,#2837,.T.);
#7695=EDGE_CURVE('',#5910,#5909,#2268,.F.);
#7696=EDGE_CURVE('',#5910,#5908,#2838,.T.);
#7697=EDGE_CURVE('',#5911,#5912,#3917,.T.);
#7698=EDGE_CURVE('',#5912,#5913,#2839,.T.);
#7699=EDGE_CURVE('',#5914,#5913,#2269,.T.);
#7700=EDGE_CURVE('',#5911,#5914,#2840,.T.);
#7701=EDGE_CURVE('',#5915,#5916,#3918,.T.);
#7702=EDGE_CURVE('',#5916,#5912,#2841,.T.);
#7703=EDGE_CURVE('',#5915,#5911,#2842,.T.);
#7704=EDGE_CURVE('',#5917,#5918,#3919,.T.);
#7705=EDGE_CURVE('',#5918,#5916,#2843,.T.);
#7706=EDGE_CURVE('',#5917,#5915,#2844,.T.);
#7707=EDGE_CURVE('',#5919,#5920,#3920,.T.);
#7708=EDGE_CURVE('',#5920,#5918,#2845,.T.);
#7709=EDGE_CURVE('',#5919,#5917,#2846,.T.);
#7710=EDGE_CURVE('',#5921,#5922,#3921,.T.);
#7711=EDGE_CURVE('',#5923,#5921,#2847,.T.);
#7712=EDGE_CURVE('',#5924,#5923,#2270,.T.);
#7713=EDGE_CURVE('',#5924,#5922,#2848,.T.);
#7714=EDGE_CURVE('',#5925,#5926,#3922,.T.);
#7715=EDGE_CURVE('',#5926,#5927,#2849,.T.);
#7716=EDGE_CURVE('',#5927,#5928,#2271,.T.);
#7717=EDGE_CURVE('',#5928,#5929,#2850,.T.);
#7718=EDGE_CURVE('',#5929,#5930,#3923,.T.);
#7719=EDGE_CURVE('',#5930,#5930,#2272,.F.);
#7720=EDGE_CURVE('',#5929,#5925,#2851,.T.);
#7721=EDGE_CURVE('',#5931,#5932,#3924,.T.);
#7722=EDGE_CURVE('',#5932,#5926,#2852,.T.);
#7723=EDGE_CURVE('',#5925,#5931,#2853,.T.);
#7724=EDGE_CURVE('',#5933,#5934,#3925,.T.);
#7725=EDGE_CURVE('',#5934,#5932,#2854,.T.);
#7726=EDGE_CURVE('',#5931,#5933,#2855,.T.);
#7727=EDGE_CURVE('',#5935,#5936,#3926,.T.);
#7728=EDGE_CURVE('',#5935,#5937,#2856,.T.);
#7729=EDGE_CURVE('',#5938,#5937,#2273,.F.);
#7730=EDGE_CURVE('',#5938,#5936,#2857,.T.);
#7731=EDGE_CURVE('',#5939,#5940,#3927,.T.);
#7732=EDGE_CURVE('',#5940,#5941,#2858,.T.);
#7733=EDGE_CURVE('',#5942,#5941,#2274,.T.);
#7734=EDGE_CURVE('',#5939,#5942,#2859,.T.);
#7735=EDGE_CURVE('',#5943,#5944,#3928,.T.);
#7736=EDGE_CURVE('',#5944,#5940,#2860,.T.);
#7737=EDGE_CURVE('',#5943,#5939,#2861,.T.);
#7738=EDGE_CURVE('',#5945,#5946,#3929,.T.);
#7739=EDGE_CURVE('',#5946,#5944,#2862,.T.);
#7740=EDGE_CURVE('',#5945,#5943,#2863,.T.);
#7741=EDGE_CURVE('',#5947,#5948,#3930,.T.);
#7742=EDGE_CURVE('',#5948,#5946,#2864,.T.);
#7743=EDGE_CURVE('',#5947,#5945,#2865,.T.);
#7744=EDGE_CURVE('',#5949,#5950,#3931,.T.);
#7745=EDGE_CURVE('',#5951,#5949,#2866,.T.);
#7746=EDGE_CURVE('',#5952,#5951,#2275,.T.);
#7747=EDGE_CURVE('',#5952,#5950,#2867,.T.);
#7748=EDGE_CURVE('',#5953,#5954,#3932,.T.);
#7749=EDGE_CURVE('',#5954,#5955,#2868,.T.);
#7750=EDGE_CURVE('',#5955,#5956,#2276,.T.);
#7751=EDGE_CURVE('',#5956,#5957,#2869,.T.);
#7752=EDGE_CURVE('',#5957,#5958,#3933,.T.);
#7753=EDGE_CURVE('',#5958,#5958,#2277,.F.);
#7754=EDGE_CURVE('',#5957,#5953,#2870,.T.);
#7755=EDGE_CURVE('',#5959,#5960,#3934,.T.);
#7756=EDGE_CURVE('',#5960,#5954,#2871,.T.);
#7757=EDGE_CURVE('',#5953,#5959,#2872,.T.);
#7758=EDGE_CURVE('',#5961,#5962,#3935,.T.);
#7759=EDGE_CURVE('',#5962,#5960,#2873,.T.);
#7760=EDGE_CURVE('',#5959,#5961,#2874,.T.);
#7761=EDGE_CURVE('',#5963,#5964,#3936,.T.);
#7762=EDGE_CURVE('',#5963,#5965,#2875,.T.);
#7763=EDGE_CURVE('',#5966,#5965,#2278,.F.);
#7764=EDGE_CURVE('',#5966,#5964,#2876,.T.);
#7765=EDGE_CURVE('',#5967,#5968,#3937,.T.);
#7766=EDGE_CURVE('',#5968,#5969,#2877,.T.);
#7767=EDGE_CURVE('',#5970,#5969,#2279,.T.);
#7768=EDGE_CURVE('',#5967,#5970,#2878,.T.);
#7769=EDGE_CURVE('',#5971,#5972,#3938,.T.);
#7770=EDGE_CURVE('',#5972,#5968,#2879,.T.);
#7771=EDGE_CURVE('',#5971,#5967,#2880,.T.);
#7772=EDGE_CURVE('',#5973,#5974,#3939,.T.);
#7773=EDGE_CURVE('',#5974,#5972,#2881,.T.);
#7774=EDGE_CURVE('',#5973,#5971,#2882,.T.);
#7775=EDGE_CURVE('',#5975,#5976,#3940,.T.);
#7776=EDGE_CURVE('',#5976,#5974,#2883,.T.);
#7777=EDGE_CURVE('',#5975,#5973,#2884,.T.);
#7778=EDGE_CURVE('',#5977,#5978,#3941,.T.);
#7779=EDGE_CURVE('',#5979,#5977,#2885,.T.);
#7780=EDGE_CURVE('',#5980,#5979,#2280,.T.);
#7781=EDGE_CURVE('',#5980,#5978,#2886,.T.);
#7782=EDGE_CURVE('',#5955,#5970,#2887,.T.);
#7783=EDGE_CURVE('',#5969,#5956,#2888,.T.);
#7784=EDGE_CURVE('',#5978,#5976,#2889,.T.);
#7785=EDGE_CURVE('',#5977,#5975,#2890,.T.);
#7786=EDGE_CURVE('',#5965,#5980,#2891,.T.);
#7787=EDGE_CURVE('',#5961,#5963,#2892,.T.);
#7788=EDGE_CURVE('',#5964,#5962,#2893,.T.);
#7789=EDGE_CURVE('',#5979,#5966,#2894,.T.);
#7790=EDGE_CURVE('',#5927,#5942,#2895,.T.);
#7791=EDGE_CURVE('',#5941,#5928,#2896,.T.);
#7792=EDGE_CURVE('',#5950,#5948,#2897,.T.);
#7793=EDGE_CURVE('',#5949,#5947,#2898,.T.);
#7794=EDGE_CURVE('',#5937,#5952,#2899,.T.);
#7795=EDGE_CURVE('',#5933,#5935,#2900,.T.);
#7796=EDGE_CURVE('',#5936,#5934,#2901,.T.);
#7797=EDGE_CURVE('',#5951,#5938,#2902,.T.);
#7798=EDGE_CURVE('',#5899,#5914,#2903,.T.);
#7799=EDGE_CURVE('',#5913,#5900,#2904,.T.);
#7800=EDGE_CURVE('',#5922,#5920,#2905,.T.);
#7801=EDGE_CURVE('',#5921,#5919,#2906,.T.);
#7802=EDGE_CURVE('',#5909,#5924,#2907,.T.);
#7803=EDGE_CURVE('',#5905,#5907,#2908,.T.);
#7804=EDGE_CURVE('',#5908,#5906,#2909,.T.);
#7805=EDGE_CURVE('',#5923,#5910,#2910,.T.);
#7806=EDGE_CURVE('',#5871,#5886,#2911,.T.);
#7807=EDGE_CURVE('',#5885,#5872,#2912,.T.);
#7808=EDGE_CURVE('',#5894,#5892,#2913,.T.);
#7809=EDGE_CURVE('',#5893,#5891,#2914,.T.);
#7810=EDGE_CURVE('',#5881,#5896,#2915,.T.);
#7811=EDGE_CURVE('',#5877,#5879,#2916,.T.);
#7812=EDGE_CURVE('',#5880,#5878,#2917,.T.);
#7813=EDGE_CURVE('',#5895,#5882,#2918,.T.);
#7814=EDGE_CURVE('',#5833,#5854,#2919,.T.);
#7815=EDGE_CURVE('',#5853,#5836,#2920,.T.);
#7816=EDGE_CURVE('',#5866,#5864,#2921,.T.);
#7817=EDGE_CURVE('',#5865,#5863,#2922,.T.);
#7818=EDGE_CURVE('',#5849,#5868,#2923,.T.);
#7819=EDGE_CURVE('',#5845,#5847,#2924,.T.);
#7820=EDGE_CURVE('',#5848,#5846,#2925,.T.);
#7821=EDGE_CURVE('',#5867,#5850,#2926,.T.);
#7822=EDGE_CURVE('',#5795,#5816,#2927,.T.);
#7823=EDGE_CURVE('',#5815,#5798,#2928,.T.);
#7824=EDGE_CURVE('',#5828,#5826,#2929,.T.);
#7825=EDGE_CURVE('',#5827,#5825,#2930,.T.);
#7826=EDGE_CURVE('',#5811,#5830,#2931,.T.);
#7827=EDGE_CURVE('',#5807,#5809,#2932,.T.);
#7828=EDGE_CURVE('',#5810,#5808,#2933,.T.);
#7829=EDGE_CURVE('',#5829,#5812,#2934,.T.);
#7830=EDGE_CURVE('',#5757,#5778,#2935,.T.);
#7831=EDGE_CURVE('',#5777,#5760,#2936,.T.);
#7832=EDGE_CURVE('',#5790,#5788,#2937,.T.);
#7833=EDGE_CURVE('',#5789,#5787,#2938,.T.);
#7834=EDGE_CURVE('',#5773,#5792,#2939,.T.);
#7835=EDGE_CURVE('',#5769,#5771,#2940,.T.);
#7836=EDGE_CURVE('',#5772,#5770,#2941,.T.);
#7837=EDGE_CURVE('',#5791,#5774,#2942,.T.);
#7838=EDGE_CURVE('',#5719,#5740,#2943,.T.);
#7839=EDGE_CURVE('',#5739,#5722,#2944,.T.);
#7840=EDGE_CURVE('',#5752,#5750,#2945,.T.);
#7841=EDGE_CURVE('',#5751,#5749,#2946,.T.);
#7842=EDGE_CURVE('',#5735,#5754,#2947,.T.);
#7843=EDGE_CURVE('',#5731,#5733,#2948,.T.);
#7844=EDGE_CURVE('',#5734,#5732,#2949,.T.);
#7845=EDGE_CURVE('',#5753,#5736,#2950,.T.);
#7846=EDGE_CURVE('',#5981,#5981,#2281,.T.);
#7847=EDGE_CURVE('',#5981,#5982,#3942,.T.);
#7848=EDGE_CURVE('',#5982,#5982,#2282,.T.);
#7849=EDGE_CURVE('',#5983,#5983,#2283,.T.);
#7850=EDGE_CURVE('',#5983,#5984,#3943,.T.);
#7851=EDGE_CURVE('',#5984,#5984,#2284,.T.);
#7852=EDGE_CURVE('',#5985,#5985,#2285,.F.);
#7853=EDGE_CURVE('',#5985,#5986,#3944,.T.);
#7854=EDGE_CURVE('',#5986,#5986,#2286,.F.);
#7855=EDGE_CURVE('',#5987,#5988,#3945,.T.);
#7856=EDGE_CURVE('',#5988,#5989,#2951,.T.);
#7857=EDGE_CURVE('',#5990,#5989,#2287,.T.);
#7858=EDGE_CURVE('',#5990,#5987,#2952,.T.);
#7859=EDGE_CURVE('',#5991,#5992,#3946,.T.);
#7860=EDGE_CURVE('',#5992,#5988,#2953,.T.);
#7861=EDGE_CURVE('',#5987,#5991,#2954,.T.);
#7862=EDGE_CURVE('',#5993,#5994,#3947,.T.);
#7863=EDGE_CURVE('',#5994,#5992,#2955,.T.);
#7864=EDGE_CURVE('',#5991,#5993,#2956,.T.);
#7865=EDGE_CURVE('',#5995,#5996,#3948,.T.);
#7866=EDGE_CURVE('',#5996,#5994,#2957,.T.);
#7867=EDGE_CURVE('',#5993,#5995,#2958,.T.);
#7868=EDGE_CURVE('',#5997,#5998,#3949,.T.);
#7869=EDGE_CURVE('',#5998,#5996,#2959,.T.);
#7870=EDGE_CURVE('',#5995,#5997,#2960,.T.);
#7871=EDGE_CURVE('',#5999,#6000,#3950,.T.);
#7872=EDGE_CURVE('',#6000,#5998,#2961,.T.);
#7873=EDGE_CURVE('',#5997,#5999,#2962,.T.);
#7874=EDGE_CURVE('',#6001,#6002,#3951,.T.);
#7875=EDGE_CURVE('',#6002,#6000,#2963,.T.);
#7876=EDGE_CURVE('',#5999,#6001,#2964,.T.);
#7877=EDGE_CURVE('',#6003,#6004,#3952,.T.);
#7878=EDGE_CURVE('',#6004,#6002,#2965,.T.);
#7879=EDGE_CURVE('',#6001,#6003,#2966,.T.);
#7880=EDGE_CURVE('',#6005,#6006,#3953,.T.);
#7881=EDGE_CURVE('',#6006,#6004,#2967,.T.);
#7882=EDGE_CURVE('',#6003,#6005,#2968,.T.);
#7883=EDGE_CURVE('',#6007,#6008,#3954,.T.);
#7884=EDGE_CURVE('',#6008,#6006,#2969,.T.);
#7885=EDGE_CURVE('',#6005,#6007,#2970,.T.);
#7886=EDGE_CURVE('',#6009,#6010,#3955,.T.);
#7887=EDGE_CURVE('',#6010,#6008,#2971,.T.);
#7888=EDGE_CURVE('',#6007,#6009,#2972,.T.);
#7889=EDGE_CURVE('',#6011,#6012,#3956,.T.);
#7890=EDGE_CURVE('',#6012,#6010,#2973,.T.);
#7891=EDGE_CURVE('',#6009,#6011,#2974,.T.);
#7892=EDGE_CURVE('',#6013,#6014,#3957,.T.);
#7893=EDGE_CURVE('',#6014,#6012,#2975,.T.);
#7894=EDGE_CURVE('',#6011,#6013,#2976,.T.);
#7895=EDGE_CURVE('',#6015,#6016,#3958,.T.);
#7896=EDGE_CURVE('',#6016,#6014,#2977,.T.);
#7897=EDGE_CURVE('',#6013,#6015,#2978,.T.);
#7898=EDGE_CURVE('',#6017,#6018,#3959,.T.);
#7899=EDGE_CURVE('',#6018,#6016,#2979,.T.);
#7900=EDGE_CURVE('',#6015,#6017,#2980,.T.);
#7901=EDGE_CURVE('',#6019,#6020,#3960,.T.);
#7902=EDGE_CURVE('',#6020,#6018,#2981,.T.);
#7903=EDGE_CURVE('',#6017,#6019,#2982,.T.);
#7904=EDGE_CURVE('',#6021,#6022,#3961,.T.);
#7905=EDGE_CURVE('',#6022,#6020,#2983,.T.);
#7906=EDGE_CURVE('',#6019,#6021,#2984,.T.);
#7907=EDGE_CURVE('',#6023,#6024,#3962,.T.);
#7908=EDGE_CURVE('',#6024,#6022,#2985,.T.);
#7909=EDGE_CURVE('',#6021,#6023,#2986,.T.);
#7910=EDGE_CURVE('',#6025,#6026,#3963,.T.);
#7911=EDGE_CURVE('',#6026,#6024,#2987,.T.);
#7912=EDGE_CURVE('',#6023,#6025,#2988,.T.);
#7913=EDGE_CURVE('',#6027,#6028,#3964,.T.);
#7914=EDGE_CURVE('',#6028,#6026,#2989,.T.);
#7915=EDGE_CURVE('',#6025,#6027,#2990,.T.);
#7916=EDGE_CURVE('',#6029,#6030,#3965,.T.);
#7917=EDGE_CURVE('',#6030,#6028,#2991,.T.);
#7918=EDGE_CURVE('',#6027,#6029,#2992,.T.);
#7919=EDGE_CURVE('',#6031,#6032,#3966,.T.);
#7920=EDGE_CURVE('',#6032,#6030,#2993,.T.);
#7921=EDGE_CURVE('',#6029,#6031,#2994,.T.);
#7922=EDGE_CURVE('',#6033,#6034,#3967,.T.);
#7923=EDGE_CURVE('',#6034,#6032,#2995,.T.);
#7924=EDGE_CURVE('',#6031,#6033,#2996,.T.);
#7925=EDGE_CURVE('',#6035,#6036,#3968,.T.);
#7926=EDGE_CURVE('',#6036,#6034,#2997,.T.);
#7927=EDGE_CURVE('',#6033,#6035,#2998,.T.);
#7928=EDGE_CURVE('',#6037,#6038,#3969,.T.);
#7929=EDGE_CURVE('',#6038,#6036,#2999,.T.);
#7930=EDGE_CURVE('',#6035,#6037,#3000,.T.);
#7931=EDGE_CURVE('',#6039,#6040,#3970,.T.);
#7932=EDGE_CURVE('',#6040,#6038,#3001,.T.);
#7933=EDGE_CURVE('',#6037,#6039,#3002,.T.);
#7934=EDGE_CURVE('',#6041,#6042,#3971,.T.);
#7935=EDGE_CURVE('',#6042,#6040,#3003,.T.);
#7936=EDGE_CURVE('',#6039,#6041,#3004,.T.);
#7937=EDGE_CURVE('',#6043,#6044,#3972,.T.);
#7938=EDGE_CURVE('',#6043,#6045,#3005,.T.);
#7939=EDGE_CURVE('',#6046,#6045,#2288,.T.);
#7940=EDGE_CURVE('',#6046,#6044,#3006,.T.);
#7941=EDGE_CURVE('',#6047,#6048,#3973,.T.);
#7942=EDGE_CURVE('',#6048,#6049,#3007,.T.);
#7943=EDGE_CURVE('',#6050,#6049,#2289,.T.);
#7944=EDGE_CURVE('',#6047,#6050,#3008,.T.);
#7945=EDGE_CURVE('',#6051,#6052,#3974,.T.);
#7946=EDGE_CURVE('',#6052,#6048,#3009,.T.);
#7947=EDGE_CURVE('',#6051,#6047,#3010,.T.);
#7948=EDGE_CURVE('',#6053,#6054,#3975,.T.);
#7949=EDGE_CURVE('',#6054,#6052,#3011,.T.);
#7950=EDGE_CURVE('',#6053,#6051,#3012,.T.);
#7951=EDGE_CURVE('',#6055,#6056,#3976,.T.);
#7952=EDGE_CURVE('',#6056,#6054,#3013,.T.);
#7953=EDGE_CURVE('',#6055,#6053,#3014,.T.);
#7954=EDGE_CURVE('',#6057,#6058,#3977,.T.);
#7955=EDGE_CURVE('',#6058,#6056,#3015,.T.);
#7956=EDGE_CURVE('',#6057,#6055,#3016,.T.);
#7957=EDGE_CURVE('',#6059,#6060,#3978,.T.);
#7958=EDGE_CURVE('',#6060,#6058,#3017,.T.);
#7959=EDGE_CURVE('',#6059,#6057,#3018,.T.);
#7960=EDGE_CURVE('',#6061,#6062,#3979,.T.);
#7961=EDGE_CURVE('',#6062,#6060,#3019,.T.);
#7962=EDGE_CURVE('',#6061,#6059,#3020,.T.);
#7963=EDGE_CURVE('',#6063,#6064,#3980,.T.);
#7964=EDGE_CURVE('',#6064,#6062,#3021,.T.);
#7965=EDGE_CURVE('',#6063,#6061,#3022,.T.);
#7966=EDGE_CURVE('',#6065,#6066,#3981,.T.);
#7967=EDGE_CURVE('',#6066,#6064,#3023,.T.);
#7968=EDGE_CURVE('',#6065,#6063,#3024,.T.);
#7969=EDGE_CURVE('',#6067,#6068,#3982,.T.);
#7970=EDGE_CURVE('',#6068,#6066,#3025,.T.);
#7971=EDGE_CURVE('',#6067,#6065,#3026,.T.);
#7972=EDGE_CURVE('',#6069,#6070,#3983,.T.);
#7973=EDGE_CURVE('',#6070,#6068,#3027,.T.);
#7974=EDGE_CURVE('',#6069,#6067,#3028,.T.);
#7975=EDGE_CURVE('',#6071,#6072,#3984,.T.);
#7976=EDGE_CURVE('',#6072,#6070,#3029,.T.);
#7977=EDGE_CURVE('',#6071,#6069,#3030,.T.);
#7978=EDGE_CURVE('',#6073,#6074,#3985,.T.);
#7979=EDGE_CURVE('',#6074,#6072,#3031,.T.);
#7980=EDGE_CURVE('',#6073,#6071,#3032,.T.);
#7981=EDGE_CURVE('',#6075,#6076,#3986,.T.);
#7982=EDGE_CURVE('',#6076,#6074,#3033,.T.);
#7983=EDGE_CURVE('',#6075,#6073,#3034,.T.);
#7984=EDGE_CURVE('',#6077,#6078,#3987,.T.);
#7985=EDGE_CURVE('',#6078,#6076,#3035,.T.);
#7986=EDGE_CURVE('',#6077,#6075,#3036,.T.);
#7987=EDGE_CURVE('',#6079,#6080,#3988,.T.);
#7988=EDGE_CURVE('',#6080,#6078,#3037,.T.);
#7989=EDGE_CURVE('',#6079,#6077,#3038,.T.);
#7990=EDGE_CURVE('',#6081,#6082,#3989,.T.);
#7991=EDGE_CURVE('',#6082,#6080,#3039,.T.);
#7992=EDGE_CURVE('',#6081,#6079,#3040,.T.);
#7993=EDGE_CURVE('',#6083,#6084,#3990,.T.);
#7994=EDGE_CURVE('',#6084,#6082,#3041,.T.);
#7995=EDGE_CURVE('',#6083,#6081,#3042,.T.);
#7996=EDGE_CURVE('',#6085,#6086,#3991,.T.);
#7997=EDGE_CURVE('',#6086,#6084,#3043,.T.);
#7998=EDGE_CURVE('',#6085,#6083,#3044,.T.);
#7999=EDGE_CURVE('',#6087,#6088,#3992,.T.);
#8000=EDGE_CURVE('',#6088,#6086,#3045,.T.);
#8001=EDGE_CURVE('',#6087,#6085,#3046,.T.);
#8002=EDGE_CURVE('',#6089,#6090,#3993,.T.);
#8003=EDGE_CURVE('',#6090,#6088,#3047,.T.);
#8004=EDGE_CURVE('',#6089,#6087,#3048,.T.);
#8005=EDGE_CURVE('',#6091,#6092,#3994,.T.);
#8006=EDGE_CURVE('',#6092,#6090,#3049,.T.);
#8007=EDGE_CURVE('',#6091,#6089,#3050,.T.);
#8008=EDGE_CURVE('',#6093,#6094,#3995,.T.);
#8009=EDGE_CURVE('',#6094,#6092,#3051,.T.);
#8010=EDGE_CURVE('',#6093,#6091,#3052,.T.);
#8011=EDGE_CURVE('',#6095,#6096,#3996,.T.);
#8012=EDGE_CURVE('',#6096,#6094,#3053,.T.);
#8013=EDGE_CURVE('',#6095,#6093,#3054,.T.);
#8014=EDGE_CURVE('',#6097,#6098,#3997,.T.);
#8015=EDGE_CURVE('',#6098,#6096,#3055,.T.);
#8016=EDGE_CURVE('',#6097,#6095,#3056,.T.);
#8017=EDGE_CURVE('',#6099,#6100,#3998,.T.);
#8018=EDGE_CURVE('',#6100,#6098,#3057,.T.);
#8019=EDGE_CURVE('',#6099,#6097,#3058,.T.);
#8020=EDGE_CURVE('',#6101,#6102,#3999,.T.);
#8021=EDGE_CURVE('',#6102,#6100,#3059,.T.);
#8022=EDGE_CURVE('',#6101,#6099,#3060,.T.);
#8023=EDGE_CURVE('',#6103,#6104,#4000,.T.);
#8024=EDGE_CURVE('',#6104,#6102,#3061,.T.);
#8025=EDGE_CURVE('',#6103,#6101,#3062,.T.);
#8026=EDGE_CURVE('',#6105,#6106,#4001,.T.);
#8027=EDGE_CURVE('',#6107,#6105,#3063,.T.);
#8028=EDGE_CURVE('',#6108,#6107,#2290,.T.);
#8029=EDGE_CURVE('',#6108,#6106,#3064,.T.);
#8030=EDGE_CURVE('',#6106,#6104,#3065,.T.);
#8031=EDGE_CURVE('',#6105,#6103,#3066,.T.);
#8032=EDGE_CURVE('',#6049,#5990,#3067,.T.);
#8033=EDGE_CURVE('',#6045,#6108,#3068,.T.);
#8034=EDGE_CURVE('',#6041,#6043,#3069,.T.);
#8035=EDGE_CURVE('',#5989,#6050,#3070,.T.);
#8036=EDGE_CURVE('',#6044,#6042,#3071,.T.);
#8037=EDGE_CURVE('',#6107,#6046,#3072,.T.);
#8038=EDGE_CURVE('',#6109,#6110,#4002,.T.);
#8039=EDGE_CURVE('',#6110,#6111,#4003,.T.);
#8040=EDGE_CURVE('',#6112,#6111,#4004,.T.);
#8041=EDGE_CURVE('',#6112,#6113,#4005,.T.);
#8042=EDGE_CURVE('',#6114,#6113,#4006,.T.);
#8043=EDGE_CURVE('',#6115,#6114,#4007,.T.);
#8044=EDGE_CURVE('',#6116,#6115,#4008,.T.);
#8045=EDGE_CURVE('',#6109,#6116,#4009,.T.);
#8046=EDGE_CURVE('',#6117,#6118,#4010,.T.);
#8047=EDGE_CURVE('',#6117,#6119,#4011,.T.);
#8048=EDGE_CURVE('',#6120,#6119,#4012,.T.);
#8049=EDGE_CURVE('',#6118,#6120,#4013,.T.);
#8050=EDGE_CURVE('',#6121,#6122,#4014,.T.);
#8051=EDGE_CURVE('',#6122,#6120,#4015,.T.);
#8052=EDGE_CURVE('',#6119,#6121,#4016,.T.);
#8053=EDGE_CURVE('',#6118,#6114,#4017,.T.);
#8054=EDGE_CURVE('',#6113,#6117,#4018,.T.);
#8055=EDGE_CURVE('',#6123,#6112,#4019,.T.);
#8056=EDGE_CURVE('',#6123,#6121,#4020,.T.);
#8057=EDGE_CURVE('',#6115,#6124,#4021,.T.);
#8058=EDGE_CURVE('',#6124,#6122,#4022,.T.);
#8059=EDGE_CURVE('',#6111,#6125,#4023,.T.);
#8060=EDGE_CURVE('',#6125,#6123,#4024,.T.);
#8061=EDGE_CURVE('',#6124,#6126,#4025,.T.);
#8062=EDGE_CURVE('',#6126,#6116,#4026,.T.);
#8063=EDGE_CURVE('',#6110,#6127,#4027,.T.);
#8064=EDGE_CURVE('',#6127,#6125,#4028,.T.);
#8065=EDGE_CURVE('',#6128,#6109,#4029,.T.);
#8066=EDGE_CURVE('',#6128,#6126,#4030,.T.);
#8067=EDGE_CURVE('',#6127,#6128,#4031,.T.);
#8068=EDGE_CURVE('',#6129,#6129,#2291,.T.);
#8069=EDGE_CURVE('',#6129,#6130,#4032,.T.);
#8070=EDGE_CURVE('',#6130,#6130,#2292,.T.);
#8071=EDGE_CURVE('',#6131,#6131,#2293,.T.);
#8072=EDGE_CURVE('',#6131,#6132,#4033,.T.);
#8073=EDGE_CURVE('',#6132,#6132,#2294,.T.);
#8074=EDGE_CURVE('',#6133,#6134,#4034,.T.);
#8075=EDGE_CURVE('',#6135,#6133,#2295,.T.);
#8076=EDGE_CURVE('',#6136,#6135,#4035,.T.);
#8077=EDGE_CURVE('',#6136,#6134,#2296,.T.);
#8078=EDGE_CURVE('',#6137,#6138,#4036,.T.);
#8079=EDGE_CURVE('',#6137,#6139,#2297,.T.);
#8080=EDGE_CURVE('',#6140,#6139,#4037,.T.);
#8081=EDGE_CURVE('',#6138,#6140,#2298,.T.);
#8082=EDGE_CURVE('',#6136,#6141,#4038,.T.);
#8083=EDGE_CURVE('',#6142,#6141,#4039,.T.);
#8084=EDGE_CURVE('',#6142,#6143,#4040,.T.);
#8085=EDGE_CURVE('',#6144,#6143,#4041,.T.);
#8086=EDGE_CURVE('',#6145,#6144,#4042,.T.);
#8087=EDGE_CURVE('',#6145,#6146,#4043,.T.);
#8088=EDGE_CURVE('',#6146,#6147,#4044,.T.);
#8089=EDGE_CURVE('',#6147,#6148,#4045,.T.);
#8090=EDGE_CURVE('',#6148,#6139,#4046,.T.);
#8091=EDGE_CURVE('',#6134,#6137,#4047,.T.);
#8092=EDGE_CURVE('',#6149,#6149,#2299,.T.);
#8093=EDGE_CURVE('',#6133,#6150,#4048,.T.);
#8094=EDGE_CURVE('',#6150,#6151,#4049,.T.);
#8095=EDGE_CURVE('',#6152,#6151,#4050,.T.);
#8096=EDGE_CURVE('',#6152,#6153,#4051,.T.);
#8097=EDGE_CURVE('',#6153,#6154,#4052,.T.);
#8098=EDGE_CURVE('',#6154,#6155,#4053,.T.);
#8099=EDGE_CURVE('',#6155,#6135,#4054,.T.);
#8100=EDGE_CURVE('',#6140,#6156,#4055,.T.);
#8101=EDGE_CURVE('',#6156,#6157,#4056,.T.);
#8102=EDGE_CURVE('',#6157,#6158,#4057,.T.);
#8103=EDGE_CURVE('',#6158,#6159,#4058,.T.);
#8104=EDGE_CURVE('',#6160,#6159,#4059,.T.);
#8105=EDGE_CURVE('',#6161,#6160,#4060,.T.);
#8106=EDGE_CURVE('',#6161,#6138,#4061,.T.);
#8107=EDGE_CURVE('',#6141,#6155,#4062,.T.);
#8108=EDGE_CURVE('',#6162,#6163,#4063,.T.);
#8109=EDGE_CURVE('',#6163,#6162,#2300,.T.);
#8110=EDGE_CURVE('',#6164,#6164,#2301,.T.);
#8111=EDGE_CURVE('',#6165,#6162,#4064,.T.);
#8112=EDGE_CURVE('',#6166,#6165,#2302,.T.);
#8113=EDGE_CURVE('',#6163,#6166,#4065,.T.);
#8114=EDGE_CURVE('',#6167,#6161,#4066,.T.);
#8115=EDGE_CURVE('',#6165,#6167,#4067,.T.);
#8116=EDGE_CURVE('',#6168,#6166,#4068,.T.);
#8117=EDGE_CURVE('',#6150,#6168,#4069,.T.);
#8118=EDGE_CURVE('',#6164,#6149,#4070,.T.);
#8119=EDGE_CURVE('',#6143,#6153,#4071,.T.);
#8120=EDGE_CURVE('',#6154,#6142,#4072,.T.);
#8121=EDGE_CURVE('',#6147,#6157,#4073,.T.);
#8122=EDGE_CURVE('',#6156,#6148,#4074,.T.);
#8123=EDGE_CURVE('',#6158,#6146,#4075,.T.);
#8124=EDGE_CURVE('',#6144,#6152,#4076,.T.);
#8125=EDGE_CURVE('',#6159,#6145,#4077,.T.);
#8126=EDGE_CURVE('',#6169,#6160,#4078,.T.);
#8127=EDGE_CURVE('',#6167,#6169,#4079,.T.);
#8128=EDGE_CURVE('',#6170,#6169,#4080,.T.);
#8129=EDGE_CURVE('',#6168,#6170,#4081,.T.);
#8130=EDGE_CURVE('',#6151,#6170,#4082,.T.);
#8131=EDGE_CURVE('',#6171,#6172,#4083,.T.);
#8132=EDGE_CURVE('',#6171,#6173,#3073,.T.);
#8133=EDGE_CURVE('',#6173,#6174,#2303,.F.);
#8134=EDGE_CURVE('',#6174,#6172,#3074,.T.);
#8135=EDGE_CURVE('',#6175,#6176,#4084,.T.);
#8136=EDGE_CURVE('',#6175,#6171,#3075,.T.);
#8137=EDGE_CURVE('',#6172,#6176,#3076,.T.);
#8138=EDGE_CURVE('',#6177,#6178,#4085,.T.);
#8139=EDGE_CURVE('',#6177,#6175,#3077,.T.);
#8140=EDGE_CURVE('',#6176,#6178,#3078,.T.);
#8141=EDGE_CURVE('',#6179,#6180,#4086,.T.);
#8142=EDGE_CURVE('',#6179,#6177,#3079,.T.);
#8143=EDGE_CURVE('',#6178,#6180,#3080,.T.);
#8144=EDGE_CURVE('',#6181,#6182,#4087,.T.);
#8145=EDGE_CURVE('',#6181,#6179,#3081,.T.);
#8146=EDGE_CURVE('',#6180,#6182,#3082,.T.);
#8147=EDGE_CURVE('',#6183,#6184,#4088,.T.);
#8148=EDGE_CURVE('',#6183,#6181,#3083,.T.);
#8149=EDGE_CURVE('',#6182,#6184,#3084,.T.);
#8150=EDGE_CURVE('',#6185,#6186,#4089,.T.);
#8151=EDGE_CURVE('',#6185,#6183,#3085,.T.);
#8152=EDGE_CURVE('',#6184,#6186,#3086,.T.);
#8153=EDGE_CURVE('',#6187,#6188,#4090,.T.);
#8154=EDGE_CURVE('',#6187,#6185,#3087,.T.);
#8155=EDGE_CURVE('',#6186,#6188,#3088,.T.);
#8156=EDGE_CURVE('',#6189,#6190,#4091,.T.);
#8157=EDGE_CURVE('',#6189,#6187,#3089,.T.);
#8158=EDGE_CURVE('',#6188,#6190,#3090,.T.);
#8159=EDGE_CURVE('',#6191,#6192,#4092,.T.);
#8160=EDGE_CURVE('',#6191,#6189,#3091,.T.);
#8161=EDGE_CURVE('',#6190,#6192,#3092,.T.);
#8162=EDGE_CURVE('',#6193,#6194,#4093,.T.);
#8163=EDGE_CURVE('',#6193,#6191,#3093,.T.);
#8164=EDGE_CURVE('',#6192,#6194,#3094,.T.);
#8165=EDGE_CURVE('',#6195,#6196,#4094,.T.);
#8166=EDGE_CURVE('',#6195,#6193,#3095,.T.);
#8167=EDGE_CURVE('',#6194,#6196,#3096,.T.);
#8168=EDGE_CURVE('',#6197,#6198,#4095,.T.);
#8169=EDGE_CURVE('',#6197,#6195,#3097,.T.);
#8170=EDGE_CURVE('',#6196,#6198,#3098,.T.);
#8171=EDGE_CURVE('',#6199,#6200,#4096,.T.);
#8172=EDGE_CURVE('',#6199,#6197,#3099,.T.);
#8173=EDGE_CURVE('',#6198,#6200,#3100,.T.);
#8174=EDGE_CURVE('',#6201,#6202,#4097,.T.);
#8175=EDGE_CURVE('',#6201,#6199,#3101,.T.);
#8176=EDGE_CURVE('',#6200,#6202,#3102,.T.);
#8177=EDGE_CURVE('',#6203,#6204,#4098,.T.);
#8178=EDGE_CURVE('',#6203,#6201,#3103,.T.);
#8179=EDGE_CURVE('',#6202,#6204,#3104,.T.);
#8180=EDGE_CURVE('',#6205,#6206,#4099,.T.);
#8181=EDGE_CURVE('',#6205,#6203,#3105,.T.);
#8182=EDGE_CURVE('',#6204,#6206,#3106,.T.);
#8183=EDGE_CURVE('',#6207,#6208,#4100,.T.);
#8184=EDGE_CURVE('',#6207,#6205,#3107,.T.);
#8185=EDGE_CURVE('',#6206,#6208,#3108,.T.);
#8186=EDGE_CURVE('',#6209,#6210,#4101,.T.);
#8187=EDGE_CURVE('',#6209,#6207,#3109,.T.);
#8188=EDGE_CURVE('',#6208,#6210,#3110,.T.);
#8189=EDGE_CURVE('',#6211,#6212,#4102,.T.);
#8190=EDGE_CURVE('',#6211,#6209,#3111,.T.);
#8191=EDGE_CURVE('',#6210,#6212,#3112,.T.);
#8192=EDGE_CURVE('',#6213,#6214,#4103,.T.);
#8193=EDGE_CURVE('',#6213,#6211,#3113,.T.);
#8194=EDGE_CURVE('',#6212,#6214,#3114,.T.);
#8195=EDGE_CURVE('',#6215,#6216,#4104,.T.);
#8196=EDGE_CURVE('',#6215,#6213,#3115,.T.);
#8197=EDGE_CURVE('',#6214,#6216,#3116,.T.);
#8198=EDGE_CURVE('',#6217,#6218,#4105,.T.);
#8199=EDGE_CURVE('',#6217,#6215,#3117,.T.);
#8200=EDGE_CURVE('',#6216,#6218,#3118,.T.);
#8201=EDGE_CURVE('',#6219,#6220,#4106,.T.);
#8202=EDGE_CURVE('',#6219,#6217,#3119,.T.);
#8203=EDGE_CURVE('',#6218,#6220,#3120,.T.);
#8204=EDGE_CURVE('',#6221,#6222,#4107,.T.);
#8205=EDGE_CURVE('',#6221,#6219,#3121,.T.);
#8206=EDGE_CURVE('',#6220,#6222,#3122,.T.);
#8207=EDGE_CURVE('',#6223,#6224,#4108,.T.);
#8208=EDGE_CURVE('',#6223,#6221,#3123,.T.);
#8209=EDGE_CURVE('',#6222,#6224,#3124,.T.);
#8210=EDGE_CURVE('',#6225,#6226,#4109,.T.);
#8211=EDGE_CURVE('',#6225,#6223,#3125,.T.);
#8212=EDGE_CURVE('',#6224,#6226,#3126,.T.);
#8213=EDGE_CURVE('',#6227,#6228,#4110,.T.);
#8214=EDGE_CURVE('',#6227,#6225,#3127,.T.);
#8215=EDGE_CURVE('',#6226,#6228,#3128,.T.);
#8216=EDGE_CURVE('',#6229,#6230,#4111,.T.);
#8217=EDGE_CURVE('',#6229,#6227,#3129,.T.);
#8218=EDGE_CURVE('',#6228,#6230,#3130,.T.);
#8219=EDGE_CURVE('',#6231,#6232,#4112,.T.);
#8220=EDGE_CURVE('',#6231,#6229,#3131,.T.);
#8221=EDGE_CURVE('',#6230,#6232,#3132,.T.);
#8222=EDGE_CURVE('',#6233,#6234,#4113,.T.);
#8223=EDGE_CURVE('',#6233,#6231,#3133,.T.);
#8224=EDGE_CURVE('',#6232,#6234,#3134,.T.);
#8225=EDGE_CURVE('',#6235,#6236,#4114,.T.);
#8226=EDGE_CURVE('',#6235,#6233,#3135,.T.);
#8227=EDGE_CURVE('',#6234,#6236,#3136,.T.);
#8228=EDGE_CURVE('',#6237,#6238,#4115,.T.);
#8229=EDGE_CURVE('',#6237,#6235,#3137,.T.);
#8230=EDGE_CURVE('',#6236,#6238,#3138,.T.);
#8231=EDGE_CURVE('',#6239,#6240,#4116,.T.);
#8232=EDGE_CURVE('',#6239,#6237,#3139,.T.);
#8233=EDGE_CURVE('',#6238,#6240,#3140,.T.);
#8234=EDGE_CURVE('',#6241,#6242,#4117,.T.);
#8235=EDGE_CURVE('',#6241,#6239,#3141,.T.);
#8236=EDGE_CURVE('',#6240,#6242,#3142,.T.);
#8237=EDGE_CURVE('',#6243,#6244,#4118,.T.);
#8238=EDGE_CURVE('',#6243,#6241,#3143,.T.);
#8239=EDGE_CURVE('',#6242,#6244,#3144,.T.);
#8240=EDGE_CURVE('',#6245,#6245,#2304,.T.);
#8241=EDGE_CURVE('',#6245,#6246,#4119,.T.);
#8242=EDGE_CURVE('',#6246,#6247,#2305,.T.);
#8243=EDGE_CURVE('',#6247,#6248,#3145,.T.);
#8244=EDGE_CURVE('',#6248,#6249,#4120,.T.);
#8245=EDGE_CURVE('',#6249,#6250,#3146,.T.);
#8246=EDGE_CURVE('',#6250,#6246,#2306,.T.);
#8247=EDGE_CURVE('',#6251,#6252,#4121,.T.);
#8248=EDGE_CURVE('',#6251,#6253,#3147,.T.);
#8249=EDGE_CURVE('',#6254,#6253,#2307,.T.);
#8250=EDGE_CURVE('',#6252,#6254,#3148,.T.);
#8251=EDGE_CURVE('',#6255,#6256,#4122,.T.);
#8252=EDGE_CURVE('',#6255,#6251,#3149,.T.);
#8253=EDGE_CURVE('',#6256,#6252,#3150,.T.);
#8254=EDGE_CURVE('',#6257,#6258,#4123,.T.);
#8255=EDGE_CURVE('',#6257,#6255,#3151,.T.);
#8256=EDGE_CURVE('',#6258,#6256,#3152,.T.);
#8257=EDGE_CURVE('',#6259,#6260,#4124,.T.);
#8258=EDGE_CURVE('',#6259,#6257,#3153,.T.);
#8259=EDGE_CURVE('',#6260,#6258,#3154,.T.);
#8260=EDGE_CURVE('',#6261,#6262,#4125,.T.);
#8261=EDGE_CURVE('',#6261,#6259,#3155,.T.);
#8262=EDGE_CURVE('',#6262,#6260,#3156,.T.);
#8263=EDGE_CURVE('',#6263,#6264,#4126,.T.);
#8264=EDGE_CURVE('',#6263,#6261,#3157,.T.);
#8265=EDGE_CURVE('',#6264,#6262,#3158,.T.);
#8266=EDGE_CURVE('',#6265,#6266,#4127,.T.);
#8267=EDGE_CURVE('',#6265,#6263,#3159,.T.);
#8268=EDGE_CURVE('',#6266,#6264,#3160,.T.);
#8269=EDGE_CURVE('',#6267,#6268,#4128,.T.);
#8270=EDGE_CURVE('',#6267,#6265,#3161,.T.);
#8271=EDGE_CURVE('',#6268,#6266,#3162,.T.);
#8272=EDGE_CURVE('',#6269,#6270,#4129,.T.);
#8273=EDGE_CURVE('',#6269,#6267,#3163,.T.);
#8274=EDGE_CURVE('',#6270,#6268,#3164,.T.);
#8275=EDGE_CURVE('',#6271,#6272,#4130,.T.);
#8276=EDGE_CURVE('',#6271,#6269,#3165,.T.);
#8277=EDGE_CURVE('',#6272,#6270,#3166,.T.);
#8278=EDGE_CURVE('',#6273,#6274,#4131,.T.);
#8279=EDGE_CURVE('',#6273,#6271,#3167,.T.);
#8280=EDGE_CURVE('',#6274,#6272,#3168,.T.);
#8281=EDGE_CURVE('',#6275,#6276,#4132,.T.);
#8282=EDGE_CURVE('',#6275,#6273,#3169,.T.);
#8283=EDGE_CURVE('',#6276,#6274,#3170,.T.);
#8284=EDGE_CURVE('',#6277,#6278,#4133,.T.);
#8285=EDGE_CURVE('',#6277,#6275,#3171,.T.);
#8286=EDGE_CURVE('',#6278,#6276,#3172,.T.);
#8287=EDGE_CURVE('',#6279,#6280,#4134,.T.);
#8288=EDGE_CURVE('',#6279,#6277,#3173,.T.);
#8289=EDGE_CURVE('',#6280,#6278,#3174,.T.);
#8290=EDGE_CURVE('',#6281,#6282,#4135,.T.);
#8291=EDGE_CURVE('',#6281,#6279,#3175,.T.);
#8292=EDGE_CURVE('',#6282,#6280,#3176,.T.);
#8293=EDGE_CURVE('',#6283,#6284,#4136,.T.);
#8294=EDGE_CURVE('',#6283,#6281,#3177,.T.);
#8295=EDGE_CURVE('',#6284,#6282,#3178,.T.);
#8296=EDGE_CURVE('',#6285,#6286,#4137,.T.);
#8297=EDGE_CURVE('',#6285,#6283,#3179,.T.);
#8298=EDGE_CURVE('',#6286,#6284,#3180,.T.);
#8299=EDGE_CURVE('',#6287,#6288,#4138,.T.);
#8300=EDGE_CURVE('',#6287,#6285,#3181,.T.);
#8301=EDGE_CURVE('',#6288,#6286,#3182,.T.);
#8302=EDGE_CURVE('',#6289,#6290,#4139,.T.);
#8303=EDGE_CURVE('',#6289,#6287,#3183,.T.);
#8304=EDGE_CURVE('',#6290,#6288,#3184,.T.);
#8305=EDGE_CURVE('',#6291,#6292,#4140,.T.);
#8306=EDGE_CURVE('',#6291,#6289,#3185,.T.);
#8307=EDGE_CURVE('',#6292,#6290,#3186,.T.);
#8308=EDGE_CURVE('',#6293,#6294,#4141,.T.);
#8309=EDGE_CURVE('',#6293,#6291,#3187,.T.);
#8310=EDGE_CURVE('',#6294,#6292,#3188,.T.);
#8311=EDGE_CURVE('',#6295,#6296,#4142,.T.);
#8312=EDGE_CURVE('',#6295,#6293,#3189,.T.);
#8313=EDGE_CURVE('',#6296,#6294,#3190,.T.);
#8314=EDGE_CURVE('',#6297,#6298,#4143,.T.);
#8315=EDGE_CURVE('',#6297,#6295,#3191,.T.);
#8316=EDGE_CURVE('',#6298,#6296,#3192,.T.);
#8317=EDGE_CURVE('',#6299,#6300,#4144,.T.);
#8318=EDGE_CURVE('',#6299,#6297,#3193,.T.);
#8319=EDGE_CURVE('',#6300,#6298,#3194,.T.);
#8320=EDGE_CURVE('',#6301,#6302,#4145,.T.);
#8321=EDGE_CURVE('',#6301,#6299,#3195,.T.);
#8322=EDGE_CURVE('',#6302,#6300,#3196,.T.);
#8323=EDGE_CURVE('',#6303,#6304,#4146,.T.);
#8324=EDGE_CURVE('',#6303,#6301,#3197,.T.);
#8325=EDGE_CURVE('',#6304,#6302,#3198,.T.);
#8326=EDGE_CURVE('',#6305,#6306,#4147,.T.);
#8327=EDGE_CURVE('',#6305,#6303,#3199,.T.);
#8328=EDGE_CURVE('',#6306,#6304,#3200,.T.);
#8329=EDGE_CURVE('',#6307,#6308,#4148,.T.);
#8330=EDGE_CURVE('',#6307,#6305,#3201,.T.);
#8331=EDGE_CURVE('',#6308,#6306,#3202,.T.);
#8332=EDGE_CURVE('',#6309,#6310,#4149,.T.);
#8333=EDGE_CURVE('',#6309,#6307,#3203,.T.);
#8334=EDGE_CURVE('',#6310,#6308,#3204,.T.);
#8335=EDGE_CURVE('',#6311,#6312,#4150,.T.);
#8336=EDGE_CURVE('',#6311,#6309,#3205,.T.);
#8337=EDGE_CURVE('',#6312,#6310,#3206,.T.);
#8338=EDGE_CURVE('',#6313,#6314,#4151,.T.);
#8339=EDGE_CURVE('',#6313,#6311,#3207,.T.);
#8340=EDGE_CURVE('',#6314,#6312,#3208,.T.);
#8341=EDGE_CURVE('',#6315,#6316,#4152,.T.);
#8342=EDGE_CURVE('',#6315,#6313,#3209,.T.);
#8343=EDGE_CURVE('',#6316,#6314,#3210,.T.);
#8344=EDGE_CURVE('',#6317,#6318,#4153,.T.);
#8345=EDGE_CURVE('',#6317,#6315,#3211,.T.);
#8346=EDGE_CURVE('',#6318,#6316,#3212,.T.);
#8347=EDGE_CURVE('',#6319,#6320,#4154,.T.);
#8348=EDGE_CURVE('',#6319,#6317,#3213,.T.);
#8349=EDGE_CURVE('',#6320,#6318,#3214,.T.);
#8350=EDGE_CURVE('',#6321,#6322,#4155,.T.);
#8351=EDGE_CURVE('',#6321,#6319,#3215,.T.);
#8352=EDGE_CURVE('',#6322,#6320,#3216,.T.);
#8353=EDGE_CURVE('',#6323,#6324,#4156,.T.);
#8354=EDGE_CURVE('',#6323,#6321,#3217,.T.);
#8355=EDGE_CURVE('',#6324,#6322,#3218,.T.);
#8356=EDGE_CURVE('',#6325,#6326,#4157,.T.);
#8357=EDGE_CURVE('',#6325,#6327,#4158,.T.);
#8358=EDGE_CURVE('',#6327,#6328,#4159,.T.);
#8359=EDGE_CURVE('',#6326,#6328,#4160,.T.);
#8360=EDGE_CURVE('',#6329,#6325,#4161,.T.);
#8361=EDGE_CURVE('',#6329,#6330,#4162,.T.);
#8362=EDGE_CURVE('',#6330,#6327,#4163,.T.);
#8363=EDGE_CURVE('',#6331,#6329,#4164,.T.);
#8364=EDGE_CURVE('',#6331,#6332,#4165,.T.);
#8365=EDGE_CURVE('',#6332,#6330,#4166,.T.);
#8366=EDGE_CURVE('',#6333,#6331,#4167,.T.);
#8367=EDGE_CURVE('',#6333,#6334,#4168,.T.);
#8368=EDGE_CURVE('',#6334,#6332,#4169,.T.);
#8369=EDGE_CURVE('',#6335,#6333,#4170,.T.);
#8370=EDGE_CURVE('',#6335,#6336,#4171,.T.);
#8371=EDGE_CURVE('',#6336,#6334,#4172,.T.);
#8372=EDGE_CURVE('',#6326,#6335,#4173,.T.);
#8373=EDGE_CURVE('',#6328,#6336,#4174,.T.);
#8374=EDGE_CURVE('',#6337,#6337,#2308,.T.);
#8375=EDGE_CURVE('',#6337,#6338,#4175,.T.);
#8376=EDGE_CURVE('',#6338,#6338,#2309,.T.);
#8377=EDGE_CURVE('',#6339,#6339,#2310,.T.);
#8378=EDGE_CURVE('',#6340,#6340,#2311,.F.);
#8379=EDGE_CURVE('',#6340,#6339,#4176,.T.);
#8380=EDGE_CURVE('',#6253,#6247,#3219,.T.);
#8381=EDGE_CURVE('',#6250,#6254,#3220,.T.);
#8382=EDGE_CURVE('',#6244,#6249,#3221,.T.);
#8383=EDGE_CURVE('',#6341,#6174,#3222,.T.);
#8384=EDGE_CURVE('',#6341,#6324,#3223,.T.);
#8385=EDGE_CURVE('',#6342,#6341,#2312,.T.);
#8386=EDGE_CURVE('',#6342,#6323,#3224,.T.);
#8387=EDGE_CURVE('',#6173,#6342,#3225,.T.);
#8388=EDGE_CURVE('',#6248,#6243,#3226,.T.);
#8389=EDGE_CURVE('',#6343,#6343,#2313,.T.);
#8390=EDGE_CURVE('',#6344,#6344,#2314,.T.);
#8391=EDGE_CURVE('',#6344,#6343,#4177,.T.);
#8392=EDGE_CURVE('',#6345,#6346,#4178,.T.);
#8393=EDGE_CURVE('',#6347,#6345,#4179,.T.);
#8394=EDGE_CURVE('',#6348,#6347,#4180,.T.);
#8395=EDGE_CURVE('',#6346,#6348,#4181,.T.);
#8396=EDGE_CURVE('',#6349,#6350,#4182,.T.);
#8397=EDGE_CURVE('',#6351,#6349,#4183,.T.);
#8398=EDGE_CURVE('',#6352,#6351,#4184,.T.);
#8399=EDGE_CURVE('',#6350,#6352,#4185,.T.);
#8400=EDGE_CURVE('',#6347,#6352,#2315,.T.);
#8401=EDGE_CURVE('',#6350,#6345,#2316,.T.);
#8402=EDGE_CURVE('',#6349,#6346,#2317,.T.);
#8403=EDGE_CURVE('',#6348,#6351,#2318,.T.);
#8404=EDGE_CURVE('',#6353,#6353,#2319,.T.);
#8405=EDGE_CURVE('',#6353,#6354,#4186,.T.);
#8406=EDGE_CURVE('',#6354,#6354,#2320,.T.);
#8407=EDGE_CURVE('',#6355,#6355,#2321,.T.);
#8408=EDGE_CURVE('',#6355,#6356,#4187,.T.);
#8409=EDGE_CURVE('',#6356,#6356,#2322,.T.);
#8410=EDGE_CURVE('',#6357,#6357,#2323,.T.);
#8411=EDGE_CURVE('',#6357,#6358,#4188,.T.);
#8412=EDGE_CURVE('',#6358,#6358,#2324,.T.);
#8413=EDGE_CURVE('',#6359,#6359,#2325,.T.);
#8414=EDGE_CURVE('',#6359,#6360,#4189,.T.);
#8415=EDGE_CURVE('',#6360,#6360,#2326,.T.);
#8416=EDGE_CURVE('',#6361,#6362,#4190,.T.);
#8417=EDGE_CURVE('',#6361,#6363,#3227,.T.);
#8418=EDGE_CURVE('',#6363,#6364,#2327,.F.);
#8419=EDGE_CURVE('',#6364,#6362,#3228,.T.);
#8420=EDGE_CURVE('',#6365,#6366,#4191,.T.);
#8421=EDGE_CURVE('',#6365,#6361,#3229,.T.);
#8422=EDGE_CURVE('',#6362,#6366,#3230,.T.);
#8423=EDGE_CURVE('',#6367,#6368,#4192,.T.);
#8424=EDGE_CURVE('',#6367,#6365,#3231,.T.);
#8425=EDGE_CURVE('',#6366,#6368,#3232,.T.);
#8426=EDGE_CURVE('',#6369,#6370,#4193,.T.);
#8427=EDGE_CURVE('',#6369,#6367,#3233,.T.);
#8428=EDGE_CURVE('',#6368,#6370,#3234,.T.);
#8429=EDGE_CURVE('',#6371,#6372,#4194,.T.);
#8430=EDGE_CURVE('',#6371,#6369,#3235,.T.);
#8431=EDGE_CURVE('',#6370,#6372,#3236,.T.);
#8432=EDGE_CURVE('',#6373,#6374,#4195,.T.);
#8433=EDGE_CURVE('',#6373,#6371,#3237,.T.);
#8434=EDGE_CURVE('',#6372,#6374,#3238,.T.);
#8435=EDGE_CURVE('',#6375,#6376,#4196,.T.);
#8436=EDGE_CURVE('',#6375,#6373,#3239,.T.);
#8437=EDGE_CURVE('',#6374,#6376,#3240,.T.);
#8438=EDGE_CURVE('',#6377,#6378,#4197,.T.);
#8439=EDGE_CURVE('',#6377,#6375,#3241,.T.);
#8440=EDGE_CURVE('',#6376,#6378,#3242,.T.);
#8441=EDGE_CURVE('',#6379,#6380,#4198,.T.);
#8442=EDGE_CURVE('',#6379,#6377,#3243,.T.);
#8443=EDGE_CURVE('',#6378,#6380,#3244,.T.);
#8444=EDGE_CURVE('',#6381,#6382,#4199,.T.);
#8445=EDGE_CURVE('',#6381,#6379,#3245,.T.);
#8446=EDGE_CURVE('',#6380,#6382,#3246,.T.);
#8447=EDGE_CURVE('',#6383,#6384,#4200,.T.);
#8448=EDGE_CURVE('',#6383,#6381,#3247,.T.);
#8449=EDGE_CURVE('',#6382,#6384,#3248,.T.);
#8450=EDGE_CURVE('',#6385,#6386,#4201,.T.);
#8451=EDGE_CURVE('',#6385,#6383,#3249,.T.);
#8452=EDGE_CURVE('',#6384,#6386,#3250,.T.);
#8453=EDGE_CURVE('',#6387,#6388,#4202,.T.);
#8454=EDGE_CURVE('',#6387,#6385,#3251,.T.);
#8455=EDGE_CURVE('',#6386,#6388,#3252,.T.);
#8456=EDGE_CURVE('',#6389,#6390,#4203,.T.);
#8457=EDGE_CURVE('',#6389,#6387,#3253,.T.);
#8458=EDGE_CURVE('',#6388,#6390,#3254,.T.);
#8459=EDGE_CURVE('',#6391,#6392,#4204,.T.);
#8460=EDGE_CURVE('',#6391,#6389,#3255,.T.);
#8461=EDGE_CURVE('',#6390,#6392,#3256,.T.);
#8462=EDGE_CURVE('',#6393,#6394,#4205,.T.);
#8463=EDGE_CURVE('',#6393,#6391,#3257,.T.);
#8464=EDGE_CURVE('',#6392,#6394,#3258,.T.);
#8465=EDGE_CURVE('',#6395,#6396,#4206,.T.);
#8466=EDGE_CURVE('',#6395,#6393,#3259,.T.);
#8467=EDGE_CURVE('',#6394,#6396,#3260,.T.);
#8468=EDGE_CURVE('',#6397,#6398,#4207,.T.);
#8469=EDGE_CURVE('',#6397,#6395,#3261,.T.);
#8470=EDGE_CURVE('',#6396,#6398,#3262,.T.);
#8471=EDGE_CURVE('',#6399,#6400,#4208,.T.);
#8472=EDGE_CURVE('',#6399,#6397,#3263,.T.);
#8473=EDGE_CURVE('',#6398,#6400,#3264,.T.);
#8474=EDGE_CURVE('',#6401,#6402,#4209,.T.);
#8475=EDGE_CURVE('',#6401,#6399,#3265,.T.);
#8476=EDGE_CURVE('',#6400,#6402,#3266,.T.);
#8477=EDGE_CURVE('',#6403,#6404,#4210,.T.);
#8478=EDGE_CURVE('',#6403,#6401,#3267,.T.);
#8479=EDGE_CURVE('',#6402,#6404,#3268,.T.);
#8480=EDGE_CURVE('',#6405,#6406,#4211,.T.);
#8481=EDGE_CURVE('',#6405,#6403,#3269,.T.);
#8482=EDGE_CURVE('',#6404,#6406,#3270,.T.);
#8483=EDGE_CURVE('',#6407,#6408,#4212,.T.);
#8484=EDGE_CURVE('',#6407,#6405,#3271,.T.);
#8485=EDGE_CURVE('',#6406,#6408,#3272,.T.);
#8486=EDGE_CURVE('',#6409,#6410,#4213,.T.);
#8487=EDGE_CURVE('',#6409,#6407,#3273,.T.);
#8488=EDGE_CURVE('',#6408,#6410,#3274,.T.);
#8489=EDGE_CURVE('',#6411,#6412,#4214,.T.);
#8490=EDGE_CURVE('',#6411,#6409,#3275,.T.);
#8491=EDGE_CURVE('',#6410,#6412,#3276,.T.);
#8492=EDGE_CURVE('',#6413,#6414,#4215,.T.);
#8493=EDGE_CURVE('',#6413,#6411,#3277,.T.);
#8494=EDGE_CURVE('',#6412,#6414,#3278,.T.);
#8495=EDGE_CURVE('',#6415,#6416,#4216,.T.);
#8496=EDGE_CURVE('',#6415,#6413,#3279,.T.);
#8497=EDGE_CURVE('',#6414,#6416,#3280,.T.);
#8498=EDGE_CURVE('',#6417,#6418,#4217,.T.);
#8499=EDGE_CURVE('',#6417,#6415,#3281,.T.);
#8500=EDGE_CURVE('',#6416,#6418,#3282,.T.);
#8501=EDGE_CURVE('',#6419,#6420,#4218,.T.);
#8502=EDGE_CURVE('',#6419,#6417,#3283,.T.);
#8503=EDGE_CURVE('',#6418,#6420,#3284,.T.);
#8504=EDGE_CURVE('',#6421,#6422,#4219,.T.);
#8505=EDGE_CURVE('',#6421,#6419,#3285,.T.);
#8506=EDGE_CURVE('',#6420,#6422,#3286,.T.);
#8507=EDGE_CURVE('',#6423,#6424,#4220,.T.);
#8508=EDGE_CURVE('',#6423,#6421,#3287,.T.);
#8509=EDGE_CURVE('',#6422,#6424,#3288,.T.);
#8510=EDGE_CURVE('',#6425,#6426,#4221,.T.);
#8511=EDGE_CURVE('',#6425,#6423,#3289,.T.);
#8512=EDGE_CURVE('',#6424,#6426,#3290,.T.);
#8513=EDGE_CURVE('',#6427,#6428,#4222,.T.);
#8514=EDGE_CURVE('',#6427,#6425,#3291,.T.);
#8515=EDGE_CURVE('',#6426,#6428,#3292,.T.);
#8516=EDGE_CURVE('',#6429,#6430,#4223,.T.);
#8517=EDGE_CURVE('',#6429,#6427,#3293,.T.);
#8518=EDGE_CURVE('',#6428,#6430,#3294,.T.);
#8519=EDGE_CURVE('',#6431,#6432,#4224,.T.);
#8520=EDGE_CURVE('',#6431,#6429,#3295,.T.);
#8521=EDGE_CURVE('',#6430,#6432,#3296,.T.);
#8522=EDGE_CURVE('',#6433,#6434,#4225,.T.);
#8523=EDGE_CURVE('',#6433,#6431,#3297,.T.);
#8524=EDGE_CURVE('',#6432,#6434,#3298,.T.);
#8525=EDGE_CURVE('',#6435,#6436,#4226,.T.);
#8526=EDGE_CURVE('',#6435,#6433,#3299,.T.);
#8527=EDGE_CURVE('',#6434,#6436,#3300,.T.);
#8528=EDGE_CURVE('',#6437,#6438,#4227,.T.);
#8529=EDGE_CURVE('',#6437,#6435,#3301,.T.);
#8530=EDGE_CURVE('',#6436,#6438,#3302,.T.);
#8531=EDGE_CURVE('',#6439,#6440,#4228,.T.);
#8532=EDGE_CURVE('',#6439,#6437,#3303,.T.);
#8533=EDGE_CURVE('',#6438,#6440,#3304,.T.);
#8534=EDGE_CURVE('',#6441,#6442,#4229,.T.);
#8535=EDGE_CURVE('',#6441,#6443,#3305,.T.);
#8536=EDGE_CURVE('',#6443,#6444,#2328,.T.);
#8537=EDGE_CURVE('',#6442,#6444,#3306,.T.);
#8538=EDGE_CURVE('',#6445,#6446,#4230,.T.);
#8539=EDGE_CURVE('',#6445,#6441,#3307,.T.);
#8540=EDGE_CURVE('',#6446,#6442,#3308,.T.);
#8541=EDGE_CURVE('',#6447,#6448,#4231,.T.);
#8542=EDGE_CURVE('',#6447,#6445,#3309,.T.);
#8543=EDGE_CURVE('',#6448,#6446,#3310,.T.);
#8544=EDGE_CURVE('',#6449,#6450,#4232,.T.);
#8545=EDGE_CURVE('',#6449,#6447,#3311,.T.);
#8546=EDGE_CURVE('',#6450,#6448,#3312,.T.);
#8547=EDGE_CURVE('',#6451,#6452,#4233,.T.);
#8548=EDGE_CURVE('',#6451,#6449,#3313,.T.);
#8549=EDGE_CURVE('',#6452,#6450,#3314,.T.);
#8550=EDGE_CURVE('',#6453,#6454,#4234,.T.);
#8551=EDGE_CURVE('',#6453,#6451,#3315,.T.);
#8552=EDGE_CURVE('',#6454,#6452,#3316,.T.);
#8553=EDGE_CURVE('',#6455,#6456,#4235,.T.);
#8554=EDGE_CURVE('',#6455,#6453,#3317,.T.);
#8555=EDGE_CURVE('',#6456,#6454,#3318,.T.);
#8556=EDGE_CURVE('',#6457,#6458,#4236,.T.);
#8557=EDGE_CURVE('',#6457,#6455,#3319,.T.);
#8558=EDGE_CURVE('',#6458,#6456,#3320,.T.);
#8559=EDGE_CURVE('',#6459,#6460,#4237,.T.);
#8560=EDGE_CURVE('',#6459,#6457,#3321,.T.);
#8561=EDGE_CURVE('',#6460,#6458,#3322,.T.);
#8562=EDGE_CURVE('',#6461,#6462,#4238,.T.);
#8563=EDGE_CURVE('',#6461,#6459,#3323,.T.);
#8564=EDGE_CURVE('',#6462,#6460,#3324,.T.);
#8565=EDGE_CURVE('',#6463,#6464,#4239,.T.);
#8566=EDGE_CURVE('',#6463,#6461,#3325,.T.);
#8567=EDGE_CURVE('',#6464,#6462,#3326,.T.);
#8568=EDGE_CURVE('',#6465,#6466,#4240,.T.);
#8569=EDGE_CURVE('',#6465,#6463,#3327,.T.);
#8570=EDGE_CURVE('',#6466,#6464,#3328,.T.);
#8571=EDGE_CURVE('',#6467,#6468,#4241,.T.);
#8572=EDGE_CURVE('',#6467,#6465,#3329,.T.);
#8573=EDGE_CURVE('',#6468,#6466,#3330,.T.);
#8574=EDGE_CURVE('',#6469,#6470,#4242,.T.);
#8575=EDGE_CURVE('',#6469,#6467,#3331,.T.);
#8576=EDGE_CURVE('',#6470,#6468,#3332,.T.);
#8577=EDGE_CURVE('',#6471,#6472,#4243,.T.);
#8578=EDGE_CURVE('',#6471,#6469,#3333,.T.);
#8579=EDGE_CURVE('',#6472,#6470,#3334,.T.);
#8580=EDGE_CURVE('',#6473,#6474,#4244,.T.);
#8581=EDGE_CURVE('',#6473,#6471,#3335,.T.);
#8582=EDGE_CURVE('',#6474,#6472,#3336,.T.);
#8583=EDGE_CURVE('',#6475,#6476,#4245,.T.);
#8584=EDGE_CURVE('',#6475,#6473,#3337,.T.);
#8585=EDGE_CURVE('',#6476,#6474,#3338,.T.);
#8586=EDGE_CURVE('',#6477,#6478,#4246,.T.);
#8587=EDGE_CURVE('',#6477,#6475,#3339,.T.);
#8588=EDGE_CURVE('',#6478,#6476,#3340,.T.);
#8589=EDGE_CURVE('',#6479,#6480,#4247,.T.);
#8590=EDGE_CURVE('',#6479,#6477,#3341,.T.);
#8591=EDGE_CURVE('',#6480,#6478,#3342,.T.);
#8592=EDGE_CURVE('',#6481,#6482,#4248,.T.);
#8593=EDGE_CURVE('',#6481,#6479,#3343,.T.);
#8594=EDGE_CURVE('',#6482,#6480,#3344,.T.);
#8595=EDGE_CURVE('',#6483,#6484,#4249,.T.);
#8596=EDGE_CURVE('',#6483,#6481,#3345,.T.);
#8597=EDGE_CURVE('',#6484,#6482,#3346,.T.);
#8598=EDGE_CURVE('',#6485,#6486,#4250,.T.);
#8599=EDGE_CURVE('',#6485,#6483,#3347,.T.);
#8600=EDGE_CURVE('',#6486,#6484,#3348,.T.);
#8601=EDGE_CURVE('',#6487,#6488,#4251,.T.);
#8602=EDGE_CURVE('',#6487,#6485,#3349,.T.);
#8603=EDGE_CURVE('',#6488,#6486,#3350,.T.);
#8604=EDGE_CURVE('',#6489,#6490,#4252,.T.);
#8605=EDGE_CURVE('',#6489,#6487,#3351,.T.);
#8606=EDGE_CURVE('',#6490,#6488,#3352,.T.);
#8607=EDGE_CURVE('',#6491,#6492,#4253,.T.);
#8608=EDGE_CURVE('',#6491,#6489,#3353,.T.);
#8609=EDGE_CURVE('',#6492,#6490,#3354,.T.);
#8610=EDGE_CURVE('',#6493,#6494,#4254,.T.);
#8611=EDGE_CURVE('',#6493,#6491,#3355,.T.);
#8612=EDGE_CURVE('',#6494,#6492,#3356,.T.);
#8613=EDGE_CURVE('',#6495,#6496,#4255,.T.);
#8614=EDGE_CURVE('',#6495,#6493,#3357,.T.);
#8615=EDGE_CURVE('',#6496,#6494,#3358,.T.);
#8616=EDGE_CURVE('',#6497,#6498,#4256,.T.);
#8617=EDGE_CURVE('',#6497,#6495,#3359,.T.);
#8618=EDGE_CURVE('',#6498,#6496,#3360,.T.);
#8619=EDGE_CURVE('',#6499,#6500,#4257,.T.);
#8620=EDGE_CURVE('',#6499,#6497,#3361,.T.);
#8621=EDGE_CURVE('',#6500,#6498,#3362,.T.);
#8622=EDGE_CURVE('',#6501,#6502,#4258,.T.);
#8623=EDGE_CURVE('',#6501,#6499,#3363,.T.);
#8624=EDGE_CURVE('',#6502,#6500,#3364,.T.);
#8625=EDGE_CURVE('',#6503,#6504,#4259,.T.);
#8626=EDGE_CURVE('',#6503,#6501,#3365,.T.);
#8627=EDGE_CURVE('',#6504,#6502,#3366,.T.);
#8628=EDGE_CURVE('',#6505,#6506,#4260,.T.);
#8629=EDGE_CURVE('',#6505,#6503,#3367,.T.);
#8630=EDGE_CURVE('',#6506,#6504,#3368,.T.);
#8631=EDGE_CURVE('',#6507,#6508,#4261,.T.);
#8632=EDGE_CURVE('',#6507,#6505,#3369,.T.);
#8633=EDGE_CURVE('',#6508,#6506,#3370,.T.);
#8634=EDGE_CURVE('',#6509,#6510,#4262,.T.);
#8635=EDGE_CURVE('',#6509,#6507,#3371,.T.);
#8636=EDGE_CURVE('',#6510,#6508,#3372,.T.);
#8637=EDGE_CURVE('',#6511,#6512,#4263,.T.);
#8638=EDGE_CURVE('',#6511,#6509,#3373,.T.);
#8639=EDGE_CURVE('',#6512,#6510,#3374,.T.);
#8640=EDGE_CURVE('',#6513,#6514,#4264,.T.);
#8641=EDGE_CURVE('',#6513,#6511,#3375,.T.);
#8642=EDGE_CURVE('',#6514,#6512,#3376,.T.);
#8643=EDGE_CURVE('',#6515,#6516,#4265,.T.);
#8644=EDGE_CURVE('',#6515,#6513,#3377,.T.);
#8645=EDGE_CURVE('',#6516,#6514,#3378,.T.);
#8646=EDGE_CURVE('',#6517,#6518,#4266,.T.);
#8647=EDGE_CURVE('',#6517,#6515,#3379,.T.);
#8648=EDGE_CURVE('',#6518,#6516,#3380,.T.);
#8649=EDGE_CURVE('',#6519,#6520,#4267,.T.);
#8650=EDGE_CURVE('',#6519,#6517,#3381,.T.);
#8651=EDGE_CURVE('',#6520,#6518,#3382,.T.);
#8652=EDGE_CURVE('',#6444,#6521,#3383,.T.);
#8653=EDGE_CURVE('',#6522,#6443,#3384,.T.);
#8654=EDGE_CURVE('',#6523,#6522,#2329,.T.);
#8655=EDGE_CURVE('',#6521,#6523,#3385,.T.);
#8656=EDGE_CURVE('',#6521,#6524,#4268,.T.);
#8657=EDGE_CURVE('',#6524,#6524,#2330,.T.);
#8658=EDGE_CURVE('',#6525,#6519,#3386,.T.);
#8659=EDGE_CURVE('',#6363,#6525,#3387,.T.);
#8660=EDGE_CURVE('',#6522,#6439,#3388,.T.);
#8661=EDGE_CURVE('',#6526,#6520,#3389,.T.);
#8662=EDGE_CURVE('',#6525,#6526,#2331,.T.);
#8663=EDGE_CURVE('',#6440,#6523,#3390,.T.);
#8664=EDGE_CURVE('',#6526,#6364,#3391,.T.);
#8665=EDGE_CURVE('',#6527,#6528,#4269,.T.);
#8666=EDGE_CURVE('',#6527,#6529,#4270,.T.);
#8667=EDGE_CURVE('',#6529,#6530,#4271,.T.);
#8668=EDGE_CURVE('',#6528,#6530,#4272,.T.);
#8669=EDGE_CURVE('',#6531,#6527,#4273,.T.);
#8670=EDGE_CURVE('',#6531,#6532,#4274,.T.);
#8671=EDGE_CURVE('',#6532,#6529,#4275,.T.);
#8672=EDGE_CURVE('',#6533,#6531,#4276,.T.);
#8673=EDGE_CURVE('',#6533,#6534,#4277,.T.);
#8674=EDGE_CURVE('',#6534,#6532,#4278,.T.);
#8675=EDGE_CURVE('',#6535,#6533,#4279,.T.);
#8676=EDGE_CURVE('',#6535,#6536,#4280,.T.);
#8677=EDGE_CURVE('',#6536,#6534,#4281,.T.);
#8678=EDGE_CURVE('',#6537,#6535,#4282,.T.);
#8679=EDGE_CURVE('',#6537,#6538,#4283,.T.);
#8680=EDGE_CURVE('',#6538,#6536,#4284,.T.);
#8681=EDGE_CURVE('',#6528,#6537,#4285,.T.);
#8682=EDGE_CURVE('',#6530,#6538,#4286,.T.);
#8683=EDGE_CURVE('',#6539,#6539,#2332,.T.);
#8684=EDGE_CURVE('',#6539,#6540,#4287,.T.);
#8685=EDGE_CURVE('',#6540,#6540,#2333,.T.);
#8686=EDGE_CURVE('',#6541,#6541,#2334,.T.);
#8687=EDGE_CURVE('',#6541,#6542,#4288,.T.);
#8688=EDGE_CURVE('',#6542,#6542,#2335,.T.);
#8689=EDGE_CURVE('',#6543,#6543,#2336,.T.);
#8690=EDGE_CURVE('',#6543,#6544,#4289,.T.);
#8691=EDGE_CURVE('',#6544,#6544,#2337,.T.);
#8692=EDGE_CURVE('',#6545,#6546,#4290,.T.);
#8693=EDGE_CURVE('',#6545,#6547,#3392,.T.);
#8694=EDGE_CURVE('',#6547,#6548,#2338,.F.);
#8695=EDGE_CURVE('',#6548,#6546,#3393,.T.);
#8696=EDGE_CURVE('',#6549,#6550,#4291,.T.);
#8697=EDGE_CURVE('',#6549,#6545,#3394,.T.);
#8698=EDGE_CURVE('',#6546,#6550,#3395,.T.);
#8699=EDGE_CURVE('',#6551,#6552,#4292,.T.);
#8700=EDGE_CURVE('',#6551,#6549,#3396,.T.);
#8701=EDGE_CURVE('',#6550,#6552,#3397,.T.);
#8702=EDGE_CURVE('',#6553,#6554,#4293,.T.);
#8703=EDGE_CURVE('',#6553,#6551,#3398,.T.);
#8704=EDGE_CURVE('',#6552,#6554,#3399,.T.);
#8705=EDGE_CURVE('',#6555,#6556,#4294,.T.);
#8706=EDGE_CURVE('',#6555,#6553,#3400,.T.);
#8707=EDGE_CURVE('',#6554,#6556,#3401,.T.);
#8708=EDGE_CURVE('',#6557,#6558,#4295,.T.);
#8709=EDGE_CURVE('',#6557,#6555,#3402,.T.);
#8710=EDGE_CURVE('',#6556,#6558,#3403,.T.);
#8711=EDGE_CURVE('',#6559,#6560,#4296,.T.);
#8712=EDGE_CURVE('',#6559,#6557,#3404,.T.);
#8713=EDGE_CURVE('',#6558,#6560,#3405,.T.);
#8714=EDGE_CURVE('',#6561,#6562,#4297,.T.);
#8715=EDGE_CURVE('',#6561,#6559,#3406,.T.);
#8716=EDGE_CURVE('',#6560,#6562,#3407,.T.);
#8717=EDGE_CURVE('',#6563,#6564,#4298,.T.);
#8718=EDGE_CURVE('',#6563,#6561,#3408,.T.);
#8719=EDGE_CURVE('',#6562,#6564,#3409,.T.);
#8720=EDGE_CURVE('',#6565,#6566,#4299,.T.);
#8721=EDGE_CURVE('',#6565,#6563,#3410,.T.);
#8722=EDGE_CURVE('',#6564,#6566,#3411,.T.);
#8723=EDGE_CURVE('',#6567,#6568,#4300,.T.);
#8724=EDGE_CURVE('',#6567,#6565,#3412,.T.);
#8725=EDGE_CURVE('',#6566,#6568,#3413,.T.);
#8726=EDGE_CURVE('',#6569,#6570,#4301,.T.);
#8727=EDGE_CURVE('',#6569,#6567,#3414,.T.);
#8728=EDGE_CURVE('',#6568,#6570,#3415,.T.);
#8729=EDGE_CURVE('',#6571,#6572,#4302,.T.);
#8730=EDGE_CURVE('',#6571,#6569,#3416,.T.);
#8731=EDGE_CURVE('',#6570,#6572,#3417,.T.);
#8732=EDGE_CURVE('',#6573,#6574,#4303,.T.);
#8733=EDGE_CURVE('',#6573,#6571,#3418,.T.);
#8734=EDGE_CURVE('',#6572,#6574,#3419,.T.);
#8735=EDGE_CURVE('',#6575,#6576,#4304,.T.);
#8736=EDGE_CURVE('',#6575,#6573,#3420,.T.);
#8737=EDGE_CURVE('',#6574,#6576,#3421,.T.);
#8738=EDGE_CURVE('',#6577,#6578,#4305,.T.);
#8739=EDGE_CURVE('',#6577,#6575,#3422,.T.);
#8740=EDGE_CURVE('',#6576,#6578,#3423,.T.);
#8741=EDGE_CURVE('',#6579,#6580,#4306,.T.);
#8742=EDGE_CURVE('',#6579,#6577,#3424,.T.);
#8743=EDGE_CURVE('',#6578,#6580,#3425,.T.);
#8744=EDGE_CURVE('',#6581,#6582,#4307,.T.);
#8745=EDGE_CURVE('',#6581,#6579,#3426,.T.);
#8746=EDGE_CURVE('',#6580,#6582,#3427,.T.);
#8747=EDGE_CURVE('',#6583,#6584,#4308,.T.);
#8748=EDGE_CURVE('',#6583,#6581,#3428,.T.);
#8749=EDGE_CURVE('',#6582,#6584,#3429,.T.);
#8750=EDGE_CURVE('',#6585,#6586,#4309,.T.);
#8751=EDGE_CURVE('',#6585,#6583,#3430,.T.);
#8752=EDGE_CURVE('',#6584,#6586,#3431,.T.);
#8753=EDGE_CURVE('',#6587,#6588,#4310,.T.);
#8754=EDGE_CURVE('',#6587,#6585,#3432,.T.);
#8755=EDGE_CURVE('',#6586,#6588,#3433,.T.);
#8756=EDGE_CURVE('',#6589,#6590,#4311,.T.);
#8757=EDGE_CURVE('',#6589,#6587,#3434,.T.);
#8758=EDGE_CURVE('',#6588,#6590,#3435,.T.);
#8759=EDGE_CURVE('',#6591,#6592,#4312,.T.);
#8760=EDGE_CURVE('',#6591,#6589,#3436,.T.);
#8761=EDGE_CURVE('',#6590,#6592,#3437,.T.);
#8762=EDGE_CURVE('',#6593,#6594,#4313,.T.);
#8763=EDGE_CURVE('',#6593,#6591,#3438,.T.);
#8764=EDGE_CURVE('',#6592,#6594,#3439,.T.);
#8765=EDGE_CURVE('',#6595,#6596,#4314,.T.);
#8766=EDGE_CURVE('',#6595,#6593,#3440,.T.);
#8767=EDGE_CURVE('',#6594,#6596,#3441,.T.);
#8768=EDGE_CURVE('',#6597,#6598,#4315,.T.);
#8769=EDGE_CURVE('',#6597,#6595,#3442,.T.);
#8770=EDGE_CURVE('',#6596,#6598,#3443,.T.);
#8771=EDGE_CURVE('',#6599,#6600,#4316,.T.);
#8772=EDGE_CURVE('',#6599,#6597,#3444,.T.);
#8773=EDGE_CURVE('',#6598,#6600,#3445,.T.);
#8774=EDGE_CURVE('',#6601,#6602,#4317,.T.);
#8775=EDGE_CURVE('',#6601,#6599,#3446,.T.);
#8776=EDGE_CURVE('',#6600,#6602,#3447,.T.);
#8777=EDGE_CURVE('',#6603,#6604,#4318,.T.);
#8778=EDGE_CURVE('',#6603,#6601,#3448,.T.);
#8779=EDGE_CURVE('',#6602,#6604,#3449,.T.);
#8780=EDGE_CURVE('',#6605,#6606,#4319,.T.);
#8781=EDGE_CURVE('',#6605,#6603,#3450,.T.);
#8782=EDGE_CURVE('',#6604,#6606,#3451,.T.);
#8783=EDGE_CURVE('',#6607,#6608,#4320,.T.);
#8784=EDGE_CURVE('',#6607,#6605,#3452,.T.);
#8785=EDGE_CURVE('',#6606,#6608,#3453,.T.);
#8786=EDGE_CURVE('',#6609,#6610,#4321,.T.);
#8787=EDGE_CURVE('',#6609,#6611,#2339,.T.);
#8788=EDGE_CURVE('',#6611,#6607,#3454,.T.);
#8789=EDGE_CURVE('',#6608,#6610,#3455,.T.);
#8790=EDGE_CURVE('',#6612,#6613,#4322,.T.);
#8791=EDGE_CURVE('',#6612,#6614,#3456,.T.);
#8792=EDGE_CURVE('',#6614,#6613,#2340,.T.);
#8793=EDGE_CURVE('',#6615,#6616,#4323,.T.);
#8794=EDGE_CURVE('',#6615,#6612,#3457,.T.);
#8795=EDGE_CURVE('',#6613,#6617,#2341,.T.);
#8796=EDGE_CURVE('',#6616,#6617,#3458,.T.);
#8797=EDGE_CURVE('',#6618,#6619,#4324,.T.);
#8798=EDGE_CURVE('',#6618,#6615,#3459,.T.);
#8799=EDGE_CURVE('',#6619,#6616,#3460,.T.);
#8800=EDGE_CURVE('',#6620,#6621,#4325,.T.);
#8801=EDGE_CURVE('',#6620,#6618,#3461,.T.);
#8802=EDGE_CURVE('',#6621,#6619,#3462,.T.);
#8803=EDGE_CURVE('',#6622,#6623,#4326,.T.);
#8804=EDGE_CURVE('',#6622,#6620,#3463,.T.);
#8805=EDGE_CURVE('',#6623,#6621,#3464,.T.);
#8806=EDGE_CURVE('',#6624,#6625,#4327,.T.);
#8807=EDGE_CURVE('',#6624,#6622,#3465,.T.);
#8808=EDGE_CURVE('',#6625,#6623,#3466,.T.);
#8809=EDGE_CURVE('',#6626,#6627,#4328,.T.);
#8810=EDGE_CURVE('',#6626,#6624,#3467,.T.);
#8811=EDGE_CURVE('',#6627,#6625,#3468,.T.);
#8812=EDGE_CURVE('',#6628,#6629,#4329,.T.);
#8813=EDGE_CURVE('',#6628,#6626,#3469,.T.);
#8814=EDGE_CURVE('',#6629,#6627,#3470,.T.);
#8815=EDGE_CURVE('',#6630,#6631,#4330,.T.);
#8816=EDGE_CURVE('',#6630,#6628,#3471,.T.);
#8817=EDGE_CURVE('',#6631,#6629,#3472,.T.);
#8818=EDGE_CURVE('',#6632,#6633,#4331,.T.);
#8819=EDGE_CURVE('',#6632,#6630,#3473,.T.);
#8820=EDGE_CURVE('',#6633,#6631,#3474,.T.);
#8821=EDGE_CURVE('',#6634,#6635,#4332,.T.);
#8822=EDGE_CURVE('',#6634,#6632,#3475,.T.);
#8823=EDGE_CURVE('',#6635,#6633,#3476,.T.);
#8824=EDGE_CURVE('',#6636,#6637,#4333,.T.);
#8825=EDGE_CURVE('',#6636,#6634,#3477,.T.);
#8826=EDGE_CURVE('',#6637,#6635,#3478,.T.);
#8827=EDGE_CURVE('',#6638,#6639,#4334,.T.);
#8828=EDGE_CURVE('',#6638,#6636,#3479,.T.);
#8829=EDGE_CURVE('',#6639,#6637,#3480,.T.);
#8830=EDGE_CURVE('',#6640,#6641,#4335,.T.);
#8831=EDGE_CURVE('',#6640,#6638,#3481,.T.);
#8832=EDGE_CURVE('',#6641,#6639,#3482,.T.);
#8833=EDGE_CURVE('',#6642,#6643,#4336,.T.);
#8834=EDGE_CURVE('',#6642,#6640,#3483,.T.);
#8835=EDGE_CURVE('',#6643,#6641,#3484,.T.);
#8836=EDGE_CURVE('',#6644,#6645,#4337,.T.);
#8837=EDGE_CURVE('',#6644,#6642,#3485,.T.);
#8838=EDGE_CURVE('',#6645,#6643,#3486,.T.);
#8839=EDGE_CURVE('',#6646,#6647,#4338,.T.);
#8840=EDGE_CURVE('',#6646,#6644,#3487,.T.);
#8841=EDGE_CURVE('',#6647,#6645,#3488,.T.);
#8842=EDGE_CURVE('',#6648,#6649,#4339,.T.);
#8843=EDGE_CURVE('',#6648,#6646,#3489,.T.);
#8844=EDGE_CURVE('',#6649,#6647,#3490,.T.);
#8845=EDGE_CURVE('',#6650,#6651,#4340,.T.);
#8846=EDGE_CURVE('',#6650,#6648,#3491,.T.);
#8847=EDGE_CURVE('',#6651,#6649,#3492,.T.);
#8848=EDGE_CURVE('',#6652,#6653,#4341,.T.);
#8849=EDGE_CURVE('',#6652,#6650,#3493,.T.);
#8850=EDGE_CURVE('',#6653,#6651,#3494,.T.);
#8851=EDGE_CURVE('',#6654,#6655,#4342,.T.);
#8852=EDGE_CURVE('',#6654,#6652,#3495,.T.);
#8853=EDGE_CURVE('',#6655,#6653,#3496,.T.);
#8854=EDGE_CURVE('',#6656,#6657,#4343,.T.);
#8855=EDGE_CURVE('',#6656,#6654,#3497,.T.);
#8856=EDGE_CURVE('',#6657,#6655,#3498,.T.);
#8857=EDGE_CURVE('',#6658,#6659,#4344,.T.);
#8858=EDGE_CURVE('',#6658,#6656,#3499,.T.);
#8859=EDGE_CURVE('',#6659,#6657,#3500,.T.);
#8860=EDGE_CURVE('',#6660,#6661,#4345,.T.);
#8861=EDGE_CURVE('',#6660,#6658,#3501,.T.);
#8862=EDGE_CURVE('',#6661,#6659,#3502,.T.);
#8863=EDGE_CURVE('',#6662,#6663,#4346,.T.);
#8864=EDGE_CURVE('',#6662,#6660,#3503,.T.);
#8865=EDGE_CURVE('',#6663,#6661,#3504,.T.);
#8866=EDGE_CURVE('',#6664,#6665,#4347,.T.);
#8867=EDGE_CURVE('',#6664,#6662,#3505,.T.);
#8868=EDGE_CURVE('',#6665,#6663,#3506,.T.);
#8869=EDGE_CURVE('',#6666,#6667,#4348,.T.);
#8870=EDGE_CURVE('',#6666,#6664,#3507,.T.);
#8871=EDGE_CURVE('',#6667,#6665,#3508,.T.);
#8872=EDGE_CURVE('',#6668,#6669,#4349,.T.);
#8873=EDGE_CURVE('',#6668,#6666,#3509,.T.);
#8874=EDGE_CURVE('',#6669,#6667,#3510,.T.);
#8875=EDGE_CURVE('',#6670,#6671,#4350,.T.);
#8876=EDGE_CURVE('',#6670,#6668,#3511,.T.);
#8877=EDGE_CURVE('',#6671,#6669,#3512,.T.);
#8878=EDGE_CURVE('',#6672,#6673,#4351,.T.);
#8879=EDGE_CURVE('',#6672,#6670,#3513,.T.);
#8880=EDGE_CURVE('',#6673,#6671,#3514,.T.);
#8881=EDGE_CURVE('',#6674,#6675,#4352,.T.);
#8882=EDGE_CURVE('',#6674,#6672,#3515,.T.);
#8883=EDGE_CURVE('',#6675,#6673,#3516,.T.);
#8884=EDGE_CURVE('',#6676,#6677,#4353,.T.);
#8885=EDGE_CURVE('',#6676,#6674,#3517,.T.);
#8886=EDGE_CURVE('',#6677,#6675,#3518,.T.);
#8887=EDGE_CURVE('',#6609,#6678,#4354,.T.);
#8888=EDGE_CURVE('',#6679,#6609,#2342,.T.);
#8889=EDGE_CURVE('',#6617,#6679,#3519,.T.);
#8890=EDGE_CURVE('',#6613,#6680,#4355,.T.);
#8891=EDGE_CURVE('',#6680,#6680,#2343,.T.);
#8892=EDGE_CURVE('',#6678,#6614,#3520,.T.);
#8893=EDGE_CURVE('',#6611,#6678,#3521,.T.);
#8894=EDGE_CURVE('',#6681,#6676,#3522,.T.);
#8895=EDGE_CURVE('',#6547,#6681,#3523,.T.);
#8896=EDGE_CURVE('',#6682,#6677,#3524,.T.);
#8897=EDGE_CURVE('',#6681,#6682,#2344,.T.);
#8898=EDGE_CURVE('',#6610,#6679,#3525,.T.);
#8899=EDGE_CURVE('',#6682,#6548,#3526,.T.);
#8900=EDGE_CURVE('',#6683,#6684,#4356,.T.);
#8901=EDGE_CURVE('',#6683,#6685,#4357,.T.);
#8902=EDGE_CURVE('',#6685,#6686,#4358,.T.);
#8903=EDGE_CURVE('',#6684,#6686,#4359,.T.);
#8904=EDGE_CURVE('',#6687,#6683,#4360,.T.);
#8905=EDGE_CURVE('',#6687,#6688,#4361,.T.);
#8906=EDGE_CURVE('',#6688,#6685,#4362,.T.);
#8907=EDGE_CURVE('',#6689,#6687,#4363,.T.);
#8908=EDGE_CURVE('',#6689,#6690,#4364,.T.);
#8909=EDGE_CURVE('',#6690,#6688,#4365,.T.);
#8910=EDGE_CURVE('',#6691,#6689,#4366,.T.);
#8911=EDGE_CURVE('',#6691,#6692,#4367,.T.);
#8912=EDGE_CURVE('',#6692,#6690,#4368,.T.);
#8913=EDGE_CURVE('',#6693,#6691,#4369,.T.);
#8914=EDGE_CURVE('',#6693,#6694,#4370,.T.);
#8915=EDGE_CURVE('',#6694,#6692,#4371,.T.);
#8916=EDGE_CURVE('',#6684,#6693,#4372,.T.);
#8917=EDGE_CURVE('',#6686,#6694,#4373,.T.);
#8918=EDGE_CURVE('',#6695,#6695,#2345,.T.);
#8919=EDGE_CURVE('',#6695,#6696,#4374,.T.);
#8920=EDGE_CURVE('',#6696,#6696,#2346,.T.);
#8921=ORIENTED_EDGE('',*,*,#6697,.T.);
#8922=ORIENTED_EDGE('',*,*,#6698,.T.);
#8923=ORIENTED_EDGE('',*,*,#6699,.T.);
#8924=ORIENTED_EDGE('',*,*,#6700,.T.);
#8925=ORIENTED_EDGE('',*,*,#6701,.F.);
#8926=ORIENTED_EDGE('',*,*,#6700,.F.);
#8927=ORIENTED_EDGE('',*,*,#6702,.T.);
#8928=ORIENTED_EDGE('',*,*,#6703,.T.);
#8929=ORIENTED_EDGE('',*,*,#6704,.T.);
#8930=ORIENTED_EDGE('',*,*,#6705,.T.);
#8931=ORIENTED_EDGE('',*,*,#6697,.F.);
#8932=ORIENTED_EDGE('',*,*,#6706,.T.);
#8933=ORIENTED_EDGE('',*,*,#6707,.T.);
#8934=ORIENTED_EDGE('',*,*,#6708,.T.);
#8935=ORIENTED_EDGE('',*,*,#6704,.F.);
#8936=ORIENTED_EDGE('',*,*,#6709,.T.);
#8937=ORIENTED_EDGE('',*,*,#6710,.T.);
#8938=ORIENTED_EDGE('',*,*,#6711,.T.);
#8939=ORIENTED_EDGE('',*,*,#6707,.F.);
#8940=ORIENTED_EDGE('',*,*,#6712,.T.);
#8941=ORIENTED_EDGE('',*,*,#6713,.T.);
#8942=ORIENTED_EDGE('',*,*,#6714,.T.);
#8943=ORIENTED_EDGE('',*,*,#6710,.F.);
#8944=ORIENTED_EDGE('',*,*,#6715,.T.);
#8945=ORIENTED_EDGE('',*,*,#6716,.T.);
#8946=ORIENTED_EDGE('',*,*,#6717,.T.);
#8947=ORIENTED_EDGE('',*,*,#6713,.F.);
#8948=ORIENTED_EDGE('',*,*,#6718,.T.);
#8949=ORIENTED_EDGE('',*,*,#6719,.T.);
#8950=ORIENTED_EDGE('',*,*,#6720,.T.);
#8951=ORIENTED_EDGE('',*,*,#6716,.F.);
#8952=ORIENTED_EDGE('',*,*,#6721,.T.);
#8953=ORIENTED_EDGE('',*,*,#6722,.T.);
#8954=ORIENTED_EDGE('',*,*,#6723,.T.);
#8955=ORIENTED_EDGE('',*,*,#6719,.F.);
#8956=ORIENTED_EDGE('',*,*,#6724,.T.);
#8957=ORIENTED_EDGE('',*,*,#6725,.F.);
#8958=ORIENTED_EDGE('',*,*,#6726,.T.);
#8959=ORIENTED_EDGE('',*,*,#6727,.F.);
#8960=ORIENTED_EDGE('',*,*,#6728,.T.);
#8961=ORIENTED_EDGE('',*,*,#6729,.T.);
#8962=ORIENTED_EDGE('',*,*,#6730,.T.);
#8963=ORIENTED_EDGE('',*,*,#6731,.F.);
#8964=ORIENTED_EDGE('',*,*,#6732,.F.);
#8965=ORIENTED_EDGE('',*,*,#6733,.T.);
#8966=ORIENTED_EDGE('',*,*,#6734,.T.);
#8967=ORIENTED_EDGE('',*,*,#6729,.F.);
#8968=ORIENTED_EDGE('',*,*,#6735,.F.);
#8969=ORIENTED_EDGE('',*,*,#6736,.T.);
#8970=ORIENTED_EDGE('',*,*,#6737,.T.);
#8971=ORIENTED_EDGE('',*,*,#6733,.F.);
#8972=ORIENTED_EDGE('',*,*,#6738,.F.);
#8973=ORIENTED_EDGE('',*,*,#6739,.T.);
#8974=ORIENTED_EDGE('',*,*,#6740,.T.);
#8975=ORIENTED_EDGE('',*,*,#6736,.F.);
#8976=ORIENTED_EDGE('',*,*,#6741,.F.);
#8977=ORIENTED_EDGE('',*,*,#6742,.T.);
#8978=ORIENTED_EDGE('',*,*,#6743,.T.);
#8979=ORIENTED_EDGE('',*,*,#6739,.F.);
#8980=ORIENTED_EDGE('',*,*,#6744,.F.);
#8981=ORIENTED_EDGE('',*,*,#6745,.T.);
#8982=ORIENTED_EDGE('',*,*,#6746,.T.);
#8983=ORIENTED_EDGE('',*,*,#6742,.F.);
#8984=ORIENTED_EDGE('',*,*,#6747,.F.);
#8985=ORIENTED_EDGE('',*,*,#6748,.T.);
#8986=ORIENTED_EDGE('',*,*,#6749,.T.);
#8987=ORIENTED_EDGE('',*,*,#6745,.F.);
#8988=ORIENTED_EDGE('',*,*,#6750,.F.);
#8989=ORIENTED_EDGE('',*,*,#6751,.T.);
#8990=ORIENTED_EDGE('',*,*,#6752,.T.);
#8991=ORIENTED_EDGE('',*,*,#6748,.F.);
#8992=ORIENTED_EDGE('',*,*,#6753,.F.);
#8993=ORIENTED_EDGE('',*,*,#6754,.F.);
#8994=ORIENTED_EDGE('',*,*,#6755,.F.);
#8995=ORIENTED_EDGE('',*,*,#6756,.F.);
#8996=ORIENTED_EDGE('',*,*,#6757,.T.);
#8997=ORIENTED_EDGE('',*,*,#6758,.T.);
#8998=ORIENTED_EDGE('',*,*,#6759,.T.);
#8999=ORIENTED_EDGE('',*,*,#6760,.T.);
#9000=ORIENTED_EDGE('',*,*,#6761,.T.);
#9001=ORIENTED_EDGE('',*,*,#6762,.F.);
#9002=ORIENTED_EDGE('',*,*,#6761,.F.);
#9003=ORIENTED_EDGE('',*,*,#6763,.T.);
#9004=ORIENTED_EDGE('',*,*,#6764,.T.);
#9005=ORIENTED_EDGE('',*,*,#6765,.T.);
#9006=ORIENTED_EDGE('',*,*,#6766,.T.);
#9007=ORIENTED_EDGE('',*,*,#6758,.F.);
#9008=ORIENTED_EDGE('',*,*,#6767,.T.);
#9009=ORIENTED_EDGE('',*,*,#6768,.T.);
#9010=ORIENTED_EDGE('',*,*,#6769,.T.);
#9011=ORIENTED_EDGE('',*,*,#6765,.F.);
#9012=ORIENTED_EDGE('',*,*,#6770,.T.);
#9013=ORIENTED_EDGE('',*,*,#6771,.T.);
#9014=ORIENTED_EDGE('',*,*,#6772,.T.);
#9015=ORIENTED_EDGE('',*,*,#6768,.F.);
#9016=ORIENTED_EDGE('',*,*,#6773,.T.);
#9017=ORIENTED_EDGE('',*,*,#6774,.T.);
#9018=ORIENTED_EDGE('',*,*,#6775,.T.);
#9019=ORIENTED_EDGE('',*,*,#6771,.F.);
#9020=ORIENTED_EDGE('',*,*,#6776,.T.);
#9021=ORIENTED_EDGE('',*,*,#6777,.T.);
#9022=ORIENTED_EDGE('',*,*,#6778,.T.);
#9023=ORIENTED_EDGE('',*,*,#6774,.F.);
#9024=ORIENTED_EDGE('',*,*,#6779,.T.);
#9025=ORIENTED_EDGE('',*,*,#6780,.T.);
#9026=ORIENTED_EDGE('',*,*,#6781,.T.);
#9027=ORIENTED_EDGE('',*,*,#6777,.F.);
#9028=ORIENTED_EDGE('',*,*,#6782,.T.);
#9029=ORIENTED_EDGE('',*,*,#6783,.T.);
#9030=ORIENTED_EDGE('',*,*,#6784,.T.);
#9031=ORIENTED_EDGE('',*,*,#6780,.F.);
#9032=ORIENTED_EDGE('',*,*,#6785,.T.);
#9033=ORIENTED_EDGE('',*,*,#6786,.F.);
#9034=ORIENTED_EDGE('',*,*,#6787,.T.);
#9035=ORIENTED_EDGE('',*,*,#6788,.F.);
#9036=ORIENTED_EDGE('',*,*,#6789,.T.);
#9037=ORIENTED_EDGE('',*,*,#6790,.T.);
#9038=ORIENTED_EDGE('',*,*,#6791,.T.);
#9039=ORIENTED_EDGE('',*,*,#6792,.F.);
#9040=ORIENTED_EDGE('',*,*,#6793,.F.);
#9041=ORIENTED_EDGE('',*,*,#6794,.T.);
#9042=ORIENTED_EDGE('',*,*,#6795,.T.);
#9043=ORIENTED_EDGE('',*,*,#6790,.F.);
#9044=ORIENTED_EDGE('',*,*,#6796,.F.);
#9045=ORIENTED_EDGE('',*,*,#6797,.T.);
#9046=ORIENTED_EDGE('',*,*,#6798,.T.);
#9047=ORIENTED_EDGE('',*,*,#6794,.F.);
#9048=ORIENTED_EDGE('',*,*,#6799,.F.);
#9049=ORIENTED_EDGE('',*,*,#6800,.T.);
#9050=ORIENTED_EDGE('',*,*,#6801,.T.);
#9051=ORIENTED_EDGE('',*,*,#6797,.F.);
#9052=ORIENTED_EDGE('',*,*,#6802,.F.);
#9053=ORIENTED_EDGE('',*,*,#6803,.T.);
#9054=ORIENTED_EDGE('',*,*,#6804,.T.);
#9055=ORIENTED_EDGE('',*,*,#6800,.F.);
#9056=ORIENTED_EDGE('',*,*,#6805,.F.);
#9057=ORIENTED_EDGE('',*,*,#6806,.T.);
#9058=ORIENTED_EDGE('',*,*,#6807,.T.);
#9059=ORIENTED_EDGE('',*,*,#6803,.F.);
#9060=ORIENTED_EDGE('',*,*,#6808,.F.);
#9061=ORIENTED_EDGE('',*,*,#6809,.T.);
#9062=ORIENTED_EDGE('',*,*,#6810,.T.);
#9063=ORIENTED_EDGE('',*,*,#6806,.F.);
#9064=ORIENTED_EDGE('',*,*,#6811,.F.);
#9065=ORIENTED_EDGE('',*,*,#6812,.T.);
#9066=ORIENTED_EDGE('',*,*,#6813,.T.);
#9067=ORIENTED_EDGE('',*,*,#6809,.F.);
#9068=ORIENTED_EDGE('',*,*,#6814,.F.);
#9069=ORIENTED_EDGE('',*,*,#6815,.F.);
#9070=ORIENTED_EDGE('',*,*,#6816,.F.);
#9071=ORIENTED_EDGE('',*,*,#6817,.F.);
#9072=ORIENTED_EDGE('',*,*,#6818,.T.);
#9073=ORIENTED_EDGE('',*,*,#6819,.T.);
#9074=ORIENTED_EDGE('',*,*,#6820,.T.);
#9075=ORIENTED_EDGE('',*,*,#6821,.T.);
#9076=ORIENTED_EDGE('',*,*,#6822,.T.);
#9077=ORIENTED_EDGE('',*,*,#6823,.F.);
#9078=ORIENTED_EDGE('',*,*,#6822,.F.);
#9079=ORIENTED_EDGE('',*,*,#6824,.T.);
#9080=ORIENTED_EDGE('',*,*,#6825,.T.);
#9081=ORIENTED_EDGE('',*,*,#6826,.T.);
#9082=ORIENTED_EDGE('',*,*,#6827,.T.);
#9083=ORIENTED_EDGE('',*,*,#6819,.F.);
#9084=ORIENTED_EDGE('',*,*,#6828,.T.);
#9085=ORIENTED_EDGE('',*,*,#6829,.T.);
#9086=ORIENTED_EDGE('',*,*,#6830,.T.);
#9087=ORIENTED_EDGE('',*,*,#6826,.F.);
#9088=ORIENTED_EDGE('',*,*,#6831,.T.);
#9089=ORIENTED_EDGE('',*,*,#6832,.T.);
#9090=ORIENTED_EDGE('',*,*,#6833,.T.);
#9091=ORIENTED_EDGE('',*,*,#6829,.F.);
#9092=ORIENTED_EDGE('',*,*,#6834,.T.);
#9093=ORIENTED_EDGE('',*,*,#6835,.T.);
#9094=ORIENTED_EDGE('',*,*,#6836,.T.);
#9095=ORIENTED_EDGE('',*,*,#6832,.F.);
#9096=ORIENTED_EDGE('',*,*,#6837,.T.);
#9097=ORIENTED_EDGE('',*,*,#6838,.T.);
#9098=ORIENTED_EDGE('',*,*,#6839,.T.);
#9099=ORIENTED_EDGE('',*,*,#6835,.F.);
#9100=ORIENTED_EDGE('',*,*,#6840,.T.);
#9101=ORIENTED_EDGE('',*,*,#6841,.T.);
#9102=ORIENTED_EDGE('',*,*,#6842,.T.);
#9103=ORIENTED_EDGE('',*,*,#6838,.F.);
#9104=ORIENTED_EDGE('',*,*,#6843,.T.);
#9105=ORIENTED_EDGE('',*,*,#6844,.T.);
#9106=ORIENTED_EDGE('',*,*,#6845,.T.);
#9107=ORIENTED_EDGE('',*,*,#6841,.F.);
#9108=ORIENTED_EDGE('',*,*,#6846,.T.);
#9109=ORIENTED_EDGE('',*,*,#6847,.F.);
#9110=ORIENTED_EDGE('',*,*,#6848,.T.);
#9111=ORIENTED_EDGE('',*,*,#6849,.F.);
#9112=ORIENTED_EDGE('',*,*,#6850,.T.);
#9113=ORIENTED_EDGE('',*,*,#6851,.T.);
#9114=ORIENTED_EDGE('',*,*,#6852,.T.);
#9115=ORIENTED_EDGE('',*,*,#6853,.F.);
#9116=ORIENTED_EDGE('',*,*,#6854,.F.);
#9117=ORIENTED_EDGE('',*,*,#6855,.T.);
#9118=ORIENTED_EDGE('',*,*,#6856,.T.);
#9119=ORIENTED_EDGE('',*,*,#6851,.F.);
#9120=ORIENTED_EDGE('',*,*,#6857,.F.);
#9121=ORIENTED_EDGE('',*,*,#6858,.T.);
#9122=ORIENTED_EDGE('',*,*,#6859,.T.);
#9123=ORIENTED_EDGE('',*,*,#6855,.F.);
#9124=ORIENTED_EDGE('',*,*,#6860,.F.);
#9125=ORIENTED_EDGE('',*,*,#6861,.T.);
#9126=ORIENTED_EDGE('',*,*,#6862,.T.);
#9127=ORIENTED_EDGE('',*,*,#6858,.F.);
#9128=ORIENTED_EDGE('',*,*,#6863,.F.);
#9129=ORIENTED_EDGE('',*,*,#6864,.T.);
#9130=ORIENTED_EDGE('',*,*,#6865,.T.);
#9131=ORIENTED_EDGE('',*,*,#6861,.F.);
#9132=ORIENTED_EDGE('',*,*,#6866,.F.);
#9133=ORIENTED_EDGE('',*,*,#6867,.T.);
#9134=ORIENTED_EDGE('',*,*,#6868,.T.);
#9135=ORIENTED_EDGE('',*,*,#6864,.F.);
#9136=ORIENTED_EDGE('',*,*,#6869,.F.);
#9137=ORIENTED_EDGE('',*,*,#6870,.T.);
#9138=ORIENTED_EDGE('',*,*,#6871,.T.);
#9139=ORIENTED_EDGE('',*,*,#6867,.F.);
#9140=ORIENTED_EDGE('',*,*,#6872,.F.);
#9141=ORIENTED_EDGE('',*,*,#6873,.T.);
#9142=ORIENTED_EDGE('',*,*,#6874,.T.);
#9143=ORIENTED_EDGE('',*,*,#6870,.F.);
#9144=ORIENTED_EDGE('',*,*,#6875,.F.);
#9145=ORIENTED_EDGE('',*,*,#6876,.F.);
#9146=ORIENTED_EDGE('',*,*,#6877,.F.);
#9147=ORIENTED_EDGE('',*,*,#6878,.F.);
#9148=ORIENTED_EDGE('',*,*,#6879,.T.);
#9149=ORIENTED_EDGE('',*,*,#6880,.T.);
#9150=ORIENTED_EDGE('',*,*,#6881,.T.);
#9151=ORIENTED_EDGE('',*,*,#6882,.T.);
#9152=ORIENTED_EDGE('',*,*,#6883,.T.);
#9153=ORIENTED_EDGE('',*,*,#6884,.F.);
#9154=ORIENTED_EDGE('',*,*,#6883,.F.);
#9155=ORIENTED_EDGE('',*,*,#6885,.T.);
#9156=ORIENTED_EDGE('',*,*,#6886,.T.);
#9157=ORIENTED_EDGE('',*,*,#6887,.T.);
#9158=ORIENTED_EDGE('',*,*,#6888,.T.);
#9159=ORIENTED_EDGE('',*,*,#6880,.F.);
#9160=ORIENTED_EDGE('',*,*,#6889,.T.);
#9161=ORIENTED_EDGE('',*,*,#6890,.T.);
#9162=ORIENTED_EDGE('',*,*,#6891,.T.);
#9163=ORIENTED_EDGE('',*,*,#6887,.F.);
#9164=ORIENTED_EDGE('',*,*,#6892,.T.);
#9165=ORIENTED_EDGE('',*,*,#6893,.T.);
#9166=ORIENTED_EDGE('',*,*,#6894,.T.);
#9167=ORIENTED_EDGE('',*,*,#6890,.F.);
#9168=ORIENTED_EDGE('',*,*,#6895,.T.);
#9169=ORIENTED_EDGE('',*,*,#6896,.T.);
#9170=ORIENTED_EDGE('',*,*,#6897,.T.);
#9171=ORIENTED_EDGE('',*,*,#6893,.F.);
#9172=ORIENTED_EDGE('',*,*,#6898,.T.);
#9173=ORIENTED_EDGE('',*,*,#6899,.T.);
#9174=ORIENTED_EDGE('',*,*,#6900,.T.);
#9175=ORIENTED_EDGE('',*,*,#6896,.F.);
#9176=ORIENTED_EDGE('',*,*,#6901,.T.);
#9177=ORIENTED_EDGE('',*,*,#6902,.T.);
#9178=ORIENTED_EDGE('',*,*,#6903,.T.);
#9179=ORIENTED_EDGE('',*,*,#6899,.F.);
#9180=ORIENTED_EDGE('',*,*,#6904,.T.);
#9181=ORIENTED_EDGE('',*,*,#6905,.T.);
#9182=ORIENTED_EDGE('',*,*,#6906,.T.);
#9183=ORIENTED_EDGE('',*,*,#6902,.F.);
#9184=ORIENTED_EDGE('',*,*,#6907,.T.);
#9185=ORIENTED_EDGE('',*,*,#6908,.F.);
#9186=ORIENTED_EDGE('',*,*,#6909,.T.);
#9187=ORIENTED_EDGE('',*,*,#6910,.F.);
#9188=ORIENTED_EDGE('',*,*,#6911,.T.);
#9189=ORIENTED_EDGE('',*,*,#6912,.T.);
#9190=ORIENTED_EDGE('',*,*,#6913,.T.);
#9191=ORIENTED_EDGE('',*,*,#6914,.F.);
#9192=ORIENTED_EDGE('',*,*,#6915,.F.);
#9193=ORIENTED_EDGE('',*,*,#6916,.T.);
#9194=ORIENTED_EDGE('',*,*,#6917,.T.);
#9195=ORIENTED_EDGE('',*,*,#6912,.F.);
#9196=ORIENTED_EDGE('',*,*,#6918,.F.);
#9197=ORIENTED_EDGE('',*,*,#6919,.T.);
#9198=ORIENTED_EDGE('',*,*,#6920,.T.);
#9199=ORIENTED_EDGE('',*,*,#6916,.F.);
#9200=ORIENTED_EDGE('',*,*,#6921,.F.);
#9201=ORIENTED_EDGE('',*,*,#6922,.T.);
#9202=ORIENTED_EDGE('',*,*,#6923,.T.);
#9203=ORIENTED_EDGE('',*,*,#6919,.F.);
#9204=ORIENTED_EDGE('',*,*,#6924,.F.);
#9205=ORIENTED_EDGE('',*,*,#6925,.T.);
#9206=ORIENTED_EDGE('',*,*,#6926,.T.);
#9207=ORIENTED_EDGE('',*,*,#6922,.F.);
#9208=ORIENTED_EDGE('',*,*,#6927,.F.);
#9209=ORIENTED_EDGE('',*,*,#6928,.T.);
#9210=ORIENTED_EDGE('',*,*,#6929,.T.);
#9211=ORIENTED_EDGE('',*,*,#6925,.F.);
#9212=ORIENTED_EDGE('',*,*,#6930,.F.);
#9213=ORIENTED_EDGE('',*,*,#6931,.T.);
#9214=ORIENTED_EDGE('',*,*,#6932,.T.);
#9215=ORIENTED_EDGE('',*,*,#6928,.F.);
#9216=ORIENTED_EDGE('',*,*,#6933,.F.);
#9217=ORIENTED_EDGE('',*,*,#6934,.T.);
#9218=ORIENTED_EDGE('',*,*,#6935,.T.);
#9219=ORIENTED_EDGE('',*,*,#6931,.F.);
#9220=ORIENTED_EDGE('',*,*,#6936,.F.);
#9221=ORIENTED_EDGE('',*,*,#6937,.F.);
#9222=ORIENTED_EDGE('',*,*,#6938,.F.);
#9223=ORIENTED_EDGE('',*,*,#6939,.F.);
#9224=ORIENTED_EDGE('',*,*,#6940,.T.);
#9225=ORIENTED_EDGE('',*,*,#6941,.T.);
#9226=ORIENTED_EDGE('',*,*,#6942,.T.);
#9227=ORIENTED_EDGE('',*,*,#6943,.T.);
#9228=ORIENTED_EDGE('',*,*,#6944,.T.);
#9229=ORIENTED_EDGE('',*,*,#6945,.F.);
#9230=ORIENTED_EDGE('',*,*,#6944,.F.);
#9231=ORIENTED_EDGE('',*,*,#6946,.T.);
#9232=ORIENTED_EDGE('',*,*,#6947,.T.);
#9233=ORIENTED_EDGE('',*,*,#6948,.T.);
#9234=ORIENTED_EDGE('',*,*,#6949,.T.);
#9235=ORIENTED_EDGE('',*,*,#6941,.F.);
#9236=ORIENTED_EDGE('',*,*,#6950,.T.);
#9237=ORIENTED_EDGE('',*,*,#6951,.T.);
#9238=ORIENTED_EDGE('',*,*,#6952,.T.);
#9239=ORIENTED_EDGE('',*,*,#6948,.F.);
#9240=ORIENTED_EDGE('',*,*,#6953,.T.);
#9241=ORIENTED_EDGE('',*,*,#6954,.T.);
#9242=ORIENTED_EDGE('',*,*,#6955,.T.);
#9243=ORIENTED_EDGE('',*,*,#6951,.F.);
#9244=ORIENTED_EDGE('',*,*,#6956,.T.);
#9245=ORIENTED_EDGE('',*,*,#6957,.T.);
#9246=ORIENTED_EDGE('',*,*,#6958,.T.);
#9247=ORIENTED_EDGE('',*,*,#6954,.F.);
#9248=ORIENTED_EDGE('',*,*,#6959,.T.);
#9249=ORIENTED_EDGE('',*,*,#6960,.T.);
#9250=ORIENTED_EDGE('',*,*,#6961,.T.);
#9251=ORIENTED_EDGE('',*,*,#6957,.F.);
#9252=ORIENTED_EDGE('',*,*,#6962,.T.);
#9253=ORIENTED_EDGE('',*,*,#6963,.T.);
#9254=ORIENTED_EDGE('',*,*,#6964,.T.);
#9255=ORIENTED_EDGE('',*,*,#6960,.F.);
#9256=ORIENTED_EDGE('',*,*,#6965,.T.);
#9257=ORIENTED_EDGE('',*,*,#6966,.T.);
#9258=ORIENTED_EDGE('',*,*,#6967,.T.);
#9259=ORIENTED_EDGE('',*,*,#6963,.F.);
#9260=ORIENTED_EDGE('',*,*,#6968,.T.);
#9261=ORIENTED_EDGE('',*,*,#6969,.F.);
#9262=ORIENTED_EDGE('',*,*,#6970,.T.);
#9263=ORIENTED_EDGE('',*,*,#6971,.F.);
#9264=ORIENTED_EDGE('',*,*,#6972,.T.);
#9265=ORIENTED_EDGE('',*,*,#6973,.T.);
#9266=ORIENTED_EDGE('',*,*,#6974,.T.);
#9267=ORIENTED_EDGE('',*,*,#6975,.F.);
#9268=ORIENTED_EDGE('',*,*,#6976,.F.);
#9269=ORIENTED_EDGE('',*,*,#6977,.T.);
#9270=ORIENTED_EDGE('',*,*,#6978,.T.);
#9271=ORIENTED_EDGE('',*,*,#6973,.F.);
#9272=ORIENTED_EDGE('',*,*,#6979,.F.);
#9273=ORIENTED_EDGE('',*,*,#6980,.T.);
#9274=ORIENTED_EDGE('',*,*,#6981,.T.);
#9275=ORIENTED_EDGE('',*,*,#6977,.F.);
#9276=ORIENTED_EDGE('',*,*,#6982,.F.);
#9277=ORIENTED_EDGE('',*,*,#6983,.T.);
#9278=ORIENTED_EDGE('',*,*,#6984,.T.);
#9279=ORIENTED_EDGE('',*,*,#6980,.F.);
#9280=ORIENTED_EDGE('',*,*,#6985,.F.);
#9281=ORIENTED_EDGE('',*,*,#6986,.T.);
#9282=ORIENTED_EDGE('',*,*,#6987,.T.);
#9283=ORIENTED_EDGE('',*,*,#6983,.F.);
#9284=ORIENTED_EDGE('',*,*,#6988,.F.);
#9285=ORIENTED_EDGE('',*,*,#6989,.T.);
#9286=ORIENTED_EDGE('',*,*,#6990,.T.);
#9287=ORIENTED_EDGE('',*,*,#6986,.F.);
#9288=ORIENTED_EDGE('',*,*,#6991,.F.);
#9289=ORIENTED_EDGE('',*,*,#6992,.T.);
#9290=ORIENTED_EDGE('',*,*,#6993,.T.);
#9291=ORIENTED_EDGE('',*,*,#6989,.F.);
#9292=ORIENTED_EDGE('',*,*,#6994,.F.);
#9293=ORIENTED_EDGE('',*,*,#6995,.T.);
#9294=ORIENTED_EDGE('',*,*,#6996,.T.);
#9295=ORIENTED_EDGE('',*,*,#6992,.F.);
#9296=ORIENTED_EDGE('',*,*,#6997,.F.);
#9297=ORIENTED_EDGE('',*,*,#6998,.F.);
#9298=ORIENTED_EDGE('',*,*,#6999,.F.);
#9299=ORIENTED_EDGE('',*,*,#7000,.F.);
#9300=ORIENTED_EDGE('',*,*,#7001,.T.);
#9301=ORIENTED_EDGE('',*,*,#7002,.T.);
#9302=ORIENTED_EDGE('',*,*,#7003,.T.);
#9303=ORIENTED_EDGE('',*,*,#7004,.T.);
#9304=ORIENTED_EDGE('',*,*,#7005,.T.);
#9305=ORIENTED_EDGE('',*,*,#7006,.F.);
#9306=ORIENTED_EDGE('',*,*,#7005,.F.);
#9307=ORIENTED_EDGE('',*,*,#7007,.T.);
#9308=ORIENTED_EDGE('',*,*,#7008,.T.);
#9309=ORIENTED_EDGE('',*,*,#7009,.T.);
#9310=ORIENTED_EDGE('',*,*,#7010,.T.);
#9311=ORIENTED_EDGE('',*,*,#7002,.F.);
#9312=ORIENTED_EDGE('',*,*,#7011,.T.);
#9313=ORIENTED_EDGE('',*,*,#7012,.T.);
#9314=ORIENTED_EDGE('',*,*,#7013,.T.);
#9315=ORIENTED_EDGE('',*,*,#7009,.F.);
#9316=ORIENTED_EDGE('',*,*,#7014,.T.);
#9317=ORIENTED_EDGE('',*,*,#7015,.T.);
#9318=ORIENTED_EDGE('',*,*,#7016,.T.);
#9319=ORIENTED_EDGE('',*,*,#7012,.F.);
#9320=ORIENTED_EDGE('',*,*,#7017,.T.);
#9321=ORIENTED_EDGE('',*,*,#7018,.T.);
#9322=ORIENTED_EDGE('',*,*,#7019,.T.);
#9323=ORIENTED_EDGE('',*,*,#7015,.F.);
#9324=ORIENTED_EDGE('',*,*,#7020,.T.);
#9325=ORIENTED_EDGE('',*,*,#7021,.T.);
#9326=ORIENTED_EDGE('',*,*,#7022,.T.);
#9327=ORIENTED_EDGE('',*,*,#7018,.F.);
#9328=ORIENTED_EDGE('',*,*,#7023,.T.);
#9329=ORIENTED_EDGE('',*,*,#7024,.T.);
#9330=ORIENTED_EDGE('',*,*,#7025,.T.);
#9331=ORIENTED_EDGE('',*,*,#7021,.F.);
#9332=ORIENTED_EDGE('',*,*,#7026,.T.);
#9333=ORIENTED_EDGE('',*,*,#7027,.T.);
#9334=ORIENTED_EDGE('',*,*,#7028,.T.);
#9335=ORIENTED_EDGE('',*,*,#7024,.F.);
#9336=ORIENTED_EDGE('',*,*,#7029,.T.);
#9337=ORIENTED_EDGE('',*,*,#7030,.F.);
#9338=ORIENTED_EDGE('',*,*,#7031,.T.);
#9339=ORIENTED_EDGE('',*,*,#7032,.F.);
#9340=ORIENTED_EDGE('',*,*,#7033,.T.);
#9341=ORIENTED_EDGE('',*,*,#7034,.T.);
#9342=ORIENTED_EDGE('',*,*,#7035,.T.);
#9343=ORIENTED_EDGE('',*,*,#7036,.F.);
#9344=ORIENTED_EDGE('',*,*,#7037,.F.);
#9345=ORIENTED_EDGE('',*,*,#7038,.T.);
#9346=ORIENTED_EDGE('',*,*,#7039,.T.);
#9347=ORIENTED_EDGE('',*,*,#7034,.F.);
#9348=ORIENTED_EDGE('',*,*,#7040,.F.);
#9349=ORIENTED_EDGE('',*,*,#7041,.T.);
#9350=ORIENTED_EDGE('',*,*,#7042,.T.);
#9351=ORIENTED_EDGE('',*,*,#7038,.F.);
#9352=ORIENTED_EDGE('',*,*,#7043,.F.);
#9353=ORIENTED_EDGE('',*,*,#7044,.T.);
#9354=ORIENTED_EDGE('',*,*,#7045,.T.);
#9355=ORIENTED_EDGE('',*,*,#7041,.F.);
#9356=ORIENTED_EDGE('',*,*,#7046,.F.);
#9357=ORIENTED_EDGE('',*,*,#7047,.T.);
#9358=ORIENTED_EDGE('',*,*,#7048,.T.);
#9359=ORIENTED_EDGE('',*,*,#7044,.F.);
#9360=ORIENTED_EDGE('',*,*,#7049,.F.);
#9361=ORIENTED_EDGE('',*,*,#7050,.T.);
#9362=ORIENTED_EDGE('',*,*,#7051,.T.);
#9363=ORIENTED_EDGE('',*,*,#7047,.F.);
#9364=ORIENTED_EDGE('',*,*,#7052,.F.);
#9365=ORIENTED_EDGE('',*,*,#7053,.T.);
#9366=ORIENTED_EDGE('',*,*,#7054,.T.);
#9367=ORIENTED_EDGE('',*,*,#7050,.F.);
#9368=ORIENTED_EDGE('',*,*,#7055,.F.);
#9369=ORIENTED_EDGE('',*,*,#7056,.T.);
#9370=ORIENTED_EDGE('',*,*,#7057,.T.);
#9371=ORIENTED_EDGE('',*,*,#7053,.F.);
#9372=ORIENTED_EDGE('',*,*,#7058,.F.);
#9373=ORIENTED_EDGE('',*,*,#7059,.F.);
#9374=ORIENTED_EDGE('',*,*,#7060,.F.);
#9375=ORIENTED_EDGE('',*,*,#7061,.F.);
#9376=ORIENTED_EDGE('',*,*,#7062,.T.);
#9377=ORIENTED_EDGE('',*,*,#7063,.T.);
#9378=ORIENTED_EDGE('',*,*,#7064,.T.);
#9379=ORIENTED_EDGE('',*,*,#7065,.T.);
#9380=ORIENTED_EDGE('',*,*,#7066,.T.);
#9381=ORIENTED_EDGE('',*,*,#7067,.F.);
#9382=ORIENTED_EDGE('',*,*,#7066,.F.);
#9383=ORIENTED_EDGE('',*,*,#7068,.T.);
#9384=ORIENTED_EDGE('',*,*,#7069,.T.);
#9385=ORIENTED_EDGE('',*,*,#7070,.T.);
#9386=ORIENTED_EDGE('',*,*,#7071,.T.);
#9387=ORIENTED_EDGE('',*,*,#7063,.F.);
#9388=ORIENTED_EDGE('',*,*,#7072,.T.);
#9389=ORIENTED_EDGE('',*,*,#7073,.T.);
#9390=ORIENTED_EDGE('',*,*,#7074,.T.);
#9391=ORIENTED_EDGE('',*,*,#7070,.F.);
#9392=ORIENTED_EDGE('',*,*,#7075,.T.);
#9393=ORIENTED_EDGE('',*,*,#7076,.T.);
#9394=ORIENTED_EDGE('',*,*,#7077,.T.);
#9395=ORIENTED_EDGE('',*,*,#7073,.F.);
#9396=ORIENTED_EDGE('',*,*,#7078,.T.);
#9397=ORIENTED_EDGE('',*,*,#7079,.T.);
#9398=ORIENTED_EDGE('',*,*,#7080,.T.);
#9399=ORIENTED_EDGE('',*,*,#7076,.F.);
#9400=ORIENTED_EDGE('',*,*,#7081,.T.);
#9401=ORIENTED_EDGE('',*,*,#7082,.T.);
#9402=ORIENTED_EDGE('',*,*,#7083,.T.);
#9403=ORIENTED_EDGE('',*,*,#7079,.F.);
#9404=ORIENTED_EDGE('',*,*,#7084,.T.);
#9405=ORIENTED_EDGE('',*,*,#7085,.T.);
#9406=ORIENTED_EDGE('',*,*,#7086,.T.);
#9407=ORIENTED_EDGE('',*,*,#7082,.F.);
#9408=ORIENTED_EDGE('',*,*,#7087,.T.);
#9409=ORIENTED_EDGE('',*,*,#7088,.T.);
#9410=ORIENTED_EDGE('',*,*,#7089,.T.);
#9411=ORIENTED_EDGE('',*,*,#7085,.F.);
#9412=ORIENTED_EDGE('',*,*,#7090,.T.);
#9413=ORIENTED_EDGE('',*,*,#7091,.F.);
#9414=ORIENTED_EDGE('',*,*,#7092,.T.);
#9415=ORIENTED_EDGE('',*,*,#7093,.F.);
#9416=ORIENTED_EDGE('',*,*,#7094,.T.);
#9417=ORIENTED_EDGE('',*,*,#7095,.T.);
#9418=ORIENTED_EDGE('',*,*,#7096,.T.);
#9419=ORIENTED_EDGE('',*,*,#7097,.F.);
#9420=ORIENTED_EDGE('',*,*,#7098,.F.);
#9421=ORIENTED_EDGE('',*,*,#7099,.T.);
#9422=ORIENTED_EDGE('',*,*,#7100,.T.);
#9423=ORIENTED_EDGE('',*,*,#7095,.F.);
#9424=ORIENTED_EDGE('',*,*,#7101,.F.);
#9425=ORIENTED_EDGE('',*,*,#7102,.T.);
#9426=ORIENTED_EDGE('',*,*,#7103,.T.);
#9427=ORIENTED_EDGE('',*,*,#7099,.F.);
#9428=ORIENTED_EDGE('',*,*,#7104,.F.);
#9429=ORIENTED_EDGE('',*,*,#7105,.T.);
#9430=ORIENTED_EDGE('',*,*,#7106,.T.);
#9431=ORIENTED_EDGE('',*,*,#7102,.F.);
#9432=ORIENTED_EDGE('',*,*,#7107,.F.);
#9433=ORIENTED_EDGE('',*,*,#7108,.T.);
#9434=ORIENTED_EDGE('',*,*,#7109,.T.);
#9435=ORIENTED_EDGE('',*,*,#7105,.F.);
#9436=ORIENTED_EDGE('',*,*,#7110,.F.);
#9437=ORIENTED_EDGE('',*,*,#7111,.T.);
#9438=ORIENTED_EDGE('',*,*,#7112,.T.);
#9439=ORIENTED_EDGE('',*,*,#7108,.F.);
#9440=ORIENTED_EDGE('',*,*,#7113,.F.);
#9441=ORIENTED_EDGE('',*,*,#7114,.T.);
#9442=ORIENTED_EDGE('',*,*,#7115,.T.);
#9443=ORIENTED_EDGE('',*,*,#7111,.F.);
#9444=ORIENTED_EDGE('',*,*,#7116,.F.);
#9445=ORIENTED_EDGE('',*,*,#7117,.T.);
#9446=ORIENTED_EDGE('',*,*,#7118,.T.);
#9447=ORIENTED_EDGE('',*,*,#7114,.F.);
#9448=ORIENTED_EDGE('',*,*,#7119,.F.);
#9449=ORIENTED_EDGE('',*,*,#7120,.F.);
#9450=ORIENTED_EDGE('',*,*,#7121,.F.);
#9451=ORIENTED_EDGE('',*,*,#7122,.F.);
#9452=ORIENTED_EDGE('',*,*,#7123,.T.);
#9453=ORIENTED_EDGE('',*,*,#7124,.T.);
#9454=ORIENTED_EDGE('',*,*,#7125,.T.);
#9455=ORIENTED_EDGE('',*,*,#7126,.T.);
#9456=ORIENTED_EDGE('',*,*,#7127,.T.);
#9457=ORIENTED_EDGE('',*,*,#7128,.F.);
#9458=ORIENTED_EDGE('',*,*,#7127,.F.);
#9459=ORIENTED_EDGE('',*,*,#7129,.T.);
#9460=ORIENTED_EDGE('',*,*,#7130,.T.);
#9461=ORIENTED_EDGE('',*,*,#7131,.T.);
#9462=ORIENTED_EDGE('',*,*,#7132,.T.);
#9463=ORIENTED_EDGE('',*,*,#7124,.F.);
#9464=ORIENTED_EDGE('',*,*,#7133,.T.);
#9465=ORIENTED_EDGE('',*,*,#7134,.T.);
#9466=ORIENTED_EDGE('',*,*,#7135,.T.);
#9467=ORIENTED_EDGE('',*,*,#7131,.F.);
#9468=ORIENTED_EDGE('',*,*,#7136,.T.);
#9469=ORIENTED_EDGE('',*,*,#7137,.T.);
#9470=ORIENTED_EDGE('',*,*,#7138,.T.);
#9471=ORIENTED_EDGE('',*,*,#7134,.F.);
#9472=ORIENTED_EDGE('',*,*,#7139,.T.);
#9473=ORIENTED_EDGE('',*,*,#7140,.T.);
#9474=ORIENTED_EDGE('',*,*,#7141,.T.);
#9475=ORIENTED_EDGE('',*,*,#7137,.F.);
#9476=ORIENTED_EDGE('',*,*,#7142,.T.);
#9477=ORIENTED_EDGE('',*,*,#7143,.T.);
#9478=ORIENTED_EDGE('',*,*,#7144,.T.);
#9479=ORIENTED_EDGE('',*,*,#7140,.F.);
#9480=ORIENTED_EDGE('',*,*,#7145,.T.);
#9481=ORIENTED_EDGE('',*,*,#7146,.T.);
#9482=ORIENTED_EDGE('',*,*,#7147,.T.);
#9483=ORIENTED_EDGE('',*,*,#7143,.F.);
#9484=ORIENTED_EDGE('',*,*,#7148,.T.);
#9485=ORIENTED_EDGE('',*,*,#7149,.T.);
#9486=ORIENTED_EDGE('',*,*,#7150,.T.);
#9487=ORIENTED_EDGE('',*,*,#7146,.F.);
#9488=ORIENTED_EDGE('',*,*,#7151,.T.);
#9489=ORIENTED_EDGE('',*,*,#7152,.F.);
#9490=ORIENTED_EDGE('',*,*,#7153,.T.);
#9491=ORIENTED_EDGE('',*,*,#7154,.F.);
#9492=ORIENTED_EDGE('',*,*,#7155,.T.);
#9493=ORIENTED_EDGE('',*,*,#7156,.T.);
#9494=ORIENTED_EDGE('',*,*,#7157,.T.);
#9495=ORIENTED_EDGE('',*,*,#7158,.F.);
#9496=ORIENTED_EDGE('',*,*,#7159,.F.);
#9497=ORIENTED_EDGE('',*,*,#7160,.T.);
#9498=ORIENTED_EDGE('',*,*,#7161,.T.);
#9499=ORIENTED_EDGE('',*,*,#7156,.F.);
#9500=ORIENTED_EDGE('',*,*,#7162,.F.);
#9501=ORIENTED_EDGE('',*,*,#7163,.T.);
#9502=ORIENTED_EDGE('',*,*,#7164,.T.);
#9503=ORIENTED_EDGE('',*,*,#7160,.F.);
#9504=ORIENTED_EDGE('',*,*,#7165,.F.);
#9505=ORIENTED_EDGE('',*,*,#7166,.T.);
#9506=ORIENTED_EDGE('',*,*,#7167,.T.);
#9507=ORIENTED_EDGE('',*,*,#7163,.F.);
#9508=ORIENTED_EDGE('',*,*,#7168,.F.);
#9509=ORIENTED_EDGE('',*,*,#7169,.T.);
#9510=ORIENTED_EDGE('',*,*,#7170,.T.);
#9511=ORIENTED_EDGE('',*,*,#7166,.F.);
#9512=ORIENTED_EDGE('',*,*,#7171,.F.);
#9513=ORIENTED_EDGE('',*,*,#7172,.T.);
#9514=ORIENTED_EDGE('',*,*,#7173,.T.);
#9515=ORIENTED_EDGE('',*,*,#7169,.F.);
#9516=ORIENTED_EDGE('',*,*,#7174,.F.);
#9517=ORIENTED_EDGE('',*,*,#7175,.T.);
#9518=ORIENTED_EDGE('',*,*,#7176,.T.);
#9519=ORIENTED_EDGE('',*,*,#7172,.F.);
#9520=ORIENTED_EDGE('',*,*,#7177,.F.);
#9521=ORIENTED_EDGE('',*,*,#7178,.T.);
#9522=ORIENTED_EDGE('',*,*,#7179,.T.);
#9523=ORIENTED_EDGE('',*,*,#7175,.F.);
#9524=ORIENTED_EDGE('',*,*,#7180,.F.);
#9525=ORIENTED_EDGE('',*,*,#7181,.F.);
#9526=ORIENTED_EDGE('',*,*,#7182,.F.);
#9527=ORIENTED_EDGE('',*,*,#7183,.F.);
#9528=ORIENTED_EDGE('',*,*,#7184,.T.);
#9529=ORIENTED_EDGE('',*,*,#7185,.F.);
#9530=ORIENTED_EDGE('',*,*,#7186,.T.);
#9531=ORIENTED_EDGE('',*,*,#7187,.T.);
#9532=ORIENTED_EDGE('',*,*,#7186,.F.);
#9533=ORIENTED_EDGE('',*,*,#7187,.F.);
#9534=ORIENTED_EDGE('',*,*,#7188,.F.);
#9535=ORIENTED_EDGE('',*,*,#7189,.F.);
#9536=ORIENTED_EDGE('',*,*,#7190,.T.);
#9537=ORIENTED_EDGE('',*,*,#7191,.T.);
#9538=ORIENTED_EDGE('',*,*,#7190,.F.);
#9539=ORIENTED_EDGE('',*,*,#7191,.F.);
#9540=ORIENTED_EDGE('',*,*,#7192,.F.);
#9541=ORIENTED_EDGE('',*,*,#7193,.F.);
#9542=ORIENTED_EDGE('',*,*,#7194,.T.);
#9543=ORIENTED_EDGE('',*,*,#7195,.T.);
#9544=ORIENTED_EDGE('',*,*,#7194,.F.);
#9545=ORIENTED_EDGE('',*,*,#7195,.F.);
#9546=ORIENTED_EDGE('',*,*,#7196,.F.);
#9547=ORIENTED_EDGE('',*,*,#7197,.F.);
#9548=ORIENTED_EDGE('',*,*,#7198,.T.);
#9549=ORIENTED_EDGE('',*,*,#7199,.T.);
#9550=ORIENTED_EDGE('',*,*,#7198,.F.);
#9551=ORIENTED_EDGE('',*,*,#7199,.F.);
#9552=ORIENTED_EDGE('',*,*,#7200,.F.);
#9553=ORIENTED_EDGE('',*,*,#7188,.T.);
#9554=ORIENTED_EDGE('',*,*,#7201,.T.);
#9555=ORIENTED_EDGE('',*,*,#7202,.F.);
#9556=ORIENTED_EDGE('',*,*,#7201,.F.);
#9557=ORIENTED_EDGE('',*,*,#7192,.T.);
#9558=ORIENTED_EDGE('',*,*,#7203,.T.);
#9559=ORIENTED_EDGE('',*,*,#7204,.F.);
#9560=ORIENTED_EDGE('',*,*,#7203,.F.);
#9561=ORIENTED_EDGE('',*,*,#7196,.T.);
#9562=ORIENTED_EDGE('',*,*,#7205,.T.);
#9563=ORIENTED_EDGE('',*,*,#7206,.F.);
#9564=ORIENTED_EDGE('',*,*,#7205,.F.);
#9565=ORIENTED_EDGE('',*,*,#7200,.T.);
#9566=ORIENTED_EDGE('',*,*,#7207,.T.);
#9567=ORIENTED_EDGE('',*,*,#7208,.F.);
#9568=ORIENTED_EDGE('',*,*,#7207,.F.);
#9569=ORIENTED_EDGE('',*,*,#7126,.F.);
#9570=ORIENTED_EDGE('',*,*,#7209,.T.);
#9571=ORIENTED_EDGE('',*,*,#7158,.T.);
#9572=ORIENTED_EDGE('',*,*,#7210,.T.);
#9573=ORIENTED_EDGE('',*,*,#7129,.F.);
#9574=ORIENTED_EDGE('',*,*,#7181,.T.);
#9575=ORIENTED_EDGE('',*,*,#7211,.T.);
#9576=ORIENTED_EDGE('',*,*,#7178,.F.);
#9577=ORIENTED_EDGE('',*,*,#7212,.F.);
#9578=ORIENTED_EDGE('',*,*,#7210,.F.);
#9579=ORIENTED_EDGE('',*,*,#7157,.F.);
#9580=ORIENTED_EDGE('',*,*,#7161,.F.);
#9581=ORIENTED_EDGE('',*,*,#7164,.F.);
#9582=ORIENTED_EDGE('',*,*,#7167,.F.);
#9583=ORIENTED_EDGE('',*,*,#7170,.F.);
#9584=ORIENTED_EDGE('',*,*,#7173,.F.);
#9585=ORIENTED_EDGE('',*,*,#7176,.F.);
#9586=ORIENTED_EDGE('',*,*,#7179,.F.);
#9587=ORIENTED_EDGE('',*,*,#7211,.F.);
#9588=ORIENTED_EDGE('',*,*,#7184,.F.);
#9589=ORIENTED_EDGE('',*,*,#7213,.F.);
#9590=ORIENTED_EDGE('',*,*,#7153,.F.);
#9591=ORIENTED_EDGE('',*,*,#7214,.F.);
#9592=ORIENTED_EDGE('',*,*,#7151,.F.);
#9593=ORIENTED_EDGE('',*,*,#7148,.F.);
#9594=ORIENTED_EDGE('',*,*,#7145,.F.);
#9595=ORIENTED_EDGE('',*,*,#7142,.F.);
#9596=ORIENTED_EDGE('',*,*,#7139,.F.);
#9597=ORIENTED_EDGE('',*,*,#7136,.F.);
#9598=ORIENTED_EDGE('',*,*,#7133,.F.);
#9599=ORIENTED_EDGE('',*,*,#7130,.F.);
#9600=ORIENTED_EDGE('',*,*,#7209,.F.);
#9601=ORIENTED_EDGE('',*,*,#7125,.F.);
#9602=ORIENTED_EDGE('',*,*,#7132,.F.);
#9603=ORIENTED_EDGE('',*,*,#7135,.F.);
#9604=ORIENTED_EDGE('',*,*,#7138,.F.);
#9605=ORIENTED_EDGE('',*,*,#7141,.F.);
#9606=ORIENTED_EDGE('',*,*,#7144,.F.);
#9607=ORIENTED_EDGE('',*,*,#7147,.F.);
#9608=ORIENTED_EDGE('',*,*,#7150,.F.);
#9609=ORIENTED_EDGE('',*,*,#7215,.F.);
#9610=ORIENTED_EDGE('',*,*,#7155,.F.);
#9611=ORIENTED_EDGE('',*,*,#7216,.F.);
#9612=ORIENTED_EDGE('',*,*,#7182,.T.);
#9613=ORIENTED_EDGE('',*,*,#7212,.T.);
#9614=ORIENTED_EDGE('',*,*,#7180,.T.);
#9615=ORIENTED_EDGE('',*,*,#7177,.T.);
#9616=ORIENTED_EDGE('',*,*,#7174,.T.);
#9617=ORIENTED_EDGE('',*,*,#7171,.T.);
#9618=ORIENTED_EDGE('',*,*,#7168,.T.);
#9619=ORIENTED_EDGE('',*,*,#7165,.T.);
#9620=ORIENTED_EDGE('',*,*,#7162,.T.);
#9621=ORIENTED_EDGE('',*,*,#7159,.T.);
#9622=ORIENTED_EDGE('',*,*,#7152,.T.);
#9623=ORIENTED_EDGE('',*,*,#7215,.T.);
#9624=ORIENTED_EDGE('',*,*,#7149,.F.);
#9625=ORIENTED_EDGE('',*,*,#7214,.T.);
#9626=ORIENTED_EDGE('',*,*,#7065,.F.);
#9627=ORIENTED_EDGE('',*,*,#7217,.T.);
#9628=ORIENTED_EDGE('',*,*,#7097,.T.);
#9629=ORIENTED_EDGE('',*,*,#7218,.T.);
#9630=ORIENTED_EDGE('',*,*,#7068,.F.);
#9631=ORIENTED_EDGE('',*,*,#7120,.T.);
#9632=ORIENTED_EDGE('',*,*,#7219,.T.);
#9633=ORIENTED_EDGE('',*,*,#7117,.F.);
#9634=ORIENTED_EDGE('',*,*,#7220,.F.);
#9635=ORIENTED_EDGE('',*,*,#7218,.F.);
#9636=ORIENTED_EDGE('',*,*,#7096,.F.);
#9637=ORIENTED_EDGE('',*,*,#7100,.F.);
#9638=ORIENTED_EDGE('',*,*,#7103,.F.);
#9639=ORIENTED_EDGE('',*,*,#7106,.F.);
#9640=ORIENTED_EDGE('',*,*,#7109,.F.);
#9641=ORIENTED_EDGE('',*,*,#7112,.F.);
#9642=ORIENTED_EDGE('',*,*,#7115,.F.);
#9643=ORIENTED_EDGE('',*,*,#7118,.F.);
#9644=ORIENTED_EDGE('',*,*,#7219,.F.);
#9645=ORIENTED_EDGE('',*,*,#7123,.F.);
#9646=ORIENTED_EDGE('',*,*,#7221,.F.);
#9647=ORIENTED_EDGE('',*,*,#7092,.F.);
#9648=ORIENTED_EDGE('',*,*,#7222,.F.);
#9649=ORIENTED_EDGE('',*,*,#7090,.F.);
#9650=ORIENTED_EDGE('',*,*,#7087,.F.);
#9651=ORIENTED_EDGE('',*,*,#7084,.F.);
#9652=ORIENTED_EDGE('',*,*,#7081,.F.);
#9653=ORIENTED_EDGE('',*,*,#7078,.F.);
#9654=ORIENTED_EDGE('',*,*,#7075,.F.);
#9655=ORIENTED_EDGE('',*,*,#7072,.F.);
#9656=ORIENTED_EDGE('',*,*,#7069,.F.);
#9657=ORIENTED_EDGE('',*,*,#7217,.F.);
#9658=ORIENTED_EDGE('',*,*,#7064,.F.);
#9659=ORIENTED_EDGE('',*,*,#7071,.F.);
#9660=ORIENTED_EDGE('',*,*,#7074,.F.);
#9661=ORIENTED_EDGE('',*,*,#7077,.F.);
#9662=ORIENTED_EDGE('',*,*,#7080,.F.);
#9663=ORIENTED_EDGE('',*,*,#7083,.F.);
#9664=ORIENTED_EDGE('',*,*,#7086,.F.);
#9665=ORIENTED_EDGE('',*,*,#7089,.F.);
#9666=ORIENTED_EDGE('',*,*,#7223,.F.);
#9667=ORIENTED_EDGE('',*,*,#7094,.F.);
#9668=ORIENTED_EDGE('',*,*,#7224,.F.);
#9669=ORIENTED_EDGE('',*,*,#7121,.T.);
#9670=ORIENTED_EDGE('',*,*,#7220,.T.);
#9671=ORIENTED_EDGE('',*,*,#7119,.T.);
#9672=ORIENTED_EDGE('',*,*,#7116,.T.);
#9673=ORIENTED_EDGE('',*,*,#7113,.T.);
#9674=ORIENTED_EDGE('',*,*,#7110,.T.);
#9675=ORIENTED_EDGE('',*,*,#7107,.T.);
#9676=ORIENTED_EDGE('',*,*,#7104,.T.);
#9677=ORIENTED_EDGE('',*,*,#7101,.T.);
#9678=ORIENTED_EDGE('',*,*,#7098,.T.);
#9679=ORIENTED_EDGE('',*,*,#7091,.T.);
#9680=ORIENTED_EDGE('',*,*,#7223,.T.);
#9681=ORIENTED_EDGE('',*,*,#7088,.F.);
#9682=ORIENTED_EDGE('',*,*,#7222,.T.);
#9683=ORIENTED_EDGE('',*,*,#7004,.F.);
#9684=ORIENTED_EDGE('',*,*,#7225,.T.);
#9685=ORIENTED_EDGE('',*,*,#7036,.T.);
#9686=ORIENTED_EDGE('',*,*,#7226,.T.);
#9687=ORIENTED_EDGE('',*,*,#7007,.F.);
#9688=ORIENTED_EDGE('',*,*,#7059,.T.);
#9689=ORIENTED_EDGE('',*,*,#7227,.T.);
#9690=ORIENTED_EDGE('',*,*,#7056,.F.);
#9691=ORIENTED_EDGE('',*,*,#7228,.F.);
#9692=ORIENTED_EDGE('',*,*,#7226,.F.);
#9693=ORIENTED_EDGE('',*,*,#7035,.F.);
#9694=ORIENTED_EDGE('',*,*,#7039,.F.);
#9695=ORIENTED_EDGE('',*,*,#7042,.F.);
#9696=ORIENTED_EDGE('',*,*,#7045,.F.);
#9697=ORIENTED_EDGE('',*,*,#7048,.F.);
#9698=ORIENTED_EDGE('',*,*,#7051,.F.);
#9699=ORIENTED_EDGE('',*,*,#7054,.F.);
#9700=ORIENTED_EDGE('',*,*,#7057,.F.);
#9701=ORIENTED_EDGE('',*,*,#7227,.F.);
#9702=ORIENTED_EDGE('',*,*,#7062,.F.);
#9703=ORIENTED_EDGE('',*,*,#7229,.F.);
#9704=ORIENTED_EDGE('',*,*,#7031,.F.);
#9705=ORIENTED_EDGE('',*,*,#7230,.F.);
#9706=ORIENTED_EDGE('',*,*,#7029,.F.);
#9707=ORIENTED_EDGE('',*,*,#7026,.F.);
#9708=ORIENTED_EDGE('',*,*,#7023,.F.);
#9709=ORIENTED_EDGE('',*,*,#7020,.F.);
#9710=ORIENTED_EDGE('',*,*,#7017,.F.);
#9711=ORIENTED_EDGE('',*,*,#7014,.F.);
#9712=ORIENTED_EDGE('',*,*,#7011,.F.);
#9713=ORIENTED_EDGE('',*,*,#7008,.F.);
#9714=ORIENTED_EDGE('',*,*,#7225,.F.);
#9715=ORIENTED_EDGE('',*,*,#7003,.F.);
#9716=ORIENTED_EDGE('',*,*,#7010,.F.);
#9717=ORIENTED_EDGE('',*,*,#7013,.F.);
#9718=ORIENTED_EDGE('',*,*,#7016,.F.);
#9719=ORIENTED_EDGE('',*,*,#7019,.F.);
#9720=ORIENTED_EDGE('',*,*,#7022,.F.);
#9721=ORIENTED_EDGE('',*,*,#7025,.F.);
#9722=ORIENTED_EDGE('',*,*,#7028,.F.);
#9723=ORIENTED_EDGE('',*,*,#7231,.F.);
#9724=ORIENTED_EDGE('',*,*,#7033,.F.);
#9725=ORIENTED_EDGE('',*,*,#7232,.F.);
#9726=ORIENTED_EDGE('',*,*,#7060,.T.);
#9727=ORIENTED_EDGE('',*,*,#7228,.T.);
#9728=ORIENTED_EDGE('',*,*,#7058,.T.);
#9729=ORIENTED_EDGE('',*,*,#7055,.T.);
#9730=ORIENTED_EDGE('',*,*,#7052,.T.);
#9731=ORIENTED_EDGE('',*,*,#7049,.T.);
#9732=ORIENTED_EDGE('',*,*,#7046,.T.);
#9733=ORIENTED_EDGE('',*,*,#7043,.T.);
#9734=ORIENTED_EDGE('',*,*,#7040,.T.);
#9735=ORIENTED_EDGE('',*,*,#7037,.T.);
#9736=ORIENTED_EDGE('',*,*,#7030,.T.);
#9737=ORIENTED_EDGE('',*,*,#7231,.T.);
#9738=ORIENTED_EDGE('',*,*,#7027,.F.);
#9739=ORIENTED_EDGE('',*,*,#7230,.T.);
#9740=ORIENTED_EDGE('',*,*,#6943,.F.);
#9741=ORIENTED_EDGE('',*,*,#7233,.T.);
#9742=ORIENTED_EDGE('',*,*,#6975,.T.);
#9743=ORIENTED_EDGE('',*,*,#7234,.T.);
#9744=ORIENTED_EDGE('',*,*,#6946,.F.);
#9745=ORIENTED_EDGE('',*,*,#6998,.T.);
#9746=ORIENTED_EDGE('',*,*,#7235,.T.);
#9747=ORIENTED_EDGE('',*,*,#6995,.F.);
#9748=ORIENTED_EDGE('',*,*,#7236,.F.);
#9749=ORIENTED_EDGE('',*,*,#7234,.F.);
#9750=ORIENTED_EDGE('',*,*,#6974,.F.);
#9751=ORIENTED_EDGE('',*,*,#6978,.F.);
#9752=ORIENTED_EDGE('',*,*,#6981,.F.);
#9753=ORIENTED_EDGE('',*,*,#6984,.F.);
#9754=ORIENTED_EDGE('',*,*,#6987,.F.);
#9755=ORIENTED_EDGE('',*,*,#6990,.F.);
#9756=ORIENTED_EDGE('',*,*,#6993,.F.);
#9757=ORIENTED_EDGE('',*,*,#6996,.F.);
#9758=ORIENTED_EDGE('',*,*,#7235,.F.);
#9759=ORIENTED_EDGE('',*,*,#7001,.F.);
#9760=ORIENTED_EDGE('',*,*,#7237,.F.);
#9761=ORIENTED_EDGE('',*,*,#6970,.F.);
#9762=ORIENTED_EDGE('',*,*,#7238,.F.);
#9763=ORIENTED_EDGE('',*,*,#6968,.F.);
#9764=ORIENTED_EDGE('',*,*,#6965,.F.);
#9765=ORIENTED_EDGE('',*,*,#6962,.F.);
#9766=ORIENTED_EDGE('',*,*,#6959,.F.);
#9767=ORIENTED_EDGE('',*,*,#6956,.F.);
#9768=ORIENTED_EDGE('',*,*,#6953,.F.);
#9769=ORIENTED_EDGE('',*,*,#6950,.F.);
#9770=ORIENTED_EDGE('',*,*,#6947,.F.);
#9771=ORIENTED_EDGE('',*,*,#7233,.F.);
#9772=ORIENTED_EDGE('',*,*,#6942,.F.);
#9773=ORIENTED_EDGE('',*,*,#6949,.F.);
#9774=ORIENTED_EDGE('',*,*,#6952,.F.);
#9775=ORIENTED_EDGE('',*,*,#6955,.F.);
#9776=ORIENTED_EDGE('',*,*,#6958,.F.);
#9777=ORIENTED_EDGE('',*,*,#6961,.F.);
#9778=ORIENTED_EDGE('',*,*,#6964,.F.);
#9779=ORIENTED_EDGE('',*,*,#6967,.F.);
#9780=ORIENTED_EDGE('',*,*,#7239,.F.);
#9781=ORIENTED_EDGE('',*,*,#6972,.F.);
#9782=ORIENTED_EDGE('',*,*,#7240,.F.);
#9783=ORIENTED_EDGE('',*,*,#6999,.T.);
#9784=ORIENTED_EDGE('',*,*,#7236,.T.);
#9785=ORIENTED_EDGE('',*,*,#6997,.T.);
#9786=ORIENTED_EDGE('',*,*,#6994,.T.);
#9787=ORIENTED_EDGE('',*,*,#6991,.T.);
#9788=ORIENTED_EDGE('',*,*,#6988,.T.);
#9789=ORIENTED_EDGE('',*,*,#6985,.T.);
#9790=ORIENTED_EDGE('',*,*,#6982,.T.);
#9791=ORIENTED_EDGE('',*,*,#6979,.T.);
#9792=ORIENTED_EDGE('',*,*,#6976,.T.);
#9793=ORIENTED_EDGE('',*,*,#6969,.T.);
#9794=ORIENTED_EDGE('',*,*,#7239,.T.);
#9795=ORIENTED_EDGE('',*,*,#6966,.F.);
#9796=ORIENTED_EDGE('',*,*,#7238,.T.);
#9797=ORIENTED_EDGE('',*,*,#6882,.F.);
#9798=ORIENTED_EDGE('',*,*,#7241,.T.);
#9799=ORIENTED_EDGE('',*,*,#6914,.T.);
#9800=ORIENTED_EDGE('',*,*,#7242,.T.);
#9801=ORIENTED_EDGE('',*,*,#6885,.F.);
#9802=ORIENTED_EDGE('',*,*,#6937,.T.);
#9803=ORIENTED_EDGE('',*,*,#7243,.T.);
#9804=ORIENTED_EDGE('',*,*,#6934,.F.);
#9805=ORIENTED_EDGE('',*,*,#7244,.F.);
#9806=ORIENTED_EDGE('',*,*,#7242,.F.);
#9807=ORIENTED_EDGE('',*,*,#6913,.F.);
#9808=ORIENTED_EDGE('',*,*,#6917,.F.);
#9809=ORIENTED_EDGE('',*,*,#6920,.F.);
#9810=ORIENTED_EDGE('',*,*,#6923,.F.);
#9811=ORIENTED_EDGE('',*,*,#6926,.F.);
#9812=ORIENTED_EDGE('',*,*,#6929,.F.);
#9813=ORIENTED_EDGE('',*,*,#6932,.F.);
#9814=ORIENTED_EDGE('',*,*,#6935,.F.);
#9815=ORIENTED_EDGE('',*,*,#7243,.F.);
#9816=ORIENTED_EDGE('',*,*,#6940,.F.);
#9817=ORIENTED_EDGE('',*,*,#7245,.F.);
#9818=ORIENTED_EDGE('',*,*,#6909,.F.);
#9819=ORIENTED_EDGE('',*,*,#7246,.F.);
#9820=ORIENTED_EDGE('',*,*,#6907,.F.);
#9821=ORIENTED_EDGE('',*,*,#6904,.F.);
#9822=ORIENTED_EDGE('',*,*,#6901,.F.);
#9823=ORIENTED_EDGE('',*,*,#6898,.F.);
#9824=ORIENTED_EDGE('',*,*,#6895,.F.);
#9825=ORIENTED_EDGE('',*,*,#6892,.F.);
#9826=ORIENTED_EDGE('',*,*,#6889,.F.);
#9827=ORIENTED_EDGE('',*,*,#6886,.F.);
#9828=ORIENTED_EDGE('',*,*,#7241,.F.);
#9829=ORIENTED_EDGE('',*,*,#6881,.F.);
#9830=ORIENTED_EDGE('',*,*,#6888,.F.);
#9831=ORIENTED_EDGE('',*,*,#6891,.F.);
#9832=ORIENTED_EDGE('',*,*,#6894,.F.);
#9833=ORIENTED_EDGE('',*,*,#6897,.F.);
#9834=ORIENTED_EDGE('',*,*,#6900,.F.);
#9835=ORIENTED_EDGE('',*,*,#6903,.F.);
#9836=ORIENTED_EDGE('',*,*,#6906,.F.);
#9837=ORIENTED_EDGE('',*,*,#7247,.F.);
#9838=ORIENTED_EDGE('',*,*,#6911,.F.);
#9839=ORIENTED_EDGE('',*,*,#7248,.F.);
#9840=ORIENTED_EDGE('',*,*,#6938,.T.);
#9841=ORIENTED_EDGE('',*,*,#7244,.T.);
#9842=ORIENTED_EDGE('',*,*,#6936,.T.);
#9843=ORIENTED_EDGE('',*,*,#6933,.T.);
#9844=ORIENTED_EDGE('',*,*,#6930,.T.);
#9845=ORIENTED_EDGE('',*,*,#6927,.T.);
#9846=ORIENTED_EDGE('',*,*,#6924,.T.);
#9847=ORIENTED_EDGE('',*,*,#6921,.T.);
#9848=ORIENTED_EDGE('',*,*,#6918,.T.);
#9849=ORIENTED_EDGE('',*,*,#6915,.T.);
#9850=ORIENTED_EDGE('',*,*,#6908,.T.);
#9851=ORIENTED_EDGE('',*,*,#7247,.T.);
#9852=ORIENTED_EDGE('',*,*,#6905,.F.);
#9853=ORIENTED_EDGE('',*,*,#7246,.T.);
#9854=ORIENTED_EDGE('',*,*,#6821,.F.);
#9855=ORIENTED_EDGE('',*,*,#7249,.T.);
#9856=ORIENTED_EDGE('',*,*,#6853,.T.);
#9857=ORIENTED_EDGE('',*,*,#7250,.T.);
#9858=ORIENTED_EDGE('',*,*,#6824,.F.);
#9859=ORIENTED_EDGE('',*,*,#6876,.T.);
#9860=ORIENTED_EDGE('',*,*,#7251,.T.);
#9861=ORIENTED_EDGE('',*,*,#6873,.F.);
#9862=ORIENTED_EDGE('',*,*,#7252,.F.);
#9863=ORIENTED_EDGE('',*,*,#7250,.F.);
#9864=ORIENTED_EDGE('',*,*,#6852,.F.);
#9865=ORIENTED_EDGE('',*,*,#6856,.F.);
#9866=ORIENTED_EDGE('',*,*,#6859,.F.);
#9867=ORIENTED_EDGE('',*,*,#6862,.F.);
#9868=ORIENTED_EDGE('',*,*,#6865,.F.);
#9869=ORIENTED_EDGE('',*,*,#6868,.F.);
#9870=ORIENTED_EDGE('',*,*,#6871,.F.);
#9871=ORIENTED_EDGE('',*,*,#6874,.F.);
#9872=ORIENTED_EDGE('',*,*,#7251,.F.);
#9873=ORIENTED_EDGE('',*,*,#6879,.F.);
#9874=ORIENTED_EDGE('',*,*,#7253,.F.);
#9875=ORIENTED_EDGE('',*,*,#6848,.F.);
#9876=ORIENTED_EDGE('',*,*,#7254,.F.);
#9877=ORIENTED_EDGE('',*,*,#6846,.F.);
#9878=ORIENTED_EDGE('',*,*,#6843,.F.);
#9879=ORIENTED_EDGE('',*,*,#6840,.F.);
#9880=ORIENTED_EDGE('',*,*,#6837,.F.);
#9881=ORIENTED_EDGE('',*,*,#6834,.F.);
#9882=ORIENTED_EDGE('',*,*,#6831,.F.);
#9883=ORIENTED_EDGE('',*,*,#6828,.F.);
#9884=ORIENTED_EDGE('',*,*,#6825,.F.);
#9885=ORIENTED_EDGE('',*,*,#7249,.F.);
#9886=ORIENTED_EDGE('',*,*,#6820,.F.);
#9887=ORIENTED_EDGE('',*,*,#6827,.F.);
#9888=ORIENTED_EDGE('',*,*,#6830,.F.);
#9889=ORIENTED_EDGE('',*,*,#6833,.F.);
#9890=ORIENTED_EDGE('',*,*,#6836,.F.);
#9891=ORIENTED_EDGE('',*,*,#6839,.F.);
#9892=ORIENTED_EDGE('',*,*,#6842,.F.);
#9893=ORIENTED_EDGE('',*,*,#6845,.F.);
#9894=ORIENTED_EDGE('',*,*,#7255,.F.);
#9895=ORIENTED_EDGE('',*,*,#6850,.F.);
#9896=ORIENTED_EDGE('',*,*,#7256,.F.);
#9897=ORIENTED_EDGE('',*,*,#6877,.T.);
#9898=ORIENTED_EDGE('',*,*,#7252,.T.);
#9899=ORIENTED_EDGE('',*,*,#6875,.T.);
#9900=ORIENTED_EDGE('',*,*,#6872,.T.);
#9901=ORIENTED_EDGE('',*,*,#6869,.T.);
#9902=ORIENTED_EDGE('',*,*,#6866,.T.);
#9903=ORIENTED_EDGE('',*,*,#6863,.T.);
#9904=ORIENTED_EDGE('',*,*,#6860,.T.);
#9905=ORIENTED_EDGE('',*,*,#6857,.T.);
#9906=ORIENTED_EDGE('',*,*,#6854,.T.);
#9907=ORIENTED_EDGE('',*,*,#6847,.T.);
#9908=ORIENTED_EDGE('',*,*,#7255,.T.);
#9909=ORIENTED_EDGE('',*,*,#6844,.F.);
#9910=ORIENTED_EDGE('',*,*,#7254,.T.);
#9911=ORIENTED_EDGE('',*,*,#6760,.F.);
#9912=ORIENTED_EDGE('',*,*,#7257,.T.);
#9913=ORIENTED_EDGE('',*,*,#6792,.T.);
#9914=ORIENTED_EDGE('',*,*,#7258,.T.);
#9915=ORIENTED_EDGE('',*,*,#6763,.F.);
#9916=ORIENTED_EDGE('',*,*,#6815,.T.);
#9917=ORIENTED_EDGE('',*,*,#7259,.T.);
#9918=ORIENTED_EDGE('',*,*,#6812,.F.);
#9919=ORIENTED_EDGE('',*,*,#7260,.F.);
#9920=ORIENTED_EDGE('',*,*,#7258,.F.);
#9921=ORIENTED_EDGE('',*,*,#6791,.F.);
#9922=ORIENTED_EDGE('',*,*,#6795,.F.);
#9923=ORIENTED_EDGE('',*,*,#6798,.F.);
#9924=ORIENTED_EDGE('',*,*,#6801,.F.);
#9925=ORIENTED_EDGE('',*,*,#6804,.F.);
#9926=ORIENTED_EDGE('',*,*,#6807,.F.);
#9927=ORIENTED_EDGE('',*,*,#6810,.F.);
#9928=ORIENTED_EDGE('',*,*,#6813,.F.);
#9929=ORIENTED_EDGE('',*,*,#7259,.F.);
#9930=ORIENTED_EDGE('',*,*,#6818,.F.);
#9931=ORIENTED_EDGE('',*,*,#7261,.F.);
#9932=ORIENTED_EDGE('',*,*,#6787,.F.);
#9933=ORIENTED_EDGE('',*,*,#7262,.F.);
#9934=ORIENTED_EDGE('',*,*,#6785,.F.);
#9935=ORIENTED_EDGE('',*,*,#6782,.F.);
#9936=ORIENTED_EDGE('',*,*,#6779,.F.);
#9937=ORIENTED_EDGE('',*,*,#6776,.F.);
#9938=ORIENTED_EDGE('',*,*,#6773,.F.);
#9939=ORIENTED_EDGE('',*,*,#6770,.F.);
#9940=ORIENTED_EDGE('',*,*,#6767,.F.);
#9941=ORIENTED_EDGE('',*,*,#6764,.F.);
#9942=ORIENTED_EDGE('',*,*,#7257,.F.);
#9943=ORIENTED_EDGE('',*,*,#6759,.F.);
#9944=ORIENTED_EDGE('',*,*,#6766,.F.);
#9945=ORIENTED_EDGE('',*,*,#6769,.F.);
#9946=ORIENTED_EDGE('',*,*,#6772,.F.);
#9947=ORIENTED_EDGE('',*,*,#6775,.F.);
#9948=ORIENTED_EDGE('',*,*,#6778,.F.);
#9949=ORIENTED_EDGE('',*,*,#6781,.F.);
#9950=ORIENTED_EDGE('',*,*,#6784,.F.);
#9951=ORIENTED_EDGE('',*,*,#7263,.F.);
#9952=ORIENTED_EDGE('',*,*,#6789,.F.);
#9953=ORIENTED_EDGE('',*,*,#7264,.F.);
#9954=ORIENTED_EDGE('',*,*,#6816,.T.);
#9955=ORIENTED_EDGE('',*,*,#7260,.T.);
#9956=ORIENTED_EDGE('',*,*,#6814,.T.);
#9957=ORIENTED_EDGE('',*,*,#6811,.T.);
#9958=ORIENTED_EDGE('',*,*,#6808,.T.);
#9959=ORIENTED_EDGE('',*,*,#6805,.T.);
#9960=ORIENTED_EDGE('',*,*,#6802,.T.);
#9961=ORIENTED_EDGE('',*,*,#6799,.T.);
#9962=ORIENTED_EDGE('',*,*,#6796,.T.);
#9963=ORIENTED_EDGE('',*,*,#6793,.T.);
#9964=ORIENTED_EDGE('',*,*,#6786,.T.);
#9965=ORIENTED_EDGE('',*,*,#7263,.T.);
#9966=ORIENTED_EDGE('',*,*,#6783,.F.);
#9967=ORIENTED_EDGE('',*,*,#7262,.T.);
#9968=ORIENTED_EDGE('',*,*,#6699,.F.);
#9969=ORIENTED_EDGE('',*,*,#7265,.T.);
#9970=ORIENTED_EDGE('',*,*,#6731,.T.);
#9971=ORIENTED_EDGE('',*,*,#7266,.T.);
#9972=ORIENTED_EDGE('',*,*,#6702,.F.);
#9973=ORIENTED_EDGE('',*,*,#6754,.T.);
#9974=ORIENTED_EDGE('',*,*,#7267,.T.);
#9975=ORIENTED_EDGE('',*,*,#6751,.F.);
#9976=ORIENTED_EDGE('',*,*,#7268,.F.);
#9977=ORIENTED_EDGE('',*,*,#7266,.F.);
#9978=ORIENTED_EDGE('',*,*,#6730,.F.);
#9979=ORIENTED_EDGE('',*,*,#6734,.F.);
#9980=ORIENTED_EDGE('',*,*,#6737,.F.);
#9981=ORIENTED_EDGE('',*,*,#6740,.F.);
#9982=ORIENTED_EDGE('',*,*,#6743,.F.);
#9983=ORIENTED_EDGE('',*,*,#6746,.F.);
#9984=ORIENTED_EDGE('',*,*,#6749,.F.);
#9985=ORIENTED_EDGE('',*,*,#6752,.F.);
#9986=ORIENTED_EDGE('',*,*,#7267,.F.);
#9987=ORIENTED_EDGE('',*,*,#6757,.F.);
#9988=ORIENTED_EDGE('',*,*,#7269,.F.);
#9989=ORIENTED_EDGE('',*,*,#6726,.F.);
#9990=ORIENTED_EDGE('',*,*,#7270,.F.);
#9991=ORIENTED_EDGE('',*,*,#6724,.F.);
#9992=ORIENTED_EDGE('',*,*,#6721,.F.);
#9993=ORIENTED_EDGE('',*,*,#6718,.F.);
#9994=ORIENTED_EDGE('',*,*,#6715,.F.);
#9995=ORIENTED_EDGE('',*,*,#6712,.F.);
#9996=ORIENTED_EDGE('',*,*,#6709,.F.);
#9997=ORIENTED_EDGE('',*,*,#6706,.F.);
#9998=ORIENTED_EDGE('',*,*,#6703,.F.);
#9999=ORIENTED_EDGE('',*,*,#7265,.F.);
#10000=ORIENTED_EDGE('',*,*,#6698,.F.);
#10001=ORIENTED_EDGE('',*,*,#6705,.F.);
#10002=ORIENTED_EDGE('',*,*,#6708,.F.);
#10003=ORIENTED_EDGE('',*,*,#6711,.F.);
#10004=ORIENTED_EDGE('',*,*,#6714,.F.);
#10005=ORIENTED_EDGE('',*,*,#6717,.F.);
#10006=ORIENTED_EDGE('',*,*,#6720,.F.);
#10007=ORIENTED_EDGE('',*,*,#6723,.F.);
#10008=ORIENTED_EDGE('',*,*,#7271,.F.);
#10009=ORIENTED_EDGE('',*,*,#6728,.F.);
#10010=ORIENTED_EDGE('',*,*,#7272,.F.);
#10011=ORIENTED_EDGE('',*,*,#6755,.T.);
#10012=ORIENTED_EDGE('',*,*,#7268,.T.);
#10013=ORIENTED_EDGE('',*,*,#6753,.T.);
#10014=ORIENTED_EDGE('',*,*,#6750,.T.);
#10015=ORIENTED_EDGE('',*,*,#6747,.T.);
#10016=ORIENTED_EDGE('',*,*,#6744,.T.);
#10017=ORIENTED_EDGE('',*,*,#6741,.T.);
#10018=ORIENTED_EDGE('',*,*,#6738,.T.);
#10019=ORIENTED_EDGE('',*,*,#6735,.T.);
#10020=ORIENTED_EDGE('',*,*,#6732,.T.);
#10021=ORIENTED_EDGE('',*,*,#6725,.T.);
#10022=ORIENTED_EDGE('',*,*,#7271,.T.);
#10023=ORIENTED_EDGE('',*,*,#6722,.F.);
#10024=ORIENTED_EDGE('',*,*,#7270,.T.);
#10025=ORIENTED_EDGE('',*,*,#7273,.F.);
#10026=ORIENTED_EDGE('',*,*,#7274,.T.);
#10027=ORIENTED_EDGE('',*,*,#7275,.F.);
#10028=ORIENTED_EDGE('',*,*,#7276,.F.);
#10029=ORIENTED_EDGE('',*,*,#7277,.F.);
#10030=ORIENTED_EDGE('',*,*,#7278,.F.);
#10031=ORIENTED_EDGE('',*,*,#7275,.T.);
#10032=ORIENTED_EDGE('',*,*,#7279,.T.);
#10033=ORIENTED_EDGE('',*,*,#7280,.F.);
#10034=ORIENTED_EDGE('',*,*,#7281,.F.);
#10035=ORIENTED_EDGE('',*,*,#7282,.F.);
#10036=ORIENTED_EDGE('',*,*,#7283,.F.);
#10037=ORIENTED_EDGE('',*,*,#7284,.F.);
#10038=ORIENTED_EDGE('',*,*,#7285,.F.);
#10039=ORIENTED_EDGE('',*,*,#7286,.F.);
#10040=ORIENTED_EDGE('',*,*,#7287,.F.);
#10041=ORIENTED_EDGE('',*,*,#7288,.F.);
#10042=ORIENTED_EDGE('',*,*,#7289,.F.);
#10043=ORIENTED_EDGE('',*,*,#7280,.T.);
#10044=ORIENTED_EDGE('',*,*,#7290,.T.);
#10045=ORIENTED_EDGE('',*,*,#7291,.F.);
#10046=ORIENTED_EDGE('',*,*,#7290,.F.);
#10047=ORIENTED_EDGE('',*,*,#7279,.F.);
#10048=ORIENTED_EDGE('',*,*,#7274,.F.);
#10049=ORIENTED_EDGE('',*,*,#7224,.T.);
#10050=ORIENTED_EDGE('',*,*,#7093,.T.);
#10051=ORIENTED_EDGE('',*,*,#7221,.T.);
#10052=ORIENTED_EDGE('',*,*,#7122,.T.);
#10053=ORIENTED_EDGE('',*,*,#7248,.T.);
#10054=ORIENTED_EDGE('',*,*,#6910,.T.);
#10055=ORIENTED_EDGE('',*,*,#7245,.T.);
#10056=ORIENTED_EDGE('',*,*,#6939,.T.);
#10057=ORIENTED_EDGE('',*,*,#7292,.F.);
#10058=ORIENTED_EDGE('',*,*,#7293,.F.);
#10059=ORIENTED_EDGE('',*,*,#7294,.T.);
#10060=ORIENTED_EDGE('',*,*,#7295,.T.);
#10061=ORIENTED_EDGE('',*,*,#7296,.F.);
#10062=ORIENTED_EDGE('',*,*,#7297,.F.);
#10063=ORIENTED_EDGE('',*,*,#7298,.F.);
#10064=ORIENTED_EDGE('',*,*,#7299,.F.);
#10065=ORIENTED_EDGE('',*,*,#7300,.F.);
#10066=ORIENTED_EDGE('',*,*,#7301,.F.);
#10067=ORIENTED_EDGE('',*,*,#7302,.F.);
#10068=ORIENTED_EDGE('',*,*,#7303,.F.);
#10069=ORIENTED_EDGE('',*,*,#7304,.F.);
#10070=ORIENTED_EDGE('',*,*,#7305,.T.);
#10071=ORIENTED_EDGE('',*,*,#7294,.F.);
#10072=ORIENTED_EDGE('',*,*,#7306,.F.);
#10073=ORIENTED_EDGE('',*,*,#7307,.F.);
#10074=ORIENTED_EDGE('',*,*,#7308,.F.);
#10075=ORIENTED_EDGE('',*,*,#7296,.T.);
#10076=ORIENTED_EDGE('',*,*,#7309,.T.);
#10077=ORIENTED_EDGE('',*,*,#7310,.F.);
#10078=ORIENTED_EDGE('',*,*,#7309,.F.);
#10079=ORIENTED_EDGE('',*,*,#7295,.F.);
#10080=ORIENTED_EDGE('',*,*,#7305,.F.);
#10081=ORIENTED_EDGE('',*,*,#7232,.T.);
#10082=ORIENTED_EDGE('',*,*,#7032,.T.);
#10083=ORIENTED_EDGE('',*,*,#7229,.T.);
#10084=ORIENTED_EDGE('',*,*,#7061,.T.);
#10085=ORIENTED_EDGE('',*,*,#7256,.T.);
#10086=ORIENTED_EDGE('',*,*,#6849,.T.);
#10087=ORIENTED_EDGE('',*,*,#7253,.T.);
#10088=ORIENTED_EDGE('',*,*,#6878,.T.);
#10089=ORIENTED_EDGE('',*,*,#7285,.T.);
#10090=ORIENTED_EDGE('',*,*,#7311,.F.);
#10091=ORIENTED_EDGE('',*,*,#7312,.F.);
#10092=ORIENTED_EDGE('',*,*,#7313,.F.);
#10093=ORIENTED_EDGE('',*,*,#7314,.F.);
#10094=ORIENTED_EDGE('',*,*,#7315,.F.);
#10095=ORIENTED_EDGE('',*,*,#7284,.T.);
#10096=ORIENTED_EDGE('',*,*,#7316,.T.);
#10097=ORIENTED_EDGE('',*,*,#7317,.T.);
#10098=ORIENTED_EDGE('',*,*,#7311,.T.);
#10099=ORIENTED_EDGE('',*,*,#7289,.T.);
#10100=ORIENTED_EDGE('',*,*,#7318,.T.);
#10101=ORIENTED_EDGE('',*,*,#7319,.T.);
#10102=ORIENTED_EDGE('',*,*,#7320,.T.);
#10103=ORIENTED_EDGE('',*,*,#7321,.T.);
#10104=ORIENTED_EDGE('',*,*,#7322,.T.);
#10105=ORIENTED_EDGE('',*,*,#7323,.T.);
#10106=ORIENTED_EDGE('',*,*,#7324,.T.);
#10107=ORIENTED_EDGE('',*,*,#7325,.T.);
#10108=ORIENTED_EDGE('',*,*,#7281,.T.);
#10109=ORIENTED_EDGE('',*,*,#7185,.T.);
#10110=ORIENTED_EDGE('',*,*,#7276,.T.);
#10111=ORIENTED_EDGE('',*,*,#7278,.T.);
#10112=ORIENTED_EDGE('',*,*,#7326,.T.);
#10113=ORIENTED_EDGE('',*,*,#7327,.T.);
#10114=ORIENTED_EDGE('',*,*,#7328,.T.);
#10115=ORIENTED_EDGE('',*,*,#7329,.T.);
#10116=ORIENTED_EDGE('',*,*,#7330,.T.);
#10117=ORIENTED_EDGE('',*,*,#7331,.T.);
#10118=ORIENTED_EDGE('',*,*,#7332,.T.);
#10119=ORIENTED_EDGE('',*,*,#7333,.T.);
#10120=ORIENTED_EDGE('',*,*,#7189,.T.);
#10121=ORIENTED_EDGE('',*,*,#7283,.T.);
#10122=ORIENTED_EDGE('',*,*,#7334,.F.);
#10123=ORIENTED_EDGE('',*,*,#7335,.F.);
#10124=ORIENTED_EDGE('',*,*,#7316,.F.);
#10125=ORIENTED_EDGE('',*,*,#7282,.T.);
#10126=ORIENTED_EDGE('',*,*,#7325,.F.);
#10127=ORIENTED_EDGE('',*,*,#7336,.T.);
#10128=ORIENTED_EDGE('',*,*,#7334,.T.);
#10129=ORIENTED_EDGE('',*,*,#7301,.T.);
#10130=ORIENTED_EDGE('',*,*,#7337,.F.);
#10131=ORIENTED_EDGE('',*,*,#7338,.F.);
#10132=ORIENTED_EDGE('',*,*,#7339,.F.);
#10133=ORIENTED_EDGE('',*,*,#7340,.F.);
#10134=ORIENTED_EDGE('',*,*,#7341,.F.);
#10135=ORIENTED_EDGE('',*,*,#7300,.T.);
#10136=ORIENTED_EDGE('',*,*,#7342,.T.);
#10137=ORIENTED_EDGE('',*,*,#7343,.T.);
#10138=ORIENTED_EDGE('',*,*,#7337,.T.);
#10139=ORIENTED_EDGE('',*,*,#7299,.T.);
#10140=ORIENTED_EDGE('',*,*,#7344,.F.);
#10141=ORIENTED_EDGE('',*,*,#7345,.F.);
#10142=ORIENTED_EDGE('',*,*,#7342,.F.);
#10143=ORIENTED_EDGE('',*,*,#7298,.T.);
#10144=ORIENTED_EDGE('',*,*,#7346,.F.);
#10145=ORIENTED_EDGE('',*,*,#7347,.T.);
#10146=ORIENTED_EDGE('',*,*,#7344,.T.);
#10147=ORIENTED_EDGE('',*,*,#7297,.T.);
#10148=ORIENTED_EDGE('',*,*,#7308,.T.);
#10149=ORIENTED_EDGE('',*,*,#7348,.T.);
#10150=ORIENTED_EDGE('',*,*,#7349,.T.);
#10151=ORIENTED_EDGE('',*,*,#7350,.T.);
#10152=ORIENTED_EDGE('',*,*,#7351,.T.);
#10153=ORIENTED_EDGE('',*,*,#7352,.T.);
#10154=ORIENTED_EDGE('',*,*,#7353,.T.);
#10155=ORIENTED_EDGE('',*,*,#7354,.T.);
#10156=ORIENTED_EDGE('',*,*,#7346,.T.);
#10157=ORIENTED_EDGE('',*,*,#7193,.T.);
#10158=ORIENTED_EDGE('',*,*,#7286,.T.);
#10159=ORIENTED_EDGE('',*,*,#7315,.T.);
#10160=ORIENTED_EDGE('',*,*,#7355,.F.);
#10161=ORIENTED_EDGE('',*,*,#7356,.T.);
#10162=ORIENTED_EDGE('',*,*,#7287,.T.);
#10163=ORIENTED_EDGE('',*,*,#7356,.F.);
#10164=ORIENTED_EDGE('',*,*,#7357,.F.);
#10165=ORIENTED_EDGE('',*,*,#7358,.F.);
#10166=ORIENTED_EDGE('',*,*,#7303,.T.);
#10167=ORIENTED_EDGE('',*,*,#7359,.F.);
#10168=ORIENTED_EDGE('',*,*,#7360,.F.);
#10169=ORIENTED_EDGE('',*,*,#7361,.F.);
#10170=ORIENTED_EDGE('',*,*,#7302,.T.);
#10171=ORIENTED_EDGE('',*,*,#7341,.T.);
#10172=ORIENTED_EDGE('',*,*,#7362,.F.);
#10173=ORIENTED_EDGE('',*,*,#7359,.T.);
#10174=ORIENTED_EDGE('',*,*,#7363,.T.);
#10175=ORIENTED_EDGE('',*,*,#7313,.T.);
#10176=ORIENTED_EDGE('',*,*,#7364,.T.);
#10177=ORIENTED_EDGE('',*,*,#7323,.F.);
#10178=ORIENTED_EDGE('',*,*,#7365,.T.);
#10179=ORIENTED_EDGE('',*,*,#7366,.T.);
#10180=ORIENTED_EDGE('',*,*,#7367,.T.);
#10181=ORIENTED_EDGE('',*,*,#7368,.F.);
#10182=ORIENTED_EDGE('',*,*,#7369,.T.);
#10183=ORIENTED_EDGE('',*,*,#7339,.T.);
#10184=ORIENTED_EDGE('',*,*,#7370,.T.);
#10185=ORIENTED_EDGE('',*,*,#7353,.F.);
#10186=ORIENTED_EDGE('',*,*,#7371,.T.);
#10187=ORIENTED_EDGE('',*,*,#7372,.T.);
#10188=ORIENTED_EDGE('',*,*,#7373,.T.);
#10189=ORIENTED_EDGE('',*,*,#7374,.T.);
#10190=ORIENTED_EDGE('',*,*,#7373,.F.);
#10191=ORIENTED_EDGE('',*,*,#7375,.T.);
#10192=ORIENTED_EDGE('',*,*,#7376,.T.);
#10193=ORIENTED_EDGE('',*,*,#7328,.F.);
#10194=ORIENTED_EDGE('',*,*,#7363,.F.);
#10195=ORIENTED_EDGE('',*,*,#7327,.F.);
#10196=ORIENTED_EDGE('',*,*,#7377,.T.);
#10197=ORIENTED_EDGE('',*,*,#7357,.T.);
#10198=ORIENTED_EDGE('',*,*,#7378,.T.);
#10199=ORIENTED_EDGE('',*,*,#7314,.T.);
#10200=ORIENTED_EDGE('',*,*,#7364,.F.);
#10201=ORIENTED_EDGE('',*,*,#7312,.T.);
#10202=ORIENTED_EDGE('',*,*,#7379,.F.);
#10203=ORIENTED_EDGE('',*,*,#7335,.T.);
#10204=ORIENTED_EDGE('',*,*,#7336,.F.);
#10205=ORIENTED_EDGE('',*,*,#7324,.F.);
#10206=ORIENTED_EDGE('',*,*,#7277,.T.);
#10207=ORIENTED_EDGE('',*,*,#7358,.T.);
#10208=ORIENTED_EDGE('',*,*,#7377,.F.);
#10209=ORIENTED_EDGE('',*,*,#7326,.F.);
#10210=ORIENTED_EDGE('',*,*,#7370,.F.);
#10211=ORIENTED_EDGE('',*,*,#7338,.T.);
#10212=ORIENTED_EDGE('',*,*,#7380,.F.);
#10213=ORIENTED_EDGE('',*,*,#7345,.T.);
#10214=ORIENTED_EDGE('',*,*,#7347,.F.);
#10215=ORIENTED_EDGE('',*,*,#7354,.F.);
#10216=ORIENTED_EDGE('',*,*,#7369,.F.);
#10217=ORIENTED_EDGE('',*,*,#7381,.F.);
#10218=ORIENTED_EDGE('',*,*,#7382,.T.);
#10219=ORIENTED_EDGE('',*,*,#7360,.T.);
#10220=ORIENTED_EDGE('',*,*,#7383,.T.);
#10221=ORIENTED_EDGE('',*,*,#7340,.T.);
#10222=ORIENTED_EDGE('',*,*,#7292,.T.);
#10223=ORIENTED_EDGE('',*,*,#7361,.T.);
#10224=ORIENTED_EDGE('',*,*,#7382,.F.);
#10225=ORIENTED_EDGE('',*,*,#7384,.F.);
#10226=ORIENTED_EDGE('',*,*,#7385,.F.);
#10227=ORIENTED_EDGE('',*,*,#7332,.F.);
#10228=ORIENTED_EDGE('',*,*,#7386,.T.);
#10229=ORIENTED_EDGE('',*,*,#7387,.T.);
#10230=ORIENTED_EDGE('',*,*,#7388,.F.);
#10231=ORIENTED_EDGE('',*,*,#7387,.F.);
#10232=ORIENTED_EDGE('',*,*,#7389,.F.);
#10233=ORIENTED_EDGE('',*,*,#7390,.F.);
#10234=ORIENTED_EDGE('',*,*,#7391,.F.);
#10235=ORIENTED_EDGE('',*,*,#7216,.T.);
#10236=ORIENTED_EDGE('',*,*,#7154,.T.);
#10237=ORIENTED_EDGE('',*,*,#7213,.T.);
#10238=ORIENTED_EDGE('',*,*,#7183,.T.);
#10239=ORIENTED_EDGE('',*,*,#7272,.T.);
#10240=ORIENTED_EDGE('',*,*,#6727,.T.);
#10241=ORIENTED_EDGE('',*,*,#7269,.T.);
#10242=ORIENTED_EDGE('',*,*,#6756,.T.);
#10243=ORIENTED_EDGE('',*,*,#7392,.F.);
#10244=ORIENTED_EDGE('',*,*,#7393,.F.);
#10245=ORIENTED_EDGE('',*,*,#7394,.F.);
#10246=ORIENTED_EDGE('',*,*,#7395,.F.);
#10247=ORIENTED_EDGE('',*,*,#7396,.F.);
#10248=ORIENTED_EDGE('',*,*,#7397,.F.);
#10249=ORIENTED_EDGE('',*,*,#7398,.F.);
#10250=ORIENTED_EDGE('',*,*,#7350,.F.);
#10251=ORIENTED_EDGE('',*,*,#7399,.T.);
#10252=ORIENTED_EDGE('',*,*,#7389,.T.);
#10253=ORIENTED_EDGE('',*,*,#7386,.F.);
#10254=ORIENTED_EDGE('',*,*,#7331,.F.);
#10255=ORIENTED_EDGE('',*,*,#7400,.F.);
#10256=ORIENTED_EDGE('',*,*,#7390,.T.);
#10257=ORIENTED_EDGE('',*,*,#7399,.F.);
#10258=ORIENTED_EDGE('',*,*,#7349,.F.);
#10259=ORIENTED_EDGE('',*,*,#7401,.F.);
#10260=ORIENTED_EDGE('',*,*,#7402,.T.);
#10261=ORIENTED_EDGE('',*,*,#7403,.F.);
#10262=ORIENTED_EDGE('',*,*,#7319,.F.);
#10263=ORIENTED_EDGE('',*,*,#7404,.F.);
#10264=ORIENTED_EDGE('',*,*,#7320,.F.);
#10265=ORIENTED_EDGE('',*,*,#7403,.T.);
#10266=ORIENTED_EDGE('',*,*,#7405,.T.);
#10267=ORIENTED_EDGE('',*,*,#7406,.F.);
#10268=ORIENTED_EDGE('',*,*,#7407,.F.);
#10269=ORIENTED_EDGE('',*,*,#7408,.F.);
#10270=ORIENTED_EDGE('',*,*,#7409,.F.);
#10271=ORIENTED_EDGE('',*,*,#7410,.F.);
#10272=ORIENTED_EDGE('',*,*,#7411,.F.);
#10273=ORIENTED_EDGE('',*,*,#7412,.F.);
#10274=ORIENTED_EDGE('',*,*,#7413,.F.);
#10275=ORIENTED_EDGE('',*,*,#7414,.F.);
#10276=ORIENTED_EDGE('',*,*,#7415,.F.);
#10277=ORIENTED_EDGE('',*,*,#7406,.T.);
#10278=ORIENTED_EDGE('',*,*,#7416,.T.);
#10279=ORIENTED_EDGE('',*,*,#7417,.F.);
#10280=ORIENTED_EDGE('',*,*,#7416,.F.);
#10281=ORIENTED_EDGE('',*,*,#7405,.F.);
#10282=ORIENTED_EDGE('',*,*,#7402,.F.);
#10283=ORIENTED_EDGE('',*,*,#7240,.T.);
#10284=ORIENTED_EDGE('',*,*,#6971,.T.);
#10285=ORIENTED_EDGE('',*,*,#7237,.T.);
#10286=ORIENTED_EDGE('',*,*,#7000,.T.);
#10287=ORIENTED_EDGE('',*,*,#7264,.T.);
#10288=ORIENTED_EDGE('',*,*,#6788,.T.);
#10289=ORIENTED_EDGE('',*,*,#7261,.T.);
#10290=ORIENTED_EDGE('',*,*,#6817,.T.);
#10291=ORIENTED_EDGE('',*,*,#7394,.T.);
#10292=ORIENTED_EDGE('',*,*,#7418,.T.);
#10293=ORIENTED_EDGE('',*,*,#7355,.T.);
#10294=ORIENTED_EDGE('',*,*,#7419,.T.);
#10295=ORIENTED_EDGE('',*,*,#7393,.T.);
#10296=ORIENTED_EDGE('',*,*,#7420,.F.);
#10297=ORIENTED_EDGE('',*,*,#7421,.F.);
#10298=ORIENTED_EDGE('',*,*,#7418,.F.);
#10299=ORIENTED_EDGE('',*,*,#7392,.T.);
#10300=ORIENTED_EDGE('',*,*,#7330,.F.);
#10301=ORIENTED_EDGE('',*,*,#7422,.T.);
#10302=ORIENTED_EDGE('',*,*,#7420,.T.);
#10303=ORIENTED_EDGE('',*,*,#7273,.T.);
#10304=ORIENTED_EDGE('',*,*,#7333,.F.);
#10305=ORIENTED_EDGE('',*,*,#7385,.T.);
#10306=ORIENTED_EDGE('',*,*,#7388,.T.);
#10307=ORIENTED_EDGE('',*,*,#7423,.T.);
#10308=ORIENTED_EDGE('',*,*,#7424,.T.);
#10309=ORIENTED_EDGE('',*,*,#7423,.F.);
#10310=ORIENTED_EDGE('',*,*,#7391,.T.);
#10311=ORIENTED_EDGE('',*,*,#7400,.T.);
#10312=ORIENTED_EDGE('',*,*,#7348,.F.);
#10313=ORIENTED_EDGE('',*,*,#7307,.T.);
#10314=ORIENTED_EDGE('',*,*,#7310,.T.);
#10315=ORIENTED_EDGE('',*,*,#7304,.T.);
#10316=ORIENTED_EDGE('',*,*,#7425,.F.);
#10317=ORIENTED_EDGE('',*,*,#7414,.T.);
#10318=ORIENTED_EDGE('',*,*,#7417,.T.);
#10319=ORIENTED_EDGE('',*,*,#7401,.T.);
#10320=ORIENTED_EDGE('',*,*,#7318,.F.);
#10321=ORIENTED_EDGE('',*,*,#7288,.T.);
#10322=ORIENTED_EDGE('',*,*,#7291,.T.);
#10323=ORIENTED_EDGE('',*,*,#7404,.T.);
#10324=ORIENTED_EDGE('',*,*,#7426,.T.);
#10325=ORIENTED_EDGE('',*,*,#7427,.F.);
#10326=ORIENTED_EDGE('',*,*,#7321,.F.);
#10327=ORIENTED_EDGE('',*,*,#7413,.T.);
#10328=ORIENTED_EDGE('',*,*,#7428,.F.);
#10329=ORIENTED_EDGE('',*,*,#7429,.F.);
#10330=ORIENTED_EDGE('',*,*,#7426,.F.);
#10331=ORIENTED_EDGE('',*,*,#7293,.T.);
#10332=ORIENTED_EDGE('',*,*,#7384,.T.);
#10333=ORIENTED_EDGE('',*,*,#7381,.T.);
#10334=ORIENTED_EDGE('',*,*,#7368,.T.);
#10335=ORIENTED_EDGE('',*,*,#7430,.T.);
#10336=ORIENTED_EDGE('',*,*,#7431,.T.);
#10337=ORIENTED_EDGE('',*,*,#7407,.T.);
#10338=ORIENTED_EDGE('',*,*,#7415,.T.);
#10339=ORIENTED_EDGE('',*,*,#7425,.T.);
#10340=ORIENTED_EDGE('',*,*,#7306,.T.);
#10341=ORIENTED_EDGE('',*,*,#7197,.T.);
#10342=ORIENTED_EDGE('',*,*,#7412,.T.);
#10343=ORIENTED_EDGE('',*,*,#7432,.T.);
#10344=ORIENTED_EDGE('',*,*,#7317,.F.);
#10345=ORIENTED_EDGE('',*,*,#7428,.T.);
#10346=ORIENTED_EDGE('',*,*,#7411,.T.);
#10347=ORIENTED_EDGE('',*,*,#7433,.F.);
#10348=ORIENTED_EDGE('',*,*,#7434,.F.);
#10349=ORIENTED_EDGE('',*,*,#7366,.F.);
#10350=ORIENTED_EDGE('',*,*,#7435,.F.);
#10351=ORIENTED_EDGE('',*,*,#7432,.F.);
#10352=ORIENTED_EDGE('',*,*,#7410,.T.);
#10353=ORIENTED_EDGE('',*,*,#7436,.T.);
#10354=ORIENTED_EDGE('',*,*,#7362,.T.);
#10355=ORIENTED_EDGE('',*,*,#7433,.T.);
#10356=ORIENTED_EDGE('',*,*,#7395,.T.);
#10357=ORIENTED_EDGE('',*,*,#7419,.F.);
#10358=ORIENTED_EDGE('',*,*,#7437,.F.);
#10359=ORIENTED_EDGE('',*,*,#7375,.F.);
#10360=ORIENTED_EDGE('',*,*,#7372,.F.);
#10361=ORIENTED_EDGE('',*,*,#7438,.F.);
#10362=ORIENTED_EDGE('',*,*,#7439,.F.);
#10363=ORIENTED_EDGE('',*,*,#7397,.T.);
#10364=ORIENTED_EDGE('',*,*,#7440,.F.);
#10365=ORIENTED_EDGE('',*,*,#7441,.F.);
#10366=ORIENTED_EDGE('',*,*,#7442,.F.);
#10367=ORIENTED_EDGE('',*,*,#7396,.T.);
#10368=ORIENTED_EDGE('',*,*,#7439,.T.);
#10369=ORIENTED_EDGE('',*,*,#7343,.F.);
#10370=ORIENTED_EDGE('',*,*,#7440,.T.);
#10371=ORIENTED_EDGE('',*,*,#7409,.T.);
#10372=ORIENTED_EDGE('',*,*,#7443,.F.);
#10373=ORIENTED_EDGE('',*,*,#7444,.F.);
#10374=ORIENTED_EDGE('',*,*,#7436,.F.);
#10375=ORIENTED_EDGE('',*,*,#7376,.F.);
#10376=ORIENTED_EDGE('',*,*,#7437,.T.);
#10377=ORIENTED_EDGE('',*,*,#7378,.F.);
#10378=ORIENTED_EDGE('',*,*,#7421,.T.);
#10379=ORIENTED_EDGE('',*,*,#7422,.F.);
#10380=ORIENTED_EDGE('',*,*,#7329,.F.);
#10381=ORIENTED_EDGE('',*,*,#7371,.F.);
#10382=ORIENTED_EDGE('',*,*,#7352,.F.);
#10383=ORIENTED_EDGE('',*,*,#7445,.T.);
#10384=ORIENTED_EDGE('',*,*,#7441,.T.);
#10385=ORIENTED_EDGE('',*,*,#7380,.T.);
#10386=ORIENTED_EDGE('',*,*,#7438,.T.);
#10387=ORIENTED_EDGE('',*,*,#7398,.T.);
#10388=ORIENTED_EDGE('',*,*,#7442,.T.);
#10389=ORIENTED_EDGE('',*,*,#7445,.F.);
#10390=ORIENTED_EDGE('',*,*,#7351,.F.);
#10391=ORIENTED_EDGE('',*,*,#7365,.F.);
#10392=ORIENTED_EDGE('',*,*,#7322,.F.);
#10393=ORIENTED_EDGE('',*,*,#7427,.T.);
#10394=ORIENTED_EDGE('',*,*,#7429,.T.);
#10395=ORIENTED_EDGE('',*,*,#7379,.T.);
#10396=ORIENTED_EDGE('',*,*,#7435,.T.);
#10397=ORIENTED_EDGE('',*,*,#7408,.T.);
#10398=ORIENTED_EDGE('',*,*,#7431,.F.);
#10399=ORIENTED_EDGE('',*,*,#7446,.T.);
#10400=ORIENTED_EDGE('',*,*,#7443,.T.);
#10401=ORIENTED_EDGE('',*,*,#7367,.F.);
#10402=ORIENTED_EDGE('',*,*,#7434,.T.);
#10403=ORIENTED_EDGE('',*,*,#7383,.F.);
#10404=ORIENTED_EDGE('',*,*,#7444,.T.);
#10405=ORIENTED_EDGE('',*,*,#7446,.F.);
#10406=ORIENTED_EDGE('',*,*,#7430,.F.);
#10407=ORIENTED_EDGE('',*,*,#7447,.F.);
#10408=ORIENTED_EDGE('',*,*,#7448,.T.);
#10409=ORIENTED_EDGE('',*,*,#7449,.T.);
#10410=ORIENTED_EDGE('',*,*,#7448,.F.);
#10411=ORIENTED_EDGE('',*,*,#7449,.F.);
#10412=ORIENTED_EDGE('',*,*,#7374,.F.);
#10413=ORIENTED_EDGE('',*,*,#7424,.F.);
#10414=ORIENTED_EDGE('',*,*,#6884,.T.);
#10415=ORIENTED_EDGE('',*,*,#7128,.T.);
#10416=ORIENTED_EDGE('',*,*,#7006,.T.);
#10417=ORIENTED_EDGE('',*,*,#6945,.T.);
#10418=ORIENTED_EDGE('',*,*,#6762,.T.);
#10419=ORIENTED_EDGE('',*,*,#6823,.T.);
#10420=ORIENTED_EDGE('',*,*,#6701,.T.);
#10421=ORIENTED_EDGE('',*,*,#7067,.T.);
#10422=ORIENTED_EDGE('',*,*,#7447,.T.);
#10423=ORIENTED_EDGE('',*,*,#7208,.T.);
#10424=ORIENTED_EDGE('',*,*,#7206,.T.);
#10425=ORIENTED_EDGE('',*,*,#7204,.T.);
#10426=ORIENTED_EDGE('',*,*,#7202,.T.);
#10427=ORIENTED_EDGE('',*,*,#7450,.T.);
#10428=ORIENTED_EDGE('',*,*,#7451,.T.);
#10429=ORIENTED_EDGE('',*,*,#7452,.T.);
#10430=ORIENTED_EDGE('',*,*,#7453,.T.);
#10431=ORIENTED_EDGE('',*,*,#7454,.F.);
#10432=ORIENTED_EDGE('',*,*,#7453,.F.);
#10433=ORIENTED_EDGE('',*,*,#7455,.T.);
#10434=ORIENTED_EDGE('',*,*,#7456,.T.);
#10435=ORIENTED_EDGE('',*,*,#7457,.T.);
#10436=ORIENTED_EDGE('',*,*,#7458,.T.);
#10437=ORIENTED_EDGE('',*,*,#7450,.F.);
#10438=ORIENTED_EDGE('',*,*,#7459,.T.);
#10439=ORIENTED_EDGE('',*,*,#7460,.T.);
#10440=ORIENTED_EDGE('',*,*,#7461,.T.);
#10441=ORIENTED_EDGE('',*,*,#7457,.F.);
#10442=ORIENTED_EDGE('',*,*,#7462,.T.);
#10443=ORIENTED_EDGE('',*,*,#7463,.T.);
#10444=ORIENTED_EDGE('',*,*,#7464,.T.);
#10445=ORIENTED_EDGE('',*,*,#7460,.F.);
#10446=ORIENTED_EDGE('',*,*,#7465,.T.);
#10447=ORIENTED_EDGE('',*,*,#7466,.T.);
#10448=ORIENTED_EDGE('',*,*,#7467,.T.);
#10449=ORIENTED_EDGE('',*,*,#7463,.F.);
#10450=ORIENTED_EDGE('',*,*,#7468,.T.);
#10451=ORIENTED_EDGE('',*,*,#7469,.T.);
#10452=ORIENTED_EDGE('',*,*,#7470,.T.);
#10453=ORIENTED_EDGE('',*,*,#7466,.F.);
#10454=ORIENTED_EDGE('',*,*,#7471,.T.);
#10455=ORIENTED_EDGE('',*,*,#7472,.F.);
#10456=ORIENTED_EDGE('',*,*,#7473,.T.);
#10457=ORIENTED_EDGE('',*,*,#7474,.F.);
#10458=ORIENTED_EDGE('',*,*,#7475,.T.);
#10459=ORIENTED_EDGE('',*,*,#7476,.T.);
#10460=ORIENTED_EDGE('',*,*,#7477,.T.);
#10461=ORIENTED_EDGE('',*,*,#7478,.F.);
#10462=ORIENTED_EDGE('',*,*,#7479,.F.);
#10463=ORIENTED_EDGE('',*,*,#7480,.T.);
#10464=ORIENTED_EDGE('',*,*,#7481,.T.);
#10465=ORIENTED_EDGE('',*,*,#7476,.F.);
#10466=ORIENTED_EDGE('',*,*,#7482,.F.);
#10467=ORIENTED_EDGE('',*,*,#7483,.T.);
#10468=ORIENTED_EDGE('',*,*,#7484,.T.);
#10469=ORIENTED_EDGE('',*,*,#7480,.F.);
#10470=ORIENTED_EDGE('',*,*,#7485,.F.);
#10471=ORIENTED_EDGE('',*,*,#7486,.T.);
#10472=ORIENTED_EDGE('',*,*,#7487,.T.);
#10473=ORIENTED_EDGE('',*,*,#7483,.F.);
#10474=ORIENTED_EDGE('',*,*,#7488,.F.);
#10475=ORIENTED_EDGE('',*,*,#7489,.T.);
#10476=ORIENTED_EDGE('',*,*,#7490,.T.);
#10477=ORIENTED_EDGE('',*,*,#7486,.F.);
#10478=ORIENTED_EDGE('',*,*,#7491,.F.);
#10479=ORIENTED_EDGE('',*,*,#7492,.T.);
#10480=ORIENTED_EDGE('',*,*,#7493,.T.);
#10481=ORIENTED_EDGE('',*,*,#7489,.F.);
#10482=ORIENTED_EDGE('',*,*,#7494,.F.);
#10483=ORIENTED_EDGE('',*,*,#7495,.F.);
#10484=ORIENTED_EDGE('',*,*,#7496,.F.);
#10485=ORIENTED_EDGE('',*,*,#7497,.F.);
#10486=ORIENTED_EDGE('',*,*,#7498,.T.);
#10487=ORIENTED_EDGE('',*,*,#7499,.T.);
#10488=ORIENTED_EDGE('',*,*,#7500,.T.);
#10489=ORIENTED_EDGE('',*,*,#7501,.T.);
#10490=ORIENTED_EDGE('',*,*,#7502,.T.);
#10491=ORIENTED_EDGE('',*,*,#7503,.F.);
#10492=ORIENTED_EDGE('',*,*,#7502,.F.);
#10493=ORIENTED_EDGE('',*,*,#7504,.T.);
#10494=ORIENTED_EDGE('',*,*,#7505,.T.);
#10495=ORIENTED_EDGE('',*,*,#7506,.T.);
#10496=ORIENTED_EDGE('',*,*,#7507,.T.);
#10497=ORIENTED_EDGE('',*,*,#7499,.F.);
#10498=ORIENTED_EDGE('',*,*,#7508,.T.);
#10499=ORIENTED_EDGE('',*,*,#7509,.T.);
#10500=ORIENTED_EDGE('',*,*,#7510,.T.);
#10501=ORIENTED_EDGE('',*,*,#7506,.F.);
#10502=ORIENTED_EDGE('',*,*,#7511,.T.);
#10503=ORIENTED_EDGE('',*,*,#7512,.T.);
#10504=ORIENTED_EDGE('',*,*,#7513,.T.);
#10505=ORIENTED_EDGE('',*,*,#7509,.F.);
#10506=ORIENTED_EDGE('',*,*,#7514,.T.);
#10507=ORIENTED_EDGE('',*,*,#7515,.T.);
#10508=ORIENTED_EDGE('',*,*,#7516,.T.);
#10509=ORIENTED_EDGE('',*,*,#7512,.F.);
#10510=ORIENTED_EDGE('',*,*,#7517,.T.);
#10511=ORIENTED_EDGE('',*,*,#7518,.T.);
#10512=ORIENTED_EDGE('',*,*,#7519,.T.);
#10513=ORIENTED_EDGE('',*,*,#7515,.F.);
#10514=ORIENTED_EDGE('',*,*,#7520,.T.);
#10515=ORIENTED_EDGE('',*,*,#7521,.F.);
#10516=ORIENTED_EDGE('',*,*,#7522,.T.);
#10517=ORIENTED_EDGE('',*,*,#7523,.F.);
#10518=ORIENTED_EDGE('',*,*,#7524,.T.);
#10519=ORIENTED_EDGE('',*,*,#7525,.T.);
#10520=ORIENTED_EDGE('',*,*,#7526,.T.);
#10521=ORIENTED_EDGE('',*,*,#7527,.F.);
#10522=ORIENTED_EDGE('',*,*,#7528,.F.);
#10523=ORIENTED_EDGE('',*,*,#7529,.T.);
#10524=ORIENTED_EDGE('',*,*,#7530,.T.);
#10525=ORIENTED_EDGE('',*,*,#7525,.F.);
#10526=ORIENTED_EDGE('',*,*,#7531,.F.);
#10527=ORIENTED_EDGE('',*,*,#7532,.T.);
#10528=ORIENTED_EDGE('',*,*,#7533,.T.);
#10529=ORIENTED_EDGE('',*,*,#7529,.F.);
#10530=ORIENTED_EDGE('',*,*,#7534,.F.);
#10531=ORIENTED_EDGE('',*,*,#7535,.T.);
#10532=ORIENTED_EDGE('',*,*,#7536,.T.);
#10533=ORIENTED_EDGE('',*,*,#7532,.F.);
#10534=ORIENTED_EDGE('',*,*,#7537,.F.);
#10535=ORIENTED_EDGE('',*,*,#7538,.T.);
#10536=ORIENTED_EDGE('',*,*,#7539,.T.);
#10537=ORIENTED_EDGE('',*,*,#7535,.F.);
#10538=ORIENTED_EDGE('',*,*,#7540,.F.);
#10539=ORIENTED_EDGE('',*,*,#7541,.T.);
#10540=ORIENTED_EDGE('',*,*,#7542,.T.);
#10541=ORIENTED_EDGE('',*,*,#7538,.F.);
#10542=ORIENTED_EDGE('',*,*,#7543,.F.);
#10543=ORIENTED_EDGE('',*,*,#7544,.F.);
#10544=ORIENTED_EDGE('',*,*,#7545,.F.);
#10545=ORIENTED_EDGE('',*,*,#7546,.F.);
#10546=ORIENTED_EDGE('',*,*,#7547,.T.);
#10547=ORIENTED_EDGE('',*,*,#7548,.T.);
#10548=ORIENTED_EDGE('',*,*,#7549,.T.);
#10549=ORIENTED_EDGE('',*,*,#7550,.T.);
#10550=ORIENTED_EDGE('',*,*,#7551,.T.);
#10551=ORIENTED_EDGE('',*,*,#7552,.F.);
#10552=ORIENTED_EDGE('',*,*,#7551,.F.);
#10553=ORIENTED_EDGE('',*,*,#7553,.T.);
#10554=ORIENTED_EDGE('',*,*,#7554,.T.);
#10555=ORIENTED_EDGE('',*,*,#7555,.T.);
#10556=ORIENTED_EDGE('',*,*,#7556,.T.);
#10557=ORIENTED_EDGE('',*,*,#7548,.F.);
#10558=ORIENTED_EDGE('',*,*,#7557,.T.);
#10559=ORIENTED_EDGE('',*,*,#7558,.T.);
#10560=ORIENTED_EDGE('',*,*,#7559,.T.);
#10561=ORIENTED_EDGE('',*,*,#7555,.F.);
#10562=ORIENTED_EDGE('',*,*,#7560,.T.);
#10563=ORIENTED_EDGE('',*,*,#7561,.T.);
#10564=ORIENTED_EDGE('',*,*,#7562,.T.);
#10565=ORIENTED_EDGE('',*,*,#7558,.F.);
#10566=ORIENTED_EDGE('',*,*,#7563,.T.);
#10567=ORIENTED_EDGE('',*,*,#7564,.T.);
#10568=ORIENTED_EDGE('',*,*,#7565,.T.);
#10569=ORIENTED_EDGE('',*,*,#7561,.F.);
#10570=ORIENTED_EDGE('',*,*,#7566,.T.);
#10571=ORIENTED_EDGE('',*,*,#7567,.T.);
#10572=ORIENTED_EDGE('',*,*,#7568,.T.);
#10573=ORIENTED_EDGE('',*,*,#7564,.F.);
#10574=ORIENTED_EDGE('',*,*,#7569,.T.);
#10575=ORIENTED_EDGE('',*,*,#7570,.F.);
#10576=ORIENTED_EDGE('',*,*,#7571,.T.);
#10577=ORIENTED_EDGE('',*,*,#7572,.F.);
#10578=ORIENTED_EDGE('',*,*,#7573,.T.);
#10579=ORIENTED_EDGE('',*,*,#7574,.T.);
#10580=ORIENTED_EDGE('',*,*,#7575,.T.);
#10581=ORIENTED_EDGE('',*,*,#7576,.F.);
#10582=ORIENTED_EDGE('',*,*,#7577,.F.);
#10583=ORIENTED_EDGE('',*,*,#7578,.T.);
#10584=ORIENTED_EDGE('',*,*,#7579,.T.);
#10585=ORIENTED_EDGE('',*,*,#7574,.F.);
#10586=ORIENTED_EDGE('',*,*,#7580,.F.);
#10587=ORIENTED_EDGE('',*,*,#7581,.T.);
#10588=ORIENTED_EDGE('',*,*,#7582,.T.);
#10589=ORIENTED_EDGE('',*,*,#7578,.F.);
#10590=ORIENTED_EDGE('',*,*,#7583,.F.);
#10591=ORIENTED_EDGE('',*,*,#7584,.T.);
#10592=ORIENTED_EDGE('',*,*,#7585,.T.);
#10593=ORIENTED_EDGE('',*,*,#7581,.F.);
#10594=ORIENTED_EDGE('',*,*,#7586,.F.);
#10595=ORIENTED_EDGE('',*,*,#7587,.T.);
#10596=ORIENTED_EDGE('',*,*,#7588,.T.);
#10597=ORIENTED_EDGE('',*,*,#7584,.F.);
#10598=ORIENTED_EDGE('',*,*,#7589,.F.);
#10599=ORIENTED_EDGE('',*,*,#7590,.T.);
#10600=ORIENTED_EDGE('',*,*,#7591,.T.);
#10601=ORIENTED_EDGE('',*,*,#7587,.F.);
#10602=ORIENTED_EDGE('',*,*,#7592,.F.);
#10603=ORIENTED_EDGE('',*,*,#7593,.F.);
#10604=ORIENTED_EDGE('',*,*,#7594,.F.);
#10605=ORIENTED_EDGE('',*,*,#7595,.F.);
#10606=ORIENTED_EDGE('',*,*,#7596,.T.);
#10607=ORIENTED_EDGE('',*,*,#7597,.T.);
#10608=ORIENTED_EDGE('',*,*,#7598,.T.);
#10609=ORIENTED_EDGE('',*,*,#7599,.T.);
#10610=ORIENTED_EDGE('',*,*,#7600,.T.);
#10611=ORIENTED_EDGE('',*,*,#7601,.F.);
#10612=ORIENTED_EDGE('',*,*,#7600,.F.);
#10613=ORIENTED_EDGE('',*,*,#7602,.T.);
#10614=ORIENTED_EDGE('',*,*,#7603,.T.);
#10615=ORIENTED_EDGE('',*,*,#7604,.T.);
#10616=ORIENTED_EDGE('',*,*,#7605,.T.);
#10617=ORIENTED_EDGE('',*,*,#7597,.F.);
#10618=ORIENTED_EDGE('',*,*,#7606,.T.);
#10619=ORIENTED_EDGE('',*,*,#7607,.T.);
#10620=ORIENTED_EDGE('',*,*,#7608,.T.);
#10621=ORIENTED_EDGE('',*,*,#7604,.F.);
#10622=ORIENTED_EDGE('',*,*,#7609,.T.);
#10623=ORIENTED_EDGE('',*,*,#7610,.T.);
#10624=ORIENTED_EDGE('',*,*,#7611,.T.);
#10625=ORIENTED_EDGE('',*,*,#7607,.F.);
#10626=ORIENTED_EDGE('',*,*,#7612,.T.);
#10627=ORIENTED_EDGE('',*,*,#7613,.T.);
#10628=ORIENTED_EDGE('',*,*,#7614,.T.);
#10629=ORIENTED_EDGE('',*,*,#7610,.F.);
#10630=ORIENTED_EDGE('',*,*,#7615,.T.);
#10631=ORIENTED_EDGE('',*,*,#7616,.T.);
#10632=ORIENTED_EDGE('',*,*,#7617,.T.);
#10633=ORIENTED_EDGE('',*,*,#7613,.F.);
#10634=ORIENTED_EDGE('',*,*,#7618,.T.);
#10635=ORIENTED_EDGE('',*,*,#7619,.F.);
#10636=ORIENTED_EDGE('',*,*,#7620,.T.);
#10637=ORIENTED_EDGE('',*,*,#7621,.F.);
#10638=ORIENTED_EDGE('',*,*,#7622,.T.);
#10639=ORIENTED_EDGE('',*,*,#7623,.T.);
#10640=ORIENTED_EDGE('',*,*,#7624,.T.);
#10641=ORIENTED_EDGE('',*,*,#7625,.F.);
#10642=ORIENTED_EDGE('',*,*,#7626,.F.);
#10643=ORIENTED_EDGE('',*,*,#7627,.T.);
#10644=ORIENTED_EDGE('',*,*,#7628,.T.);
#10645=ORIENTED_EDGE('',*,*,#7623,.F.);
#10646=ORIENTED_EDGE('',*,*,#7629,.F.);
#10647=ORIENTED_EDGE('',*,*,#7630,.T.);
#10648=ORIENTED_EDGE('',*,*,#7631,.T.);
#10649=ORIENTED_EDGE('',*,*,#7627,.F.);
#10650=ORIENTED_EDGE('',*,*,#7632,.F.);
#10651=ORIENTED_EDGE('',*,*,#7633,.T.);
#10652=ORIENTED_EDGE('',*,*,#7634,.T.);
#10653=ORIENTED_EDGE('',*,*,#7630,.F.);
#10654=ORIENTED_EDGE('',*,*,#7635,.F.);
#10655=ORIENTED_EDGE('',*,*,#7636,.T.);
#10656=ORIENTED_EDGE('',*,*,#7637,.T.);
#10657=ORIENTED_EDGE('',*,*,#7633,.F.);
#10658=ORIENTED_EDGE('',*,*,#7638,.F.);
#10659=ORIENTED_EDGE('',*,*,#7639,.T.);
#10660=ORIENTED_EDGE('',*,*,#7640,.T.);
#10661=ORIENTED_EDGE('',*,*,#7636,.F.);
#10662=ORIENTED_EDGE('',*,*,#7641,.F.);
#10663=ORIENTED_EDGE('',*,*,#7642,.F.);
#10664=ORIENTED_EDGE('',*,*,#7643,.F.);
#10665=ORIENTED_EDGE('',*,*,#7644,.F.);
#10666=ORIENTED_EDGE('',*,*,#7645,.T.);
#10667=ORIENTED_EDGE('',*,*,#7646,.T.);
#10668=ORIENTED_EDGE('',*,*,#7647,.T.);
#10669=ORIENTED_EDGE('',*,*,#7648,.T.);
#10670=ORIENTED_EDGE('',*,*,#7649,.T.);
#10671=ORIENTED_EDGE('',*,*,#7650,.T.);
#10672=ORIENTED_EDGE('',*,*,#7651,.T.);
#10673=ORIENTED_EDGE('',*,*,#7650,.F.);
#10674=ORIENTED_EDGE('',*,*,#7652,.T.);
#10675=ORIENTED_EDGE('',*,*,#7653,.T.);
#10676=ORIENTED_EDGE('',*,*,#7654,.T.);
#10677=ORIENTED_EDGE('',*,*,#7646,.F.);
#10678=ORIENTED_EDGE('',*,*,#7655,.T.);
#10679=ORIENTED_EDGE('',*,*,#7656,.T.);
#10680=ORIENTED_EDGE('',*,*,#7657,.T.);
#10681=ORIENTED_EDGE('',*,*,#7653,.F.);
#10682=ORIENTED_EDGE('',*,*,#7658,.T.);
#10683=ORIENTED_EDGE('',*,*,#7659,.F.);
#10684=ORIENTED_EDGE('',*,*,#7660,.T.);
#10685=ORIENTED_EDGE('',*,*,#7661,.F.);
#10686=ORIENTED_EDGE('',*,*,#7662,.T.);
#10687=ORIENTED_EDGE('',*,*,#7663,.T.);
#10688=ORIENTED_EDGE('',*,*,#7664,.T.);
#10689=ORIENTED_EDGE('',*,*,#7665,.F.);
#10690=ORIENTED_EDGE('',*,*,#7666,.F.);
#10691=ORIENTED_EDGE('',*,*,#7667,.T.);
#10692=ORIENTED_EDGE('',*,*,#7668,.T.);
#10693=ORIENTED_EDGE('',*,*,#7663,.F.);
#10694=ORIENTED_EDGE('',*,*,#7669,.F.);
#10695=ORIENTED_EDGE('',*,*,#7670,.T.);
#10696=ORIENTED_EDGE('',*,*,#7671,.T.);
#10697=ORIENTED_EDGE('',*,*,#7667,.F.);
#10698=ORIENTED_EDGE('',*,*,#7672,.F.);
#10699=ORIENTED_EDGE('',*,*,#7673,.T.);
#10700=ORIENTED_EDGE('',*,*,#7674,.T.);
#10701=ORIENTED_EDGE('',*,*,#7670,.F.);
#10702=ORIENTED_EDGE('',*,*,#7675,.F.);
#10703=ORIENTED_EDGE('',*,*,#7676,.F.);
#10704=ORIENTED_EDGE('',*,*,#7677,.F.);
#10705=ORIENTED_EDGE('',*,*,#7678,.F.);
#10706=ORIENTED_EDGE('',*,*,#7679,.T.);
#10707=ORIENTED_EDGE('',*,*,#7680,.T.);
#10708=ORIENTED_EDGE('',*,*,#7681,.T.);
#10709=ORIENTED_EDGE('',*,*,#7682,.T.);
#10710=ORIENTED_EDGE('',*,*,#7683,.T.);
#10711=ORIENTED_EDGE('',*,*,#7684,.T.);
#10712=ORIENTED_EDGE('',*,*,#7685,.T.);
#10713=ORIENTED_EDGE('',*,*,#7684,.F.);
#10714=ORIENTED_EDGE('',*,*,#7686,.T.);
#10715=ORIENTED_EDGE('',*,*,#7687,.T.);
#10716=ORIENTED_EDGE('',*,*,#7688,.T.);
#10717=ORIENTED_EDGE('',*,*,#7680,.F.);
#10718=ORIENTED_EDGE('',*,*,#7689,.T.);
#10719=ORIENTED_EDGE('',*,*,#7690,.T.);
#10720=ORIENTED_EDGE('',*,*,#7691,.T.);
#10721=ORIENTED_EDGE('',*,*,#7687,.F.);
#10722=ORIENTED_EDGE('',*,*,#7692,.T.);
#10723=ORIENTED_EDGE('',*,*,#7693,.F.);
#10724=ORIENTED_EDGE('',*,*,#7694,.T.);
#10725=ORIENTED_EDGE('',*,*,#7695,.F.);
#10726=ORIENTED_EDGE('',*,*,#7696,.T.);
#10727=ORIENTED_EDGE('',*,*,#7697,.T.);
#10728=ORIENTED_EDGE('',*,*,#7698,.T.);
#10729=ORIENTED_EDGE('',*,*,#7699,.F.);
#10730=ORIENTED_EDGE('',*,*,#7700,.F.);
#10731=ORIENTED_EDGE('',*,*,#7701,.T.);
#10732=ORIENTED_EDGE('',*,*,#7702,.T.);
#10733=ORIENTED_EDGE('',*,*,#7697,.F.);
#10734=ORIENTED_EDGE('',*,*,#7703,.F.);
#10735=ORIENTED_EDGE('',*,*,#7704,.T.);
#10736=ORIENTED_EDGE('',*,*,#7705,.T.);
#10737=ORIENTED_EDGE('',*,*,#7701,.F.);
#10738=ORIENTED_EDGE('',*,*,#7706,.F.);
#10739=ORIENTED_EDGE('',*,*,#7707,.T.);
#10740=ORIENTED_EDGE('',*,*,#7708,.T.);
#10741=ORIENTED_EDGE('',*,*,#7704,.F.);
#10742=ORIENTED_EDGE('',*,*,#7709,.F.);
#10743=ORIENTED_EDGE('',*,*,#7710,.F.);
#10744=ORIENTED_EDGE('',*,*,#7711,.F.);
#10745=ORIENTED_EDGE('',*,*,#7712,.F.);
#10746=ORIENTED_EDGE('',*,*,#7713,.T.);
#10747=ORIENTED_EDGE('',*,*,#7714,.T.);
#10748=ORIENTED_EDGE('',*,*,#7715,.T.);
#10749=ORIENTED_EDGE('',*,*,#7716,.T.);
#10750=ORIENTED_EDGE('',*,*,#7717,.T.);
#10751=ORIENTED_EDGE('',*,*,#7718,.T.);
#10752=ORIENTED_EDGE('',*,*,#7719,.T.);
#10753=ORIENTED_EDGE('',*,*,#7718,.F.);
#10754=ORIENTED_EDGE('',*,*,#7720,.T.);
#10755=ORIENTED_EDGE('',*,*,#7721,.T.);
#10756=ORIENTED_EDGE('',*,*,#7722,.T.);
#10757=ORIENTED_EDGE('',*,*,#7714,.F.);
#10758=ORIENTED_EDGE('',*,*,#7723,.T.);
#10759=ORIENTED_EDGE('',*,*,#7724,.T.);
#10760=ORIENTED_EDGE('',*,*,#7725,.T.);
#10761=ORIENTED_EDGE('',*,*,#7721,.F.);
#10762=ORIENTED_EDGE('',*,*,#7726,.T.);
#10763=ORIENTED_EDGE('',*,*,#7727,.F.);
#10764=ORIENTED_EDGE('',*,*,#7728,.T.);
#10765=ORIENTED_EDGE('',*,*,#7729,.F.);
#10766=ORIENTED_EDGE('',*,*,#7730,.T.);
#10767=ORIENTED_EDGE('',*,*,#7731,.T.);
#10768=ORIENTED_EDGE('',*,*,#7732,.T.);
#10769=ORIENTED_EDGE('',*,*,#7733,.F.);
#10770=ORIENTED_EDGE('',*,*,#7734,.F.);
#10771=ORIENTED_EDGE('',*,*,#7735,.T.);
#10772=ORIENTED_EDGE('',*,*,#7736,.T.);
#10773=ORIENTED_EDGE('',*,*,#7731,.F.);
#10774=ORIENTED_EDGE('',*,*,#7737,.F.);
#10775=ORIENTED_EDGE('',*,*,#7738,.T.);
#10776=ORIENTED_EDGE('',*,*,#7739,.T.);
#10777=ORIENTED_EDGE('',*,*,#7735,.F.);
#10778=ORIENTED_EDGE('',*,*,#7740,.F.);
#10779=ORIENTED_EDGE('',*,*,#7741,.T.);
#10780=ORIENTED_EDGE('',*,*,#7742,.T.);
#10781=ORIENTED_EDGE('',*,*,#7738,.F.);
#10782=ORIENTED_EDGE('',*,*,#7743,.F.);
#10783=ORIENTED_EDGE('',*,*,#7744,.F.);
#10784=ORIENTED_EDGE('',*,*,#7745,.F.);
#10785=ORIENTED_EDGE('',*,*,#7746,.F.);
#10786=ORIENTED_EDGE('',*,*,#7747,.T.);
#10787=ORIENTED_EDGE('',*,*,#7748,.T.);
#10788=ORIENTED_EDGE('',*,*,#7749,.T.);
#10789=ORIENTED_EDGE('',*,*,#7750,.T.);
#10790=ORIENTED_EDGE('',*,*,#7751,.T.);
#10791=ORIENTED_EDGE('',*,*,#7752,.T.);
#10792=ORIENTED_EDGE('',*,*,#7753,.T.);
#10793=ORIENTED_EDGE('',*,*,#7752,.F.);
#10794=ORIENTED_EDGE('',*,*,#7754,.T.);
#10795=ORIENTED_EDGE('',*,*,#7755,.T.);
#10796=ORIENTED_EDGE('',*,*,#7756,.T.);
#10797=ORIENTED_EDGE('',*,*,#7748,.F.);
#10798=ORIENTED_EDGE('',*,*,#7757,.T.);
#10799=ORIENTED_EDGE('',*,*,#7758,.T.);
#10800=ORIENTED_EDGE('',*,*,#7759,.T.);
#10801=ORIENTED_EDGE('',*,*,#7755,.F.);
#10802=ORIENTED_EDGE('',*,*,#7760,.T.);
#10803=ORIENTED_EDGE('',*,*,#7761,.F.);
#10804=ORIENTED_EDGE('',*,*,#7762,.T.);
#10805=ORIENTED_EDGE('',*,*,#7763,.F.);
#10806=ORIENTED_EDGE('',*,*,#7764,.T.);
#10807=ORIENTED_EDGE('',*,*,#7765,.T.);
#10808=ORIENTED_EDGE('',*,*,#7766,.T.);
#10809=ORIENTED_EDGE('',*,*,#7767,.F.);
#10810=ORIENTED_EDGE('',*,*,#7768,.F.);
#10811=ORIENTED_EDGE('',*,*,#7769,.T.);
#10812=ORIENTED_EDGE('',*,*,#7770,.T.);
#10813=ORIENTED_EDGE('',*,*,#7765,.F.);
#10814=ORIENTED_EDGE('',*,*,#7771,.F.);
#10815=ORIENTED_EDGE('',*,*,#7772,.T.);
#10816=ORIENTED_EDGE('',*,*,#7773,.T.);
#10817=ORIENTED_EDGE('',*,*,#7769,.F.);
#10818=ORIENTED_EDGE('',*,*,#7774,.F.);
#10819=ORIENTED_EDGE('',*,*,#7775,.T.);
#10820=ORIENTED_EDGE('',*,*,#7776,.T.);
#10821=ORIENTED_EDGE('',*,*,#7772,.F.);
#10822=ORIENTED_EDGE('',*,*,#7777,.F.);
#10823=ORIENTED_EDGE('',*,*,#7778,.F.);
#10824=ORIENTED_EDGE('',*,*,#7779,.F.);
#10825=ORIENTED_EDGE('',*,*,#7780,.F.);
#10826=ORIENTED_EDGE('',*,*,#7781,.T.);
#10827=ORIENTED_EDGE('',*,*,#7750,.F.);
#10828=ORIENTED_EDGE('',*,*,#7782,.T.);
#10829=ORIENTED_EDGE('',*,*,#7767,.T.);
#10830=ORIENTED_EDGE('',*,*,#7783,.T.);
#10831=ORIENTED_EDGE('',*,*,#7778,.T.);
#10832=ORIENTED_EDGE('',*,*,#7784,.T.);
#10833=ORIENTED_EDGE('',*,*,#7775,.F.);
#10834=ORIENTED_EDGE('',*,*,#7785,.F.);
#10835=ORIENTED_EDGE('',*,*,#7783,.F.);
#10836=ORIENTED_EDGE('',*,*,#7766,.F.);
#10837=ORIENTED_EDGE('',*,*,#7770,.F.);
#10838=ORIENTED_EDGE('',*,*,#7773,.F.);
#10839=ORIENTED_EDGE('',*,*,#7776,.F.);
#10840=ORIENTED_EDGE('',*,*,#7784,.F.);
#10841=ORIENTED_EDGE('',*,*,#7781,.F.);
#10842=ORIENTED_EDGE('',*,*,#7786,.F.);
#10843=ORIENTED_EDGE('',*,*,#7762,.F.);
#10844=ORIENTED_EDGE('',*,*,#7787,.F.);
#10845=ORIENTED_EDGE('',*,*,#7760,.F.);
#10846=ORIENTED_EDGE('',*,*,#7757,.F.);
#10847=ORIENTED_EDGE('',*,*,#7754,.F.);
#10848=ORIENTED_EDGE('',*,*,#7751,.F.);
#10849=ORIENTED_EDGE('',*,*,#7782,.F.);
#10850=ORIENTED_EDGE('',*,*,#7749,.F.);
#10851=ORIENTED_EDGE('',*,*,#7756,.F.);
#10852=ORIENTED_EDGE('',*,*,#7759,.F.);
#10853=ORIENTED_EDGE('',*,*,#7788,.F.);
#10854=ORIENTED_EDGE('',*,*,#7764,.F.);
#10855=ORIENTED_EDGE('',*,*,#7789,.F.);
#10856=ORIENTED_EDGE('',*,*,#7779,.T.);
#10857=ORIENTED_EDGE('',*,*,#7785,.T.);
#10858=ORIENTED_EDGE('',*,*,#7777,.T.);
#10859=ORIENTED_EDGE('',*,*,#7774,.T.);
#10860=ORIENTED_EDGE('',*,*,#7771,.T.);
#10861=ORIENTED_EDGE('',*,*,#7768,.T.);
#10862=ORIENTED_EDGE('',*,*,#7761,.T.);
#10863=ORIENTED_EDGE('',*,*,#7788,.T.);
#10864=ORIENTED_EDGE('',*,*,#7758,.F.);
#10865=ORIENTED_EDGE('',*,*,#7787,.T.);
#10866=ORIENTED_EDGE('',*,*,#7716,.F.);
#10867=ORIENTED_EDGE('',*,*,#7790,.T.);
#10868=ORIENTED_EDGE('',*,*,#7733,.T.);
#10869=ORIENTED_EDGE('',*,*,#7791,.T.);
#10870=ORIENTED_EDGE('',*,*,#7744,.T.);
#10871=ORIENTED_EDGE('',*,*,#7792,.T.);
#10872=ORIENTED_EDGE('',*,*,#7741,.F.);
#10873=ORIENTED_EDGE('',*,*,#7793,.F.);
#10874=ORIENTED_EDGE('',*,*,#7791,.F.);
#10875=ORIENTED_EDGE('',*,*,#7732,.F.);
#10876=ORIENTED_EDGE('',*,*,#7736,.F.);
#10877=ORIENTED_EDGE('',*,*,#7739,.F.);
#10878=ORIENTED_EDGE('',*,*,#7742,.F.);
#10879=ORIENTED_EDGE('',*,*,#7792,.F.);
#10880=ORIENTED_EDGE('',*,*,#7747,.F.);
#10881=ORIENTED_EDGE('',*,*,#7794,.F.);
#10882=ORIENTED_EDGE('',*,*,#7728,.F.);
#10883=ORIENTED_EDGE('',*,*,#7795,.F.);
#10884=ORIENTED_EDGE('',*,*,#7726,.F.);
#10885=ORIENTED_EDGE('',*,*,#7723,.F.);
#10886=ORIENTED_EDGE('',*,*,#7720,.F.);
#10887=ORIENTED_EDGE('',*,*,#7717,.F.);
#10888=ORIENTED_EDGE('',*,*,#7790,.F.);
#10889=ORIENTED_EDGE('',*,*,#7715,.F.);
#10890=ORIENTED_EDGE('',*,*,#7722,.F.);
#10891=ORIENTED_EDGE('',*,*,#7725,.F.);
#10892=ORIENTED_EDGE('',*,*,#7796,.F.);
#10893=ORIENTED_EDGE('',*,*,#7730,.F.);
#10894=ORIENTED_EDGE('',*,*,#7797,.F.);
#10895=ORIENTED_EDGE('',*,*,#7745,.T.);
#10896=ORIENTED_EDGE('',*,*,#7793,.T.);
#10897=ORIENTED_EDGE('',*,*,#7743,.T.);
#10898=ORIENTED_EDGE('',*,*,#7740,.T.);
#10899=ORIENTED_EDGE('',*,*,#7737,.T.);
#10900=ORIENTED_EDGE('',*,*,#7734,.T.);
#10901=ORIENTED_EDGE('',*,*,#7727,.T.);
#10902=ORIENTED_EDGE('',*,*,#7796,.T.);
#10903=ORIENTED_EDGE('',*,*,#7724,.F.);
#10904=ORIENTED_EDGE('',*,*,#7795,.T.);
#10905=ORIENTED_EDGE('',*,*,#7682,.F.);
#10906=ORIENTED_EDGE('',*,*,#7798,.T.);
#10907=ORIENTED_EDGE('',*,*,#7699,.T.);
#10908=ORIENTED_EDGE('',*,*,#7799,.T.);
#10909=ORIENTED_EDGE('',*,*,#7710,.T.);
#10910=ORIENTED_EDGE('',*,*,#7800,.T.);
#10911=ORIENTED_EDGE('',*,*,#7707,.F.);
#10912=ORIENTED_EDGE('',*,*,#7801,.F.);
#10913=ORIENTED_EDGE('',*,*,#7799,.F.);
#10914=ORIENTED_EDGE('',*,*,#7698,.F.);
#10915=ORIENTED_EDGE('',*,*,#7702,.F.);
#10916=ORIENTED_EDGE('',*,*,#7705,.F.);
#10917=ORIENTED_EDGE('',*,*,#7708,.F.);
#10918=ORIENTED_EDGE('',*,*,#7800,.F.);
#10919=ORIENTED_EDGE('',*,*,#7713,.F.);
#10920=ORIENTED_EDGE('',*,*,#7802,.F.);
#10921=ORIENTED_EDGE('',*,*,#7694,.F.);
#10922=ORIENTED_EDGE('',*,*,#7803,.F.);
#10923=ORIENTED_EDGE('',*,*,#7692,.F.);
#10924=ORIENTED_EDGE('',*,*,#7689,.F.);
#10925=ORIENTED_EDGE('',*,*,#7686,.F.);
#10926=ORIENTED_EDGE('',*,*,#7683,.F.);
#10927=ORIENTED_EDGE('',*,*,#7798,.F.);
#10928=ORIENTED_EDGE('',*,*,#7681,.F.);
#10929=ORIENTED_EDGE('',*,*,#7688,.F.);
#10930=ORIENTED_EDGE('',*,*,#7691,.F.);
#10931=ORIENTED_EDGE('',*,*,#7804,.F.);
#10932=ORIENTED_EDGE('',*,*,#7696,.F.);
#10933=ORIENTED_EDGE('',*,*,#7805,.F.);
#10934=ORIENTED_EDGE('',*,*,#7711,.T.);
#10935=ORIENTED_EDGE('',*,*,#7801,.T.);
#10936=ORIENTED_EDGE('',*,*,#7709,.T.);
#10937=ORIENTED_EDGE('',*,*,#7706,.T.);
#10938=ORIENTED_EDGE('',*,*,#7703,.T.);
#10939=ORIENTED_EDGE('',*,*,#7700,.T.);
#10940=ORIENTED_EDGE('',*,*,#7693,.T.);
#10941=ORIENTED_EDGE('',*,*,#7804,.T.);
#10942=ORIENTED_EDGE('',*,*,#7690,.F.);
#10943=ORIENTED_EDGE('',*,*,#7803,.T.);
#10944=ORIENTED_EDGE('',*,*,#7648,.F.);
#10945=ORIENTED_EDGE('',*,*,#7806,.T.);
#10946=ORIENTED_EDGE('',*,*,#7665,.T.);
#10947=ORIENTED_EDGE('',*,*,#7807,.T.);
#10948=ORIENTED_EDGE('',*,*,#7676,.T.);
#10949=ORIENTED_EDGE('',*,*,#7808,.T.);
#10950=ORIENTED_EDGE('',*,*,#7673,.F.);
#10951=ORIENTED_EDGE('',*,*,#7809,.F.);
#10952=ORIENTED_EDGE('',*,*,#7807,.F.);
#10953=ORIENTED_EDGE('',*,*,#7664,.F.);
#10954=ORIENTED_EDGE('',*,*,#7668,.F.);
#10955=ORIENTED_EDGE('',*,*,#7671,.F.);
#10956=ORIENTED_EDGE('',*,*,#7674,.F.);
#10957=ORIENTED_EDGE('',*,*,#7808,.F.);
#10958=ORIENTED_EDGE('',*,*,#7679,.F.);
#10959=ORIENTED_EDGE('',*,*,#7810,.F.);
#10960=ORIENTED_EDGE('',*,*,#7660,.F.);
#10961=ORIENTED_EDGE('',*,*,#7811,.F.);
#10962=ORIENTED_EDGE('',*,*,#7658,.F.);
#10963=ORIENTED_EDGE('',*,*,#7655,.F.);
#10964=ORIENTED_EDGE('',*,*,#7652,.F.);
#10965=ORIENTED_EDGE('',*,*,#7649,.F.);
#10966=ORIENTED_EDGE('',*,*,#7806,.F.);
#10967=ORIENTED_EDGE('',*,*,#7647,.F.);
#10968=ORIENTED_EDGE('',*,*,#7654,.F.);
#10969=ORIENTED_EDGE('',*,*,#7657,.F.);
#10970=ORIENTED_EDGE('',*,*,#7812,.F.);
#10971=ORIENTED_EDGE('',*,*,#7662,.F.);
#10972=ORIENTED_EDGE('',*,*,#7813,.F.);
#10973=ORIENTED_EDGE('',*,*,#7677,.T.);
#10974=ORIENTED_EDGE('',*,*,#7809,.T.);
#10975=ORIENTED_EDGE('',*,*,#7675,.T.);
#10976=ORIENTED_EDGE('',*,*,#7672,.T.);
#10977=ORIENTED_EDGE('',*,*,#7669,.T.);
#10978=ORIENTED_EDGE('',*,*,#7666,.T.);
#10979=ORIENTED_EDGE('',*,*,#7659,.T.);
#10980=ORIENTED_EDGE('',*,*,#7812,.T.);
#10981=ORIENTED_EDGE('',*,*,#7656,.F.);
#10982=ORIENTED_EDGE('',*,*,#7811,.T.);
#10983=ORIENTED_EDGE('',*,*,#7651,.F.);
#10984=ORIENTED_EDGE('',*,*,#7685,.F.);
#10985=ORIENTED_EDGE('',*,*,#7753,.F.);
#10986=ORIENTED_EDGE('',*,*,#7719,.F.);
#10987=ORIENTED_EDGE('',*,*,#7599,.F.);
#10988=ORIENTED_EDGE('',*,*,#7814,.T.);
#10989=ORIENTED_EDGE('',*,*,#7625,.T.);
#10990=ORIENTED_EDGE('',*,*,#7815,.T.);
#10991=ORIENTED_EDGE('',*,*,#7602,.F.);
#10992=ORIENTED_EDGE('',*,*,#7642,.T.);
#10993=ORIENTED_EDGE('',*,*,#7816,.T.);
#10994=ORIENTED_EDGE('',*,*,#7639,.F.);
#10995=ORIENTED_EDGE('',*,*,#7817,.F.);
#10996=ORIENTED_EDGE('',*,*,#7815,.F.);
#10997=ORIENTED_EDGE('',*,*,#7624,.F.);
#10998=ORIENTED_EDGE('',*,*,#7628,.F.);
#10999=ORIENTED_EDGE('',*,*,#7631,.F.);
#11000=ORIENTED_EDGE('',*,*,#7634,.F.);
#11001=ORIENTED_EDGE('',*,*,#7637,.F.);
#11002=ORIENTED_EDGE('',*,*,#7640,.F.);
#11003=ORIENTED_EDGE('',*,*,#7816,.F.);
#11004=ORIENTED_EDGE('',*,*,#7645,.F.);
#11005=ORIENTED_EDGE('',*,*,#7818,.F.);
#11006=ORIENTED_EDGE('',*,*,#7620,.F.);
#11007=ORIENTED_EDGE('',*,*,#7819,.F.);
#11008=ORIENTED_EDGE('',*,*,#7618,.F.);
#11009=ORIENTED_EDGE('',*,*,#7615,.F.);
#11010=ORIENTED_EDGE('',*,*,#7612,.F.);
#11011=ORIENTED_EDGE('',*,*,#7609,.F.);
#11012=ORIENTED_EDGE('',*,*,#7606,.F.);
#11013=ORIENTED_EDGE('',*,*,#7603,.F.);
#11014=ORIENTED_EDGE('',*,*,#7814,.F.);
#11015=ORIENTED_EDGE('',*,*,#7598,.F.);
#11016=ORIENTED_EDGE('',*,*,#7605,.F.);
#11017=ORIENTED_EDGE('',*,*,#7608,.F.);
#11018=ORIENTED_EDGE('',*,*,#7611,.F.);
#11019=ORIENTED_EDGE('',*,*,#7614,.F.);
#11020=ORIENTED_EDGE('',*,*,#7617,.F.);
#11021=ORIENTED_EDGE('',*,*,#7820,.F.);
#11022=ORIENTED_EDGE('',*,*,#7622,.F.);
#11023=ORIENTED_EDGE('',*,*,#7821,.F.);
#11024=ORIENTED_EDGE('',*,*,#7643,.T.);
#11025=ORIENTED_EDGE('',*,*,#7817,.T.);
#11026=ORIENTED_EDGE('',*,*,#7641,.T.);
#11027=ORIENTED_EDGE('',*,*,#7638,.T.);
#11028=ORIENTED_EDGE('',*,*,#7635,.T.);
#11029=ORIENTED_EDGE('',*,*,#7632,.T.);
#11030=ORIENTED_EDGE('',*,*,#7629,.T.);
#11031=ORIENTED_EDGE('',*,*,#7626,.T.);
#11032=ORIENTED_EDGE('',*,*,#7619,.T.);
#11033=ORIENTED_EDGE('',*,*,#7820,.T.);
#11034=ORIENTED_EDGE('',*,*,#7616,.F.);
#11035=ORIENTED_EDGE('',*,*,#7819,.T.);
#11036=ORIENTED_EDGE('',*,*,#7550,.F.);
#11037=ORIENTED_EDGE('',*,*,#7822,.T.);
#11038=ORIENTED_EDGE('',*,*,#7576,.T.);
#11039=ORIENTED_EDGE('',*,*,#7823,.T.);
#11040=ORIENTED_EDGE('',*,*,#7553,.F.);
#11041=ORIENTED_EDGE('',*,*,#7593,.T.);
#11042=ORIENTED_EDGE('',*,*,#7824,.T.);
#11043=ORIENTED_EDGE('',*,*,#7590,.F.);
#11044=ORIENTED_EDGE('',*,*,#7825,.F.);
#11045=ORIENTED_EDGE('',*,*,#7823,.F.);
#11046=ORIENTED_EDGE('',*,*,#7575,.F.);
#11047=ORIENTED_EDGE('',*,*,#7579,.F.);
#11048=ORIENTED_EDGE('',*,*,#7582,.F.);
#11049=ORIENTED_EDGE('',*,*,#7585,.F.);
#11050=ORIENTED_EDGE('',*,*,#7588,.F.);
#11051=ORIENTED_EDGE('',*,*,#7591,.F.);
#11052=ORIENTED_EDGE('',*,*,#7824,.F.);
#11053=ORIENTED_EDGE('',*,*,#7596,.F.);
#11054=ORIENTED_EDGE('',*,*,#7826,.F.);
#11055=ORIENTED_EDGE('',*,*,#7571,.F.);
#11056=ORIENTED_EDGE('',*,*,#7827,.F.);
#11057=ORIENTED_EDGE('',*,*,#7569,.F.);
#11058=ORIENTED_EDGE('',*,*,#7566,.F.);
#11059=ORIENTED_EDGE('',*,*,#7563,.F.);
#11060=ORIENTED_EDGE('',*,*,#7560,.F.);
#11061=ORIENTED_EDGE('',*,*,#7557,.F.);
#11062=ORIENTED_EDGE('',*,*,#7554,.F.);
#11063=ORIENTED_EDGE('',*,*,#7822,.F.);
#11064=ORIENTED_EDGE('',*,*,#7549,.F.);
#11065=ORIENTED_EDGE('',*,*,#7556,.F.);
#11066=ORIENTED_EDGE('',*,*,#7559,.F.);
#11067=ORIENTED_EDGE('',*,*,#7562,.F.);
#11068=ORIENTED_EDGE('',*,*,#7565,.F.);
#11069=ORIENTED_EDGE('',*,*,#7568,.F.);
#11070=ORIENTED_EDGE('',*,*,#7828,.F.);
#11071=ORIENTED_EDGE('',*,*,#7573,.F.);
#11072=ORIENTED_EDGE('',*,*,#7829,.F.);
#11073=ORIENTED_EDGE('',*,*,#7594,.T.);
#11074=ORIENTED_EDGE('',*,*,#7825,.T.);
#11075=ORIENTED_EDGE('',*,*,#7592,.T.);
#11076=ORIENTED_EDGE('',*,*,#7589,.T.);
#11077=ORIENTED_EDGE('',*,*,#7586,.T.);
#11078=ORIENTED_EDGE('',*,*,#7583,.T.);
#11079=ORIENTED_EDGE('',*,*,#7580,.T.);
#11080=ORIENTED_EDGE('',*,*,#7577,.T.);
#11081=ORIENTED_EDGE('',*,*,#7570,.T.);
#11082=ORIENTED_EDGE('',*,*,#7828,.T.);
#11083=ORIENTED_EDGE('',*,*,#7567,.F.);
#11084=ORIENTED_EDGE('',*,*,#7827,.T.);
#11085=ORIENTED_EDGE('',*,*,#7501,.F.);
#11086=ORIENTED_EDGE('',*,*,#7830,.T.);
#11087=ORIENTED_EDGE('',*,*,#7527,.T.);
#11088=ORIENTED_EDGE('',*,*,#7831,.T.);
#11089=ORIENTED_EDGE('',*,*,#7504,.F.);
#11090=ORIENTED_EDGE('',*,*,#7544,.T.);
#11091=ORIENTED_EDGE('',*,*,#7832,.T.);
#11092=ORIENTED_EDGE('',*,*,#7541,.F.);
#11093=ORIENTED_EDGE('',*,*,#7833,.F.);
#11094=ORIENTED_EDGE('',*,*,#7831,.F.);
#11095=ORIENTED_EDGE('',*,*,#7526,.F.);
#11096=ORIENTED_EDGE('',*,*,#7530,.F.);
#11097=ORIENTED_EDGE('',*,*,#7533,.F.);
#11098=ORIENTED_EDGE('',*,*,#7536,.F.);
#11099=ORIENTED_EDGE('',*,*,#7539,.F.);
#11100=ORIENTED_EDGE('',*,*,#7542,.F.);
#11101=ORIENTED_EDGE('',*,*,#7832,.F.);
#11102=ORIENTED_EDGE('',*,*,#7547,.F.);
#11103=ORIENTED_EDGE('',*,*,#7834,.F.);
#11104=ORIENTED_EDGE('',*,*,#7522,.F.);
#11105=ORIENTED_EDGE('',*,*,#7835,.F.);
#11106=ORIENTED_EDGE('',*,*,#7520,.F.);
#11107=ORIENTED_EDGE('',*,*,#7517,.F.);
#11108=ORIENTED_EDGE('',*,*,#7514,.F.);
#11109=ORIENTED_EDGE('',*,*,#7511,.F.);
#11110=ORIENTED_EDGE('',*,*,#7508,.F.);
#11111=ORIENTED_EDGE('',*,*,#7505,.F.);
#11112=ORIENTED_EDGE('',*,*,#7830,.F.);
#11113=ORIENTED_EDGE('',*,*,#7500,.F.);
#11114=ORIENTED_EDGE('',*,*,#7507,.F.);
#11115=ORIENTED_EDGE('',*,*,#7510,.F.);
#11116=ORIENTED_EDGE('',*,*,#7513,.F.);
#11117=ORIENTED_EDGE('',*,*,#7516,.F.);
#11118=ORIENTED_EDGE('',*,*,#7519,.F.);
#11119=ORIENTED_EDGE('',*,*,#7836,.F.);
#11120=ORIENTED_EDGE('',*,*,#7524,.F.);
#11121=ORIENTED_EDGE('',*,*,#7837,.F.);
#11122=ORIENTED_EDGE('',*,*,#7545,.T.);
#11123=ORIENTED_EDGE('',*,*,#7833,.T.);
#11124=ORIENTED_EDGE('',*,*,#7543,.T.);
#11125=ORIENTED_EDGE('',*,*,#7540,.T.);
#11126=ORIENTED_EDGE('',*,*,#7537,.T.);
#11127=ORIENTED_EDGE('',*,*,#7534,.T.);
#11128=ORIENTED_EDGE('',*,*,#7531,.T.);
#11129=ORIENTED_EDGE('',*,*,#7528,.T.);
#11130=ORIENTED_EDGE('',*,*,#7521,.T.);
#11131=ORIENTED_EDGE('',*,*,#7836,.T.);
#11132=ORIENTED_EDGE('',*,*,#7518,.F.);
#11133=ORIENTED_EDGE('',*,*,#7835,.T.);
#11134=ORIENTED_EDGE('',*,*,#7452,.F.);
#11135=ORIENTED_EDGE('',*,*,#7838,.T.);
#11136=ORIENTED_EDGE('',*,*,#7478,.T.);
#11137=ORIENTED_EDGE('',*,*,#7839,.T.);
#11138=ORIENTED_EDGE('',*,*,#7455,.F.);
#11139=ORIENTED_EDGE('',*,*,#7495,.T.);
#11140=ORIENTED_EDGE('',*,*,#7840,.T.);
#11141=ORIENTED_EDGE('',*,*,#7492,.F.);
#11142=ORIENTED_EDGE('',*,*,#7841,.F.);
#11143=ORIENTED_EDGE('',*,*,#7839,.F.);
#11144=ORIENTED_EDGE('',*,*,#7477,.F.);
#11145=ORIENTED_EDGE('',*,*,#7481,.F.);
#11146=ORIENTED_EDGE('',*,*,#7484,.F.);
#11147=ORIENTED_EDGE('',*,*,#7487,.F.);
#11148=ORIENTED_EDGE('',*,*,#7490,.F.);
#11149=ORIENTED_EDGE('',*,*,#7493,.F.);
#11150=ORIENTED_EDGE('',*,*,#7840,.F.);
#11151=ORIENTED_EDGE('',*,*,#7498,.F.);
#11152=ORIENTED_EDGE('',*,*,#7842,.F.);
#11153=ORIENTED_EDGE('',*,*,#7473,.F.);
#11154=ORIENTED_EDGE('',*,*,#7843,.F.);
#11155=ORIENTED_EDGE('',*,*,#7471,.F.);
#11156=ORIENTED_EDGE('',*,*,#7468,.F.);
#11157=ORIENTED_EDGE('',*,*,#7465,.F.);
#11158=ORIENTED_EDGE('',*,*,#7462,.F.);
#11159=ORIENTED_EDGE('',*,*,#7459,.F.);
#11160=ORIENTED_EDGE('',*,*,#7456,.F.);
#11161=ORIENTED_EDGE('',*,*,#7838,.F.);
#11162=ORIENTED_EDGE('',*,*,#7451,.F.);
#11163=ORIENTED_EDGE('',*,*,#7458,.F.);
#11164=ORIENTED_EDGE('',*,*,#7461,.F.);
#11165=ORIENTED_EDGE('',*,*,#7464,.F.);
#11166=ORIENTED_EDGE('',*,*,#7467,.F.);
#11167=ORIENTED_EDGE('',*,*,#7470,.F.);
#11168=ORIENTED_EDGE('',*,*,#7844,.F.);
#11169=ORIENTED_EDGE('',*,*,#7475,.F.);
#11170=ORIENTED_EDGE('',*,*,#7845,.F.);
#11171=ORIENTED_EDGE('',*,*,#7496,.T.);
#11172=ORIENTED_EDGE('',*,*,#7841,.T.);
#11173=ORIENTED_EDGE('',*,*,#7494,.T.);
#11174=ORIENTED_EDGE('',*,*,#7491,.T.);
#11175=ORIENTED_EDGE('',*,*,#7488,.T.);
#11176=ORIENTED_EDGE('',*,*,#7485,.T.);
#11177=ORIENTED_EDGE('',*,*,#7482,.T.);
#11178=ORIENTED_EDGE('',*,*,#7479,.T.);
#11179=ORIENTED_EDGE('',*,*,#7472,.T.);
#11180=ORIENTED_EDGE('',*,*,#7844,.T.);
#11181=ORIENTED_EDGE('',*,*,#7469,.F.);
#11182=ORIENTED_EDGE('',*,*,#7843,.T.);
#11183=ORIENTED_EDGE('',*,*,#7846,.F.);
#11184=ORIENTED_EDGE('',*,*,#7847,.T.);
#11185=ORIENTED_EDGE('',*,*,#7848,.F.);
#11186=ORIENTED_EDGE('',*,*,#7847,.F.);
#11187=ORIENTED_EDGE('',*,*,#7846,.T.);
#11188=ORIENTED_EDGE('',*,*,#7849,.T.);
#11189=ORIENTED_EDGE('',*,*,#7849,.F.);
#11190=ORIENTED_EDGE('',*,*,#7850,.T.);
#11191=ORIENTED_EDGE('',*,*,#7851,.T.);
#11192=ORIENTED_EDGE('',*,*,#7850,.F.);
#11193=ORIENTED_EDGE('',*,*,#7852,.F.);
#11194=ORIENTED_EDGE('',*,*,#7853,.T.);
#11195=ORIENTED_EDGE('',*,*,#7854,.T.);
#11196=ORIENTED_EDGE('',*,*,#7853,.F.);
#11197=ORIENTED_EDGE('',*,*,#7852,.T.);
#11198=ORIENTED_EDGE('',*,*,#7821,.T.);
#11199=ORIENTED_EDGE('',*,*,#7621,.T.);
#11200=ORIENTED_EDGE('',*,*,#7818,.T.);
#11201=ORIENTED_EDGE('',*,*,#7644,.T.);
#11202=ORIENTED_EDGE('',*,*,#7829,.T.);
#11203=ORIENTED_EDGE('',*,*,#7572,.T.);
#11204=ORIENTED_EDGE('',*,*,#7826,.T.);
#11205=ORIENTED_EDGE('',*,*,#7595,.T.);
#11206=ORIENTED_EDGE('',*,*,#7837,.T.);
#11207=ORIENTED_EDGE('',*,*,#7523,.T.);
#11208=ORIENTED_EDGE('',*,*,#7834,.T.);
#11209=ORIENTED_EDGE('',*,*,#7546,.T.);
#11210=ORIENTED_EDGE('',*,*,#7845,.T.);
#11211=ORIENTED_EDGE('',*,*,#7474,.T.);
#11212=ORIENTED_EDGE('',*,*,#7842,.T.);
#11213=ORIENTED_EDGE('',*,*,#7497,.T.);
#11214=ORIENTED_EDGE('',*,*,#7848,.T.);
#11215=ORIENTED_EDGE('',*,*,#7854,.F.);
#11216=ORIENTED_EDGE('',*,*,#7797,.T.);
#11217=ORIENTED_EDGE('',*,*,#7729,.T.);
#11218=ORIENTED_EDGE('',*,*,#7794,.T.);
#11219=ORIENTED_EDGE('',*,*,#7746,.T.);
#11220=ORIENTED_EDGE('',*,*,#7813,.T.);
#11221=ORIENTED_EDGE('',*,*,#7661,.T.);
#11222=ORIENTED_EDGE('',*,*,#7810,.T.);
#11223=ORIENTED_EDGE('',*,*,#7678,.T.);
#11224=ORIENTED_EDGE('',*,*,#7503,.T.);
#11225=ORIENTED_EDGE('',*,*,#7454,.T.);
#11226=ORIENTED_EDGE('',*,*,#7552,.T.);
#11227=ORIENTED_EDGE('',*,*,#7601,.T.);
#11228=ORIENTED_EDGE('',*,*,#7851,.F.);
#11229=ORIENTED_EDGE('',*,*,#7805,.T.);
#11230=ORIENTED_EDGE('',*,*,#7695,.T.);
#11231=ORIENTED_EDGE('',*,*,#7802,.T.);
#11232=ORIENTED_EDGE('',*,*,#7712,.T.);
#11233=ORIENTED_EDGE('',*,*,#7789,.T.);
#11234=ORIENTED_EDGE('',*,*,#7763,.T.);
#11235=ORIENTED_EDGE('',*,*,#7786,.T.);
#11236=ORIENTED_EDGE('',*,*,#7780,.T.);
#11237=ORIENTED_EDGE('',*,*,#7855,.T.);
#11238=ORIENTED_EDGE('',*,*,#7856,.T.);
#11239=ORIENTED_EDGE('',*,*,#7857,.F.);
#11240=ORIENTED_EDGE('',*,*,#7858,.T.);
#11241=ORIENTED_EDGE('',*,*,#7859,.T.);
#11242=ORIENTED_EDGE('',*,*,#7860,.T.);
#11243=ORIENTED_EDGE('',*,*,#7855,.F.);
#11244=ORIENTED_EDGE('',*,*,#7861,.T.);
#11245=ORIENTED_EDGE('',*,*,#7862,.T.);
#11246=ORIENTED_EDGE('',*,*,#7863,.T.);
#11247=ORIENTED_EDGE('',*,*,#7859,.F.);
#11248=ORIENTED_EDGE('',*,*,#7864,.T.);
#11249=ORIENTED_EDGE('',*,*,#7865,.T.);
#11250=ORIENTED_EDGE('',*,*,#7866,.T.);
#11251=ORIENTED_EDGE('',*,*,#7862,.F.);
#11252=ORIENTED_EDGE('',*,*,#7867,.T.);
#11253=ORIENTED_EDGE('',*,*,#7868,.T.);
#11254=ORIENTED_EDGE('',*,*,#7869,.T.);
#11255=ORIENTED_EDGE('',*,*,#7865,.F.);
#11256=ORIENTED_EDGE('',*,*,#7870,.T.);
#11257=ORIENTED_EDGE('',*,*,#7871,.T.);
#11258=ORIENTED_EDGE('',*,*,#7872,.T.);
#11259=ORIENTED_EDGE('',*,*,#7868,.F.);
#11260=ORIENTED_EDGE('',*,*,#7873,.T.);
#11261=ORIENTED_EDGE('',*,*,#7874,.T.);
#11262=ORIENTED_EDGE('',*,*,#7875,.T.);
#11263=ORIENTED_EDGE('',*,*,#7871,.F.);
#11264=ORIENTED_EDGE('',*,*,#7876,.T.);
#11265=ORIENTED_EDGE('',*,*,#7877,.T.);
#11266=ORIENTED_EDGE('',*,*,#7878,.T.);
#11267=ORIENTED_EDGE('',*,*,#7874,.F.);
#11268=ORIENTED_EDGE('',*,*,#7879,.T.);
#11269=ORIENTED_EDGE('',*,*,#7880,.T.);
#11270=ORIENTED_EDGE('',*,*,#7881,.T.);
#11271=ORIENTED_EDGE('',*,*,#7877,.F.);
#11272=ORIENTED_EDGE('',*,*,#7882,.T.);
#11273=ORIENTED_EDGE('',*,*,#7883,.T.);
#11274=ORIENTED_EDGE('',*,*,#7884,.T.);
#11275=ORIENTED_EDGE('',*,*,#7880,.F.);
#11276=ORIENTED_EDGE('',*,*,#7885,.T.);
#11277=ORIENTED_EDGE('',*,*,#7886,.T.);
#11278=ORIENTED_EDGE('',*,*,#7887,.T.);
#11279=ORIENTED_EDGE('',*,*,#7883,.F.);
#11280=ORIENTED_EDGE('',*,*,#7888,.T.);
#11281=ORIENTED_EDGE('',*,*,#7889,.T.);
#11282=ORIENTED_EDGE('',*,*,#7890,.T.);
#11283=ORIENTED_EDGE('',*,*,#7886,.F.);
#11284=ORIENTED_EDGE('',*,*,#7891,.T.);
#11285=ORIENTED_EDGE('',*,*,#7892,.T.);
#11286=ORIENTED_EDGE('',*,*,#7893,.T.);
#11287=ORIENTED_EDGE('',*,*,#7889,.F.);
#11288=ORIENTED_EDGE('',*,*,#7894,.T.);
#11289=ORIENTED_EDGE('',*,*,#7895,.T.);
#11290=ORIENTED_EDGE('',*,*,#7896,.T.);
#11291=ORIENTED_EDGE('',*,*,#7892,.F.);
#11292=ORIENTED_EDGE('',*,*,#7897,.T.);
#11293=ORIENTED_EDGE('',*,*,#7898,.T.);
#11294=ORIENTED_EDGE('',*,*,#7899,.T.);
#11295=ORIENTED_EDGE('',*,*,#7895,.F.);
#11296=ORIENTED_EDGE('',*,*,#7900,.T.);
#11297=ORIENTED_EDGE('',*,*,#7901,.T.);
#11298=ORIENTED_EDGE('',*,*,#7902,.T.);
#11299=ORIENTED_EDGE('',*,*,#7898,.F.);
#11300=ORIENTED_EDGE('',*,*,#7903,.T.);
#11301=ORIENTED_EDGE('',*,*,#7904,.T.);
#11302=ORIENTED_EDGE('',*,*,#7905,.T.);
#11303=ORIENTED_EDGE('',*,*,#7901,.F.);
#11304=ORIENTED_EDGE('',*,*,#7906,.T.);
#11305=ORIENTED_EDGE('',*,*,#7907,.T.);
#11306=ORIENTED_EDGE('',*,*,#7908,.T.);
#11307=ORIENTED_EDGE('',*,*,#7904,.F.);
#11308=ORIENTED_EDGE('',*,*,#7909,.T.);
#11309=ORIENTED_EDGE('',*,*,#7910,.T.);
#11310=ORIENTED_EDGE('',*,*,#7911,.T.);
#11311=ORIENTED_EDGE('',*,*,#7907,.F.);
#11312=ORIENTED_EDGE('',*,*,#7912,.T.);
#11313=ORIENTED_EDGE('',*,*,#7913,.T.);
#11314=ORIENTED_EDGE('',*,*,#7914,.T.);
#11315=ORIENTED_EDGE('',*,*,#7910,.F.);
#11316=ORIENTED_EDGE('',*,*,#7915,.T.);
#11317=ORIENTED_EDGE('',*,*,#7916,.T.);
#11318=ORIENTED_EDGE('',*,*,#7917,.T.);
#11319=ORIENTED_EDGE('',*,*,#7913,.F.);
#11320=ORIENTED_EDGE('',*,*,#7918,.T.);
#11321=ORIENTED_EDGE('',*,*,#7919,.T.);
#11322=ORIENTED_EDGE('',*,*,#7920,.T.);
#11323=ORIENTED_EDGE('',*,*,#7916,.F.);
#11324=ORIENTED_EDGE('',*,*,#7921,.T.);
#11325=ORIENTED_EDGE('',*,*,#7922,.T.);
#11326=ORIENTED_EDGE('',*,*,#7923,.T.);
#11327=ORIENTED_EDGE('',*,*,#7919,.F.);
#11328=ORIENTED_EDGE('',*,*,#7924,.T.);
#11329=ORIENTED_EDGE('',*,*,#7925,.T.);
#11330=ORIENTED_EDGE('',*,*,#7926,.T.);
#11331=ORIENTED_EDGE('',*,*,#7922,.F.);
#11332=ORIENTED_EDGE('',*,*,#7927,.T.);
#11333=ORIENTED_EDGE('',*,*,#7928,.T.);
#11334=ORIENTED_EDGE('',*,*,#7929,.T.);
#11335=ORIENTED_EDGE('',*,*,#7925,.F.);
#11336=ORIENTED_EDGE('',*,*,#7930,.T.);
#11337=ORIENTED_EDGE('',*,*,#7931,.T.);
#11338=ORIENTED_EDGE('',*,*,#7932,.T.);
#11339=ORIENTED_EDGE('',*,*,#7928,.F.);
#11340=ORIENTED_EDGE('',*,*,#7933,.T.);
#11341=ORIENTED_EDGE('',*,*,#7934,.T.);
#11342=ORIENTED_EDGE('',*,*,#7935,.T.);
#11343=ORIENTED_EDGE('',*,*,#7931,.F.);
#11344=ORIENTED_EDGE('',*,*,#7936,.T.);
#11345=ORIENTED_EDGE('',*,*,#7937,.F.);
#11346=ORIENTED_EDGE('',*,*,#7938,.T.);
#11347=ORIENTED_EDGE('',*,*,#7939,.F.);
#11348=ORIENTED_EDGE('',*,*,#7940,.T.);
#11349=ORIENTED_EDGE('',*,*,#7941,.T.);
#11350=ORIENTED_EDGE('',*,*,#7942,.T.);
#11351=ORIENTED_EDGE('',*,*,#7943,.F.);
#11352=ORIENTED_EDGE('',*,*,#7944,.F.);
#11353=ORIENTED_EDGE('',*,*,#7945,.T.);
#11354=ORIENTED_EDGE('',*,*,#7946,.T.);
#11355=ORIENTED_EDGE('',*,*,#7941,.F.);
#11356=ORIENTED_EDGE('',*,*,#7947,.F.);
#11357=ORIENTED_EDGE('',*,*,#7948,.T.);
#11358=ORIENTED_EDGE('',*,*,#7949,.T.);
#11359=ORIENTED_EDGE('',*,*,#7945,.F.);
#11360=ORIENTED_EDGE('',*,*,#7950,.F.);
#11361=ORIENTED_EDGE('',*,*,#7951,.T.);
#11362=ORIENTED_EDGE('',*,*,#7952,.T.);
#11363=ORIENTED_EDGE('',*,*,#7948,.F.);
#11364=ORIENTED_EDGE('',*,*,#7953,.F.);
#11365=ORIENTED_EDGE('',*,*,#7954,.T.);
#11366=ORIENTED_EDGE('',*,*,#7955,.T.);
#11367=ORIENTED_EDGE('',*,*,#7951,.F.);
#11368=ORIENTED_EDGE('',*,*,#7956,.F.);
#11369=ORIENTED_EDGE('',*,*,#7957,.T.);
#11370=ORIENTED_EDGE('',*,*,#7958,.T.);
#11371=ORIENTED_EDGE('',*,*,#7954,.F.);
#11372=ORIENTED_EDGE('',*,*,#7959,.F.);
#11373=ORIENTED_EDGE('',*,*,#7960,.T.);
#11374=ORIENTED_EDGE('',*,*,#7961,.T.);
#11375=ORIENTED_EDGE('',*,*,#7957,.F.);
#11376=ORIENTED_EDGE('',*,*,#7962,.F.);
#11377=ORIENTED_EDGE('',*,*,#7963,.T.);
#11378=ORIENTED_EDGE('',*,*,#7964,.T.);
#11379=ORIENTED_EDGE('',*,*,#7960,.F.);
#11380=ORIENTED_EDGE('',*,*,#7965,.F.);
#11381=ORIENTED_EDGE('',*,*,#7966,.T.);
#11382=ORIENTED_EDGE('',*,*,#7967,.T.);
#11383=ORIENTED_EDGE('',*,*,#7963,.F.);
#11384=ORIENTED_EDGE('',*,*,#7968,.F.);
#11385=ORIENTED_EDGE('',*,*,#7969,.T.);
#11386=ORIENTED_EDGE('',*,*,#7970,.T.);
#11387=ORIENTED_EDGE('',*,*,#7966,.F.);
#11388=ORIENTED_EDGE('',*,*,#7971,.F.);
#11389=ORIENTED_EDGE('',*,*,#7972,.T.);
#11390=ORIENTED_EDGE('',*,*,#7973,.T.);
#11391=ORIENTED_EDGE('',*,*,#7969,.F.);
#11392=ORIENTED_EDGE('',*,*,#7974,.F.);
#11393=ORIENTED_EDGE('',*,*,#7975,.T.);
#11394=ORIENTED_EDGE('',*,*,#7976,.T.);
#11395=ORIENTED_EDGE('',*,*,#7972,.F.);
#11396=ORIENTED_EDGE('',*,*,#7977,.F.);
#11397=ORIENTED_EDGE('',*,*,#7978,.T.);
#11398=ORIENTED_EDGE('',*,*,#7979,.T.);
#11399=ORIENTED_EDGE('',*,*,#7975,.F.);
#11400=ORIENTED_EDGE('',*,*,#7980,.F.);
#11401=ORIENTED_EDGE('',*,*,#7981,.T.);
#11402=ORIENTED_EDGE('',*,*,#7982,.T.);
#11403=ORIENTED_EDGE('',*,*,#7978,.F.);
#11404=ORIENTED_EDGE('',*,*,#7983,.F.);
#11405=ORIENTED_EDGE('',*,*,#7984,.T.);
#11406=ORIENTED_EDGE('',*,*,#7985,.T.);
#11407=ORIENTED_EDGE('',*,*,#7981,.F.);
#11408=ORIENTED_EDGE('',*,*,#7986,.F.);
#11409=ORIENTED_EDGE('',*,*,#7987,.T.);
#11410=ORIENTED_EDGE('',*,*,#7988,.T.);
#11411=ORIENTED_EDGE('',*,*,#7984,.F.);
#11412=ORIENTED_EDGE('',*,*,#7989,.F.);
#11413=ORIENTED_EDGE('',*,*,#7990,.T.);
#11414=ORIENTED_EDGE('',*,*,#7991,.T.);
#11415=ORIENTED_EDGE('',*,*,#7987,.F.);
#11416=ORIENTED_EDGE('',*,*,#7992,.F.);
#11417=ORIENTED_EDGE('',*,*,#7993,.T.);
#11418=ORIENTED_EDGE('',*,*,#7994,.T.);
#11419=ORIENTED_EDGE('',*,*,#7990,.F.);
#11420=ORIENTED_EDGE('',*,*,#7995,.F.);
#11421=ORIENTED_EDGE('',*,*,#7996,.T.);
#11422=ORIENTED_EDGE('',*,*,#7997,.T.);
#11423=ORIENTED_EDGE('',*,*,#7993,.F.);
#11424=ORIENTED_EDGE('',*,*,#7998,.F.);
#11425=ORIENTED_EDGE('',*,*,#7999,.T.);
#11426=ORIENTED_EDGE('',*,*,#8000,.T.);
#11427=ORIENTED_EDGE('',*,*,#7996,.F.);
#11428=ORIENTED_EDGE('',*,*,#8001,.F.);
#11429=ORIENTED_EDGE('',*,*,#8002,.T.);
#11430=ORIENTED_EDGE('',*,*,#8003,.T.);
#11431=ORIENTED_EDGE('',*,*,#7999,.F.);
#11432=ORIENTED_EDGE('',*,*,#8004,.F.);
#11433=ORIENTED_EDGE('',*,*,#8005,.T.);
#11434=ORIENTED_EDGE('',*,*,#8006,.T.);
#11435=ORIENTED_EDGE('',*,*,#8002,.F.);
#11436=ORIENTED_EDGE('',*,*,#8007,.F.);
#11437=ORIENTED_EDGE('',*,*,#8008,.T.);
#11438=ORIENTED_EDGE('',*,*,#8009,.T.);
#11439=ORIENTED_EDGE('',*,*,#8005,.F.);
#11440=ORIENTED_EDGE('',*,*,#8010,.F.);
#11441=ORIENTED_EDGE('',*,*,#8011,.T.);
#11442=ORIENTED_EDGE('',*,*,#8012,.T.);
#11443=ORIENTED_EDGE('',*,*,#8008,.F.);
#11444=ORIENTED_EDGE('',*,*,#8013,.F.);
#11445=ORIENTED_EDGE('',*,*,#8014,.T.);
#11446=ORIENTED_EDGE('',*,*,#8015,.T.);
#11447=ORIENTED_EDGE('',*,*,#8011,.F.);
#11448=ORIENTED_EDGE('',*,*,#8016,.F.);
#11449=ORIENTED_EDGE('',*,*,#8017,.T.);
#11450=ORIENTED_EDGE('',*,*,#8018,.T.);
#11451=ORIENTED_EDGE('',*,*,#8014,.F.);
#11452=ORIENTED_EDGE('',*,*,#8019,.F.);
#11453=ORIENTED_EDGE('',*,*,#8020,.T.);
#11454=ORIENTED_EDGE('',*,*,#8021,.T.);
#11455=ORIENTED_EDGE('',*,*,#8017,.F.);
#11456=ORIENTED_EDGE('',*,*,#8022,.F.);
#11457=ORIENTED_EDGE('',*,*,#8023,.T.);
#11458=ORIENTED_EDGE('',*,*,#8024,.T.);
#11459=ORIENTED_EDGE('',*,*,#8020,.F.);
#11460=ORIENTED_EDGE('',*,*,#8025,.F.);
#11461=ORIENTED_EDGE('',*,*,#8026,.F.);
#11462=ORIENTED_EDGE('',*,*,#8027,.F.);
#11463=ORIENTED_EDGE('',*,*,#8028,.F.);
#11464=ORIENTED_EDGE('',*,*,#8029,.T.);
#11465=ORIENTED_EDGE('',*,*,#8026,.T.);
#11466=ORIENTED_EDGE('',*,*,#8030,.T.);
#11467=ORIENTED_EDGE('',*,*,#8023,.F.);
#11468=ORIENTED_EDGE('',*,*,#8031,.F.);
#11469=ORIENTED_EDGE('',*,*,#8032,.F.);
#11470=ORIENTED_EDGE('',*,*,#7942,.F.);
#11471=ORIENTED_EDGE('',*,*,#7946,.F.);
#11472=ORIENTED_EDGE('',*,*,#7949,.F.);
#11473=ORIENTED_EDGE('',*,*,#7952,.F.);
#11474=ORIENTED_EDGE('',*,*,#7955,.F.);
#11475=ORIENTED_EDGE('',*,*,#7958,.F.);
#11476=ORIENTED_EDGE('',*,*,#7961,.F.);
#11477=ORIENTED_EDGE('',*,*,#7964,.F.);
#11478=ORIENTED_EDGE('',*,*,#7967,.F.);
#11479=ORIENTED_EDGE('',*,*,#7970,.F.);
#11480=ORIENTED_EDGE('',*,*,#7973,.F.);
#11481=ORIENTED_EDGE('',*,*,#7976,.F.);
#11482=ORIENTED_EDGE('',*,*,#7979,.F.);
#11483=ORIENTED_EDGE('',*,*,#7982,.F.);
#11484=ORIENTED_EDGE('',*,*,#7985,.F.);
#11485=ORIENTED_EDGE('',*,*,#7988,.F.);
#11486=ORIENTED_EDGE('',*,*,#7991,.F.);
#11487=ORIENTED_EDGE('',*,*,#7994,.F.);
#11488=ORIENTED_EDGE('',*,*,#7997,.F.);
#11489=ORIENTED_EDGE('',*,*,#8000,.F.);
#11490=ORIENTED_EDGE('',*,*,#8003,.F.);
#11491=ORIENTED_EDGE('',*,*,#8006,.F.);
#11492=ORIENTED_EDGE('',*,*,#8009,.F.);
#11493=ORIENTED_EDGE('',*,*,#8012,.F.);
#11494=ORIENTED_EDGE('',*,*,#8015,.F.);
#11495=ORIENTED_EDGE('',*,*,#8018,.F.);
#11496=ORIENTED_EDGE('',*,*,#8021,.F.);
#11497=ORIENTED_EDGE('',*,*,#8024,.F.);
#11498=ORIENTED_EDGE('',*,*,#8030,.F.);
#11499=ORIENTED_EDGE('',*,*,#8029,.F.);
#11500=ORIENTED_EDGE('',*,*,#8033,.F.);
#11501=ORIENTED_EDGE('',*,*,#7938,.F.);
#11502=ORIENTED_EDGE('',*,*,#8034,.F.);
#11503=ORIENTED_EDGE('',*,*,#7936,.F.);
#11504=ORIENTED_EDGE('',*,*,#7933,.F.);
#11505=ORIENTED_EDGE('',*,*,#7930,.F.);
#11506=ORIENTED_EDGE('',*,*,#7927,.F.);
#11507=ORIENTED_EDGE('',*,*,#7924,.F.);
#11508=ORIENTED_EDGE('',*,*,#7921,.F.);
#11509=ORIENTED_EDGE('',*,*,#7918,.F.);
#11510=ORIENTED_EDGE('',*,*,#7915,.F.);
#11511=ORIENTED_EDGE('',*,*,#7912,.F.);
#11512=ORIENTED_EDGE('',*,*,#7909,.F.);
#11513=ORIENTED_EDGE('',*,*,#7906,.F.);
#11514=ORIENTED_EDGE('',*,*,#7903,.F.);
#11515=ORIENTED_EDGE('',*,*,#7900,.F.);
#11516=ORIENTED_EDGE('',*,*,#7897,.F.);
#11517=ORIENTED_EDGE('',*,*,#7894,.F.);
#11518=ORIENTED_EDGE('',*,*,#7891,.F.);
#11519=ORIENTED_EDGE('',*,*,#7888,.F.);
#11520=ORIENTED_EDGE('',*,*,#7885,.F.);
#11521=ORIENTED_EDGE('',*,*,#7882,.F.);
#11522=ORIENTED_EDGE('',*,*,#7879,.F.);
#11523=ORIENTED_EDGE('',*,*,#7876,.F.);
#11524=ORIENTED_EDGE('',*,*,#7873,.F.);
#11525=ORIENTED_EDGE('',*,*,#7870,.F.);
#11526=ORIENTED_EDGE('',*,*,#7867,.F.);
#11527=ORIENTED_EDGE('',*,*,#7864,.F.);
#11528=ORIENTED_EDGE('',*,*,#7861,.F.);
#11529=ORIENTED_EDGE('',*,*,#7858,.F.);
#11530=ORIENTED_EDGE('',*,*,#8035,.F.);
#11531=ORIENTED_EDGE('',*,*,#7856,.F.);
#11532=ORIENTED_EDGE('',*,*,#7860,.F.);
#11533=ORIENTED_EDGE('',*,*,#7863,.F.);
#11534=ORIENTED_EDGE('',*,*,#7866,.F.);
#11535=ORIENTED_EDGE('',*,*,#7869,.F.);
#11536=ORIENTED_EDGE('',*,*,#7872,.F.);
#11537=ORIENTED_EDGE('',*,*,#7875,.F.);
#11538=ORIENTED_EDGE('',*,*,#7878,.F.);
#11539=ORIENTED_EDGE('',*,*,#7881,.F.);
#11540=ORIENTED_EDGE('',*,*,#7884,.F.);
#11541=ORIENTED_EDGE('',*,*,#7887,.F.);
#11542=ORIENTED_EDGE('',*,*,#7890,.F.);
#11543=ORIENTED_EDGE('',*,*,#7893,.F.);
#11544=ORIENTED_EDGE('',*,*,#7896,.F.);
#11545=ORIENTED_EDGE('',*,*,#7899,.F.);
#11546=ORIENTED_EDGE('',*,*,#7902,.F.);
#11547=ORIENTED_EDGE('',*,*,#7905,.F.);
#11548=ORIENTED_EDGE('',*,*,#7908,.F.);
#11549=ORIENTED_EDGE('',*,*,#7911,.F.);
#11550=ORIENTED_EDGE('',*,*,#7914,.F.);
#11551=ORIENTED_EDGE('',*,*,#7917,.F.);
#11552=ORIENTED_EDGE('',*,*,#7920,.F.);
#11553=ORIENTED_EDGE('',*,*,#7923,.F.);
#11554=ORIENTED_EDGE('',*,*,#7926,.F.);
#11555=ORIENTED_EDGE('',*,*,#7929,.F.);
#11556=ORIENTED_EDGE('',*,*,#7932,.F.);
#11557=ORIENTED_EDGE('',*,*,#7935,.F.);
#11558=ORIENTED_EDGE('',*,*,#8036,.F.);
#11559=ORIENTED_EDGE('',*,*,#7940,.F.);
#11560=ORIENTED_EDGE('',*,*,#8037,.F.);
#11561=ORIENTED_EDGE('',*,*,#8027,.T.);
#11562=ORIENTED_EDGE('',*,*,#8031,.T.);
#11563=ORIENTED_EDGE('',*,*,#8025,.T.);
#11564=ORIENTED_EDGE('',*,*,#8022,.T.);
#11565=ORIENTED_EDGE('',*,*,#8019,.T.);
#11566=ORIENTED_EDGE('',*,*,#8016,.T.);
#11567=ORIENTED_EDGE('',*,*,#8013,.T.);
#11568=ORIENTED_EDGE('',*,*,#8010,.T.);
#11569=ORIENTED_EDGE('',*,*,#8007,.T.);
#11570=ORIENTED_EDGE('',*,*,#8004,.T.);
#11571=ORIENTED_EDGE('',*,*,#8001,.T.);
#11572=ORIENTED_EDGE('',*,*,#7998,.T.);
#11573=ORIENTED_EDGE('',*,*,#7995,.T.);
#11574=ORIENTED_EDGE('',*,*,#7992,.T.);
#11575=ORIENTED_EDGE('',*,*,#7989,.T.);
#11576=ORIENTED_EDGE('',*,*,#7986,.T.);
#11577=ORIENTED_EDGE('',*,*,#7983,.T.);
#11578=ORIENTED_EDGE('',*,*,#7980,.T.);
#11579=ORIENTED_EDGE('',*,*,#7977,.T.);
#11580=ORIENTED_EDGE('',*,*,#7974,.T.);
#11581=ORIENTED_EDGE('',*,*,#7971,.T.);
#11582=ORIENTED_EDGE('',*,*,#7968,.T.);
#11583=ORIENTED_EDGE('',*,*,#7965,.T.);
#11584=ORIENTED_EDGE('',*,*,#7962,.T.);
#11585=ORIENTED_EDGE('',*,*,#7959,.T.);
#11586=ORIENTED_EDGE('',*,*,#7956,.T.);
#11587=ORIENTED_EDGE('',*,*,#7953,.T.);
#11588=ORIENTED_EDGE('',*,*,#7950,.T.);
#11589=ORIENTED_EDGE('',*,*,#7947,.T.);
#11590=ORIENTED_EDGE('',*,*,#7944,.T.);
#11591=ORIENTED_EDGE('',*,*,#8038,.T.);
#11592=ORIENTED_EDGE('',*,*,#8039,.T.);
#11593=ORIENTED_EDGE('',*,*,#8040,.F.);
#11594=ORIENTED_EDGE('',*,*,#8041,.T.);
#11595=ORIENTED_EDGE('',*,*,#8042,.F.);
#11596=ORIENTED_EDGE('',*,*,#8043,.F.);
#11597=ORIENTED_EDGE('',*,*,#8044,.F.);
#11598=ORIENTED_EDGE('',*,*,#8045,.F.);
#11599=ORIENTED_EDGE('',*,*,#8033,.T.);
#11600=ORIENTED_EDGE('',*,*,#8028,.T.);
#11601=ORIENTED_EDGE('',*,*,#8037,.T.);
#11602=ORIENTED_EDGE('',*,*,#7939,.T.);
#11603=ORIENTED_EDGE('',*,*,#7937,.T.);
#11604=ORIENTED_EDGE('',*,*,#8036,.T.);
#11605=ORIENTED_EDGE('',*,*,#7934,.F.);
#11606=ORIENTED_EDGE('',*,*,#8034,.T.);
#11607=ORIENTED_EDGE('',*,*,#8046,.F.);
#11608=ORIENTED_EDGE('',*,*,#8047,.T.);
#11609=ORIENTED_EDGE('',*,*,#8048,.F.);
#11610=ORIENTED_EDGE('',*,*,#8049,.F.);
#11611=ORIENTED_EDGE('',*,*,#8050,.T.);
#11612=ORIENTED_EDGE('',*,*,#8051,.T.);
#11613=ORIENTED_EDGE('',*,*,#8048,.T.);
#11614=ORIENTED_EDGE('',*,*,#8052,.T.);
#11615=ORIENTED_EDGE('',*,*,#8046,.T.);
#11616=ORIENTED_EDGE('',*,*,#8053,.T.);
#11617=ORIENTED_EDGE('',*,*,#8042,.T.);
#11618=ORIENTED_EDGE('',*,*,#8054,.T.);
#11619=ORIENTED_EDGE('',*,*,#8055,.F.);
#11620=ORIENTED_EDGE('',*,*,#8056,.T.);
#11621=ORIENTED_EDGE('',*,*,#8052,.F.);
#11622=ORIENTED_EDGE('',*,*,#8047,.F.);
#11623=ORIENTED_EDGE('',*,*,#8054,.F.);
#11624=ORIENTED_EDGE('',*,*,#8041,.F.);
#11625=ORIENTED_EDGE('',*,*,#8057,.F.);
#11626=ORIENTED_EDGE('',*,*,#8043,.T.);
#11627=ORIENTED_EDGE('',*,*,#8053,.F.);
#11628=ORIENTED_EDGE('',*,*,#8049,.T.);
#11629=ORIENTED_EDGE('',*,*,#8051,.F.);
#11630=ORIENTED_EDGE('',*,*,#8058,.F.);
#11631=ORIENTED_EDGE('',*,*,#8055,.T.);
#11632=ORIENTED_EDGE('',*,*,#8040,.T.);
#11633=ORIENTED_EDGE('',*,*,#8059,.T.);
#11634=ORIENTED_EDGE('',*,*,#8060,.T.);
#11635=ORIENTED_EDGE('',*,*,#8057,.T.);
#11636=ORIENTED_EDGE('',*,*,#8061,.T.);
#11637=ORIENTED_EDGE('',*,*,#8062,.T.);
#11638=ORIENTED_EDGE('',*,*,#8044,.T.);
#11639=ORIENTED_EDGE('',*,*,#8063,.T.);
#11640=ORIENTED_EDGE('',*,*,#8064,.T.);
#11641=ORIENTED_EDGE('',*,*,#8059,.F.);
#11642=ORIENTED_EDGE('',*,*,#8039,.F.);
#11643=ORIENTED_EDGE('',*,*,#8065,.T.);
#11644=ORIENTED_EDGE('',*,*,#8045,.T.);
#11645=ORIENTED_EDGE('',*,*,#8062,.F.);
#11646=ORIENTED_EDGE('',*,*,#8066,.F.);
#11647=ORIENTED_EDGE('',*,*,#8067,.T.);
#11648=ORIENTED_EDGE('',*,*,#8066,.T.);
#11649=ORIENTED_EDGE('',*,*,#8061,.F.);
#11650=ORIENTED_EDGE('',*,*,#8058,.T.);
#11651=ORIENTED_EDGE('',*,*,#8050,.F.);
#11652=ORIENTED_EDGE('',*,*,#8056,.F.);
#11653=ORIENTED_EDGE('',*,*,#8060,.F.);
#11654=ORIENTED_EDGE('',*,*,#8064,.F.);
#11655=ORIENTED_EDGE('',*,*,#8032,.T.);
#11656=ORIENTED_EDGE('',*,*,#7857,.T.);
#11657=ORIENTED_EDGE('',*,*,#8035,.T.);
#11658=ORIENTED_EDGE('',*,*,#7943,.T.);
#11659=ORIENTED_EDGE('',*,*,#8067,.F.);
#11660=ORIENTED_EDGE('',*,*,#8063,.F.);
#11661=ORIENTED_EDGE('',*,*,#8038,.F.);
#11662=ORIENTED_EDGE('',*,*,#8065,.F.);
#11663=ORIENTED_EDGE('',*,*,#8068,.F.);
#11664=ORIENTED_EDGE('',*,*,#8069,.T.);
#11665=ORIENTED_EDGE('',*,*,#8070,.F.);
#11666=ORIENTED_EDGE('',*,*,#8069,.F.);
#11667=ORIENTED_EDGE('',*,*,#8071,.F.);
#11668=ORIENTED_EDGE('',*,*,#8072,.T.);
#11669=ORIENTED_EDGE('',*,*,#8073,.F.);
#11670=ORIENTED_EDGE('',*,*,#8072,.F.);
#11671=ORIENTED_EDGE('',*,*,#8074,.F.);
#11672=ORIENTED_EDGE('',*,*,#8075,.F.);
#11673=ORIENTED_EDGE('',*,*,#8076,.F.);
#11674=ORIENTED_EDGE('',*,*,#8077,.T.);
#11675=ORIENTED_EDGE('',*,*,#8078,.F.);
#11676=ORIENTED_EDGE('',*,*,#8079,.T.);
#11677=ORIENTED_EDGE('',*,*,#8080,.F.);
#11678=ORIENTED_EDGE('',*,*,#8081,.F.);
#11679=ORIENTED_EDGE('',*,*,#8082,.T.);
#11680=ORIENTED_EDGE('',*,*,#8083,.F.);
#11681=ORIENTED_EDGE('',*,*,#8084,.T.);
#11682=ORIENTED_EDGE('',*,*,#8085,.F.);
#11683=ORIENTED_EDGE('',*,*,#8086,.F.);
#11684=ORIENTED_EDGE('',*,*,#8087,.T.);
#11685=ORIENTED_EDGE('',*,*,#8088,.T.);
#11686=ORIENTED_EDGE('',*,*,#8089,.T.);
#11687=ORIENTED_EDGE('',*,*,#8090,.T.);
#11688=ORIENTED_EDGE('',*,*,#8079,.F.);
#11689=ORIENTED_EDGE('',*,*,#8091,.F.);
#11690=ORIENTED_EDGE('',*,*,#8077,.F.);
#11691=ORIENTED_EDGE('',*,*,#8092,.T.);
#11692=ORIENTED_EDGE('',*,*,#8075,.T.);
#11693=ORIENTED_EDGE('',*,*,#8093,.T.);
#11694=ORIENTED_EDGE('',*,*,#8094,.T.);
#11695=ORIENTED_EDGE('',*,*,#8095,.F.);
#11696=ORIENTED_EDGE('',*,*,#8096,.T.);
#11697=ORIENTED_EDGE('',*,*,#8097,.T.);
#11698=ORIENTED_EDGE('',*,*,#8098,.T.);
#11699=ORIENTED_EDGE('',*,*,#8099,.T.);
#11700=ORIENTED_EDGE('',*,*,#8081,.T.);
#11701=ORIENTED_EDGE('',*,*,#8100,.T.);
#11702=ORIENTED_EDGE('',*,*,#8101,.T.);
#11703=ORIENTED_EDGE('',*,*,#8102,.T.);
#11704=ORIENTED_EDGE('',*,*,#8103,.T.);
#11705=ORIENTED_EDGE('',*,*,#8104,.F.);
#11706=ORIENTED_EDGE('',*,*,#8105,.F.);
#11707=ORIENTED_EDGE('',*,*,#8106,.T.);
#11708=ORIENTED_EDGE('',*,*,#8076,.T.);
#11709=ORIENTED_EDGE('',*,*,#8099,.F.);
#11710=ORIENTED_EDGE('',*,*,#8107,.F.);
#11711=ORIENTED_EDGE('',*,*,#8082,.F.);
#11712=ORIENTED_EDGE('',*,*,#8108,.F.);
#11713=ORIENTED_EDGE('',*,*,#8109,.F.);
#11714=ORIENTED_EDGE('',*,*,#8110,.F.);
#11715=ORIENTED_EDGE('',*,*,#8111,.F.);
#11716=ORIENTED_EDGE('',*,*,#8112,.F.);
#11717=ORIENTED_EDGE('',*,*,#8113,.F.);
#11718=ORIENTED_EDGE('',*,*,#8109,.T.);
#11719=ORIENTED_EDGE('',*,*,#8078,.T.);
#11720=ORIENTED_EDGE('',*,*,#8106,.F.);
#11721=ORIENTED_EDGE('',*,*,#8114,.F.);
#11722=ORIENTED_EDGE('',*,*,#8115,.F.);
#11723=ORIENTED_EDGE('',*,*,#8111,.T.);
#11724=ORIENTED_EDGE('',*,*,#8108,.T.);
#11725=ORIENTED_EDGE('',*,*,#8113,.T.);
#11726=ORIENTED_EDGE('',*,*,#8116,.F.);
#11727=ORIENTED_EDGE('',*,*,#8117,.F.);
#11728=ORIENTED_EDGE('',*,*,#8093,.F.);
#11729=ORIENTED_EDGE('',*,*,#8074,.T.);
#11730=ORIENTED_EDGE('',*,*,#8091,.T.);
#11731=ORIENTED_EDGE('',*,*,#8070,.T.);
#11732=ORIENTED_EDGE('',*,*,#8073,.T.);
#11733=ORIENTED_EDGE('',*,*,#8110,.T.);
#11734=ORIENTED_EDGE('',*,*,#8118,.T.);
#11735=ORIENTED_EDGE('',*,*,#8092,.F.);
#11736=ORIENTED_EDGE('',*,*,#8118,.F.);
#11737=ORIENTED_EDGE('',*,*,#8119,.F.);
#11738=ORIENTED_EDGE('',*,*,#8084,.F.);
#11739=ORIENTED_EDGE('',*,*,#8120,.F.);
#11740=ORIENTED_EDGE('',*,*,#8097,.F.);
#11741=ORIENTED_EDGE('',*,*,#8120,.T.);
#11742=ORIENTED_EDGE('',*,*,#8083,.T.);
#11743=ORIENTED_EDGE('',*,*,#8107,.T.);
#11744=ORIENTED_EDGE('',*,*,#8098,.F.);
#11745=ORIENTED_EDGE('',*,*,#8121,.T.);
#11746=ORIENTED_EDGE('',*,*,#8101,.F.);
#11747=ORIENTED_EDGE('',*,*,#8122,.T.);
#11748=ORIENTED_EDGE('',*,*,#8089,.F.);
#11749=ORIENTED_EDGE('',*,*,#8123,.F.);
#11750=ORIENTED_EDGE('',*,*,#8102,.F.);
#11751=ORIENTED_EDGE('',*,*,#8121,.F.);
#11752=ORIENTED_EDGE('',*,*,#8088,.F.);
#11753=ORIENTED_EDGE('',*,*,#8080,.T.);
#11754=ORIENTED_EDGE('',*,*,#8090,.F.);
#11755=ORIENTED_EDGE('',*,*,#8122,.F.);
#11756=ORIENTED_EDGE('',*,*,#8100,.F.);
#11757=ORIENTED_EDGE('',*,*,#8124,.F.);
#11758=ORIENTED_EDGE('',*,*,#8085,.T.);
#11759=ORIENTED_EDGE('',*,*,#8119,.T.);
#11760=ORIENTED_EDGE('',*,*,#8096,.F.);
#11761=ORIENTED_EDGE('',*,*,#8125,.F.);
#11762=ORIENTED_EDGE('',*,*,#8103,.F.);
#11763=ORIENTED_EDGE('',*,*,#8123,.T.);
#11764=ORIENTED_EDGE('',*,*,#8087,.F.);
#11765=ORIENTED_EDGE('',*,*,#8114,.T.);
#11766=ORIENTED_EDGE('',*,*,#8105,.T.);
#11767=ORIENTED_EDGE('',*,*,#8126,.F.);
#11768=ORIENTED_EDGE('',*,*,#8127,.F.);
#11769=ORIENTED_EDGE('',*,*,#8112,.T.);
#11770=ORIENTED_EDGE('',*,*,#8115,.T.);
#11771=ORIENTED_EDGE('',*,*,#8127,.T.);
#11772=ORIENTED_EDGE('',*,*,#8128,.F.);
#11773=ORIENTED_EDGE('',*,*,#8129,.F.);
#11774=ORIENTED_EDGE('',*,*,#8116,.T.);
#11775=ORIENTED_EDGE('',*,*,#8117,.T.);
#11776=ORIENTED_EDGE('',*,*,#8129,.T.);
#11777=ORIENTED_EDGE('',*,*,#8130,.F.);
#11778=ORIENTED_EDGE('',*,*,#8094,.F.);
#11779=ORIENTED_EDGE('',*,*,#8124,.T.);
#11780=ORIENTED_EDGE('',*,*,#8095,.T.);
#11781=ORIENTED_EDGE('',*,*,#8130,.T.);
#11782=ORIENTED_EDGE('',*,*,#8128,.T.);
#11783=ORIENTED_EDGE('',*,*,#8126,.T.);
#11784=ORIENTED_EDGE('',*,*,#8104,.T.);
#11785=ORIENTED_EDGE('',*,*,#8125,.T.);
#11786=ORIENTED_EDGE('',*,*,#8086,.T.);
#11787=ORIENTED_EDGE('',*,*,#8068,.T.);
#11788=ORIENTED_EDGE('',*,*,#8071,.T.);
#11789=ORIENTED_EDGE('',*,*,#8131,.F.);
#11790=ORIENTED_EDGE('',*,*,#8132,.T.);
#11791=ORIENTED_EDGE('',*,*,#8133,.T.);
#11792=ORIENTED_EDGE('',*,*,#8134,.T.);
#11793=ORIENTED_EDGE('',*,*,#8135,.F.);
#11794=ORIENTED_EDGE('',*,*,#8136,.T.);
#11795=ORIENTED_EDGE('',*,*,#8131,.T.);
#11796=ORIENTED_EDGE('',*,*,#8137,.T.);
#11797=ORIENTED_EDGE('',*,*,#8138,.F.);
#11798=ORIENTED_EDGE('',*,*,#8139,.T.);
#11799=ORIENTED_EDGE('',*,*,#8135,.T.);
#11800=ORIENTED_EDGE('',*,*,#8140,.T.);
#11801=ORIENTED_EDGE('',*,*,#8141,.F.);
#11802=ORIENTED_EDGE('',*,*,#8142,.T.);
#11803=ORIENTED_EDGE('',*,*,#8138,.T.);
#11804=ORIENTED_EDGE('',*,*,#8143,.T.);
#11805=ORIENTED_EDGE('',*,*,#8144,.F.);
#11806=ORIENTED_EDGE('',*,*,#8145,.T.);
#11807=ORIENTED_EDGE('',*,*,#8141,.T.);
#11808=ORIENTED_EDGE('',*,*,#8146,.T.);
#11809=ORIENTED_EDGE('',*,*,#8147,.F.);
#11810=ORIENTED_EDGE('',*,*,#8148,.T.);
#11811=ORIENTED_EDGE('',*,*,#8144,.T.);
#11812=ORIENTED_EDGE('',*,*,#8149,.T.);
#11813=ORIENTED_EDGE('',*,*,#8150,.F.);
#11814=ORIENTED_EDGE('',*,*,#8151,.T.);
#11815=ORIENTED_EDGE('',*,*,#8147,.T.);
#11816=ORIENTED_EDGE('',*,*,#8152,.T.);
#11817=ORIENTED_EDGE('',*,*,#8153,.F.);
#11818=ORIENTED_EDGE('',*,*,#8154,.T.);
#11819=ORIENTED_EDGE('',*,*,#8150,.T.);
#11820=ORIENTED_EDGE('',*,*,#8155,.T.);
#11821=ORIENTED_EDGE('',*,*,#8156,.F.);
#11822=ORIENTED_EDGE('',*,*,#8157,.T.);
#11823=ORIENTED_EDGE('',*,*,#8153,.T.);
#11824=ORIENTED_EDGE('',*,*,#8158,.T.);
#11825=ORIENTED_EDGE('',*,*,#8159,.F.);
#11826=ORIENTED_EDGE('',*,*,#8160,.T.);
#11827=ORIENTED_EDGE('',*,*,#8156,.T.);
#11828=ORIENTED_EDGE('',*,*,#8161,.T.);
#11829=ORIENTED_EDGE('',*,*,#8162,.F.);
#11830=ORIENTED_EDGE('',*,*,#8163,.T.);
#11831=ORIENTED_EDGE('',*,*,#8159,.T.);
#11832=ORIENTED_EDGE('',*,*,#8164,.T.);
#11833=ORIENTED_EDGE('',*,*,#8165,.F.);
#11834=ORIENTED_EDGE('',*,*,#8166,.T.);
#11835=ORIENTED_EDGE('',*,*,#8162,.T.);
#11836=ORIENTED_EDGE('',*,*,#8167,.T.);
#11837=ORIENTED_EDGE('',*,*,#8168,.F.);
#11838=ORIENTED_EDGE('',*,*,#8169,.T.);
#11839=ORIENTED_EDGE('',*,*,#8165,.T.);
#11840=ORIENTED_EDGE('',*,*,#8170,.T.);
#11841=ORIENTED_EDGE('',*,*,#8171,.F.);
#11842=ORIENTED_EDGE('',*,*,#8172,.T.);
#11843=ORIENTED_EDGE('',*,*,#8168,.T.);
#11844=ORIENTED_EDGE('',*,*,#8173,.T.);
#11845=ORIENTED_EDGE('',*,*,#8174,.F.);
#11846=ORIENTED_EDGE('',*,*,#8175,.T.);
#11847=ORIENTED_EDGE('',*,*,#8171,.T.);
#11848=ORIENTED_EDGE('',*,*,#8176,.T.);
#11849=ORIENTED_EDGE('',*,*,#8177,.F.);
#11850=ORIENTED_EDGE('',*,*,#8178,.T.);
#11851=ORIENTED_EDGE('',*,*,#8174,.T.);
#11852=ORIENTED_EDGE('',*,*,#8179,.T.);
#11853=ORIENTED_EDGE('',*,*,#8180,.F.);
#11854=ORIENTED_EDGE('',*,*,#8181,.T.);
#11855=ORIENTED_EDGE('',*,*,#8177,.T.);
#11856=ORIENTED_EDGE('',*,*,#8182,.T.);
#11857=ORIENTED_EDGE('',*,*,#8183,.F.);
#11858=ORIENTED_EDGE('',*,*,#8184,.T.);
#11859=ORIENTED_EDGE('',*,*,#8180,.T.);
#11860=ORIENTED_EDGE('',*,*,#8185,.T.);
#11861=ORIENTED_EDGE('',*,*,#8186,.F.);
#11862=ORIENTED_EDGE('',*,*,#8187,.T.);
#11863=ORIENTED_EDGE('',*,*,#8183,.T.);
#11864=ORIENTED_EDGE('',*,*,#8188,.T.);
#11865=ORIENTED_EDGE('',*,*,#8189,.F.);
#11866=ORIENTED_EDGE('',*,*,#8190,.T.);
#11867=ORIENTED_EDGE('',*,*,#8186,.T.);
#11868=ORIENTED_EDGE('',*,*,#8191,.T.);
#11869=ORIENTED_EDGE('',*,*,#8192,.F.);
#11870=ORIENTED_EDGE('',*,*,#8193,.T.);
#11871=ORIENTED_EDGE('',*,*,#8189,.T.);
#11872=ORIENTED_EDGE('',*,*,#8194,.T.);
#11873=ORIENTED_EDGE('',*,*,#8195,.F.);
#11874=ORIENTED_EDGE('',*,*,#8196,.T.);
#11875=ORIENTED_EDGE('',*,*,#8192,.T.);
#11876=ORIENTED_EDGE('',*,*,#8197,.T.);
#11877=ORIENTED_EDGE('',*,*,#8198,.F.);
#11878=ORIENTED_EDGE('',*,*,#8199,.T.);
#11879=ORIENTED_EDGE('',*,*,#8195,.T.);
#11880=ORIENTED_EDGE('',*,*,#8200,.T.);
#11881=ORIENTED_EDGE('',*,*,#8201,.F.);
#11882=ORIENTED_EDGE('',*,*,#8202,.T.);
#11883=ORIENTED_EDGE('',*,*,#8198,.T.);
#11884=ORIENTED_EDGE('',*,*,#8203,.T.);
#11885=ORIENTED_EDGE('',*,*,#8204,.F.);
#11886=ORIENTED_EDGE('',*,*,#8205,.T.);
#11887=ORIENTED_EDGE('',*,*,#8201,.T.);
#11888=ORIENTED_EDGE('',*,*,#8206,.T.);
#11889=ORIENTED_EDGE('',*,*,#8207,.F.);
#11890=ORIENTED_EDGE('',*,*,#8208,.T.);
#11891=ORIENTED_EDGE('',*,*,#8204,.T.);
#11892=ORIENTED_EDGE('',*,*,#8209,.T.);
#11893=ORIENTED_EDGE('',*,*,#8210,.F.);
#11894=ORIENTED_EDGE('',*,*,#8211,.T.);
#11895=ORIENTED_EDGE('',*,*,#8207,.T.);
#11896=ORIENTED_EDGE('',*,*,#8212,.T.);
#11897=ORIENTED_EDGE('',*,*,#8213,.F.);
#11898=ORIENTED_EDGE('',*,*,#8214,.T.);
#11899=ORIENTED_EDGE('',*,*,#8210,.T.);
#11900=ORIENTED_EDGE('',*,*,#8215,.T.);
#11901=ORIENTED_EDGE('',*,*,#8216,.F.);
#11902=ORIENTED_EDGE('',*,*,#8217,.T.);
#11903=ORIENTED_EDGE('',*,*,#8213,.T.);
#11904=ORIENTED_EDGE('',*,*,#8218,.T.);
#11905=ORIENTED_EDGE('',*,*,#8219,.F.);
#11906=ORIENTED_EDGE('',*,*,#8220,.T.);
#11907=ORIENTED_EDGE('',*,*,#8216,.T.);
#11908=ORIENTED_EDGE('',*,*,#8221,.T.);
#11909=ORIENTED_EDGE('',*,*,#8222,.F.);
#11910=ORIENTED_EDGE('',*,*,#8223,.T.);
#11911=ORIENTED_EDGE('',*,*,#8219,.T.);
#11912=ORIENTED_EDGE('',*,*,#8224,.T.);
#11913=ORIENTED_EDGE('',*,*,#8225,.F.);
#11914=ORIENTED_EDGE('',*,*,#8226,.T.);
#11915=ORIENTED_EDGE('',*,*,#8222,.T.);
#11916=ORIENTED_EDGE('',*,*,#8227,.T.);
#11917=ORIENTED_EDGE('',*,*,#8228,.F.);
#11918=ORIENTED_EDGE('',*,*,#8229,.T.);
#11919=ORIENTED_EDGE('',*,*,#8225,.T.);
#11920=ORIENTED_EDGE('',*,*,#8230,.T.);
#11921=ORIENTED_EDGE('',*,*,#8231,.F.);
#11922=ORIENTED_EDGE('',*,*,#8232,.T.);
#11923=ORIENTED_EDGE('',*,*,#8228,.T.);
#11924=ORIENTED_EDGE('',*,*,#8233,.T.);
#11925=ORIENTED_EDGE('',*,*,#8234,.F.);
#11926=ORIENTED_EDGE('',*,*,#8235,.T.);
#11927=ORIENTED_EDGE('',*,*,#8231,.T.);
#11928=ORIENTED_EDGE('',*,*,#8236,.T.);
#11929=ORIENTED_EDGE('',*,*,#8237,.F.);
#11930=ORIENTED_EDGE('',*,*,#8238,.T.);
#11931=ORIENTED_EDGE('',*,*,#8234,.T.);
#11932=ORIENTED_EDGE('',*,*,#8239,.T.);
#11933=ORIENTED_EDGE('',*,*,#8240,.T.);
#11934=ORIENTED_EDGE('',*,*,#8241,.T.);
#11935=ORIENTED_EDGE('',*,*,#8242,.T.);
#11936=ORIENTED_EDGE('',*,*,#8243,.T.);
#11937=ORIENTED_EDGE('',*,*,#8244,.T.);
#11938=ORIENTED_EDGE('',*,*,#8245,.T.);
#11939=ORIENTED_EDGE('',*,*,#8246,.T.);
#11940=ORIENTED_EDGE('',*,*,#8241,.F.);
#11941=ORIENTED_EDGE('',*,*,#8247,.F.);
#11942=ORIENTED_EDGE('',*,*,#8248,.T.);
#11943=ORIENTED_EDGE('',*,*,#8249,.F.);
#11944=ORIENTED_EDGE('',*,*,#8250,.F.);
#11945=ORIENTED_EDGE('',*,*,#8251,.F.);
#11946=ORIENTED_EDGE('',*,*,#8252,.T.);
#11947=ORIENTED_EDGE('',*,*,#8247,.T.);
#11948=ORIENTED_EDGE('',*,*,#8253,.F.);
#11949=ORIENTED_EDGE('',*,*,#8254,.F.);
#11950=ORIENTED_EDGE('',*,*,#8255,.T.);
#11951=ORIENTED_EDGE('',*,*,#8251,.T.);
#11952=ORIENTED_EDGE('',*,*,#8256,.F.);
#11953=ORIENTED_EDGE('',*,*,#8257,.F.);
#11954=ORIENTED_EDGE('',*,*,#8258,.T.);
#11955=ORIENTED_EDGE('',*,*,#8254,.T.);
#11956=ORIENTED_EDGE('',*,*,#8259,.F.);
#11957=ORIENTED_EDGE('',*,*,#8260,.F.);
#11958=ORIENTED_EDGE('',*,*,#8261,.T.);
#11959=ORIENTED_EDGE('',*,*,#8257,.T.);
#11960=ORIENTED_EDGE('',*,*,#8262,.F.);
#11961=ORIENTED_EDGE('',*,*,#8263,.F.);
#11962=ORIENTED_EDGE('',*,*,#8264,.T.);
#11963=ORIENTED_EDGE('',*,*,#8260,.T.);
#11964=ORIENTED_EDGE('',*,*,#8265,.F.);
#11965=ORIENTED_EDGE('',*,*,#8266,.F.);
#11966=ORIENTED_EDGE('',*,*,#8267,.T.);
#11967=ORIENTED_EDGE('',*,*,#8263,.T.);
#11968=ORIENTED_EDGE('',*,*,#8268,.F.);
#11969=ORIENTED_EDGE('',*,*,#8269,.F.);
#11970=ORIENTED_EDGE('',*,*,#8270,.T.);
#11971=ORIENTED_EDGE('',*,*,#8266,.T.);
#11972=ORIENTED_EDGE('',*,*,#8271,.F.);
#11973=ORIENTED_EDGE('',*,*,#8272,.F.);
#11974=ORIENTED_EDGE('',*,*,#8273,.T.);
#11975=ORIENTED_EDGE('',*,*,#8269,.T.);
#11976=ORIENTED_EDGE('',*,*,#8274,.F.);
#11977=ORIENTED_EDGE('',*,*,#8275,.F.);
#11978=ORIENTED_EDGE('',*,*,#8276,.T.);
#11979=ORIENTED_EDGE('',*,*,#8272,.T.);
#11980=ORIENTED_EDGE('',*,*,#8277,.F.);
#11981=ORIENTED_EDGE('',*,*,#8278,.F.);
#11982=ORIENTED_EDGE('',*,*,#8279,.T.);
#11983=ORIENTED_EDGE('',*,*,#8275,.T.);
#11984=ORIENTED_EDGE('',*,*,#8280,.F.);
#11985=ORIENTED_EDGE('',*,*,#8281,.F.);
#11986=ORIENTED_EDGE('',*,*,#8282,.T.);
#11987=ORIENTED_EDGE('',*,*,#8278,.T.);
#11988=ORIENTED_EDGE('',*,*,#8283,.F.);
#11989=ORIENTED_EDGE('',*,*,#8284,.F.);
#11990=ORIENTED_EDGE('',*,*,#8285,.T.);
#11991=ORIENTED_EDGE('',*,*,#8281,.T.);
#11992=ORIENTED_EDGE('',*,*,#8286,.F.);
#11993=ORIENTED_EDGE('',*,*,#8287,.F.);
#11994=ORIENTED_EDGE('',*,*,#8288,.T.);
#11995=ORIENTED_EDGE('',*,*,#8284,.T.);
#11996=ORIENTED_EDGE('',*,*,#8289,.F.);
#11997=ORIENTED_EDGE('',*,*,#8290,.F.);
#11998=ORIENTED_EDGE('',*,*,#8291,.T.);
#11999=ORIENTED_EDGE('',*,*,#8287,.T.);
#12000=ORIENTED_EDGE('',*,*,#8292,.F.);
#12001=ORIENTED_EDGE('',*,*,#8293,.F.);
#12002=ORIENTED_EDGE('',*,*,#8294,.T.);
#12003=ORIENTED_EDGE('',*,*,#8290,.T.);
#12004=ORIENTED_EDGE('',*,*,#8295,.F.);
#12005=ORIENTED_EDGE('',*,*,#8296,.F.);
#12006=ORIENTED_EDGE('',*,*,#8297,.T.);
#12007=ORIENTED_EDGE('',*,*,#8293,.T.);
#12008=ORIENTED_EDGE('',*,*,#8298,.F.);
#12009=ORIENTED_EDGE('',*,*,#8299,.F.);
#12010=ORIENTED_EDGE('',*,*,#8300,.T.);
#12011=ORIENTED_EDGE('',*,*,#8296,.T.);
#12012=ORIENTED_EDGE('',*,*,#8301,.F.);
#12013=ORIENTED_EDGE('',*,*,#8302,.F.);
#12014=ORIENTED_EDGE('',*,*,#8303,.T.);
#12015=ORIENTED_EDGE('',*,*,#8299,.T.);
#12016=ORIENTED_EDGE('',*,*,#8304,.F.);
#12017=ORIENTED_EDGE('',*,*,#8305,.F.);
#12018=ORIENTED_EDGE('',*,*,#8306,.T.);
#12019=ORIENTED_EDGE('',*,*,#8302,.T.);
#12020=ORIENTED_EDGE('',*,*,#8307,.F.);
#12021=ORIENTED_EDGE('',*,*,#8308,.F.);
#12022=ORIENTED_EDGE('',*,*,#8309,.T.);
#12023=ORIENTED_EDGE('',*,*,#8305,.T.);
#12024=ORIENTED_EDGE('',*,*,#8310,.F.);
#12025=ORIENTED_EDGE('',*,*,#8311,.F.);
#12026=ORIENTED_EDGE('',*,*,#8312,.T.);
#12027=ORIENTED_EDGE('',*,*,#8308,.T.);
#12028=ORIENTED_EDGE('',*,*,#8313,.F.);
#12029=ORIENTED_EDGE('',*,*,#8314,.F.);
#12030=ORIENTED_EDGE('',*,*,#8315,.T.);
#12031=ORIENTED_EDGE('',*,*,#8311,.T.);
#12032=ORIENTED_EDGE('',*,*,#8316,.F.);
#12033=ORIENTED_EDGE('',*,*,#8317,.F.);
#12034=ORIENTED_EDGE('',*,*,#8318,.T.);
#12035=ORIENTED_EDGE('',*,*,#8314,.T.);
#12036=ORIENTED_EDGE('',*,*,#8319,.F.);
#12037=ORIENTED_EDGE('',*,*,#8320,.F.);
#12038=ORIENTED_EDGE('',*,*,#8321,.T.);
#12039=ORIENTED_EDGE('',*,*,#8317,.T.);
#12040=ORIENTED_EDGE('',*,*,#8322,.F.);
#12041=ORIENTED_EDGE('',*,*,#8323,.F.);
#12042=ORIENTED_EDGE('',*,*,#8324,.T.);
#12043=ORIENTED_EDGE('',*,*,#8320,.T.);
#12044=ORIENTED_EDGE('',*,*,#8325,.F.);
#12045=ORIENTED_EDGE('',*,*,#8326,.F.);
#12046=ORIENTED_EDGE('',*,*,#8327,.T.);
#12047=ORIENTED_EDGE('',*,*,#8323,.T.);
#12048=ORIENTED_EDGE('',*,*,#8328,.F.);
#12049=ORIENTED_EDGE('',*,*,#8329,.F.);
#12050=ORIENTED_EDGE('',*,*,#8330,.T.);
#12051=ORIENTED_EDGE('',*,*,#8326,.T.);
#12052=ORIENTED_EDGE('',*,*,#8331,.F.);
#12053=ORIENTED_EDGE('',*,*,#8332,.F.);
#12054=ORIENTED_EDGE('',*,*,#8333,.T.);
#12055=ORIENTED_EDGE('',*,*,#8329,.T.);
#12056=ORIENTED_EDGE('',*,*,#8334,.F.);
#12057=ORIENTED_EDGE('',*,*,#8335,.F.);
#12058=ORIENTED_EDGE('',*,*,#8336,.T.);
#12059=ORIENTED_EDGE('',*,*,#8332,.T.);
#12060=ORIENTED_EDGE('',*,*,#8337,.F.);
#12061=ORIENTED_EDGE('',*,*,#8338,.F.);
#12062=ORIENTED_EDGE('',*,*,#8339,.T.);
#12063=ORIENTED_EDGE('',*,*,#8335,.T.);
#12064=ORIENTED_EDGE('',*,*,#8340,.F.);
#12065=ORIENTED_EDGE('',*,*,#8341,.F.);
#12066=ORIENTED_EDGE('',*,*,#8342,.T.);
#12067=ORIENTED_EDGE('',*,*,#8338,.T.);
#12068=ORIENTED_EDGE('',*,*,#8343,.F.);
#12069=ORIENTED_EDGE('',*,*,#8344,.F.);
#12070=ORIENTED_EDGE('',*,*,#8345,.T.);
#12071=ORIENTED_EDGE('',*,*,#8341,.T.);
#12072=ORIENTED_EDGE('',*,*,#8346,.F.);
#12073=ORIENTED_EDGE('',*,*,#8347,.F.);
#12074=ORIENTED_EDGE('',*,*,#8348,.T.);
#12075=ORIENTED_EDGE('',*,*,#8344,.T.);
#12076=ORIENTED_EDGE('',*,*,#8349,.F.);
#12077=ORIENTED_EDGE('',*,*,#8350,.F.);
#12078=ORIENTED_EDGE('',*,*,#8351,.T.);
#12079=ORIENTED_EDGE('',*,*,#8347,.T.);
#12080=ORIENTED_EDGE('',*,*,#8352,.F.);
#12081=ORIENTED_EDGE('',*,*,#8353,.F.);
#12082=ORIENTED_EDGE('',*,*,#8354,.T.);
#12083=ORIENTED_EDGE('',*,*,#8350,.T.);
#12084=ORIENTED_EDGE('',*,*,#8355,.F.);
#12085=ORIENTED_EDGE('',*,*,#8356,.F.);
#12086=ORIENTED_EDGE('',*,*,#8357,.T.);
#12087=ORIENTED_EDGE('',*,*,#8358,.T.);
#12088=ORIENTED_EDGE('',*,*,#8359,.F.);
#12089=ORIENTED_EDGE('',*,*,#8360,.F.);
#12090=ORIENTED_EDGE('',*,*,#8361,.T.);
#12091=ORIENTED_EDGE('',*,*,#8362,.T.);
#12092=ORIENTED_EDGE('',*,*,#8357,.F.);
#12093=ORIENTED_EDGE('',*,*,#8363,.F.);
#12094=ORIENTED_EDGE('',*,*,#8364,.T.);
#12095=ORIENTED_EDGE('',*,*,#8365,.T.);
#12096=ORIENTED_EDGE('',*,*,#8361,.F.);
#12097=ORIENTED_EDGE('',*,*,#8366,.F.);
#12098=ORIENTED_EDGE('',*,*,#8367,.T.);
#12099=ORIENTED_EDGE('',*,*,#8368,.T.);
#12100=ORIENTED_EDGE('',*,*,#8364,.F.);
#12101=ORIENTED_EDGE('',*,*,#8369,.F.);
#12102=ORIENTED_EDGE('',*,*,#8370,.T.);
#12103=ORIENTED_EDGE('',*,*,#8371,.T.);
#12104=ORIENTED_EDGE('',*,*,#8367,.F.);
#12105=ORIENTED_EDGE('',*,*,#8372,.F.);
#12106=ORIENTED_EDGE('',*,*,#8359,.T.);
#12107=ORIENTED_EDGE('',*,*,#8373,.T.);
#12108=ORIENTED_EDGE('',*,*,#8370,.F.);
#12109=ORIENTED_EDGE('',*,*,#8373,.F.);
#12110=ORIENTED_EDGE('',*,*,#8358,.F.);
#12111=ORIENTED_EDGE('',*,*,#8362,.F.);
#12112=ORIENTED_EDGE('',*,*,#8365,.F.);
#12113=ORIENTED_EDGE('',*,*,#8368,.F.);
#12114=ORIENTED_EDGE('',*,*,#8371,.F.);
#12115=ORIENTED_EDGE('',*,*,#8374,.T.);
#12116=ORIENTED_EDGE('',*,*,#8375,.T.);
#12117=ORIENTED_EDGE('',*,*,#8376,.F.);
#12118=ORIENTED_EDGE('',*,*,#8375,.F.);
#12119=ORIENTED_EDGE('',*,*,#8240,.F.);
#12120=ORIENTED_EDGE('',*,*,#8374,.F.);
#12121=ORIENTED_EDGE('',*,*,#8377,.F.);
#12122=ORIENTED_EDGE('',*,*,#8376,.T.);
#12123=ORIENTED_EDGE('',*,*,#8378,.F.);
#12124=ORIENTED_EDGE('',*,*,#8379,.T.);
#12125=ORIENTED_EDGE('',*,*,#8377,.T.);
#12126=ORIENTED_EDGE('',*,*,#8379,.F.);
#12127=ORIENTED_EDGE('',*,*,#8249,.T.);
#12128=ORIENTED_EDGE('',*,*,#8380,.T.);
#12129=ORIENTED_EDGE('',*,*,#8242,.F.);
#12130=ORIENTED_EDGE('',*,*,#8246,.F.);
#12131=ORIENTED_EDGE('',*,*,#8381,.T.);
#12132=ORIENTED_EDGE('',*,*,#8381,.F.);
#12133=ORIENTED_EDGE('',*,*,#8245,.F.);
#12134=ORIENTED_EDGE('',*,*,#8382,.F.);
#12135=ORIENTED_EDGE('',*,*,#8239,.F.);
#12136=ORIENTED_EDGE('',*,*,#8236,.F.);
#12137=ORIENTED_EDGE('',*,*,#8233,.F.);
#12138=ORIENTED_EDGE('',*,*,#8230,.F.);
#12139=ORIENTED_EDGE('',*,*,#8227,.F.);
#12140=ORIENTED_EDGE('',*,*,#8224,.F.);
#12141=ORIENTED_EDGE('',*,*,#8221,.F.);
#12142=ORIENTED_EDGE('',*,*,#8218,.F.);
#12143=ORIENTED_EDGE('',*,*,#8215,.F.);
#12144=ORIENTED_EDGE('',*,*,#8212,.F.);
#12145=ORIENTED_EDGE('',*,*,#8209,.F.);
#12146=ORIENTED_EDGE('',*,*,#8206,.F.);
#12147=ORIENTED_EDGE('',*,*,#8203,.F.);
#12148=ORIENTED_EDGE('',*,*,#8200,.F.);
#12149=ORIENTED_EDGE('',*,*,#8197,.F.);
#12150=ORIENTED_EDGE('',*,*,#8194,.F.);
#12151=ORIENTED_EDGE('',*,*,#8191,.F.);
#12152=ORIENTED_EDGE('',*,*,#8188,.F.);
#12153=ORIENTED_EDGE('',*,*,#8185,.F.);
#12154=ORIENTED_EDGE('',*,*,#8182,.F.);
#12155=ORIENTED_EDGE('',*,*,#8179,.F.);
#12156=ORIENTED_EDGE('',*,*,#8176,.F.);
#12157=ORIENTED_EDGE('',*,*,#8173,.F.);
#12158=ORIENTED_EDGE('',*,*,#8170,.F.);
#12159=ORIENTED_EDGE('',*,*,#8167,.F.);
#12160=ORIENTED_EDGE('',*,*,#8164,.F.);
#12161=ORIENTED_EDGE('',*,*,#8161,.F.);
#12162=ORIENTED_EDGE('',*,*,#8158,.F.);
#12163=ORIENTED_EDGE('',*,*,#8155,.F.);
#12164=ORIENTED_EDGE('',*,*,#8152,.F.);
#12165=ORIENTED_EDGE('',*,*,#8149,.F.);
#12166=ORIENTED_EDGE('',*,*,#8146,.F.);
#12167=ORIENTED_EDGE('',*,*,#8143,.F.);
#12168=ORIENTED_EDGE('',*,*,#8140,.F.);
#12169=ORIENTED_EDGE('',*,*,#8137,.F.);
#12170=ORIENTED_EDGE('',*,*,#8134,.F.);
#12171=ORIENTED_EDGE('',*,*,#8383,.F.);
#12172=ORIENTED_EDGE('',*,*,#8384,.T.);
#12173=ORIENTED_EDGE('',*,*,#8355,.T.);
#12174=ORIENTED_EDGE('',*,*,#8352,.T.);
#12175=ORIENTED_EDGE('',*,*,#8349,.T.);
#12176=ORIENTED_EDGE('',*,*,#8346,.T.);
#12177=ORIENTED_EDGE('',*,*,#8343,.T.);
#12178=ORIENTED_EDGE('',*,*,#8340,.T.);
#12179=ORIENTED_EDGE('',*,*,#8337,.T.);
#12180=ORIENTED_EDGE('',*,*,#8334,.T.);
#12181=ORIENTED_EDGE('',*,*,#8331,.T.);
#12182=ORIENTED_EDGE('',*,*,#8328,.T.);
#12183=ORIENTED_EDGE('',*,*,#8325,.T.);
#12184=ORIENTED_EDGE('',*,*,#8322,.T.);
#12185=ORIENTED_EDGE('',*,*,#8319,.T.);
#12186=ORIENTED_EDGE('',*,*,#8316,.T.);
#12187=ORIENTED_EDGE('',*,*,#8313,.T.);
#12188=ORIENTED_EDGE('',*,*,#8310,.T.);
#12189=ORIENTED_EDGE('',*,*,#8307,.T.);
#12190=ORIENTED_EDGE('',*,*,#8304,.T.);
#12191=ORIENTED_EDGE('',*,*,#8301,.T.);
#12192=ORIENTED_EDGE('',*,*,#8298,.T.);
#12193=ORIENTED_EDGE('',*,*,#8295,.T.);
#12194=ORIENTED_EDGE('',*,*,#8292,.T.);
#12195=ORIENTED_EDGE('',*,*,#8289,.T.);
#12196=ORIENTED_EDGE('',*,*,#8286,.T.);
#12197=ORIENTED_EDGE('',*,*,#8283,.T.);
#12198=ORIENTED_EDGE('',*,*,#8280,.T.);
#12199=ORIENTED_EDGE('',*,*,#8277,.T.);
#12200=ORIENTED_EDGE('',*,*,#8274,.T.);
#12201=ORIENTED_EDGE('',*,*,#8271,.T.);
#12202=ORIENTED_EDGE('',*,*,#8268,.T.);
#12203=ORIENTED_EDGE('',*,*,#8265,.T.);
#12204=ORIENTED_EDGE('',*,*,#8262,.T.);
#12205=ORIENTED_EDGE('',*,*,#8259,.T.);
#12206=ORIENTED_EDGE('',*,*,#8256,.T.);
#12207=ORIENTED_EDGE('',*,*,#8253,.T.);
#12208=ORIENTED_EDGE('',*,*,#8250,.T.);
#12209=ORIENTED_EDGE('',*,*,#8353,.T.);
#12210=ORIENTED_EDGE('',*,*,#8384,.F.);
#12211=ORIENTED_EDGE('',*,*,#8385,.F.);
#12212=ORIENTED_EDGE('',*,*,#8386,.T.);
#12213=ORIENTED_EDGE('',*,*,#8380,.F.);
#12214=ORIENTED_EDGE('',*,*,#8248,.F.);
#12215=ORIENTED_EDGE('',*,*,#8252,.F.);
#12216=ORIENTED_EDGE('',*,*,#8255,.F.);
#12217=ORIENTED_EDGE('',*,*,#8258,.F.);
#12218=ORIENTED_EDGE('',*,*,#8261,.F.);
#12219=ORIENTED_EDGE('',*,*,#8264,.F.);
#12220=ORIENTED_EDGE('',*,*,#8267,.F.);
#12221=ORIENTED_EDGE('',*,*,#8270,.F.);
#12222=ORIENTED_EDGE('',*,*,#8273,.F.);
#12223=ORIENTED_EDGE('',*,*,#8276,.F.);
#12224=ORIENTED_EDGE('',*,*,#8279,.F.);
#12225=ORIENTED_EDGE('',*,*,#8282,.F.);
#12226=ORIENTED_EDGE('',*,*,#8285,.F.);
#12227=ORIENTED_EDGE('',*,*,#8288,.F.);
#12228=ORIENTED_EDGE('',*,*,#8291,.F.);
#12229=ORIENTED_EDGE('',*,*,#8294,.F.);
#12230=ORIENTED_EDGE('',*,*,#8297,.F.);
#12231=ORIENTED_EDGE('',*,*,#8300,.F.);
#12232=ORIENTED_EDGE('',*,*,#8303,.F.);
#12233=ORIENTED_EDGE('',*,*,#8306,.F.);
#12234=ORIENTED_EDGE('',*,*,#8309,.F.);
#12235=ORIENTED_EDGE('',*,*,#8312,.F.);
#12236=ORIENTED_EDGE('',*,*,#8315,.F.);
#12237=ORIENTED_EDGE('',*,*,#8318,.F.);
#12238=ORIENTED_EDGE('',*,*,#8321,.F.);
#12239=ORIENTED_EDGE('',*,*,#8324,.F.);
#12240=ORIENTED_EDGE('',*,*,#8327,.F.);
#12241=ORIENTED_EDGE('',*,*,#8330,.F.);
#12242=ORIENTED_EDGE('',*,*,#8333,.F.);
#12243=ORIENTED_EDGE('',*,*,#8336,.F.);
#12244=ORIENTED_EDGE('',*,*,#8339,.F.);
#12245=ORIENTED_EDGE('',*,*,#8342,.F.);
#12246=ORIENTED_EDGE('',*,*,#8345,.F.);
#12247=ORIENTED_EDGE('',*,*,#8348,.F.);
#12248=ORIENTED_EDGE('',*,*,#8351,.F.);
#12249=ORIENTED_EDGE('',*,*,#8354,.F.);
#12250=ORIENTED_EDGE('',*,*,#8386,.F.);
#12251=ORIENTED_EDGE('',*,*,#8387,.F.);
#12252=ORIENTED_EDGE('',*,*,#8132,.F.);
#12253=ORIENTED_EDGE('',*,*,#8136,.F.);
#12254=ORIENTED_EDGE('',*,*,#8139,.F.);
#12255=ORIENTED_EDGE('',*,*,#8142,.F.);
#12256=ORIENTED_EDGE('',*,*,#8145,.F.);
#12257=ORIENTED_EDGE('',*,*,#8148,.F.);
#12258=ORIENTED_EDGE('',*,*,#8151,.F.);
#12259=ORIENTED_EDGE('',*,*,#8154,.F.);
#12260=ORIENTED_EDGE('',*,*,#8157,.F.);
#12261=ORIENTED_EDGE('',*,*,#8160,.F.);
#12262=ORIENTED_EDGE('',*,*,#8163,.F.);
#12263=ORIENTED_EDGE('',*,*,#8166,.F.);
#12264=ORIENTED_EDGE('',*,*,#8169,.F.);
#12265=ORIENTED_EDGE('',*,*,#8172,.F.);
#12266=ORIENTED_EDGE('',*,*,#8175,.F.);
#12267=ORIENTED_EDGE('',*,*,#8178,.F.);
#12268=ORIENTED_EDGE('',*,*,#8181,.F.);
#12269=ORIENTED_EDGE('',*,*,#8184,.F.);
#12270=ORIENTED_EDGE('',*,*,#8187,.F.);
#12271=ORIENTED_EDGE('',*,*,#8190,.F.);
#12272=ORIENTED_EDGE('',*,*,#8193,.F.);
#12273=ORIENTED_EDGE('',*,*,#8196,.F.);
#12274=ORIENTED_EDGE('',*,*,#8199,.F.);
#12275=ORIENTED_EDGE('',*,*,#8202,.F.);
#12276=ORIENTED_EDGE('',*,*,#8205,.F.);
#12277=ORIENTED_EDGE('',*,*,#8208,.F.);
#12278=ORIENTED_EDGE('',*,*,#8211,.F.);
#12279=ORIENTED_EDGE('',*,*,#8214,.F.);
#12280=ORIENTED_EDGE('',*,*,#8217,.F.);
#12281=ORIENTED_EDGE('',*,*,#8220,.F.);
#12282=ORIENTED_EDGE('',*,*,#8223,.F.);
#12283=ORIENTED_EDGE('',*,*,#8226,.F.);
#12284=ORIENTED_EDGE('',*,*,#8229,.F.);
#12285=ORIENTED_EDGE('',*,*,#8232,.F.);
#12286=ORIENTED_EDGE('',*,*,#8235,.F.);
#12287=ORIENTED_EDGE('',*,*,#8238,.F.);
#12288=ORIENTED_EDGE('',*,*,#8388,.F.);
#12289=ORIENTED_EDGE('',*,*,#8243,.F.);
#12290=ORIENTED_EDGE('',*,*,#8244,.F.);
#12291=ORIENTED_EDGE('',*,*,#8388,.T.);
#12292=ORIENTED_EDGE('',*,*,#8237,.T.);
#12293=ORIENTED_EDGE('',*,*,#8382,.T.);
#12294=ORIENTED_EDGE('',*,*,#8389,.F.);
#12295=ORIENTED_EDGE('',*,*,#8378,.T.);
#12296=ORIENTED_EDGE('',*,*,#8390,.F.);
#12297=ORIENTED_EDGE('',*,*,#8391,.T.);
#12298=ORIENTED_EDGE('',*,*,#8389,.T.);
#12299=ORIENTED_EDGE('',*,*,#8391,.F.);
#12300=ORIENTED_EDGE('',*,*,#8390,.T.);
#12301=ORIENTED_EDGE('',*,*,#8356,.T.);
#12302=ORIENTED_EDGE('',*,*,#8372,.T.);
#12303=ORIENTED_EDGE('',*,*,#8369,.T.);
#12304=ORIENTED_EDGE('',*,*,#8366,.T.);
#12305=ORIENTED_EDGE('',*,*,#8363,.T.);
#12306=ORIENTED_EDGE('',*,*,#8360,.T.);
#12307=ORIENTED_EDGE('',*,*,#8383,.T.);
#12308=ORIENTED_EDGE('',*,*,#8133,.F.);
#12309=ORIENTED_EDGE('',*,*,#8387,.T.);
#12310=ORIENTED_EDGE('',*,*,#8385,.T.);
#12311=ORIENTED_EDGE('',*,*,#8392,.F.);
#12312=ORIENTED_EDGE('',*,*,#8393,.F.);
#12313=ORIENTED_EDGE('',*,*,#8394,.F.);
#12314=ORIENTED_EDGE('',*,*,#8395,.F.);
#12315=ORIENTED_EDGE('',*,*,#8396,.F.);
#12316=ORIENTED_EDGE('',*,*,#8397,.F.);
#12317=ORIENTED_EDGE('',*,*,#8398,.F.);
#12318=ORIENTED_EDGE('',*,*,#8399,.F.);
#12319=ORIENTED_EDGE('',*,*,#8399,.T.);
#12320=ORIENTED_EDGE('',*,*,#8400,.F.);
#12321=ORIENTED_EDGE('',*,*,#8393,.T.);
#12322=ORIENTED_EDGE('',*,*,#8401,.F.);
#12323=ORIENTED_EDGE('',*,*,#8396,.T.);
#12324=ORIENTED_EDGE('',*,*,#8401,.T.);
#12325=ORIENTED_EDGE('',*,*,#8392,.T.);
#12326=ORIENTED_EDGE('',*,*,#8402,.F.);
#12327=ORIENTED_EDGE('',*,*,#8398,.T.);
#12328=ORIENTED_EDGE('',*,*,#8403,.F.);
#12329=ORIENTED_EDGE('',*,*,#8394,.T.);
#12330=ORIENTED_EDGE('',*,*,#8400,.T.);
#12331=ORIENTED_EDGE('',*,*,#8397,.T.);
#12332=ORIENTED_EDGE('',*,*,#8402,.T.);
#12333=ORIENTED_EDGE('',*,*,#8395,.T.);
#12334=ORIENTED_EDGE('',*,*,#8403,.T.);
#12335=ORIENTED_EDGE('',*,*,#8404,.F.);
#12336=ORIENTED_EDGE('',*,*,#8405,.T.);
#12337=ORIENTED_EDGE('',*,*,#8406,.T.);
#12338=ORIENTED_EDGE('',*,*,#8405,.F.);
#12339=ORIENTED_EDGE('',*,*,#8407,.F.);
#12340=ORIENTED_EDGE('',*,*,#8408,.T.);
#12341=ORIENTED_EDGE('',*,*,#8409,.T.);
#12342=ORIENTED_EDGE('',*,*,#8408,.F.);
#12343=ORIENTED_EDGE('',*,*,#8407,.T.);
#12344=ORIENTED_EDGE('',*,*,#8404,.T.);
#12345=ORIENTED_EDGE('',*,*,#8409,.F.);
#12346=ORIENTED_EDGE('',*,*,#8406,.F.);
#12347=ORIENTED_EDGE('',*,*,#8410,.F.);
#12348=ORIENTED_EDGE('',*,*,#8411,.T.);
#12349=ORIENTED_EDGE('',*,*,#8412,.T.);
#12350=ORIENTED_EDGE('',*,*,#8411,.F.);
#12351=ORIENTED_EDGE('',*,*,#8413,.F.);
#12352=ORIENTED_EDGE('',*,*,#8414,.T.);
#12353=ORIENTED_EDGE('',*,*,#8415,.T.);
#12354=ORIENTED_EDGE('',*,*,#8414,.F.);
#12355=ORIENTED_EDGE('',*,*,#8413,.T.);
#12356=ORIENTED_EDGE('',*,*,#8410,.T.);
#12357=ORIENTED_EDGE('',*,*,#8415,.F.);
#12358=ORIENTED_EDGE('',*,*,#8412,.F.);
#12359=ORIENTED_EDGE('',*,*,#8416,.F.);
#12360=ORIENTED_EDGE('',*,*,#8417,.T.);
#12361=ORIENTED_EDGE('',*,*,#8418,.T.);
#12362=ORIENTED_EDGE('',*,*,#8419,.T.);
#12363=ORIENTED_EDGE('',*,*,#8420,.F.);
#12364=ORIENTED_EDGE('',*,*,#8421,.T.);
#12365=ORIENTED_EDGE('',*,*,#8416,.T.);
#12366=ORIENTED_EDGE('',*,*,#8422,.T.);
#12367=ORIENTED_EDGE('',*,*,#8423,.F.);
#12368=ORIENTED_EDGE('',*,*,#8424,.T.);
#12369=ORIENTED_EDGE('',*,*,#8420,.T.);
#12370=ORIENTED_EDGE('',*,*,#8425,.T.);
#12371=ORIENTED_EDGE('',*,*,#8426,.F.);
#12372=ORIENTED_EDGE('',*,*,#8427,.T.);
#12373=ORIENTED_EDGE('',*,*,#8423,.T.);
#12374=ORIENTED_EDGE('',*,*,#8428,.T.);
#12375=ORIENTED_EDGE('',*,*,#8429,.F.);
#12376=ORIENTED_EDGE('',*,*,#8430,.T.);
#12377=ORIENTED_EDGE('',*,*,#8426,.T.);
#12378=ORIENTED_EDGE('',*,*,#8431,.T.);
#12379=ORIENTED_EDGE('',*,*,#8432,.F.);
#12380=ORIENTED_EDGE('',*,*,#8433,.T.);
#12381=ORIENTED_EDGE('',*,*,#8429,.T.);
#12382=ORIENTED_EDGE('',*,*,#8434,.T.);
#12383=ORIENTED_EDGE('',*,*,#8435,.F.);
#12384=ORIENTED_EDGE('',*,*,#8436,.T.);
#12385=ORIENTED_EDGE('',*,*,#8432,.T.);
#12386=ORIENTED_EDGE('',*,*,#8437,.T.);
#12387=ORIENTED_EDGE('',*,*,#8438,.F.);
#12388=ORIENTED_EDGE('',*,*,#8439,.T.);
#12389=ORIENTED_EDGE('',*,*,#8435,.T.);
#12390=ORIENTED_EDGE('',*,*,#8440,.T.);
#12391=ORIENTED_EDGE('',*,*,#8441,.F.);
#12392=ORIENTED_EDGE('',*,*,#8442,.T.);
#12393=ORIENTED_EDGE('',*,*,#8438,.T.);
#12394=ORIENTED_EDGE('',*,*,#8443,.T.);
#12395=ORIENTED_EDGE('',*,*,#8444,.F.);
#12396=ORIENTED_EDGE('',*,*,#8445,.T.);
#12397=ORIENTED_EDGE('',*,*,#8441,.T.);
#12398=ORIENTED_EDGE('',*,*,#8446,.T.);
#12399=ORIENTED_EDGE('',*,*,#8447,.F.);
#12400=ORIENTED_EDGE('',*,*,#8448,.T.);
#12401=ORIENTED_EDGE('',*,*,#8444,.T.);
#12402=ORIENTED_EDGE('',*,*,#8449,.T.);
#12403=ORIENTED_EDGE('',*,*,#8450,.F.);
#12404=ORIENTED_EDGE('',*,*,#8451,.T.);
#12405=ORIENTED_EDGE('',*,*,#8447,.T.);
#12406=ORIENTED_EDGE('',*,*,#8452,.T.);
#12407=ORIENTED_EDGE('',*,*,#8453,.F.);
#12408=ORIENTED_EDGE('',*,*,#8454,.T.);
#12409=ORIENTED_EDGE('',*,*,#8450,.T.);
#12410=ORIENTED_EDGE('',*,*,#8455,.T.);
#12411=ORIENTED_EDGE('',*,*,#8456,.F.);
#12412=ORIENTED_EDGE('',*,*,#8457,.T.);
#12413=ORIENTED_EDGE('',*,*,#8453,.T.);
#12414=ORIENTED_EDGE('',*,*,#8458,.T.);
#12415=ORIENTED_EDGE('',*,*,#8459,.F.);
#12416=ORIENTED_EDGE('',*,*,#8460,.T.);
#12417=ORIENTED_EDGE('',*,*,#8456,.T.);
#12418=ORIENTED_EDGE('',*,*,#8461,.T.);
#12419=ORIENTED_EDGE('',*,*,#8462,.F.);
#12420=ORIENTED_EDGE('',*,*,#8463,.T.);
#12421=ORIENTED_EDGE('',*,*,#8459,.T.);
#12422=ORIENTED_EDGE('',*,*,#8464,.T.);
#12423=ORIENTED_EDGE('',*,*,#8465,.F.);
#12424=ORIENTED_EDGE('',*,*,#8466,.T.);
#12425=ORIENTED_EDGE('',*,*,#8462,.T.);
#12426=ORIENTED_EDGE('',*,*,#8467,.T.);
#12427=ORIENTED_EDGE('',*,*,#8468,.F.);
#12428=ORIENTED_EDGE('',*,*,#8469,.T.);
#12429=ORIENTED_EDGE('',*,*,#8465,.T.);
#12430=ORIENTED_EDGE('',*,*,#8470,.T.);
#12431=ORIENTED_EDGE('',*,*,#8471,.F.);
#12432=ORIENTED_EDGE('',*,*,#8472,.T.);
#12433=ORIENTED_EDGE('',*,*,#8468,.T.);
#12434=ORIENTED_EDGE('',*,*,#8473,.T.);
#12435=ORIENTED_EDGE('',*,*,#8474,.F.);
#12436=ORIENTED_EDGE('',*,*,#8475,.T.);
#12437=ORIENTED_EDGE('',*,*,#8471,.T.);
#12438=ORIENTED_EDGE('',*,*,#8476,.T.);
#12439=ORIENTED_EDGE('',*,*,#8477,.F.);
#12440=ORIENTED_EDGE('',*,*,#8478,.T.);
#12441=ORIENTED_EDGE('',*,*,#8474,.T.);
#12442=ORIENTED_EDGE('',*,*,#8479,.T.);
#12443=ORIENTED_EDGE('',*,*,#8480,.F.);
#12444=ORIENTED_EDGE('',*,*,#8481,.T.);
#12445=ORIENTED_EDGE('',*,*,#8477,.T.);
#12446=ORIENTED_EDGE('',*,*,#8482,.T.);
#12447=ORIENTED_EDGE('',*,*,#8483,.F.);
#12448=ORIENTED_EDGE('',*,*,#8484,.T.);
#12449=ORIENTED_EDGE('',*,*,#8480,.T.);
#12450=ORIENTED_EDGE('',*,*,#8485,.T.);
#12451=ORIENTED_EDGE('',*,*,#8486,.F.);
#12452=ORIENTED_EDGE('',*,*,#8487,.T.);
#12453=ORIENTED_EDGE('',*,*,#8483,.T.);
#12454=ORIENTED_EDGE('',*,*,#8488,.T.);
#12455=ORIENTED_EDGE('',*,*,#8489,.F.);
#12456=ORIENTED_EDGE('',*,*,#8490,.T.);
#12457=ORIENTED_EDGE('',*,*,#8486,.T.);
#12458=ORIENTED_EDGE('',*,*,#8491,.T.);
#12459=ORIENTED_EDGE('',*,*,#8492,.F.);
#12460=ORIENTED_EDGE('',*,*,#8493,.T.);
#12461=ORIENTED_EDGE('',*,*,#8489,.T.);
#12462=ORIENTED_EDGE('',*,*,#8494,.T.);
#12463=ORIENTED_EDGE('',*,*,#8495,.F.);
#12464=ORIENTED_EDGE('',*,*,#8496,.T.);
#12465=ORIENTED_EDGE('',*,*,#8492,.T.);
#12466=ORIENTED_EDGE('',*,*,#8497,.T.);
#12467=ORIENTED_EDGE('',*,*,#8498,.F.);
#12468=ORIENTED_EDGE('',*,*,#8499,.T.);
#12469=ORIENTED_EDGE('',*,*,#8495,.T.);
#12470=ORIENTED_EDGE('',*,*,#8500,.T.);
#12471=ORIENTED_EDGE('',*,*,#8501,.F.);
#12472=ORIENTED_EDGE('',*,*,#8502,.T.);
#12473=ORIENTED_EDGE('',*,*,#8498,.T.);
#12474=ORIENTED_EDGE('',*,*,#8503,.T.);
#12475=ORIENTED_EDGE('',*,*,#8504,.F.);
#12476=ORIENTED_EDGE('',*,*,#8505,.T.);
#12477=ORIENTED_EDGE('',*,*,#8501,.T.);
#12478=ORIENTED_EDGE('',*,*,#8506,.T.);
#12479=ORIENTED_EDGE('',*,*,#8507,.F.);
#12480=ORIENTED_EDGE('',*,*,#8508,.T.);
#12481=ORIENTED_EDGE('',*,*,#8504,.T.);
#12482=ORIENTED_EDGE('',*,*,#8509,.T.);
#12483=ORIENTED_EDGE('',*,*,#8510,.F.);
#12484=ORIENTED_EDGE('',*,*,#8511,.T.);
#12485=ORIENTED_EDGE('',*,*,#8507,.T.);
#12486=ORIENTED_EDGE('',*,*,#8512,.T.);
#12487=ORIENTED_EDGE('',*,*,#8513,.F.);
#12488=ORIENTED_EDGE('',*,*,#8514,.T.);
#12489=ORIENTED_EDGE('',*,*,#8510,.T.);
#12490=ORIENTED_EDGE('',*,*,#8515,.T.);
#12491=ORIENTED_EDGE('',*,*,#8516,.F.);
#12492=ORIENTED_EDGE('',*,*,#8517,.T.);
#12493=ORIENTED_EDGE('',*,*,#8513,.T.);
#12494=ORIENTED_EDGE('',*,*,#8518,.T.);
#12495=ORIENTED_EDGE('',*,*,#8519,.F.);
#12496=ORIENTED_EDGE('',*,*,#8520,.T.);
#12497=ORIENTED_EDGE('',*,*,#8516,.T.);
#12498=ORIENTED_EDGE('',*,*,#8521,.T.);
#12499=ORIENTED_EDGE('',*,*,#8522,.F.);
#12500=ORIENTED_EDGE('',*,*,#8523,.T.);
#12501=ORIENTED_EDGE('',*,*,#8519,.T.);
#12502=ORIENTED_EDGE('',*,*,#8524,.T.);
#12503=ORIENTED_EDGE('',*,*,#8525,.F.);
#12504=ORIENTED_EDGE('',*,*,#8526,.T.);
#12505=ORIENTED_EDGE('',*,*,#8522,.T.);
#12506=ORIENTED_EDGE('',*,*,#8527,.T.);
#12507=ORIENTED_EDGE('',*,*,#8528,.F.);
#12508=ORIENTED_EDGE('',*,*,#8529,.T.);
#12509=ORIENTED_EDGE('',*,*,#8525,.T.);
#12510=ORIENTED_EDGE('',*,*,#8530,.T.);
#12511=ORIENTED_EDGE('',*,*,#8531,.F.);
#12512=ORIENTED_EDGE('',*,*,#8532,.T.);
#12513=ORIENTED_EDGE('',*,*,#8528,.T.);
#12514=ORIENTED_EDGE('',*,*,#8533,.T.);
#12515=ORIENTED_EDGE('',*,*,#8534,.F.);
#12516=ORIENTED_EDGE('',*,*,#8535,.T.);
#12517=ORIENTED_EDGE('',*,*,#8536,.T.);
#12518=ORIENTED_EDGE('',*,*,#8537,.F.);
#12519=ORIENTED_EDGE('',*,*,#8538,.F.);
#12520=ORIENTED_EDGE('',*,*,#8539,.T.);
#12521=ORIENTED_EDGE('',*,*,#8534,.T.);
#12522=ORIENTED_EDGE('',*,*,#8540,.F.);
#12523=ORIENTED_EDGE('',*,*,#8541,.F.);
#12524=ORIENTED_EDGE('',*,*,#8542,.T.);
#12525=ORIENTED_EDGE('',*,*,#8538,.T.);
#12526=ORIENTED_EDGE('',*,*,#8543,.F.);
#12527=ORIENTED_EDGE('',*,*,#8544,.F.);
#12528=ORIENTED_EDGE('',*,*,#8545,.T.);
#12529=ORIENTED_EDGE('',*,*,#8541,.T.);
#12530=ORIENTED_EDGE('',*,*,#8546,.F.);
#12531=ORIENTED_EDGE('',*,*,#8547,.F.);
#12532=ORIENTED_EDGE('',*,*,#8548,.T.);
#12533=ORIENTED_EDGE('',*,*,#8544,.T.);
#12534=ORIENTED_EDGE('',*,*,#8549,.F.);
#12535=ORIENTED_EDGE('',*,*,#8550,.F.);
#12536=ORIENTED_EDGE('',*,*,#8551,.T.);
#12537=ORIENTED_EDGE('',*,*,#8547,.T.);
#12538=ORIENTED_EDGE('',*,*,#8552,.F.);
#12539=ORIENTED_EDGE('',*,*,#8553,.F.);
#12540=ORIENTED_EDGE('',*,*,#8554,.T.);
#12541=ORIENTED_EDGE('',*,*,#8550,.T.);
#12542=ORIENTED_EDGE('',*,*,#8555,.F.);
#12543=ORIENTED_EDGE('',*,*,#8556,.F.);
#12544=ORIENTED_EDGE('',*,*,#8557,.T.);
#12545=ORIENTED_EDGE('',*,*,#8553,.T.);
#12546=ORIENTED_EDGE('',*,*,#8558,.F.);
#12547=ORIENTED_EDGE('',*,*,#8559,.F.);
#12548=ORIENTED_EDGE('',*,*,#8560,.T.);
#12549=ORIENTED_EDGE('',*,*,#8556,.T.);
#12550=ORIENTED_EDGE('',*,*,#8561,.F.);
#12551=ORIENTED_EDGE('',*,*,#8562,.F.);
#12552=ORIENTED_EDGE('',*,*,#8563,.T.);
#12553=ORIENTED_EDGE('',*,*,#8559,.T.);
#12554=ORIENTED_EDGE('',*,*,#8564,.F.);
#12555=ORIENTED_EDGE('',*,*,#8565,.F.);
#12556=ORIENTED_EDGE('',*,*,#8566,.T.);
#12557=ORIENTED_EDGE('',*,*,#8562,.T.);
#12558=ORIENTED_EDGE('',*,*,#8567,.F.);
#12559=ORIENTED_EDGE('',*,*,#8568,.F.);
#12560=ORIENTED_EDGE('',*,*,#8569,.T.);
#12561=ORIENTED_EDGE('',*,*,#8565,.T.);
#12562=ORIENTED_EDGE('',*,*,#8570,.F.);
#12563=ORIENTED_EDGE('',*,*,#8571,.F.);
#12564=ORIENTED_EDGE('',*,*,#8572,.T.);
#12565=ORIENTED_EDGE('',*,*,#8568,.T.);
#12566=ORIENTED_EDGE('',*,*,#8573,.F.);
#12567=ORIENTED_EDGE('',*,*,#8574,.F.);
#12568=ORIENTED_EDGE('',*,*,#8575,.T.);
#12569=ORIENTED_EDGE('',*,*,#8571,.T.);
#12570=ORIENTED_EDGE('',*,*,#8576,.F.);
#12571=ORIENTED_EDGE('',*,*,#8577,.F.);
#12572=ORIENTED_EDGE('',*,*,#8578,.T.);
#12573=ORIENTED_EDGE('',*,*,#8574,.T.);
#12574=ORIENTED_EDGE('',*,*,#8579,.F.);
#12575=ORIENTED_EDGE('',*,*,#8580,.F.);
#12576=ORIENTED_EDGE('',*,*,#8581,.T.);
#12577=ORIENTED_EDGE('',*,*,#8577,.T.);
#12578=ORIENTED_EDGE('',*,*,#8582,.F.);
#12579=ORIENTED_EDGE('',*,*,#8583,.F.);
#12580=ORIENTED_EDGE('',*,*,#8584,.T.);
#12581=ORIENTED_EDGE('',*,*,#8580,.T.);
#12582=ORIENTED_EDGE('',*,*,#8585,.F.);
#12583=ORIENTED_EDGE('',*,*,#8586,.F.);
#12584=ORIENTED_EDGE('',*,*,#8587,.T.);
#12585=ORIENTED_EDGE('',*,*,#8583,.T.);
#12586=ORIENTED_EDGE('',*,*,#8588,.F.);
#12587=ORIENTED_EDGE('',*,*,#8589,.F.);
#12588=ORIENTED_EDGE('',*,*,#8590,.T.);
#12589=ORIENTED_EDGE('',*,*,#8586,.T.);
#12590=ORIENTED_EDGE('',*,*,#8591,.F.);
#12591=ORIENTED_EDGE('',*,*,#8592,.F.);
#12592=ORIENTED_EDGE('',*,*,#8593,.T.);
#12593=ORIENTED_EDGE('',*,*,#8589,.T.);
#12594=ORIENTED_EDGE('',*,*,#8594,.F.);
#12595=ORIENTED_EDGE('',*,*,#8595,.F.);
#12596=ORIENTED_EDGE('',*,*,#8596,.T.);
#12597=ORIENTED_EDGE('',*,*,#8592,.T.);
#12598=ORIENTED_EDGE('',*,*,#8597,.F.);
#12599=ORIENTED_EDGE('',*,*,#8598,.F.);
#12600=ORIENTED_EDGE('',*,*,#8599,.T.);
#12601=ORIENTED_EDGE('',*,*,#8595,.T.);
#12602=ORIENTED_EDGE('',*,*,#8600,.F.);
#12603=ORIENTED_EDGE('',*,*,#8601,.F.);
#12604=ORIENTED_EDGE('',*,*,#8602,.T.);
#12605=ORIENTED_EDGE('',*,*,#8598,.T.);
#12606=ORIENTED_EDGE('',*,*,#8603,.F.);
#12607=ORIENTED_EDGE('',*,*,#8604,.F.);
#12608=ORIENTED_EDGE('',*,*,#8605,.T.);
#12609=ORIENTED_EDGE('',*,*,#8601,.T.);
#12610=ORIENTED_EDGE('',*,*,#8606,.F.);
#12611=ORIENTED_EDGE('',*,*,#8607,.F.);
#12612=ORIENTED_EDGE('',*,*,#8608,.T.);
#12613=ORIENTED_EDGE('',*,*,#8604,.T.);
#12614=ORIENTED_EDGE('',*,*,#8609,.F.);
#12615=ORIENTED_EDGE('',*,*,#8610,.F.);
#12616=ORIENTED_EDGE('',*,*,#8611,.T.);
#12617=ORIENTED_EDGE('',*,*,#8607,.T.);
#12618=ORIENTED_EDGE('',*,*,#8612,.F.);
#12619=ORIENTED_EDGE('',*,*,#8613,.F.);
#12620=ORIENTED_EDGE('',*,*,#8614,.T.);
#12621=ORIENTED_EDGE('',*,*,#8610,.T.);
#12622=ORIENTED_EDGE('',*,*,#8615,.F.);
#12623=ORIENTED_EDGE('',*,*,#8616,.F.);
#12624=ORIENTED_EDGE('',*,*,#8617,.T.);
#12625=ORIENTED_EDGE('',*,*,#8613,.T.);
#12626=ORIENTED_EDGE('',*,*,#8618,.F.);
#12627=ORIENTED_EDGE('',*,*,#8619,.F.);
#12628=ORIENTED_EDGE('',*,*,#8620,.T.);
#12629=ORIENTED_EDGE('',*,*,#8616,.T.);
#12630=ORIENTED_EDGE('',*,*,#8621,.F.);
#12631=ORIENTED_EDGE('',*,*,#8622,.F.);
#12632=ORIENTED_EDGE('',*,*,#8623,.T.);
#12633=ORIENTED_EDGE('',*,*,#8619,.T.);
#12634=ORIENTED_EDGE('',*,*,#8624,.F.);
#12635=ORIENTED_EDGE('',*,*,#8625,.F.);
#12636=ORIENTED_EDGE('',*,*,#8626,.T.);
#12637=ORIENTED_EDGE('',*,*,#8622,.T.);
#12638=ORIENTED_EDGE('',*,*,#8627,.F.);
#12639=ORIENTED_EDGE('',*,*,#8628,.F.);
#12640=ORIENTED_EDGE('',*,*,#8629,.T.);
#12641=ORIENTED_EDGE('',*,*,#8625,.T.);
#12642=ORIENTED_EDGE('',*,*,#8630,.F.);
#12643=ORIENTED_EDGE('',*,*,#8631,.F.);
#12644=ORIENTED_EDGE('',*,*,#8632,.T.);
#12645=ORIENTED_EDGE('',*,*,#8628,.T.);
#12646=ORIENTED_EDGE('',*,*,#8633,.F.);
#12647=ORIENTED_EDGE('',*,*,#8634,.F.);
#12648=ORIENTED_EDGE('',*,*,#8635,.T.);
#12649=ORIENTED_EDGE('',*,*,#8631,.T.);
#12650=ORIENTED_EDGE('',*,*,#8636,.F.);
#12651=ORIENTED_EDGE('',*,*,#8637,.F.);
#12652=ORIENTED_EDGE('',*,*,#8638,.T.);
#12653=ORIENTED_EDGE('',*,*,#8634,.T.);
#12654=ORIENTED_EDGE('',*,*,#8639,.F.);
#12655=ORIENTED_EDGE('',*,*,#8640,.F.);
#12656=ORIENTED_EDGE('',*,*,#8641,.T.);
#12657=ORIENTED_EDGE('',*,*,#8637,.T.);
#12658=ORIENTED_EDGE('',*,*,#8642,.F.);
#12659=ORIENTED_EDGE('',*,*,#8643,.F.);
#12660=ORIENTED_EDGE('',*,*,#8644,.T.);
#12661=ORIENTED_EDGE('',*,*,#8640,.T.);
#12662=ORIENTED_EDGE('',*,*,#8645,.F.);
#12663=ORIENTED_EDGE('',*,*,#8646,.F.);
#12664=ORIENTED_EDGE('',*,*,#8647,.T.);
#12665=ORIENTED_EDGE('',*,*,#8643,.T.);
#12666=ORIENTED_EDGE('',*,*,#8648,.F.);
#12667=ORIENTED_EDGE('',*,*,#8649,.F.);
#12668=ORIENTED_EDGE('',*,*,#8650,.T.);
#12669=ORIENTED_EDGE('',*,*,#8646,.T.);
#12670=ORIENTED_EDGE('',*,*,#8651,.F.);
#12671=ORIENTED_EDGE('',*,*,#8652,.F.);
#12672=ORIENTED_EDGE('',*,*,#8536,.F.);
#12673=ORIENTED_EDGE('',*,*,#8653,.F.);
#12674=ORIENTED_EDGE('',*,*,#8654,.F.);
#12675=ORIENTED_EDGE('',*,*,#8655,.F.);
#12676=ORIENTED_EDGE('',*,*,#8656,.T.);
#12677=ORIENTED_EDGE('',*,*,#8657,.F.);
#12678=ORIENTED_EDGE('',*,*,#8656,.F.);
#12679=ORIENTED_EDGE('',*,*,#8653,.T.);
#12680=ORIENTED_EDGE('',*,*,#8535,.F.);
#12681=ORIENTED_EDGE('',*,*,#8539,.F.);
#12682=ORIENTED_EDGE('',*,*,#8542,.F.);
#12683=ORIENTED_EDGE('',*,*,#8545,.F.);
#12684=ORIENTED_EDGE('',*,*,#8548,.F.);
#12685=ORIENTED_EDGE('',*,*,#8551,.F.);
#12686=ORIENTED_EDGE('',*,*,#8554,.F.);
#12687=ORIENTED_EDGE('',*,*,#8557,.F.);
#12688=ORIENTED_EDGE('',*,*,#8560,.F.);
#12689=ORIENTED_EDGE('',*,*,#8563,.F.);
#12690=ORIENTED_EDGE('',*,*,#8566,.F.);
#12691=ORIENTED_EDGE('',*,*,#8569,.F.);
#12692=ORIENTED_EDGE('',*,*,#8572,.F.);
#12693=ORIENTED_EDGE('',*,*,#8575,.F.);
#12694=ORIENTED_EDGE('',*,*,#8578,.F.);
#12695=ORIENTED_EDGE('',*,*,#8581,.F.);
#12696=ORIENTED_EDGE('',*,*,#8584,.F.);
#12697=ORIENTED_EDGE('',*,*,#8587,.F.);
#12698=ORIENTED_EDGE('',*,*,#8590,.F.);
#12699=ORIENTED_EDGE('',*,*,#8593,.F.);
#12700=ORIENTED_EDGE('',*,*,#8596,.F.);
#12701=ORIENTED_EDGE('',*,*,#8599,.F.);
#12702=ORIENTED_EDGE('',*,*,#8602,.F.);
#12703=ORIENTED_EDGE('',*,*,#8605,.F.);
#12704=ORIENTED_EDGE('',*,*,#8608,.F.);
#12705=ORIENTED_EDGE('',*,*,#8611,.F.);
#12706=ORIENTED_EDGE('',*,*,#8614,.F.);
#12707=ORIENTED_EDGE('',*,*,#8617,.F.);
#12708=ORIENTED_EDGE('',*,*,#8620,.F.);
#12709=ORIENTED_EDGE('',*,*,#8623,.F.);
#12710=ORIENTED_EDGE('',*,*,#8626,.F.);
#12711=ORIENTED_EDGE('',*,*,#8629,.F.);
#12712=ORIENTED_EDGE('',*,*,#8632,.F.);
#12713=ORIENTED_EDGE('',*,*,#8635,.F.);
#12714=ORIENTED_EDGE('',*,*,#8638,.F.);
#12715=ORIENTED_EDGE('',*,*,#8641,.F.);
#12716=ORIENTED_EDGE('',*,*,#8644,.F.);
#12717=ORIENTED_EDGE('',*,*,#8647,.F.);
#12718=ORIENTED_EDGE('',*,*,#8650,.F.);
#12719=ORIENTED_EDGE('',*,*,#8658,.F.);
#12720=ORIENTED_EDGE('',*,*,#8659,.F.);
#12721=ORIENTED_EDGE('',*,*,#8417,.F.);
#12722=ORIENTED_EDGE('',*,*,#8421,.F.);
#12723=ORIENTED_EDGE('',*,*,#8424,.F.);
#12724=ORIENTED_EDGE('',*,*,#8427,.F.);
#12725=ORIENTED_EDGE('',*,*,#8430,.F.);
#12726=ORIENTED_EDGE('',*,*,#8433,.F.);
#12727=ORIENTED_EDGE('',*,*,#8436,.F.);
#12728=ORIENTED_EDGE('',*,*,#8439,.F.);
#12729=ORIENTED_EDGE('',*,*,#8442,.F.);
#12730=ORIENTED_EDGE('',*,*,#8445,.F.);
#12731=ORIENTED_EDGE('',*,*,#8448,.F.);
#12732=ORIENTED_EDGE('',*,*,#8451,.F.);
#12733=ORIENTED_EDGE('',*,*,#8454,.F.);
#12734=ORIENTED_EDGE('',*,*,#8457,.F.);
#12735=ORIENTED_EDGE('',*,*,#8460,.F.);
#12736=ORIENTED_EDGE('',*,*,#8463,.F.);
#12737=ORIENTED_EDGE('',*,*,#8466,.F.);
#12738=ORIENTED_EDGE('',*,*,#8469,.F.);
#12739=ORIENTED_EDGE('',*,*,#8472,.F.);
#12740=ORIENTED_EDGE('',*,*,#8475,.F.);
#12741=ORIENTED_EDGE('',*,*,#8478,.F.);
#12742=ORIENTED_EDGE('',*,*,#8481,.F.);
#12743=ORIENTED_EDGE('',*,*,#8484,.F.);
#12744=ORIENTED_EDGE('',*,*,#8487,.F.);
#12745=ORIENTED_EDGE('',*,*,#8490,.F.);
#12746=ORIENTED_EDGE('',*,*,#8493,.F.);
#12747=ORIENTED_EDGE('',*,*,#8496,.F.);
#12748=ORIENTED_EDGE('',*,*,#8499,.F.);
#12749=ORIENTED_EDGE('',*,*,#8502,.F.);
#12750=ORIENTED_EDGE('',*,*,#8505,.F.);
#12751=ORIENTED_EDGE('',*,*,#8508,.F.);
#12752=ORIENTED_EDGE('',*,*,#8511,.F.);
#12753=ORIENTED_EDGE('',*,*,#8514,.F.);
#12754=ORIENTED_EDGE('',*,*,#8517,.F.);
#12755=ORIENTED_EDGE('',*,*,#8520,.F.);
#12756=ORIENTED_EDGE('',*,*,#8523,.F.);
#12757=ORIENTED_EDGE('',*,*,#8526,.F.);
#12758=ORIENTED_EDGE('',*,*,#8529,.F.);
#12759=ORIENTED_EDGE('',*,*,#8532,.F.);
#12760=ORIENTED_EDGE('',*,*,#8660,.F.);
#12761=ORIENTED_EDGE('',*,*,#8649,.T.);
#12762=ORIENTED_EDGE('',*,*,#8661,.F.);
#12763=ORIENTED_EDGE('',*,*,#8662,.F.);
#12764=ORIENTED_EDGE('',*,*,#8658,.T.);
#12765=ORIENTED_EDGE('',*,*,#8652,.T.);
#12766=ORIENTED_EDGE('',*,*,#8655,.T.);
#12767=ORIENTED_EDGE('',*,*,#8663,.F.);
#12768=ORIENTED_EDGE('',*,*,#8533,.F.);
#12769=ORIENTED_EDGE('',*,*,#8530,.F.);
#12770=ORIENTED_EDGE('',*,*,#8527,.F.);
#12771=ORIENTED_EDGE('',*,*,#8524,.F.);
#12772=ORIENTED_EDGE('',*,*,#8521,.F.);
#12773=ORIENTED_EDGE('',*,*,#8518,.F.);
#12774=ORIENTED_EDGE('',*,*,#8515,.F.);
#12775=ORIENTED_EDGE('',*,*,#8512,.F.);
#12776=ORIENTED_EDGE('',*,*,#8509,.F.);
#12777=ORIENTED_EDGE('',*,*,#8506,.F.);
#12778=ORIENTED_EDGE('',*,*,#8503,.F.);
#12779=ORIENTED_EDGE('',*,*,#8500,.F.);
#12780=ORIENTED_EDGE('',*,*,#8497,.F.);
#12781=ORIENTED_EDGE('',*,*,#8494,.F.);
#12782=ORIENTED_EDGE('',*,*,#8491,.F.);
#12783=ORIENTED_EDGE('',*,*,#8488,.F.);
#12784=ORIENTED_EDGE('',*,*,#8485,.F.);
#12785=ORIENTED_EDGE('',*,*,#8482,.F.);
#12786=ORIENTED_EDGE('',*,*,#8479,.F.);
#12787=ORIENTED_EDGE('',*,*,#8476,.F.);
#12788=ORIENTED_EDGE('',*,*,#8473,.F.);
#12789=ORIENTED_EDGE('',*,*,#8470,.F.);
#12790=ORIENTED_EDGE('',*,*,#8467,.F.);
#12791=ORIENTED_EDGE('',*,*,#8464,.F.);
#12792=ORIENTED_EDGE('',*,*,#8461,.F.);
#12793=ORIENTED_EDGE('',*,*,#8458,.F.);
#12794=ORIENTED_EDGE('',*,*,#8455,.F.);
#12795=ORIENTED_EDGE('',*,*,#8452,.F.);
#12796=ORIENTED_EDGE('',*,*,#8449,.F.);
#12797=ORIENTED_EDGE('',*,*,#8446,.F.);
#12798=ORIENTED_EDGE('',*,*,#8443,.F.);
#12799=ORIENTED_EDGE('',*,*,#8440,.F.);
#12800=ORIENTED_EDGE('',*,*,#8437,.F.);
#12801=ORIENTED_EDGE('',*,*,#8434,.F.);
#12802=ORIENTED_EDGE('',*,*,#8431,.F.);
#12803=ORIENTED_EDGE('',*,*,#8428,.F.);
#12804=ORIENTED_EDGE('',*,*,#8425,.F.);
#12805=ORIENTED_EDGE('',*,*,#8422,.F.);
#12806=ORIENTED_EDGE('',*,*,#8419,.F.);
#12807=ORIENTED_EDGE('',*,*,#8664,.F.);
#12808=ORIENTED_EDGE('',*,*,#8661,.T.);
#12809=ORIENTED_EDGE('',*,*,#8651,.T.);
#12810=ORIENTED_EDGE('',*,*,#8648,.T.);
#12811=ORIENTED_EDGE('',*,*,#8645,.T.);
#12812=ORIENTED_EDGE('',*,*,#8642,.T.);
#12813=ORIENTED_EDGE('',*,*,#8639,.T.);
#12814=ORIENTED_EDGE('',*,*,#8636,.T.);
#12815=ORIENTED_EDGE('',*,*,#8633,.T.);
#12816=ORIENTED_EDGE('',*,*,#8630,.T.);
#12817=ORIENTED_EDGE('',*,*,#8627,.T.);
#12818=ORIENTED_EDGE('',*,*,#8624,.T.);
#12819=ORIENTED_EDGE('',*,*,#8621,.T.);
#12820=ORIENTED_EDGE('',*,*,#8618,.T.);
#12821=ORIENTED_EDGE('',*,*,#8615,.T.);
#12822=ORIENTED_EDGE('',*,*,#8612,.T.);
#12823=ORIENTED_EDGE('',*,*,#8609,.T.);
#12824=ORIENTED_EDGE('',*,*,#8606,.T.);
#12825=ORIENTED_EDGE('',*,*,#8603,.T.);
#12826=ORIENTED_EDGE('',*,*,#8600,.T.);
#12827=ORIENTED_EDGE('',*,*,#8597,.T.);
#12828=ORIENTED_EDGE('',*,*,#8594,.T.);
#12829=ORIENTED_EDGE('',*,*,#8591,.T.);
#12830=ORIENTED_EDGE('',*,*,#8588,.T.);
#12831=ORIENTED_EDGE('',*,*,#8585,.T.);
#12832=ORIENTED_EDGE('',*,*,#8582,.T.);
#12833=ORIENTED_EDGE('',*,*,#8579,.T.);
#12834=ORIENTED_EDGE('',*,*,#8576,.T.);
#12835=ORIENTED_EDGE('',*,*,#8573,.T.);
#12836=ORIENTED_EDGE('',*,*,#8570,.T.);
#12837=ORIENTED_EDGE('',*,*,#8567,.T.);
#12838=ORIENTED_EDGE('',*,*,#8564,.T.);
#12839=ORIENTED_EDGE('',*,*,#8561,.T.);
#12840=ORIENTED_EDGE('',*,*,#8558,.T.);
#12841=ORIENTED_EDGE('',*,*,#8555,.T.);
#12842=ORIENTED_EDGE('',*,*,#8552,.T.);
#12843=ORIENTED_EDGE('',*,*,#8549,.T.);
#12844=ORIENTED_EDGE('',*,*,#8546,.T.);
#12845=ORIENTED_EDGE('',*,*,#8543,.T.);
#12846=ORIENTED_EDGE('',*,*,#8540,.T.);
#12847=ORIENTED_EDGE('',*,*,#8537,.T.);
#12848=ORIENTED_EDGE('',*,*,#8531,.T.);
#12849=ORIENTED_EDGE('',*,*,#8663,.T.);
#12850=ORIENTED_EDGE('',*,*,#8654,.T.);
#12851=ORIENTED_EDGE('',*,*,#8660,.T.);
#12852=ORIENTED_EDGE('',*,*,#8665,.F.);
#12853=ORIENTED_EDGE('',*,*,#8666,.T.);
#12854=ORIENTED_EDGE('',*,*,#8667,.T.);
#12855=ORIENTED_EDGE('',*,*,#8668,.F.);
#12856=ORIENTED_EDGE('',*,*,#8669,.F.);
#12857=ORIENTED_EDGE('',*,*,#8670,.T.);
#12858=ORIENTED_EDGE('',*,*,#8671,.T.);
#12859=ORIENTED_EDGE('',*,*,#8666,.F.);
#12860=ORIENTED_EDGE('',*,*,#8672,.F.);
#12861=ORIENTED_EDGE('',*,*,#8673,.T.);
#12862=ORIENTED_EDGE('',*,*,#8674,.T.);
#12863=ORIENTED_EDGE('',*,*,#8670,.F.);
#12864=ORIENTED_EDGE('',*,*,#8675,.F.);
#12865=ORIENTED_EDGE('',*,*,#8676,.T.);
#12866=ORIENTED_EDGE('',*,*,#8677,.T.);
#12867=ORIENTED_EDGE('',*,*,#8673,.F.);
#12868=ORIENTED_EDGE('',*,*,#8678,.F.);
#12869=ORIENTED_EDGE('',*,*,#8679,.T.);
#12870=ORIENTED_EDGE('',*,*,#8680,.T.);
#12871=ORIENTED_EDGE('',*,*,#8676,.F.);
#12872=ORIENTED_EDGE('',*,*,#8681,.F.);
#12873=ORIENTED_EDGE('',*,*,#8668,.T.);
#12874=ORIENTED_EDGE('',*,*,#8682,.T.);
#12875=ORIENTED_EDGE('',*,*,#8679,.F.);
#12876=ORIENTED_EDGE('',*,*,#8682,.F.);
#12877=ORIENTED_EDGE('',*,*,#8667,.F.);
#12878=ORIENTED_EDGE('',*,*,#8671,.F.);
#12879=ORIENTED_EDGE('',*,*,#8674,.F.);
#12880=ORIENTED_EDGE('',*,*,#8677,.F.);
#12881=ORIENTED_EDGE('',*,*,#8680,.F.);
#12882=ORIENTED_EDGE('',*,*,#8683,.T.);
#12883=ORIENTED_EDGE('',*,*,#8659,.T.);
#12884=ORIENTED_EDGE('',*,*,#8662,.T.);
#12885=ORIENTED_EDGE('',*,*,#8664,.T.);
#12886=ORIENTED_EDGE('',*,*,#8418,.F.);
#12887=ORIENTED_EDGE('',*,*,#8683,.F.);
#12888=ORIENTED_EDGE('',*,*,#8684,.T.);
#12889=ORIENTED_EDGE('',*,*,#8685,.T.);
#12890=ORIENTED_EDGE('',*,*,#8684,.F.);
#12891=ORIENTED_EDGE('',*,*,#8685,.F.);
#12892=ORIENTED_EDGE('',*,*,#8665,.T.);
#12893=ORIENTED_EDGE('',*,*,#8681,.T.);
#12894=ORIENTED_EDGE('',*,*,#8678,.T.);
#12895=ORIENTED_EDGE('',*,*,#8675,.T.);
#12896=ORIENTED_EDGE('',*,*,#8672,.T.);
#12897=ORIENTED_EDGE('',*,*,#8669,.T.);
#12898=ORIENTED_EDGE('',*,*,#8657,.T.);
#12899=ORIENTED_EDGE('',*,*,#8686,.F.);
#12900=ORIENTED_EDGE('',*,*,#8687,.T.);
#12901=ORIENTED_EDGE('',*,*,#8688,.T.);
#12902=ORIENTED_EDGE('',*,*,#8687,.F.);
#12903=ORIENTED_EDGE('',*,*,#8689,.F.);
#12904=ORIENTED_EDGE('',*,*,#8690,.T.);
#12905=ORIENTED_EDGE('',*,*,#8691,.T.);
#12906=ORIENTED_EDGE('',*,*,#8690,.F.);
#12907=ORIENTED_EDGE('',*,*,#8689,.T.);
#12908=ORIENTED_EDGE('',*,*,#8686,.T.);
#12909=ORIENTED_EDGE('',*,*,#8691,.F.);
#12910=ORIENTED_EDGE('',*,*,#8688,.F.);
#12911=ORIENTED_EDGE('',*,*,#8692,.F.);
#12912=ORIENTED_EDGE('',*,*,#8693,.T.);
#12913=ORIENTED_EDGE('',*,*,#8694,.T.);
#12914=ORIENTED_EDGE('',*,*,#8695,.T.);
#12915=ORIENTED_EDGE('',*,*,#8696,.F.);
#12916=ORIENTED_EDGE('',*,*,#8697,.T.);
#12917=ORIENTED_EDGE('',*,*,#8692,.T.);
#12918=ORIENTED_EDGE('',*,*,#8698,.T.);
#12919=ORIENTED_EDGE('',*,*,#8699,.F.);
#12920=ORIENTED_EDGE('',*,*,#8700,.T.);
#12921=ORIENTED_EDGE('',*,*,#8696,.T.);
#12922=ORIENTED_EDGE('',*,*,#8701,.T.);
#12923=ORIENTED_EDGE('',*,*,#8702,.F.);
#12924=ORIENTED_EDGE('',*,*,#8703,.T.);
#12925=ORIENTED_EDGE('',*,*,#8699,.T.);
#12926=ORIENTED_EDGE('',*,*,#8704,.T.);
#12927=ORIENTED_EDGE('',*,*,#8705,.F.);
#12928=ORIENTED_EDGE('',*,*,#8706,.T.);
#12929=ORIENTED_EDGE('',*,*,#8702,.T.);
#12930=ORIENTED_EDGE('',*,*,#8707,.T.);
#12931=ORIENTED_EDGE('',*,*,#8708,.F.);
#12932=ORIENTED_EDGE('',*,*,#8709,.T.);
#12933=ORIENTED_EDGE('',*,*,#8705,.T.);
#12934=ORIENTED_EDGE('',*,*,#8710,.T.);
#12935=ORIENTED_EDGE('',*,*,#8711,.F.);
#12936=ORIENTED_EDGE('',*,*,#8712,.T.);
#12937=ORIENTED_EDGE('',*,*,#8708,.T.);
#12938=ORIENTED_EDGE('',*,*,#8713,.T.);
#12939=ORIENTED_EDGE('',*,*,#8714,.F.);
#12940=ORIENTED_EDGE('',*,*,#8715,.T.);
#12941=ORIENTED_EDGE('',*,*,#8711,.T.);
#12942=ORIENTED_EDGE('',*,*,#8716,.T.);
#12943=ORIENTED_EDGE('',*,*,#8717,.F.);
#12944=ORIENTED_EDGE('',*,*,#8718,.T.);
#12945=ORIENTED_EDGE('',*,*,#8714,.T.);
#12946=ORIENTED_EDGE('',*,*,#8719,.T.);
#12947=ORIENTED_EDGE('',*,*,#8720,.F.);
#12948=ORIENTED_EDGE('',*,*,#8721,.T.);
#12949=ORIENTED_EDGE('',*,*,#8717,.T.);
#12950=ORIENTED_EDGE('',*,*,#8722,.T.);
#12951=ORIENTED_EDGE('',*,*,#8723,.F.);
#12952=ORIENTED_EDGE('',*,*,#8724,.T.);
#12953=ORIENTED_EDGE('',*,*,#8720,.T.);
#12954=ORIENTED_EDGE('',*,*,#8725,.T.);
#12955=ORIENTED_EDGE('',*,*,#8726,.F.);
#12956=ORIENTED_EDGE('',*,*,#8727,.T.);
#12957=ORIENTED_EDGE('',*,*,#8723,.T.);
#12958=ORIENTED_EDGE('',*,*,#8728,.T.);
#12959=ORIENTED_EDGE('',*,*,#8729,.F.);
#12960=ORIENTED_EDGE('',*,*,#8730,.T.);
#12961=ORIENTED_EDGE('',*,*,#8726,.T.);
#12962=ORIENTED_EDGE('',*,*,#8731,.T.);
#12963=ORIENTED_EDGE('',*,*,#8732,.F.);
#12964=ORIENTED_EDGE('',*,*,#8733,.T.);
#12965=ORIENTED_EDGE('',*,*,#8729,.T.);
#12966=ORIENTED_EDGE('',*,*,#8734,.T.);
#12967=ORIENTED_EDGE('',*,*,#8735,.F.);
#12968=ORIENTED_EDGE('',*,*,#8736,.T.);
#12969=ORIENTED_EDGE('',*,*,#8732,.T.);
#12970=ORIENTED_EDGE('',*,*,#8737,.T.);
#12971=ORIENTED_EDGE('',*,*,#8738,.F.);
#12972=ORIENTED_EDGE('',*,*,#8739,.T.);
#12973=ORIENTED_EDGE('',*,*,#8735,.T.);
#12974=ORIENTED_EDGE('',*,*,#8740,.T.);
#12975=ORIENTED_EDGE('',*,*,#8741,.F.);
#12976=ORIENTED_EDGE('',*,*,#8742,.T.);
#12977=ORIENTED_EDGE('',*,*,#8738,.T.);
#12978=ORIENTED_EDGE('',*,*,#8743,.T.);
#12979=ORIENTED_EDGE('',*,*,#8744,.F.);
#12980=ORIENTED_EDGE('',*,*,#8745,.T.);
#12981=ORIENTED_EDGE('',*,*,#8741,.T.);
#12982=ORIENTED_EDGE('',*,*,#8746,.T.);
#12983=ORIENTED_EDGE('',*,*,#8747,.F.);
#12984=ORIENTED_EDGE('',*,*,#8748,.T.);
#12985=ORIENTED_EDGE('',*,*,#8744,.T.);
#12986=ORIENTED_EDGE('',*,*,#8749,.T.);
#12987=ORIENTED_EDGE('',*,*,#8750,.F.);
#12988=ORIENTED_EDGE('',*,*,#8751,.T.);
#12989=ORIENTED_EDGE('',*,*,#8747,.T.);
#12990=ORIENTED_EDGE('',*,*,#8752,.T.);
#12991=ORIENTED_EDGE('',*,*,#8753,.F.);
#12992=ORIENTED_EDGE('',*,*,#8754,.T.);
#12993=ORIENTED_EDGE('',*,*,#8750,.T.);
#12994=ORIENTED_EDGE('',*,*,#8755,.T.);
#12995=ORIENTED_EDGE('',*,*,#8756,.F.);
#12996=ORIENTED_EDGE('',*,*,#8757,.T.);
#12997=ORIENTED_EDGE('',*,*,#8753,.T.);
#12998=ORIENTED_EDGE('',*,*,#8758,.T.);
#12999=ORIENTED_EDGE('',*,*,#8759,.F.);
#13000=ORIENTED_EDGE('',*,*,#8760,.T.);
#13001=ORIENTED_EDGE('',*,*,#8756,.T.);
#13002=ORIENTED_EDGE('',*,*,#8761,.T.);
#13003=ORIENTED_EDGE('',*,*,#8762,.F.);
#13004=ORIENTED_EDGE('',*,*,#8763,.T.);
#13005=ORIENTED_EDGE('',*,*,#8759,.T.);
#13006=ORIENTED_EDGE('',*,*,#8764,.T.);
#13007=ORIENTED_EDGE('',*,*,#8765,.F.);
#13008=ORIENTED_EDGE('',*,*,#8766,.T.);
#13009=ORIENTED_EDGE('',*,*,#8762,.T.);
#13010=ORIENTED_EDGE('',*,*,#8767,.T.);
#13011=ORIENTED_EDGE('',*,*,#8768,.F.);
#13012=ORIENTED_EDGE('',*,*,#8769,.T.);
#13013=ORIENTED_EDGE('',*,*,#8765,.T.);
#13014=ORIENTED_EDGE('',*,*,#8770,.T.);
#13015=ORIENTED_EDGE('',*,*,#8771,.F.);
#13016=ORIENTED_EDGE('',*,*,#8772,.T.);
#13017=ORIENTED_EDGE('',*,*,#8768,.T.);
#13018=ORIENTED_EDGE('',*,*,#8773,.T.);
#13019=ORIENTED_EDGE('',*,*,#8774,.F.);
#13020=ORIENTED_EDGE('',*,*,#8775,.T.);
#13021=ORIENTED_EDGE('',*,*,#8771,.T.);
#13022=ORIENTED_EDGE('',*,*,#8776,.T.);
#13023=ORIENTED_EDGE('',*,*,#8777,.F.);
#13024=ORIENTED_EDGE('',*,*,#8778,.T.);
#13025=ORIENTED_EDGE('',*,*,#8774,.T.);
#13026=ORIENTED_EDGE('',*,*,#8779,.T.);
#13027=ORIENTED_EDGE('',*,*,#8780,.F.);
#13028=ORIENTED_EDGE('',*,*,#8781,.T.);
#13029=ORIENTED_EDGE('',*,*,#8777,.T.);
#13030=ORIENTED_EDGE('',*,*,#8782,.T.);
#13031=ORIENTED_EDGE('',*,*,#8783,.F.);
#13032=ORIENTED_EDGE('',*,*,#8784,.T.);
#13033=ORIENTED_EDGE('',*,*,#8780,.T.);
#13034=ORIENTED_EDGE('',*,*,#8785,.T.);
#13035=ORIENTED_EDGE('',*,*,#8786,.F.);
#13036=ORIENTED_EDGE('',*,*,#8787,.T.);
#13037=ORIENTED_EDGE('',*,*,#8788,.T.);
#13038=ORIENTED_EDGE('',*,*,#8783,.T.);
#13039=ORIENTED_EDGE('',*,*,#8789,.T.);
#13040=ORIENTED_EDGE('',*,*,#8790,.F.);
#13041=ORIENTED_EDGE('',*,*,#8791,.T.);
#13042=ORIENTED_EDGE('',*,*,#8792,.T.);
#13043=ORIENTED_EDGE('',*,*,#8793,.F.);
#13044=ORIENTED_EDGE('',*,*,#8794,.T.);
#13045=ORIENTED_EDGE('',*,*,#8790,.T.);
#13046=ORIENTED_EDGE('',*,*,#8795,.T.);
#13047=ORIENTED_EDGE('',*,*,#8796,.F.);
#13048=ORIENTED_EDGE('',*,*,#8797,.F.);
#13049=ORIENTED_EDGE('',*,*,#8798,.T.);
#13050=ORIENTED_EDGE('',*,*,#8793,.T.);
#13051=ORIENTED_EDGE('',*,*,#8799,.F.);
#13052=ORIENTED_EDGE('',*,*,#8800,.F.);
#13053=ORIENTED_EDGE('',*,*,#8801,.T.);
#13054=ORIENTED_EDGE('',*,*,#8797,.T.);
#13055=ORIENTED_EDGE('',*,*,#8802,.F.);
#13056=ORIENTED_EDGE('',*,*,#8803,.F.);
#13057=ORIENTED_EDGE('',*,*,#8804,.T.);
#13058=ORIENTED_EDGE('',*,*,#8800,.T.);
#13059=ORIENTED_EDGE('',*,*,#8805,.F.);
#13060=ORIENTED_EDGE('',*,*,#8806,.F.);
#13061=ORIENTED_EDGE('',*,*,#8807,.T.);
#13062=ORIENTED_EDGE('',*,*,#8803,.T.);
#13063=ORIENTED_EDGE('',*,*,#8808,.F.);
#13064=ORIENTED_EDGE('',*,*,#8809,.F.);
#13065=ORIENTED_EDGE('',*,*,#8810,.T.);
#13066=ORIENTED_EDGE('',*,*,#8806,.T.);
#13067=ORIENTED_EDGE('',*,*,#8811,.F.);
#13068=ORIENTED_EDGE('',*,*,#8812,.F.);
#13069=ORIENTED_EDGE('',*,*,#8813,.T.);
#13070=ORIENTED_EDGE('',*,*,#8809,.T.);
#13071=ORIENTED_EDGE('',*,*,#8814,.F.);
#13072=ORIENTED_EDGE('',*,*,#8815,.F.);
#13073=ORIENTED_EDGE('',*,*,#8816,.T.);
#13074=ORIENTED_EDGE('',*,*,#8812,.T.);
#13075=ORIENTED_EDGE('',*,*,#8817,.F.);
#13076=ORIENTED_EDGE('',*,*,#8818,.F.);
#13077=ORIENTED_EDGE('',*,*,#8819,.T.);
#13078=ORIENTED_EDGE('',*,*,#8815,.T.);
#13079=ORIENTED_EDGE('',*,*,#8820,.F.);
#13080=ORIENTED_EDGE('',*,*,#8821,.F.);
#13081=ORIENTED_EDGE('',*,*,#8822,.T.);
#13082=ORIENTED_EDGE('',*,*,#8818,.T.);
#13083=ORIENTED_EDGE('',*,*,#8823,.F.);
#13084=ORIENTED_EDGE('',*,*,#8824,.F.);
#13085=ORIENTED_EDGE('',*,*,#8825,.T.);
#13086=ORIENTED_EDGE('',*,*,#8821,.T.);
#13087=ORIENTED_EDGE('',*,*,#8826,.F.);
#13088=ORIENTED_EDGE('',*,*,#8827,.F.);
#13089=ORIENTED_EDGE('',*,*,#8828,.T.);
#13090=ORIENTED_EDGE('',*,*,#8824,.T.);
#13091=ORIENTED_EDGE('',*,*,#8829,.F.);
#13092=ORIENTED_EDGE('',*,*,#8830,.F.);
#13093=ORIENTED_EDGE('',*,*,#8831,.T.);
#13094=ORIENTED_EDGE('',*,*,#8827,.T.);
#13095=ORIENTED_EDGE('',*,*,#8832,.F.);
#13096=ORIENTED_EDGE('',*,*,#8833,.F.);
#13097=ORIENTED_EDGE('',*,*,#8834,.T.);
#13098=ORIENTED_EDGE('',*,*,#8830,.T.);
#13099=ORIENTED_EDGE('',*,*,#8835,.F.);
#13100=ORIENTED_EDGE('',*,*,#8836,.F.);
#13101=ORIENTED_EDGE('',*,*,#8837,.T.);
#13102=ORIENTED_EDGE('',*,*,#8833,.T.);
#13103=ORIENTED_EDGE('',*,*,#8838,.F.);
#13104=ORIENTED_EDGE('',*,*,#8839,.F.);
#13105=ORIENTED_EDGE('',*,*,#8840,.T.);
#13106=ORIENTED_EDGE('',*,*,#8836,.T.);
#13107=ORIENTED_EDGE('',*,*,#8841,.F.);
#13108=ORIENTED_EDGE('',*,*,#8842,.F.);
#13109=ORIENTED_EDGE('',*,*,#8843,.T.);
#13110=ORIENTED_EDGE('',*,*,#8839,.T.);
#13111=ORIENTED_EDGE('',*,*,#8844,.F.);
#13112=ORIENTED_EDGE('',*,*,#8845,.F.);
#13113=ORIENTED_EDGE('',*,*,#8846,.T.);
#13114=ORIENTED_EDGE('',*,*,#8842,.T.);
#13115=ORIENTED_EDGE('',*,*,#8847,.F.);
#13116=ORIENTED_EDGE('',*,*,#8848,.F.);
#13117=ORIENTED_EDGE('',*,*,#8849,.T.);
#13118=ORIENTED_EDGE('',*,*,#8845,.T.);
#13119=ORIENTED_EDGE('',*,*,#8850,.F.);
#13120=ORIENTED_EDGE('',*,*,#8851,.F.);
#13121=ORIENTED_EDGE('',*,*,#8852,.T.);
#13122=ORIENTED_EDGE('',*,*,#8848,.T.);
#13123=ORIENTED_EDGE('',*,*,#8853,.F.);
#13124=ORIENTED_EDGE('',*,*,#8854,.F.);
#13125=ORIENTED_EDGE('',*,*,#8855,.T.);
#13126=ORIENTED_EDGE('',*,*,#8851,.T.);
#13127=ORIENTED_EDGE('',*,*,#8856,.F.);
#13128=ORIENTED_EDGE('',*,*,#8857,.F.);
#13129=ORIENTED_EDGE('',*,*,#8858,.T.);
#13130=ORIENTED_EDGE('',*,*,#8854,.T.);
#13131=ORIENTED_EDGE('',*,*,#8859,.F.);
#13132=ORIENTED_EDGE('',*,*,#8860,.F.);
#13133=ORIENTED_EDGE('',*,*,#8861,.T.);
#13134=ORIENTED_EDGE('',*,*,#8857,.T.);
#13135=ORIENTED_EDGE('',*,*,#8862,.F.);
#13136=ORIENTED_EDGE('',*,*,#8863,.F.);
#13137=ORIENTED_EDGE('',*,*,#8864,.T.);
#13138=ORIENTED_EDGE('',*,*,#8860,.T.);
#13139=ORIENTED_EDGE('',*,*,#8865,.F.);
#13140=ORIENTED_EDGE('',*,*,#8866,.F.);
#13141=ORIENTED_EDGE('',*,*,#8867,.T.);
#13142=ORIENTED_EDGE('',*,*,#8863,.T.);
#13143=ORIENTED_EDGE('',*,*,#8868,.F.);
#13144=ORIENTED_EDGE('',*,*,#8869,.F.);
#13145=ORIENTED_EDGE('',*,*,#8870,.T.);
#13146=ORIENTED_EDGE('',*,*,#8866,.T.);
#13147=ORIENTED_EDGE('',*,*,#8871,.F.);
#13148=ORIENTED_EDGE('',*,*,#8872,.F.);
#13149=ORIENTED_EDGE('',*,*,#8873,.T.);
#13150=ORIENTED_EDGE('',*,*,#8869,.T.);
#13151=ORIENTED_EDGE('',*,*,#8874,.F.);
#13152=ORIENTED_EDGE('',*,*,#8875,.F.);
#13153=ORIENTED_EDGE('',*,*,#8876,.T.);
#13154=ORIENTED_EDGE('',*,*,#8872,.T.);
#13155=ORIENTED_EDGE('',*,*,#8877,.F.);
#13156=ORIENTED_EDGE('',*,*,#8878,.F.);
#13157=ORIENTED_EDGE('',*,*,#8879,.T.);
#13158=ORIENTED_EDGE('',*,*,#8875,.T.);
#13159=ORIENTED_EDGE('',*,*,#8880,.F.);
#13160=ORIENTED_EDGE('',*,*,#8881,.F.);
#13161=ORIENTED_EDGE('',*,*,#8882,.T.);
#13162=ORIENTED_EDGE('',*,*,#8878,.T.);
#13163=ORIENTED_EDGE('',*,*,#8883,.F.);
#13164=ORIENTED_EDGE('',*,*,#8884,.F.);
#13165=ORIENTED_EDGE('',*,*,#8885,.T.);
#13166=ORIENTED_EDGE('',*,*,#8881,.T.);
#13167=ORIENTED_EDGE('',*,*,#8886,.F.);
#13168=ORIENTED_EDGE('',*,*,#8887,.F.);
#13169=ORIENTED_EDGE('',*,*,#8888,.F.);
#13170=ORIENTED_EDGE('',*,*,#8889,.F.);
#13171=ORIENTED_EDGE('',*,*,#8795,.F.);
#13172=ORIENTED_EDGE('',*,*,#8890,.T.);
#13173=ORIENTED_EDGE('',*,*,#8891,.F.);
#13174=ORIENTED_EDGE('',*,*,#8890,.F.);
#13175=ORIENTED_EDGE('',*,*,#8792,.F.);
#13176=ORIENTED_EDGE('',*,*,#8892,.F.);
#13177=ORIENTED_EDGE('',*,*,#8887,.T.);
#13178=ORIENTED_EDGE('',*,*,#8893,.F.);
#13179=ORIENTED_EDGE('',*,*,#8787,.F.);
#13180=ORIENTED_EDGE('',*,*,#8893,.T.);
#13181=ORIENTED_EDGE('',*,*,#8892,.T.);
#13182=ORIENTED_EDGE('',*,*,#8791,.F.);
#13183=ORIENTED_EDGE('',*,*,#8794,.F.);
#13184=ORIENTED_EDGE('',*,*,#8798,.F.);
#13185=ORIENTED_EDGE('',*,*,#8801,.F.);
#13186=ORIENTED_EDGE('',*,*,#8804,.F.);
#13187=ORIENTED_EDGE('',*,*,#8807,.F.);
#13188=ORIENTED_EDGE('',*,*,#8810,.F.);
#13189=ORIENTED_EDGE('',*,*,#8813,.F.);
#13190=ORIENTED_EDGE('',*,*,#8816,.F.);
#13191=ORIENTED_EDGE('',*,*,#8819,.F.);
#13192=ORIENTED_EDGE('',*,*,#8822,.F.);
#13193=ORIENTED_EDGE('',*,*,#8825,.F.);
#13194=ORIENTED_EDGE('',*,*,#8828,.F.);
#13195=ORIENTED_EDGE('',*,*,#8831,.F.);
#13196=ORIENTED_EDGE('',*,*,#8834,.F.);
#13197=ORIENTED_EDGE('',*,*,#8837,.F.);
#13198=ORIENTED_EDGE('',*,*,#8840,.F.);
#13199=ORIENTED_EDGE('',*,*,#8843,.F.);
#13200=ORIENTED_EDGE('',*,*,#8846,.F.);
#13201=ORIENTED_EDGE('',*,*,#8849,.F.);
#13202=ORIENTED_EDGE('',*,*,#8852,.F.);
#13203=ORIENTED_EDGE('',*,*,#8855,.F.);
#13204=ORIENTED_EDGE('',*,*,#8858,.F.);
#13205=ORIENTED_EDGE('',*,*,#8861,.F.);
#13206=ORIENTED_EDGE('',*,*,#8864,.F.);
#13207=ORIENTED_EDGE('',*,*,#8867,.F.);
#13208=ORIENTED_EDGE('',*,*,#8870,.F.);
#13209=ORIENTED_EDGE('',*,*,#8873,.F.);
#13210=ORIENTED_EDGE('',*,*,#8876,.F.);
#13211=ORIENTED_EDGE('',*,*,#8879,.F.);
#13212=ORIENTED_EDGE('',*,*,#8882,.F.);
#13213=ORIENTED_EDGE('',*,*,#8885,.F.);
#13214=ORIENTED_EDGE('',*,*,#8894,.F.);
#13215=ORIENTED_EDGE('',*,*,#8895,.F.);
#13216=ORIENTED_EDGE('',*,*,#8693,.F.);
#13217=ORIENTED_EDGE('',*,*,#8697,.F.);
#13218=ORIENTED_EDGE('',*,*,#8700,.F.);
#13219=ORIENTED_EDGE('',*,*,#8703,.F.);
#13220=ORIENTED_EDGE('',*,*,#8706,.F.);
#13221=ORIENTED_EDGE('',*,*,#8709,.F.);
#13222=ORIENTED_EDGE('',*,*,#8712,.F.);
#13223=ORIENTED_EDGE('',*,*,#8715,.F.);
#13224=ORIENTED_EDGE('',*,*,#8718,.F.);
#13225=ORIENTED_EDGE('',*,*,#8721,.F.);
#13226=ORIENTED_EDGE('',*,*,#8724,.F.);
#13227=ORIENTED_EDGE('',*,*,#8727,.F.);
#13228=ORIENTED_EDGE('',*,*,#8730,.F.);
#13229=ORIENTED_EDGE('',*,*,#8733,.F.);
#13230=ORIENTED_EDGE('',*,*,#8736,.F.);
#13231=ORIENTED_EDGE('',*,*,#8739,.F.);
#13232=ORIENTED_EDGE('',*,*,#8742,.F.);
#13233=ORIENTED_EDGE('',*,*,#8745,.F.);
#13234=ORIENTED_EDGE('',*,*,#8748,.F.);
#13235=ORIENTED_EDGE('',*,*,#8751,.F.);
#13236=ORIENTED_EDGE('',*,*,#8754,.F.);
#13237=ORIENTED_EDGE('',*,*,#8757,.F.);
#13238=ORIENTED_EDGE('',*,*,#8760,.F.);
#13239=ORIENTED_EDGE('',*,*,#8763,.F.);
#13240=ORIENTED_EDGE('',*,*,#8766,.F.);
#13241=ORIENTED_EDGE('',*,*,#8769,.F.);
#13242=ORIENTED_EDGE('',*,*,#8772,.F.);
#13243=ORIENTED_EDGE('',*,*,#8775,.F.);
#13244=ORIENTED_EDGE('',*,*,#8778,.F.);
#13245=ORIENTED_EDGE('',*,*,#8781,.F.);
#13246=ORIENTED_EDGE('',*,*,#8784,.F.);
#13247=ORIENTED_EDGE('',*,*,#8788,.F.);
#13248=ORIENTED_EDGE('',*,*,#8884,.T.);
#13249=ORIENTED_EDGE('',*,*,#8896,.F.);
#13250=ORIENTED_EDGE('',*,*,#8897,.F.);
#13251=ORIENTED_EDGE('',*,*,#8894,.T.);
#13252=ORIENTED_EDGE('',*,*,#8889,.T.);
#13253=ORIENTED_EDGE('',*,*,#8898,.F.);
#13254=ORIENTED_EDGE('',*,*,#8789,.F.);
#13255=ORIENTED_EDGE('',*,*,#8785,.F.);
#13256=ORIENTED_EDGE('',*,*,#8782,.F.);
#13257=ORIENTED_EDGE('',*,*,#8779,.F.);
#13258=ORIENTED_EDGE('',*,*,#8776,.F.);
#13259=ORIENTED_EDGE('',*,*,#8773,.F.);
#13260=ORIENTED_EDGE('',*,*,#8770,.F.);
#13261=ORIENTED_EDGE('',*,*,#8767,.F.);
#13262=ORIENTED_EDGE('',*,*,#8764,.F.);
#13263=ORIENTED_EDGE('',*,*,#8761,.F.);
#13264=ORIENTED_EDGE('',*,*,#8758,.F.);
#13265=ORIENTED_EDGE('',*,*,#8755,.F.);
#13266=ORIENTED_EDGE('',*,*,#8752,.F.);
#13267=ORIENTED_EDGE('',*,*,#8749,.F.);
#13268=ORIENTED_EDGE('',*,*,#8746,.F.);
#13269=ORIENTED_EDGE('',*,*,#8743,.F.);
#13270=ORIENTED_EDGE('',*,*,#8740,.F.);
#13271=ORIENTED_EDGE('',*,*,#8737,.F.);
#13272=ORIENTED_EDGE('',*,*,#8734,.F.);
#13273=ORIENTED_EDGE('',*,*,#8731,.F.);
#13274=ORIENTED_EDGE('',*,*,#8728,.F.);
#13275=ORIENTED_EDGE('',*,*,#8725,.F.);
#13276=ORIENTED_EDGE('',*,*,#8722,.F.);
#13277=ORIENTED_EDGE('',*,*,#8719,.F.);
#13278=ORIENTED_EDGE('',*,*,#8716,.F.);
#13279=ORIENTED_EDGE('',*,*,#8713,.F.);
#13280=ORIENTED_EDGE('',*,*,#8710,.F.);
#13281=ORIENTED_EDGE('',*,*,#8707,.F.);
#13282=ORIENTED_EDGE('',*,*,#8704,.F.);
#13283=ORIENTED_EDGE('',*,*,#8701,.F.);
#13284=ORIENTED_EDGE('',*,*,#8698,.F.);
#13285=ORIENTED_EDGE('',*,*,#8695,.F.);
#13286=ORIENTED_EDGE('',*,*,#8899,.F.);
#13287=ORIENTED_EDGE('',*,*,#8896,.T.);
#13288=ORIENTED_EDGE('',*,*,#8886,.T.);
#13289=ORIENTED_EDGE('',*,*,#8883,.T.);
#13290=ORIENTED_EDGE('',*,*,#8880,.T.);
#13291=ORIENTED_EDGE('',*,*,#8877,.T.);
#13292=ORIENTED_EDGE('',*,*,#8874,.T.);
#13293=ORIENTED_EDGE('',*,*,#8871,.T.);
#13294=ORIENTED_EDGE('',*,*,#8868,.T.);
#13295=ORIENTED_EDGE('',*,*,#8865,.T.);
#13296=ORIENTED_EDGE('',*,*,#8862,.T.);
#13297=ORIENTED_EDGE('',*,*,#8859,.T.);
#13298=ORIENTED_EDGE('',*,*,#8856,.T.);
#13299=ORIENTED_EDGE('',*,*,#8853,.T.);
#13300=ORIENTED_EDGE('',*,*,#8850,.T.);
#13301=ORIENTED_EDGE('',*,*,#8847,.T.);
#13302=ORIENTED_EDGE('',*,*,#8844,.T.);
#13303=ORIENTED_EDGE('',*,*,#8841,.T.);
#13304=ORIENTED_EDGE('',*,*,#8838,.T.);
#13305=ORIENTED_EDGE('',*,*,#8835,.T.);
#13306=ORIENTED_EDGE('',*,*,#8832,.T.);
#13307=ORIENTED_EDGE('',*,*,#8829,.T.);
#13308=ORIENTED_EDGE('',*,*,#8826,.T.);
#13309=ORIENTED_EDGE('',*,*,#8823,.T.);
#13310=ORIENTED_EDGE('',*,*,#8820,.T.);
#13311=ORIENTED_EDGE('',*,*,#8817,.T.);
#13312=ORIENTED_EDGE('',*,*,#8814,.T.);
#13313=ORIENTED_EDGE('',*,*,#8811,.T.);
#13314=ORIENTED_EDGE('',*,*,#8808,.T.);
#13315=ORIENTED_EDGE('',*,*,#8805,.T.);
#13316=ORIENTED_EDGE('',*,*,#8802,.T.);
#13317=ORIENTED_EDGE('',*,*,#8799,.T.);
#13318=ORIENTED_EDGE('',*,*,#8796,.T.);
#13319=ORIENTED_EDGE('',*,*,#8786,.T.);
#13320=ORIENTED_EDGE('',*,*,#8898,.T.);
#13321=ORIENTED_EDGE('',*,*,#8888,.T.);
#13322=ORIENTED_EDGE('',*,*,#8900,.F.);
#13323=ORIENTED_EDGE('',*,*,#8901,.T.);
#13324=ORIENTED_EDGE('',*,*,#8902,.T.);
#13325=ORIENTED_EDGE('',*,*,#8903,.F.);
#13326=ORIENTED_EDGE('',*,*,#8904,.F.);
#13327=ORIENTED_EDGE('',*,*,#8905,.T.);
#13328=ORIENTED_EDGE('',*,*,#8906,.T.);
#13329=ORIENTED_EDGE('',*,*,#8901,.F.);
#13330=ORIENTED_EDGE('',*,*,#8907,.F.);
#13331=ORIENTED_EDGE('',*,*,#8908,.T.);
#13332=ORIENTED_EDGE('',*,*,#8909,.T.);
#13333=ORIENTED_EDGE('',*,*,#8905,.F.);
#13334=ORIENTED_EDGE('',*,*,#8910,.F.);
#13335=ORIENTED_EDGE('',*,*,#8911,.T.);
#13336=ORIENTED_EDGE('',*,*,#8912,.T.);
#13337=ORIENTED_EDGE('',*,*,#8908,.F.);
#13338=ORIENTED_EDGE('',*,*,#8913,.F.);
#13339=ORIENTED_EDGE('',*,*,#8914,.T.);
#13340=ORIENTED_EDGE('',*,*,#8915,.T.);
#13341=ORIENTED_EDGE('',*,*,#8911,.F.);
#13342=ORIENTED_EDGE('',*,*,#8916,.F.);
#13343=ORIENTED_EDGE('',*,*,#8903,.T.);
#13344=ORIENTED_EDGE('',*,*,#8917,.T.);
#13345=ORIENTED_EDGE('',*,*,#8914,.F.);
#13346=ORIENTED_EDGE('',*,*,#8917,.F.);
#13347=ORIENTED_EDGE('',*,*,#8902,.F.);
#13348=ORIENTED_EDGE('',*,*,#8906,.F.);
#13349=ORIENTED_EDGE('',*,*,#8909,.F.);
#13350=ORIENTED_EDGE('',*,*,#8912,.F.);
#13351=ORIENTED_EDGE('',*,*,#8915,.F.);
#13352=ORIENTED_EDGE('',*,*,#8918,.T.);
#13353=ORIENTED_EDGE('',*,*,#8895,.T.);
#13354=ORIENTED_EDGE('',*,*,#8897,.T.);
#13355=ORIENTED_EDGE('',*,*,#8899,.T.);
#13356=ORIENTED_EDGE('',*,*,#8694,.F.);
#13357=ORIENTED_EDGE('',*,*,#8918,.F.);
#13358=ORIENTED_EDGE('',*,*,#8919,.T.);
#13359=ORIENTED_EDGE('',*,*,#8920,.T.);
#13360=ORIENTED_EDGE('',*,*,#8919,.F.);
#13361=ORIENTED_EDGE('',*,*,#8920,.F.);
#13362=ORIENTED_EDGE('',*,*,#8900,.T.);
#13363=ORIENTED_EDGE('',*,*,#8916,.T.);
#13364=ORIENTED_EDGE('',*,*,#8913,.T.);
#13365=ORIENTED_EDGE('',*,*,#8910,.T.);
#13366=ORIENTED_EDGE('',*,*,#8907,.T.);
#13367=ORIENTED_EDGE('',*,*,#8904,.T.);
#13368=ORIENTED_EDGE('',*,*,#8891,.T.);
#13369=CYLINDRICAL_SURFACE('',#14866,2.5175);
#13370=CYLINDRICAL_SURFACE('',#14870,2.5175);
#13371=CYLINDRICAL_SURFACE('',#14871,2.5175);
#13372=CYLINDRICAL_SURFACE('',#14872,2.5175);
#13373=CYLINDRICAL_SURFACE('',#14873,2.5175);
#13374=CYLINDRICAL_SURFACE('',#14874,2.5175);
#13375=CYLINDRICAL_SURFACE('',#14875,2.5175);
#13376=CYLINDRICAL_SURFACE('',#14876,2.5175);
#13377=CYLINDRICAL_SURFACE('',#14877,2.5175);
#13378=CYLINDRICAL_SURFACE('',#14879,3.0735);
#13379=CYLINDRICAL_SURFACE('',#14881,3.0735);
#13380=CYLINDRICAL_SURFACE('',#14882,3.0735);
#13381=CYLINDRICAL_SURFACE('',#14883,3.0735);
#13382=CYLINDRICAL_SURFACE('',#14884,3.0735);
#13383=CYLINDRICAL_SURFACE('',#14885,3.0735);
#13384=CYLINDRICAL_SURFACE('',#14886,3.0735);
#13385=CYLINDRICAL_SURFACE('',#14887,3.0735);
#13386=CYLINDRICAL_SURFACE('',#14888,3.0735);
#13387=CYLINDRICAL_SURFACE('',#14890,2.5175);
#13388=CYLINDRICAL_SURFACE('',#14894,2.5175);
#13389=CYLINDRICAL_SURFACE('',#14895,2.5175);
#13390=CYLINDRICAL_SURFACE('',#14896,2.5175);
#13391=CYLINDRICAL_SURFACE('',#14897,2.5175);
#13392=CYLINDRICAL_SURFACE('',#14898,2.5175);
#13393=CYLINDRICAL_SURFACE('',#14899,2.5175);
#13394=CYLINDRICAL_SURFACE('',#14900,2.5175);
#13395=CYLINDRICAL_SURFACE('',#14901,2.5175);
#13396=CYLINDRICAL_SURFACE('',#14903,3.0735);
#13397=CYLINDRICAL_SURFACE('',#14905,3.0735);
#13398=CYLINDRICAL_SURFACE('',#14906,3.0735);
#13399=CYLINDRICAL_SURFACE('',#14907,3.0735);
#13400=CYLINDRICAL_SURFACE('',#14908,3.0735);
#13401=CYLINDRICAL_SURFACE('',#14909,3.0735);
#13402=CYLINDRICAL_SURFACE('',#14910,3.0735);
#13403=CYLINDRICAL_SURFACE('',#14911,3.0735);
#13404=CYLINDRICAL_SURFACE('',#14912,3.0735);
#13405=CYLINDRICAL_SURFACE('',#14914,2.5175);
#13406=CYLINDRICAL_SURFACE('',#14918,2.5175);
#13407=CYLINDRICAL_SURFACE('',#14919,2.5175);
#13408=CYLINDRICAL_SURFACE('',#14920,2.5175);
#13409=CYLINDRICAL_SURFACE('',#14921,2.5175);
#13410=CYLINDRICAL_SURFACE('',#14922,2.5175);
#13411=CYLINDRICAL_SURFACE('',#14923,2.5175);
#13412=CYLINDRICAL_SURFACE('',#14924,2.5175);
#13413=CYLINDRICAL_SURFACE('',#14925,2.5175);
#13414=CYLINDRICAL_SURFACE('',#14927,3.0735);
#13415=CYLINDRICAL_SURFACE('',#14929,3.0735);
#13416=CYLINDRICAL_SURFACE('',#14930,3.0735);
#13417=CYLINDRICAL_SURFACE('',#14931,3.0735);
#13418=CYLINDRICAL_SURFACE('',#14932,3.0735);
#13419=CYLINDRICAL_SURFACE('',#14933,3.0735);
#13420=CYLINDRICAL_SURFACE('',#14934,3.0735);
#13421=CYLINDRICAL_SURFACE('',#14935,3.0735);
#13422=CYLINDRICAL_SURFACE('',#14936,3.0735);
#13423=CYLINDRICAL_SURFACE('',#14938,2.5175);
#13424=CYLINDRICAL_SURFACE('',#14942,2.5175);
#13425=CYLINDRICAL_SURFACE('',#14943,2.5175);
#13426=CYLINDRICAL_SURFACE('',#14944,2.5175);
#13427=CYLINDRICAL_SURFACE('',#14945,2.5175);
#13428=CYLINDRICAL_SURFACE('',#14946,2.5175);
#13429=CYLINDRICAL_SURFACE('',#14947,2.5175);
#13430=CYLINDRICAL_SURFACE('',#14948,2.5175);
#13431=CYLINDRICAL_SURFACE('',#14949,2.5175);
#13432=CYLINDRICAL_SURFACE('',#14951,3.0735);
#13433=CYLINDRICAL_SURFACE('',#14953,3.0735);
#13434=CYLINDRICAL_SURFACE('',#14954,3.0735);
#13435=CYLINDRICAL_SURFACE('',#14955,3.0735);
#13436=CYLINDRICAL_SURFACE('',#14956,3.0735);
#13437=CYLINDRICAL_SURFACE('',#14957,3.0735);
#13438=CYLINDRICAL_SURFACE('',#14958,3.0735);
#13439=CYLINDRICAL_SURFACE('',#14959,3.0735);
#13440=CYLINDRICAL_SURFACE('',#14960,3.0735);
#13441=CYLINDRICAL_SURFACE('',#14962,2.5175);
#13442=CYLINDRICAL_SURFACE('',#14966,2.5175);
#13443=CYLINDRICAL_SURFACE('',#14967,2.5175);
#13444=CYLINDRICAL_SURFACE('',#14968,2.5175);
#13445=CYLINDRICAL_SURFACE('',#14969,2.5175);
#13446=CYLINDRICAL_SURFACE('',#14970,2.5175);
#13447=CYLINDRICAL_SURFACE('',#14971,2.5175);
#13448=CYLINDRICAL_SURFACE('',#14972,2.5175);
#13449=CYLINDRICAL_SURFACE('',#14973,2.5175);
#13450=CYLINDRICAL_SURFACE('',#14975,3.0735);
#13451=CYLINDRICAL_SURFACE('',#14977,3.0735);
#13452=CYLINDRICAL_SURFACE('',#14978,3.0735);
#13453=CYLINDRICAL_SURFACE('',#14979,3.0735);
#13454=CYLINDRICAL_SURFACE('',#14980,3.0735);
#13455=CYLINDRICAL_SURFACE('',#14981,3.0735);
#13456=CYLINDRICAL_SURFACE('',#14982,3.0735);
#13457=CYLINDRICAL_SURFACE('',#14983,3.0735);
#13458=CYLINDRICAL_SURFACE('',#14984,3.0735);
#13459=CYLINDRICAL_SURFACE('',#14986,2.5175);
#13460=CYLINDRICAL_SURFACE('',#14990,2.5175);
#13461=CYLINDRICAL_SURFACE('',#14991,2.5175);
#13462=CYLINDRICAL_SURFACE('',#14992,2.5175);
#13463=CYLINDRICAL_SURFACE('',#14993,2.5175);
#13464=CYLINDRICAL_SURFACE('',#14994,2.5175);
#13465=CYLINDRICAL_SURFACE('',#14995,2.5175);
#13466=CYLINDRICAL_SURFACE('',#14996,2.5175);
#13467=CYLINDRICAL_SURFACE('',#14997,2.5175);
#13468=CYLINDRICAL_SURFACE('',#14999,3.0735);
#13469=CYLINDRICAL_SURFACE('',#15001,3.0735);
#13470=CYLINDRICAL_SURFACE('',#15002,3.0735);
#13471=CYLINDRICAL_SURFACE('',#15003,3.0735);
#13472=CYLINDRICAL_SURFACE('',#15004,3.0735);
#13473=CYLINDRICAL_SURFACE('',#15005,3.0735);
#13474=CYLINDRICAL_SURFACE('',#15006,3.0735);
#13475=CYLINDRICAL_SURFACE('',#15007,3.0735);
#13476=CYLINDRICAL_SURFACE('',#15008,3.0735);
#13477=CYLINDRICAL_SURFACE('',#15010,2.5175);
#13478=CYLINDRICAL_SURFACE('',#15014,2.5175);
#13479=CYLINDRICAL_SURFACE('',#15015,2.5175);
#13480=CYLINDRICAL_SURFACE('',#15016,2.5175);
#13481=CYLINDRICAL_SURFACE('',#15017,2.5175);
#13482=CYLINDRICAL_SURFACE('',#15018,2.5175);
#13483=CYLINDRICAL_SURFACE('',#15019,2.5175);
#13484=CYLINDRICAL_SURFACE('',#15020,2.5175);
#13485=CYLINDRICAL_SURFACE('',#15021,2.5175);
#13486=CYLINDRICAL_SURFACE('',#15023,3.0735);
#13487=CYLINDRICAL_SURFACE('',#15025,3.0735);
#13488=CYLINDRICAL_SURFACE('',#15026,3.0735);
#13489=CYLINDRICAL_SURFACE('',#15027,3.0735);
#13490=CYLINDRICAL_SURFACE('',#15028,3.0735);
#13491=CYLINDRICAL_SURFACE('',#15029,3.0735);
#13492=CYLINDRICAL_SURFACE('',#15030,3.0735);
#13493=CYLINDRICAL_SURFACE('',#15031,3.0735);
#13494=CYLINDRICAL_SURFACE('',#15032,3.0735);
#13495=CYLINDRICAL_SURFACE('',#15034,2.5175);
#13496=CYLINDRICAL_SURFACE('',#15038,2.5175);
#13497=CYLINDRICAL_SURFACE('',#15039,2.5175);
#13498=CYLINDRICAL_SURFACE('',#15040,2.5175);
#13499=CYLINDRICAL_SURFACE('',#15041,2.5175);
#13500=CYLINDRICAL_SURFACE('',#15042,2.5175);
#13501=CYLINDRICAL_SURFACE('',#15043,2.5175);
#13502=CYLINDRICAL_SURFACE('',#15044,2.5175);
#13503=CYLINDRICAL_SURFACE('',#15045,2.5175);
#13504=CYLINDRICAL_SURFACE('',#15047,3.0735);
#13505=CYLINDRICAL_SURFACE('',#15049,3.0735);
#13506=CYLINDRICAL_SURFACE('',#15050,3.0735);
#13507=CYLINDRICAL_SURFACE('',#15051,3.0735);
#13508=CYLINDRICAL_SURFACE('',#15052,3.0735);
#13509=CYLINDRICAL_SURFACE('',#15053,3.0735);
#13510=CYLINDRICAL_SURFACE('',#15054,3.0735);
#13511=CYLINDRICAL_SURFACE('',#15055,3.0735);
#13512=CYLINDRICAL_SURFACE('',#15056,3.0735);
#13513=CYLINDRICAL_SURFACE('',#15058,7.);
#13514=CYLINDRICAL_SURFACE('',#15063,7.);
#13515=CYLINDRICAL_SURFACE('',#15068,7.);
#13516=CYLINDRICAL_SURFACE('',#15073,7.);
#13517=CYLINDRICAL_SURFACE('',#15078,4.5);
#13518=CYLINDRICAL_SURFACE('',#15080,4.5);
#13519=CYLINDRICAL_SURFACE('',#15082,4.5);
#13520=CYLINDRICAL_SURFACE('',#15084,4.5);
#13521=CYLINDRICAL_SURFACE('',#15087,3.0735);
#13522=CYLINDRICAL_SURFACE('',#15088,2.5175);
#13523=CYLINDRICAL_SURFACE('',#15090,3.0735);
#13524=CYLINDRICAL_SURFACE('',#15091,2.5175);
#13525=CYLINDRICAL_SURFACE('',#15093,3.0735);
#13526=CYLINDRICAL_SURFACE('',#15094,2.5175);
#13527=CYLINDRICAL_SURFACE('',#15096,3.0735);
#13528=CYLINDRICAL_SURFACE('',#15097,2.5175);
#13529=CYLINDRICAL_SURFACE('',#15099,3.0735);
#13530=CYLINDRICAL_SURFACE('',#15100,2.5175);
#13531=CYLINDRICAL_SURFACE('',#15102,3.0735);
#13532=CYLINDRICAL_SURFACE('',#15103,2.5175);
#13533=CYLINDRICAL_SURFACE('',#15105,3.0735);
#13534=CYLINDRICAL_SURFACE('',#15106,2.5175);
#13535=CYLINDRICAL_SURFACE('',#15108,3.0735);
#13536=CYLINDRICAL_SURFACE('',#15109,2.5175);
#13537=CYLINDRICAL_SURFACE('',#15143,20.);
#13538=CYLINDRICAL_SURFACE('',#15169,100.);
#13539=CYLINDRICAL_SURFACE('',#15188,40.);
#13540=CYLINDRICAL_SURFACE('',#15194,3.38975);
#13541=CYLINDRICAL_SURFACE('',#15198,3.38975);
#13542=CYLINDRICAL_SURFACE('',#15199,3.38975);
#13543=CYLINDRICAL_SURFACE('',#15200,3.38975);
#13544=CYLINDRICAL_SURFACE('',#15201,3.38975);
#13545=CYLINDRICAL_SURFACE('',#15202,3.38975);
#13546=CYLINDRICAL_SURFACE('',#15203,3.38975);
#13547=CYLINDRICAL_SURFACE('',#15205,4.085);
#13548=CYLINDRICAL_SURFACE('',#15207,4.085);
#13549=CYLINDRICAL_SURFACE('',#15208,4.085);
#13550=CYLINDRICAL_SURFACE('',#15209,4.085);
#13551=CYLINDRICAL_SURFACE('',#15210,4.085);
#13552=CYLINDRICAL_SURFACE('',#15211,4.085);
#13553=CYLINDRICAL_SURFACE('',#15212,4.085);
#13554=CYLINDRICAL_SURFACE('',#15214,3.38975);
#13555=CYLINDRICAL_SURFACE('',#15218,3.38975);
#13556=CYLINDRICAL_SURFACE('',#15219,3.38975);
#13557=CYLINDRICAL_SURFACE('',#15220,3.38975);
#13558=CYLINDRICAL_SURFACE('',#15221,3.38975);
#13559=CYLINDRICAL_SURFACE('',#15222,3.38975);
#13560=CYLINDRICAL_SURFACE('',#15223,3.38975);
#13561=CYLINDRICAL_SURFACE('',#15225,4.085);
#13562=CYLINDRICAL_SURFACE('',#15227,4.085);
#13563=CYLINDRICAL_SURFACE('',#15228,4.085);
#13564=CYLINDRICAL_SURFACE('',#15229,4.085);
#13565=CYLINDRICAL_SURFACE('',#15230,4.085);
#13566=CYLINDRICAL_SURFACE('',#15231,4.085);
#13567=CYLINDRICAL_SURFACE('',#15232,4.085);
#13568=CYLINDRICAL_SURFACE('',#15234,3.38975);
#13569=CYLINDRICAL_SURFACE('',#15238,3.38975);
#13570=CYLINDRICAL_SURFACE('',#15239,3.38975);
#13571=CYLINDRICAL_SURFACE('',#15240,3.38975);
#13572=CYLINDRICAL_SURFACE('',#15241,3.38975);
#13573=CYLINDRICAL_SURFACE('',#15242,3.38975);
#13574=CYLINDRICAL_SURFACE('',#15243,3.38975);
#13575=CYLINDRICAL_SURFACE('',#15245,4.085);
#13576=CYLINDRICAL_SURFACE('',#15247,4.085);
#13577=CYLINDRICAL_SURFACE('',#15248,4.085);
#13578=CYLINDRICAL_SURFACE('',#15249,4.085);
#13579=CYLINDRICAL_SURFACE('',#15250,4.085);
#13580=CYLINDRICAL_SURFACE('',#15251,4.085);
#13581=CYLINDRICAL_SURFACE('',#15252,4.085);
#13582=CYLINDRICAL_SURFACE('',#15254,3.38975);
#13583=CYLINDRICAL_SURFACE('',#15258,3.38975);
#13584=CYLINDRICAL_SURFACE('',#15259,3.38975);
#13585=CYLINDRICAL_SURFACE('',#15260,3.38975);
#13586=CYLINDRICAL_SURFACE('',#15261,3.38975);
#13587=CYLINDRICAL_SURFACE('',#15262,3.38975);
#13588=CYLINDRICAL_SURFACE('',#15263,3.38975);
#13589=CYLINDRICAL_SURFACE('',#15265,4.085);
#13590=CYLINDRICAL_SURFACE('',#15267,4.085);
#13591=CYLINDRICAL_SURFACE('',#15268,4.085);
#13592=CYLINDRICAL_SURFACE('',#15269,4.085);
#13593=CYLINDRICAL_SURFACE('',#15270,4.085);
#13594=CYLINDRICAL_SURFACE('',#15271,4.085);
#13595=CYLINDRICAL_SURFACE('',#15272,4.085);
#13596=CYLINDRICAL_SURFACE('',#15274,4.263);
#13597=CYLINDRICAL_SURFACE('',#15277,4.263);
#13598=CYLINDRICAL_SURFACE('',#15278,4.263);
#13599=CYLINDRICAL_SURFACE('',#15279,4.263);
#13600=CYLINDRICAL_SURFACE('',#15281,5.099);
#13601=CYLINDRICAL_SURFACE('',#15283,5.099);
#13602=CYLINDRICAL_SURFACE('',#15284,5.099);
#13603=CYLINDRICAL_SURFACE('',#15285,5.099);
#13604=CYLINDRICAL_SURFACE('',#15286,5.099);
#13605=CYLINDRICAL_SURFACE('',#15288,4.263);
#13606=CYLINDRICAL_SURFACE('',#15291,4.263);
#13607=CYLINDRICAL_SURFACE('',#15292,4.263);
#13608=CYLINDRICAL_SURFACE('',#15293,4.263);
#13609=CYLINDRICAL_SURFACE('',#15295,5.099);
#13610=CYLINDRICAL_SURFACE('',#15297,5.099);
#13611=CYLINDRICAL_SURFACE('',#15298,5.099);
#13612=CYLINDRICAL_SURFACE('',#15299,5.099);
#13613=CYLINDRICAL_SURFACE('',#15300,5.099);
#13614=CYLINDRICAL_SURFACE('',#15302,4.263);
#13615=CYLINDRICAL_SURFACE('',#15305,4.263);
#13616=CYLINDRICAL_SURFACE('',#15306,4.263);
#13617=CYLINDRICAL_SURFACE('',#15307,4.263);
#13618=CYLINDRICAL_SURFACE('',#15309,5.099);
#13619=CYLINDRICAL_SURFACE('',#15311,5.099);
#13620=CYLINDRICAL_SURFACE('',#15312,5.099);
#13621=CYLINDRICAL_SURFACE('',#15313,5.099);
#13622=CYLINDRICAL_SURFACE('',#15314,5.099);
#13623=CYLINDRICAL_SURFACE('',#15316,4.263);
#13624=CYLINDRICAL_SURFACE('',#15319,4.263);
#13625=CYLINDRICAL_SURFACE('',#15320,4.263);
#13626=CYLINDRICAL_SURFACE('',#15321,4.263);
#13627=CYLINDRICAL_SURFACE('',#15323,5.099);
#13628=CYLINDRICAL_SURFACE('',#15325,5.099);
#13629=CYLINDRICAL_SURFACE('',#15326,5.099);
#13630=CYLINDRICAL_SURFACE('',#15327,5.099);
#13631=CYLINDRICAL_SURFACE('',#15328,5.099);
#13632=CYLINDRICAL_SURFACE('',#15331,5.099);
#13633=CYLINDRICAL_SURFACE('',#15332,4.263);
#13634=CYLINDRICAL_SURFACE('',#15334,5.099);
#13635=CYLINDRICAL_SURFACE('',#15335,4.263);
#13636=CYLINDRICAL_SURFACE('',#15337,5.099);
#13637=CYLINDRICAL_SURFACE('',#15338,4.263);
#13638=CYLINDRICAL_SURFACE('',#15340,5.099);
#13639=CYLINDRICAL_SURFACE('',#15341,4.263);
#13640=CYLINDRICAL_SURFACE('',#15347,4.085);
#13641=CYLINDRICAL_SURFACE('',#15348,3.38975);
#13642=CYLINDRICAL_SURFACE('',#15350,4.085);
#13643=CYLINDRICAL_SURFACE('',#15351,3.38975);
#13644=CYLINDRICAL_SURFACE('',#15353,4.085);
#13645=CYLINDRICAL_SURFACE('',#15354,3.38975);
#13646=CYLINDRICAL_SURFACE('',#15356,4.085);
#13647=CYLINDRICAL_SURFACE('',#15357,3.38975);
#13648=CYLINDRICAL_SURFACE('',#15358,40.);
#13649=CYLINDRICAL_SURFACE('',#15363,20.);
#13650=CYLINDRICAL_SURFACE('',#15365,110.);
#13651=CYLINDRICAL_SURFACE('',#15371,5.13675);
#13652=CYLINDRICAL_SURFACE('',#15373,5.13675);
#13653=CYLINDRICAL_SURFACE('',#15374,5.13675);
#13654=CYLINDRICAL_SURFACE('',#15375,5.13675);
#13655=CYLINDRICAL_SURFACE('',#15376,5.13675);
#13656=CYLINDRICAL_SURFACE('',#15377,5.13675);
#13657=CYLINDRICAL_SURFACE('',#15378,5.13675);
#13658=CYLINDRICAL_SURFACE('',#15379,5.13675);
#13659=CYLINDRICAL_SURFACE('',#15380,5.13675);
#13660=CYLINDRICAL_SURFACE('',#15381,5.13675);
#13661=CYLINDRICAL_SURFACE('',#15382,5.13675);
#13662=CYLINDRICAL_SURFACE('',#15383,5.13675);
#13663=CYLINDRICAL_SURFACE('',#15384,5.13675);
#13664=CYLINDRICAL_SURFACE('',#15385,5.13675);
#13665=CYLINDRICAL_SURFACE('',#15386,5.13675);
#13666=CYLINDRICAL_SURFACE('',#15387,5.13675);
#13667=CYLINDRICAL_SURFACE('',#15388,5.13675);
#13668=CYLINDRICAL_SURFACE('',#15389,5.13675);
#13669=CYLINDRICAL_SURFACE('',#15390,5.13675);
#13670=CYLINDRICAL_SURFACE('',#15391,5.13675);
#13671=CYLINDRICAL_SURFACE('',#15392,5.13675);
#13672=CYLINDRICAL_SURFACE('',#15393,5.13675);
#13673=CYLINDRICAL_SURFACE('',#15394,5.13675);
#13674=CYLINDRICAL_SURFACE('',#15395,5.13675);
#13675=CYLINDRICAL_SURFACE('',#15396,5.13675);
#13676=CYLINDRICAL_SURFACE('',#15397,5.13675);
#13677=CYLINDRICAL_SURFACE('',#15398,5.13675);
#13678=CYLINDRICAL_SURFACE('',#15399,5.13675);
#13679=CYLINDRICAL_SURFACE('',#15401,6.11325);
#13680=CYLINDRICAL_SURFACE('',#15403,6.11325);
#13681=CYLINDRICAL_SURFACE('',#15404,6.11325);
#13682=CYLINDRICAL_SURFACE('',#15405,6.11325);
#13683=CYLINDRICAL_SURFACE('',#15406,6.11325);
#13684=CYLINDRICAL_SURFACE('',#15407,6.11325);
#13685=CYLINDRICAL_SURFACE('',#15408,6.11325);
#13686=CYLINDRICAL_SURFACE('',#15409,6.11325);
#13687=CYLINDRICAL_SURFACE('',#15410,6.11325);
#13688=CYLINDRICAL_SURFACE('',#15411,6.11325);
#13689=CYLINDRICAL_SURFACE('',#15412,6.11325);
#13690=CYLINDRICAL_SURFACE('',#15413,6.11325);
#13691=CYLINDRICAL_SURFACE('',#15414,6.11325);
#13692=CYLINDRICAL_SURFACE('',#15415,6.11325);
#13693=CYLINDRICAL_SURFACE('',#15416,6.11325);
#13694=CYLINDRICAL_SURFACE('',#15417,6.11325);
#13695=CYLINDRICAL_SURFACE('',#15418,6.11325);
#13696=CYLINDRICAL_SURFACE('',#15419,6.11325);
#13697=CYLINDRICAL_SURFACE('',#15420,6.11325);
#13698=CYLINDRICAL_SURFACE('',#15421,6.11325);
#13699=CYLINDRICAL_SURFACE('',#15422,6.11325);
#13700=CYLINDRICAL_SURFACE('',#15423,6.11325);
#13701=CYLINDRICAL_SURFACE('',#15424,6.11325);
#13702=CYLINDRICAL_SURFACE('',#15425,6.11325);
#13703=CYLINDRICAL_SURFACE('',#15426,6.11325);
#13704=CYLINDRICAL_SURFACE('',#15427,6.11325);
#13705=CYLINDRICAL_SURFACE('',#15428,6.11325);
#13706=CYLINDRICAL_SURFACE('',#15429,6.11325);
#13707=CYLINDRICAL_SURFACE('',#15430,6.11325);
#13708=CYLINDRICAL_SURFACE('',#15432,6.11325);
#13709=CYLINDRICAL_SURFACE('',#15434,5.13675);
#13710=CYLINDRICAL_SURFACE('',#15447,3.5);
#13711=CYLINDRICAL_SURFACE('',#15450,3.5);
#13712=CYLINDRICAL_SURFACE('',#15453,11.);
#13713=CYLINDRICAL_SURFACE('',#15456,11.);
#13714=CYLINDRICAL_SURFACE('',#15467,11.);
#13715=CYLINDRICAL_SURFACE('',#15470,7.);
#13716=CYLINDRICAL_SURFACE('',#15483,5.91675);
#13717=CYLINDRICAL_SURFACE('',#15485,5.91675);
#13718=CYLINDRICAL_SURFACE('',#15486,5.91675);
#13719=CYLINDRICAL_SURFACE('',#15487,5.91675);
#13720=CYLINDRICAL_SURFACE('',#15488,5.91675);
#13721=CYLINDRICAL_SURFACE('',#15489,5.91675);
#13722=CYLINDRICAL_SURFACE('',#15490,5.91675);
#13723=CYLINDRICAL_SURFACE('',#15491,5.91675);
#13724=CYLINDRICAL_SURFACE('',#15492,5.91675);
#13725=CYLINDRICAL_SURFACE('',#15493,5.91675);
#13726=CYLINDRICAL_SURFACE('',#15494,5.91675);
#13727=CYLINDRICAL_SURFACE('',#15495,5.91675);
#13728=CYLINDRICAL_SURFACE('',#15496,5.91675);
#13729=CYLINDRICAL_SURFACE('',#15497,5.91675);
#13730=CYLINDRICAL_SURFACE('',#15498,5.91675);
#13731=CYLINDRICAL_SURFACE('',#15499,5.91675);
#13732=CYLINDRICAL_SURFACE('',#15500,5.91675);
#13733=CYLINDRICAL_SURFACE('',#15501,5.91675);
#13734=CYLINDRICAL_SURFACE('',#15502,5.91675);
#13735=CYLINDRICAL_SURFACE('',#15503,5.91675);
#13736=CYLINDRICAL_SURFACE('',#15504,5.91675);
#13737=CYLINDRICAL_SURFACE('',#15505,5.91675);
#13738=CYLINDRICAL_SURFACE('',#15506,5.91675);
#13739=CYLINDRICAL_SURFACE('',#15507,5.91675);
#13740=CYLINDRICAL_SURFACE('',#15508,5.91675);
#13741=CYLINDRICAL_SURFACE('',#15509,5.91675);
#13742=CYLINDRICAL_SURFACE('',#15510,5.91675);
#13743=CYLINDRICAL_SURFACE('',#15511,5.91675);
#13744=CYLINDRICAL_SURFACE('',#15512,5.91675);
#13745=CYLINDRICAL_SURFACE('',#15513,5.91675);
#13746=CYLINDRICAL_SURFACE('',#15514,5.91675);
#13747=CYLINDRICAL_SURFACE('',#15515,5.91675);
#13748=CYLINDRICAL_SURFACE('',#15516,5.91675);
#13749=CYLINDRICAL_SURFACE('',#15517,5.91675);
#13750=CYLINDRICAL_SURFACE('',#15518,5.91675);
#13751=CYLINDRICAL_SURFACE('',#15519,5.91675);
#13752=CYLINDRICAL_SURFACE('',#15520,5.91675);
#13753=CYLINDRICAL_SURFACE('',#15524,4.91825);
#13754=CYLINDRICAL_SURFACE('',#15526,4.91825);
#13755=CYLINDRICAL_SURFACE('',#15527,4.91825);
#13756=CYLINDRICAL_SURFACE('',#15528,4.91825);
#13757=CYLINDRICAL_SURFACE('',#15529,4.91825);
#13758=CYLINDRICAL_SURFACE('',#15530,4.91825);
#13759=CYLINDRICAL_SURFACE('',#15531,4.91825);
#13760=CYLINDRICAL_SURFACE('',#15532,4.91825);
#13761=CYLINDRICAL_SURFACE('',#15533,4.91825);
#13762=CYLINDRICAL_SURFACE('',#15534,4.91825);
#13763=CYLINDRICAL_SURFACE('',#15535,4.91825);
#13764=CYLINDRICAL_SURFACE('',#15536,4.91825);
#13765=CYLINDRICAL_SURFACE('',#15537,4.91825);
#13766=CYLINDRICAL_SURFACE('',#15538,4.91825);
#13767=CYLINDRICAL_SURFACE('',#15539,4.91825);
#13768=CYLINDRICAL_SURFACE('',#15540,4.91825);
#13769=CYLINDRICAL_SURFACE('',#15541,4.91825);
#13770=CYLINDRICAL_SURFACE('',#15542,4.91825);
#13771=CYLINDRICAL_SURFACE('',#15543,4.91825);
#13772=CYLINDRICAL_SURFACE('',#15544,4.91825);
#13773=CYLINDRICAL_SURFACE('',#15545,4.91825);
#13774=CYLINDRICAL_SURFACE('',#15546,4.91825);
#13775=CYLINDRICAL_SURFACE('',#15547,4.91825);
#13776=CYLINDRICAL_SURFACE('',#15548,4.91825);
#13777=CYLINDRICAL_SURFACE('',#15549,4.91825);
#13778=CYLINDRICAL_SURFACE('',#15550,4.91825);
#13779=CYLINDRICAL_SURFACE('',#15551,4.91825);
#13780=CYLINDRICAL_SURFACE('',#15552,4.91825);
#13781=CYLINDRICAL_SURFACE('',#15553,4.91825);
#13782=CYLINDRICAL_SURFACE('',#15554,4.91825);
#13783=CYLINDRICAL_SURFACE('',#15555,4.91825);
#13784=CYLINDRICAL_SURFACE('',#15556,4.91825);
#13785=CYLINDRICAL_SURFACE('',#15557,4.91825);
#13786=CYLINDRICAL_SURFACE('',#15558,4.91825);
#13787=CYLINDRICAL_SURFACE('',#15559,4.91825);
#13788=CYLINDRICAL_SURFACE('',#15560,4.91825);
#13789=CYLINDRICAL_SURFACE('',#15568,5.);
#13790=CYLINDRICAL_SURFACE('',#15574,5.91675);
#13791=CYLINDRICAL_SURFACE('',#15577,4.91825);
#13792=CYLINDRICAL_SURFACE('',#15579,5.91675);
#13793=CYLINDRICAL_SURFACE('',#15582,10.);
#13794=CYLINDRICAL_SURFACE('',#15592,5.);
#13795=CYLINDRICAL_SURFACE('',#15594,9.);
#13796=CYLINDRICAL_SURFACE('',#15598,6.);
#13797=CYLINDRICAL_SURFACE('',#15601,7.);
#13798=CYLINDRICAL_SURFACE('',#15607,6.);
#13799=CYLINDRICAL_SURFACE('',#15610,10.);
#13800=CYLINDRICAL_SURFACE('',#15616,2.942);
#13801=CYLINDRICAL_SURFACE('',#15618,2.942);
#13802=CYLINDRICAL_SURFACE('',#15619,2.942);
#13803=CYLINDRICAL_SURFACE('',#15620,2.942);
#13804=CYLINDRICAL_SURFACE('',#15621,2.942);
#13805=CYLINDRICAL_SURFACE('',#15622,2.942);
#13806=CYLINDRICAL_SURFACE('',#15623,2.942);
#13807=CYLINDRICAL_SURFACE('',#15624,2.942);
#13808=CYLINDRICAL_SURFACE('',#15625,2.942);
#13809=CYLINDRICAL_SURFACE('',#15626,2.942);
#13810=CYLINDRICAL_SURFACE('',#15627,2.942);
#13811=CYLINDRICAL_SURFACE('',#15628,2.942);
#13812=CYLINDRICAL_SURFACE('',#15629,2.942);
#13813=CYLINDRICAL_SURFACE('',#15630,2.942);
#13814=CYLINDRICAL_SURFACE('',#15631,2.942);
#13815=CYLINDRICAL_SURFACE('',#15632,2.942);
#13816=CYLINDRICAL_SURFACE('',#15633,2.942);
#13817=CYLINDRICAL_SURFACE('',#15634,2.942);
#13818=CYLINDRICAL_SURFACE('',#15635,2.942);
#13819=CYLINDRICAL_SURFACE('',#15636,2.942);
#13820=CYLINDRICAL_SURFACE('',#15637,2.942);
#13821=CYLINDRICAL_SURFACE('',#15638,2.942);
#13822=CYLINDRICAL_SURFACE('',#15639,2.942);
#13823=CYLINDRICAL_SURFACE('',#15640,2.942);
#13824=CYLINDRICAL_SURFACE('',#15641,2.942);
#13825=CYLINDRICAL_SURFACE('',#15642,2.942);
#13826=CYLINDRICAL_SURFACE('',#15643,2.942);
#13827=CYLINDRICAL_SURFACE('',#15644,2.942);
#13828=CYLINDRICAL_SURFACE('',#15645,2.942);
#13829=CYLINDRICAL_SURFACE('',#15646,2.942);
#13830=CYLINDRICAL_SURFACE('',#15647,2.942);
#13831=CYLINDRICAL_SURFACE('',#15648,2.942);
#13832=CYLINDRICAL_SURFACE('',#15649,2.942);
#13833=CYLINDRICAL_SURFACE('',#15650,2.942);
#13834=CYLINDRICAL_SURFACE('',#15651,2.942);
#13835=CYLINDRICAL_SURFACE('',#15652,2.942);
#13836=CYLINDRICAL_SURFACE('',#15653,2.942);
#13837=CYLINDRICAL_SURFACE('',#15654,2.942);
#13838=CYLINDRICAL_SURFACE('',#15655,2.942);
#13839=CYLINDRICAL_SURFACE('',#15656,2.37175);
#13840=CYLINDRICAL_SURFACE('',#15658,2.37175);
#13841=CYLINDRICAL_SURFACE('',#15659,2.37175);
#13842=CYLINDRICAL_SURFACE('',#15660,2.37175);
#13843=CYLINDRICAL_SURFACE('',#15661,2.37175);
#13844=CYLINDRICAL_SURFACE('',#15662,2.37175);
#13845=CYLINDRICAL_SURFACE('',#15663,2.37175);
#13846=CYLINDRICAL_SURFACE('',#15664,2.37175);
#13847=CYLINDRICAL_SURFACE('',#15665,2.37175);
#13848=CYLINDRICAL_SURFACE('',#15666,2.37175);
#13849=CYLINDRICAL_SURFACE('',#15667,2.37175);
#13850=CYLINDRICAL_SURFACE('',#15668,2.37175);
#13851=CYLINDRICAL_SURFACE('',#15669,2.37175);
#13852=CYLINDRICAL_SURFACE('',#15670,2.37175);
#13853=CYLINDRICAL_SURFACE('',#15671,2.37175);
#13854=CYLINDRICAL_SURFACE('',#15672,2.37175);
#13855=CYLINDRICAL_SURFACE('',#15673,2.37175);
#13856=CYLINDRICAL_SURFACE('',#15674,2.37175);
#13857=CYLINDRICAL_SURFACE('',#15675,2.37175);
#13858=CYLINDRICAL_SURFACE('',#15676,2.37175);
#13859=CYLINDRICAL_SURFACE('',#15677,2.37175);
#13860=CYLINDRICAL_SURFACE('',#15678,2.37175);
#13861=CYLINDRICAL_SURFACE('',#15679,2.37175);
#13862=CYLINDRICAL_SURFACE('',#15680,2.37175);
#13863=CYLINDRICAL_SURFACE('',#15681,2.37175);
#13864=CYLINDRICAL_SURFACE('',#15682,2.37175);
#13865=CYLINDRICAL_SURFACE('',#15683,2.37175);
#13866=CYLINDRICAL_SURFACE('',#15684,2.37175);
#13867=CYLINDRICAL_SURFACE('',#15685,2.37175);
#13868=CYLINDRICAL_SURFACE('',#15686,2.37175);
#13869=CYLINDRICAL_SURFACE('',#15687,2.37175);
#13870=CYLINDRICAL_SURFACE('',#15688,2.37175);
#13871=CYLINDRICAL_SURFACE('',#15689,2.37175);
#13872=CYLINDRICAL_SURFACE('',#15690,2.37175);
#13873=CYLINDRICAL_SURFACE('',#15691,2.37175);
#13874=CYLINDRICAL_SURFACE('',#15692,2.37175);
#13875=CYLINDRICAL_SURFACE('',#15693,2.37175);
#13876=CYLINDRICAL_SURFACE('',#15694,2.37175);
#13877=CYLINDRICAL_SURFACE('',#15695,2.37175);
#13878=CYLINDRICAL_SURFACE('',#15699,2.37175);
#13879=CYLINDRICAL_SURFACE('',#15701,2.942);
#13880=CYLINDRICAL_SURFACE('',#15711,5.);
#13881=CYLINDRICAL_SURFACE('',#15716,3.5);
#13882=CYLINDRICAL_SURFACE('',#15719,7.);
#13883=CYLINDRICAL_SURFACE('',#15725,3.933);
#13884=CYLINDRICAL_SURFACE('',#15727,3.933);
#13885=CYLINDRICAL_SURFACE('',#15728,3.933);
#13886=CYLINDRICAL_SURFACE('',#15729,3.933);
#13887=CYLINDRICAL_SURFACE('',#15730,3.933);
#13888=CYLINDRICAL_SURFACE('',#15731,3.933);
#13889=CYLINDRICAL_SURFACE('',#15732,3.933);
#13890=CYLINDRICAL_SURFACE('',#15733,3.933);
#13891=CYLINDRICAL_SURFACE('',#15734,3.933);
#13892=CYLINDRICAL_SURFACE('',#15735,3.933);
#13893=CYLINDRICAL_SURFACE('',#15736,3.933);
#13894=CYLINDRICAL_SURFACE('',#15737,3.933);
#13895=CYLINDRICAL_SURFACE('',#15738,3.933);
#13896=CYLINDRICAL_SURFACE('',#15739,3.933);
#13897=CYLINDRICAL_SURFACE('',#15740,3.933);
#13898=CYLINDRICAL_SURFACE('',#15741,3.933);
#13899=CYLINDRICAL_SURFACE('',#15742,3.933);
#13900=CYLINDRICAL_SURFACE('',#15743,3.933);
#13901=CYLINDRICAL_SURFACE('',#15744,3.933);
#13902=CYLINDRICAL_SURFACE('',#15745,3.933);
#13903=CYLINDRICAL_SURFACE('',#15746,3.933);
#13904=CYLINDRICAL_SURFACE('',#15747,3.933);
#13905=CYLINDRICAL_SURFACE('',#15748,3.933);
#13906=CYLINDRICAL_SURFACE('',#15749,3.933);
#13907=CYLINDRICAL_SURFACE('',#15750,3.933);
#13908=CYLINDRICAL_SURFACE('',#15751,3.933);
#13909=CYLINDRICAL_SURFACE('',#15752,3.933);
#13910=CYLINDRICAL_SURFACE('',#15753,3.933);
#13911=CYLINDRICAL_SURFACE('',#15754,3.933);
#13912=CYLINDRICAL_SURFACE('',#15755,3.933);
#13913=CYLINDRICAL_SURFACE('',#15756,3.933);
#13914=CYLINDRICAL_SURFACE('',#15757,3.933);
#13915=CYLINDRICAL_SURFACE('',#15759,3.22275);
#13916=CYLINDRICAL_SURFACE('',#15761,3.22275);
#13917=CYLINDRICAL_SURFACE('',#15763,3.22275);
#13918=CYLINDRICAL_SURFACE('',#15764,3.22275);
#13919=CYLINDRICAL_SURFACE('',#15765,3.22275);
#13920=CYLINDRICAL_SURFACE('',#15766,3.22275);
#13921=CYLINDRICAL_SURFACE('',#15767,3.22275);
#13922=CYLINDRICAL_SURFACE('',#15768,3.22275);
#13923=CYLINDRICAL_SURFACE('',#15769,3.22275);
#13924=CYLINDRICAL_SURFACE('',#15770,3.22275);
#13925=CYLINDRICAL_SURFACE('',#15771,3.22275);
#13926=CYLINDRICAL_SURFACE('',#15772,3.22275);
#13927=CYLINDRICAL_SURFACE('',#15773,3.22275);
#13928=CYLINDRICAL_SURFACE('',#15774,3.22275);
#13929=CYLINDRICAL_SURFACE('',#15775,3.22275);
#13930=CYLINDRICAL_SURFACE('',#15776,3.22275);
#13931=CYLINDRICAL_SURFACE('',#15777,3.22275);
#13932=CYLINDRICAL_SURFACE('',#15778,3.22275);
#13933=CYLINDRICAL_SURFACE('',#15779,3.22275);
#13934=CYLINDRICAL_SURFACE('',#15780,3.22275);
#13935=CYLINDRICAL_SURFACE('',#15781,3.22275);
#13936=CYLINDRICAL_SURFACE('',#15782,3.22275);
#13937=CYLINDRICAL_SURFACE('',#15783,3.22275);
#13938=CYLINDRICAL_SURFACE('',#15784,3.22275);
#13939=CYLINDRICAL_SURFACE('',#15785,3.22275);
#13940=CYLINDRICAL_SURFACE('',#15786,3.22275);
#13941=CYLINDRICAL_SURFACE('',#15787,3.22275);
#13942=CYLINDRICAL_SURFACE('',#15788,3.22275);
#13943=CYLINDRICAL_SURFACE('',#15789,3.22275);
#13944=CYLINDRICAL_SURFACE('',#15790,3.22275);
#13945=CYLINDRICAL_SURFACE('',#15791,3.22275);
#13946=CYLINDRICAL_SURFACE('',#15792,3.22275);
#13947=CYLINDRICAL_SURFACE('',#15797,3.22275);
#13948=CYLINDRICAL_SURFACE('',#15799,3.933);
#13949=CYLINDRICAL_SURFACE('',#15809,6.5);
#13950=ADVANCED_FACE('',(#522),#13369,.F.);
#13951=ADVANCED_FACE('',(#523),#13370,.F.);
#13952=ADVANCED_FACE('',(#524),#13371,.F.);
#13953=ADVANCED_FACE('',(#525),#13372,.F.);
#13954=ADVANCED_FACE('',(#526),#13373,.F.);
#13955=ADVANCED_FACE('',(#527),#13374,.F.);
#13956=ADVANCED_FACE('',(#528),#13375,.F.);
#13957=ADVANCED_FACE('',(#529),#13376,.F.);
#13958=ADVANCED_FACE('',(#530),#13377,.F.);
#13959=ADVANCED_FACE('',(#531),#13378,.F.);
#13960=ADVANCED_FACE('',(#532),#13379,.F.);
#13961=ADVANCED_FACE('',(#533),#13380,.F.);
#13962=ADVANCED_FACE('',(#534),#13381,.F.);
#13963=ADVANCED_FACE('',(#535),#13382,.F.);
#13964=ADVANCED_FACE('',(#536),#13383,.F.);
#13965=ADVANCED_FACE('',(#537),#13384,.F.);
#13966=ADVANCED_FACE('',(#538),#13385,.F.);
#13967=ADVANCED_FACE('',(#539),#13386,.F.);
#13968=ADVANCED_FACE('',(#540),#13387,.F.);
#13969=ADVANCED_FACE('',(#541),#13388,.F.);
#13970=ADVANCED_FACE('',(#542),#13389,.F.);
#13971=ADVANCED_FACE('',(#543),#13390,.F.);
#13972=ADVANCED_FACE('',(#544),#13391,.F.);
#13973=ADVANCED_FACE('',(#545),#13392,.F.);
#13974=ADVANCED_FACE('',(#546),#13393,.F.);
#13975=ADVANCED_FACE('',(#547),#13394,.F.);
#13976=ADVANCED_FACE('',(#548),#13395,.F.);
#13977=ADVANCED_FACE('',(#549),#13396,.F.);
#13978=ADVANCED_FACE('',(#550),#13397,.F.);
#13979=ADVANCED_FACE('',(#551),#13398,.F.);
#13980=ADVANCED_FACE('',(#552),#13399,.F.);
#13981=ADVANCED_FACE('',(#553),#13400,.F.);
#13982=ADVANCED_FACE('',(#554),#13401,.F.);
#13983=ADVANCED_FACE('',(#555),#13402,.F.);
#13984=ADVANCED_FACE('',(#556),#13403,.F.);
#13985=ADVANCED_FACE('',(#557),#13404,.F.);
#13986=ADVANCED_FACE('',(#558),#13405,.F.);
#13987=ADVANCED_FACE('',(#559),#13406,.F.);
#13988=ADVANCED_FACE('',(#560),#13407,.F.);
#13989=ADVANCED_FACE('',(#561),#13408,.F.);
#13990=ADVANCED_FACE('',(#562),#13409,.F.);
#13991=ADVANCED_FACE('',(#563),#13410,.F.);
#13992=ADVANCED_FACE('',(#564),#13411,.F.);
#13993=ADVANCED_FACE('',(#565),#13412,.F.);
#13994=ADVANCED_FACE('',(#566),#13413,.F.);
#13995=ADVANCED_FACE('',(#567),#13414,.F.);
#13996=ADVANCED_FACE('',(#568),#13415,.F.);
#13997=ADVANCED_FACE('',(#569),#13416,.F.);
#13998=ADVANCED_FACE('',(#570),#13417,.F.);
#13999=ADVANCED_FACE('',(#571),#13418,.F.);
#14000=ADVANCED_FACE('',(#572),#13419,.F.);
#14001=ADVANCED_FACE('',(#573),#13420,.F.);
#14002=ADVANCED_FACE('',(#574),#13421,.F.);
#14003=ADVANCED_FACE('',(#575),#13422,.F.);
#14004=ADVANCED_FACE('',(#576),#13423,.F.);
#14005=ADVANCED_FACE('',(#577),#13424,.F.);
#14006=ADVANCED_FACE('',(#578),#13425,.F.);
#14007=ADVANCED_FACE('',(#579),#13426,.F.);
#14008=ADVANCED_FACE('',(#580),#13427,.F.);
#14009=ADVANCED_FACE('',(#581),#13428,.F.);
#14010=ADVANCED_FACE('',(#582),#13429,.F.);
#14011=ADVANCED_FACE('',(#583),#13430,.F.);
#14012=ADVANCED_FACE('',(#584),#13431,.F.);
#14013=ADVANCED_FACE('',(#585),#13432,.F.);
#14014=ADVANCED_FACE('',(#586),#13433,.F.);
#14015=ADVANCED_FACE('',(#587),#13434,.F.);
#14016=ADVANCED_FACE('',(#588),#13435,.F.);
#14017=ADVANCED_FACE('',(#589),#13436,.F.);
#14018=ADVANCED_FACE('',(#590),#13437,.F.);
#14019=ADVANCED_FACE('',(#591),#13438,.F.);
#14020=ADVANCED_FACE('',(#592),#13439,.F.);
#14021=ADVANCED_FACE('',(#593),#13440,.F.);
#14022=ADVANCED_FACE('',(#594),#13441,.F.);
#14023=ADVANCED_FACE('',(#595),#13442,.F.);
#14024=ADVANCED_FACE('',(#596),#13443,.F.);
#14025=ADVANCED_FACE('',(#597),#13444,.F.);
#14026=ADVANCED_FACE('',(#598),#13445,.F.);
#14027=ADVANCED_FACE('',(#599),#13446,.F.);
#14028=ADVANCED_FACE('',(#600),#13447,.F.);
#14029=ADVANCED_FACE('',(#601),#13448,.F.);
#14030=ADVANCED_FACE('',(#602),#13449,.F.);
#14031=ADVANCED_FACE('',(#603),#13450,.F.);
#14032=ADVANCED_FACE('',(#604),#13451,.F.);
#14033=ADVANCED_FACE('',(#605),#13452,.F.);
#14034=ADVANCED_FACE('',(#606),#13453,.F.);
#14035=ADVANCED_FACE('',(#607),#13454,.F.);
#14036=ADVANCED_FACE('',(#608),#13455,.F.);
#14037=ADVANCED_FACE('',(#609),#13456,.F.);
#14038=ADVANCED_FACE('',(#610),#13457,.F.);
#14039=ADVANCED_FACE('',(#611),#13458,.F.);
#14040=ADVANCED_FACE('',(#612),#13459,.F.);
#14041=ADVANCED_FACE('',(#613),#13460,.F.);
#14042=ADVANCED_FACE('',(#614),#13461,.F.);
#14043=ADVANCED_FACE('',(#615),#13462,.F.);
#14044=ADVANCED_FACE('',(#616),#13463,.F.);
#14045=ADVANCED_FACE('',(#617),#13464,.F.);
#14046=ADVANCED_FACE('',(#618),#13465,.F.);
#14047=ADVANCED_FACE('',(#619),#13466,.F.);
#14048=ADVANCED_FACE('',(#620),#13467,.F.);
#14049=ADVANCED_FACE('',(#621),#13468,.F.);
#14050=ADVANCED_FACE('',(#622),#13469,.F.);
#14051=ADVANCED_FACE('',(#623),#13470,.F.);
#14052=ADVANCED_FACE('',(#624),#13471,.F.);
#14053=ADVANCED_FACE('',(#625),#13472,.F.);
#14054=ADVANCED_FACE('',(#626),#13473,.F.);
#14055=ADVANCED_FACE('',(#627),#13474,.F.);
#14056=ADVANCED_FACE('',(#628),#13475,.F.);
#14057=ADVANCED_FACE('',(#629),#13476,.F.);
#14058=ADVANCED_FACE('',(#630),#13477,.F.);
#14059=ADVANCED_FACE('',(#631),#13478,.F.);
#14060=ADVANCED_FACE('',(#632),#13479,.F.);
#14061=ADVANCED_FACE('',(#633),#13480,.F.);
#14062=ADVANCED_FACE('',(#634),#13481,.F.);
#14063=ADVANCED_FACE('',(#635),#13482,.F.);
#14064=ADVANCED_FACE('',(#636),#13483,.F.);
#14065=ADVANCED_FACE('',(#637),#13484,.F.);
#14066=ADVANCED_FACE('',(#638),#13485,.F.);
#14067=ADVANCED_FACE('',(#639),#13486,.F.);
#14068=ADVANCED_FACE('',(#640),#13487,.F.);
#14069=ADVANCED_FACE('',(#641),#13488,.F.);
#14070=ADVANCED_FACE('',(#642),#13489,.F.);
#14071=ADVANCED_FACE('',(#643),#13490,.F.);
#14072=ADVANCED_FACE('',(#644),#13491,.F.);
#14073=ADVANCED_FACE('',(#645),#13492,.F.);
#14074=ADVANCED_FACE('',(#646),#13493,.F.);
#14075=ADVANCED_FACE('',(#647),#13494,.F.);
#14076=ADVANCED_FACE('',(#648),#13495,.F.);
#14077=ADVANCED_FACE('',(#649),#13496,.F.);
#14078=ADVANCED_FACE('',(#650),#13497,.F.);
#14079=ADVANCED_FACE('',(#651),#13498,.F.);
#14080=ADVANCED_FACE('',(#652),#13499,.F.);
#14081=ADVANCED_FACE('',(#653),#13500,.F.);
#14082=ADVANCED_FACE('',(#654),#13501,.F.);
#14083=ADVANCED_FACE('',(#655),#13502,.F.);
#14084=ADVANCED_FACE('',(#656),#13503,.F.);
#14085=ADVANCED_FACE('',(#657),#13504,.F.);
#14086=ADVANCED_FACE('',(#658),#13505,.F.);
#14087=ADVANCED_FACE('',(#659),#13506,.F.);
#14088=ADVANCED_FACE('',(#660),#13507,.F.);
#14089=ADVANCED_FACE('',(#661),#13508,.F.);
#14090=ADVANCED_FACE('',(#662),#13509,.F.);
#14091=ADVANCED_FACE('',(#663),#13510,.F.);
#14092=ADVANCED_FACE('',(#664),#13511,.F.);
#14093=ADVANCED_FACE('',(#665),#13512,.F.);
#14094=ADVANCED_FACE('',(#666),#13513,.F.);
#14095=ADVANCED_FACE('',(#667,#298),#365,.F.);
#14096=ADVANCED_FACE('',(#668),#13514,.F.);
#14097=ADVANCED_FACE('',(#669,#299),#366,.F.);
#14098=ADVANCED_FACE('',(#670),#13515,.F.);
#14099=ADVANCED_FACE('',(#671,#300),#367,.F.);
#14100=ADVANCED_FACE('',(#672),#13516,.F.);
#14101=ADVANCED_FACE('',(#673,#301),#368,.F.);
#14102=ADVANCED_FACE('',(#674),#13517,.F.);
#14103=ADVANCED_FACE('',(#675),#13518,.F.);
#14104=ADVANCED_FACE('',(#676),#13519,.F.);
#14105=ADVANCED_FACE('',(#677),#13520,.F.);
#14106=ADVANCED_FACE('',(#678),#369,.T.);
#14107=ADVANCED_FACE('',(#679),#13521,.F.);
#14108=ADVANCED_FACE('',(#680),#258,.F.);
#14109=ADVANCED_FACE('',(#681),#259,.F.);
#14110=ADVANCED_FACE('',(#682),#13522,.F.);
#14111=ADVANCED_FACE('',(#683),#370,.T.);
#14112=ADVANCED_FACE('',(#684),#13523,.F.);
#14113=ADVANCED_FACE('',(#685),#260,.F.);
#14114=ADVANCED_FACE('',(#686),#261,.F.);
#14115=ADVANCED_FACE('',(#687),#13524,.F.);
#14116=ADVANCED_FACE('',(#688),#371,.T.);
#14117=ADVANCED_FACE('',(#689),#13525,.F.);
#14118=ADVANCED_FACE('',(#690),#262,.F.);
#14119=ADVANCED_FACE('',(#691),#263,.F.);
#14120=ADVANCED_FACE('',(#692),#13526,.F.);
#14121=ADVANCED_FACE('',(#693),#372,.T.);
#14122=ADVANCED_FACE('',(#694),#13527,.F.);
#14123=ADVANCED_FACE('',(#695),#264,.F.);
#14124=ADVANCED_FACE('',(#696),#265,.F.);
#14125=ADVANCED_FACE('',(#697),#13528,.F.);
#14126=ADVANCED_FACE('',(#698),#373,.T.);
#14127=ADVANCED_FACE('',(#699),#13529,.F.);
#14128=ADVANCED_FACE('',(#700),#266,.F.);
#14129=ADVANCED_FACE('',(#701),#267,.F.);
#14130=ADVANCED_FACE('',(#702),#13530,.F.);
#14131=ADVANCED_FACE('',(#703),#374,.T.);
#14132=ADVANCED_FACE('',(#704),#13531,.F.);
#14133=ADVANCED_FACE('',(#705),#268,.F.);
#14134=ADVANCED_FACE('',(#706),#269,.F.);
#14135=ADVANCED_FACE('',(#707),#13532,.F.);
#14136=ADVANCED_FACE('',(#708),#375,.T.);
#14137=ADVANCED_FACE('',(#709),#13533,.F.);
#14138=ADVANCED_FACE('',(#710),#270,.F.);
#14139=ADVANCED_FACE('',(#711),#271,.F.);
#14140=ADVANCED_FACE('',(#712),#13534,.F.);
#14141=ADVANCED_FACE('',(#713),#376,.T.);
#14142=ADVANCED_FACE('',(#714),#13535,.F.);
#14143=ADVANCED_FACE('',(#715),#272,.F.);
#14144=ADVANCED_FACE('',(#716),#273,.F.);
#14145=ADVANCED_FACE('',(#717),#13536,.F.);
#14146=ADVANCED_FACE('',(#718),#377,.F.);
#14147=ADVANCED_FACE('',(#719),#378,.F.);
#14148=ADVANCED_FACE('',(#720),#379,.F.);
#14149=ADVANCED_FACE('',(#721,#302,#303),#380,.F.);
#14150=ADVANCED_FACE('',(#722),#381,.F.);
#14151=ADVANCED_FACE('',(#723),#382,.F.);
#14152=ADVANCED_FACE('',(#724),#383,.F.);
#14153=ADVANCED_FACE('',(#725,#304,#305),#384,.F.);
#14154=ADVANCED_FACE('',(#726),#385,.F.);
#14155=ADVANCED_FACE('',(#727),#386,.F.);
#14156=ADVANCED_FACE('',(#728,#306),#387,.T.);
#14157=ADVANCED_FACE('',(#729,#307),#388,.T.);
#14158=ADVANCED_FACE('',(#730),#389,.F.);
#14159=ADVANCED_FACE('',(#731),#390,.F.);
#14160=ADVANCED_FACE('',(#732),#391,.F.);
#14161=ADVANCED_FACE('',(#733),#392,.F.);
#14162=ADVANCED_FACE('',(#734),#393,.F.);
#14163=ADVANCED_FACE('',(#735),#394,.F.);
#14164=ADVANCED_FACE('',(#736,#308),#395,.T.);
#14165=ADVANCED_FACE('',(#737),#396,.F.);
#14166=ADVANCED_FACE('',(#738),#397,.F.);
#14167=ADVANCED_FACE('',(#739),#398,.F.);
#14168=ADVANCED_FACE('',(#740),#399,.F.);
#14169=ADVANCED_FACE('',(#741),#13537,.F.);
#14170=ADVANCED_FACE('',(#742),#400,.F.);
#14171=ADVANCED_FACE('',(#743),#401,.F.);
#14172=ADVANCED_FACE('',(#744),#402,.F.);
#14173=ADVANCED_FACE('',(#745),#403,.F.);
#14174=ADVANCED_FACE('',(#746),#404,.F.);
#14175=ADVANCED_FACE('',(#747),#405,.F.);
#14176=ADVANCED_FACE('',(#748),#406,.F.);
#14177=ADVANCED_FACE('',(#749,#309,#310),#407,.F.);
#14178=ADVANCED_FACE('',(#750),#408,.F.);
#14179=ADVANCED_FACE('',(#751),#409,.F.);
#14180=ADVANCED_FACE('',(#752),#410,.F.);
#14181=ADVANCED_FACE('',(#753),#411,.F.);
#14182=ADVANCED_FACE('',(#754),#412,.F.);
#14183=ADVANCED_FACE('',(#755,#311,#312),#413,.F.);
#14184=ADVANCED_FACE('',(#756),#414,.F.);
#14185=ADVANCED_FACE('',(#757),#415,.F.);
#14186=ADVANCED_FACE('',(#758),#416,.F.);
#14187=ADVANCED_FACE('',(#759),#13538,.T.);
#14188=ADVANCED_FACE('',(#760),#417,.F.);
#14189=ADVANCED_FACE('',(#761),#418,.F.);
#14190=ADVANCED_FACE('',(#762,#313),#419,.T.);
#14191=ADVANCED_FACE('',(#763),#420,.F.);
#14192=ADVANCED_FACE('',(#764),#421,.F.);
#14193=ADVANCED_FACE('',(#765),#422,.F.);
#14194=ADVANCED_FACE('',(#766),#423,.F.);
#14195=ADVANCED_FACE('',(#767),#424,.F.);
#14196=ADVANCED_FACE('',(#768),#425,.F.);
#14197=ADVANCED_FACE('',(#769),#426,.F.);
#14198=ADVANCED_FACE('',(#770),#427,.F.);
#14199=ADVANCED_FACE('',(#771),#428,.F.);
#14200=ADVANCED_FACE('',(#772),#429,.F.);
#14201=ADVANCED_FACE('',(#773),#430,.F.);
#14202=ADVANCED_FACE('',(#774),#431,.F.);
#14203=ADVANCED_FACE('',(#775),#432,.F.);
#14204=ADVANCED_FACE('',(#776),#13539,.F.);
#14205=ADVANCED_FACE('',(#777,#314),#433,.F.);
#14206=ADVANCED_FACE('',(#778,#315,#316,#317,#318,#319,#320,#321,#322,#323,
#324,#325,#326,#327),#434,.F.);
#14207=ADVANCED_FACE('',(#779),#13540,.F.);
#14208=ADVANCED_FACE('',(#780),#13541,.F.);
#14209=ADVANCED_FACE('',(#781),#13542,.F.);
#14210=ADVANCED_FACE('',(#782),#13543,.F.);
#14211=ADVANCED_FACE('',(#783),#13544,.F.);
#14212=ADVANCED_FACE('',(#784),#13545,.F.);
#14213=ADVANCED_FACE('',(#785),#13546,.F.);
#14214=ADVANCED_FACE('',(#786),#13547,.F.);
#14215=ADVANCED_FACE('',(#787),#13548,.F.);
#14216=ADVANCED_FACE('',(#788),#13549,.F.);
#14217=ADVANCED_FACE('',(#789),#13550,.F.);
#14218=ADVANCED_FACE('',(#790),#13551,.F.);
#14219=ADVANCED_FACE('',(#791),#13552,.F.);
#14220=ADVANCED_FACE('',(#792),#13553,.F.);
#14221=ADVANCED_FACE('',(#793),#13554,.F.);
#14222=ADVANCED_FACE('',(#794),#13555,.F.);
#14223=ADVANCED_FACE('',(#795),#13556,.F.);
#14224=ADVANCED_FACE('',(#796),#13557,.F.);
#14225=ADVANCED_FACE('',(#797),#13558,.F.);
#14226=ADVANCED_FACE('',(#798),#13559,.F.);
#14227=ADVANCED_FACE('',(#799),#13560,.F.);
#14228=ADVANCED_FACE('',(#800),#13561,.F.);
#14229=ADVANCED_FACE('',(#801),#13562,.F.);
#14230=ADVANCED_FACE('',(#802),#13563,.F.);
#14231=ADVANCED_FACE('',(#803),#13564,.F.);
#14232=ADVANCED_FACE('',(#804),#13565,.F.);
#14233=ADVANCED_FACE('',(#805),#13566,.F.);
#14234=ADVANCED_FACE('',(#806),#13567,.F.);
#14235=ADVANCED_FACE('',(#807),#13568,.F.);
#14236=ADVANCED_FACE('',(#808),#13569,.F.);
#14237=ADVANCED_FACE('',(#809),#13570,.F.);
#14238=ADVANCED_FACE('',(#810),#13571,.F.);
#14239=ADVANCED_FACE('',(#811),#13572,.F.);
#14240=ADVANCED_FACE('',(#812),#13573,.F.);
#14241=ADVANCED_FACE('',(#813),#13574,.F.);
#14242=ADVANCED_FACE('',(#814),#13575,.F.);
#14243=ADVANCED_FACE('',(#815),#13576,.F.);
#14244=ADVANCED_FACE('',(#816),#13577,.F.);
#14245=ADVANCED_FACE('',(#817),#13578,.F.);
#14246=ADVANCED_FACE('',(#818),#13579,.F.);
#14247=ADVANCED_FACE('',(#819),#13580,.F.);
#14248=ADVANCED_FACE('',(#820),#13581,.F.);
#14249=ADVANCED_FACE('',(#821),#13582,.F.);
#14250=ADVANCED_FACE('',(#822),#13583,.F.);
#14251=ADVANCED_FACE('',(#823),#13584,.F.);
#14252=ADVANCED_FACE('',(#824),#13585,.F.);
#14253=ADVANCED_FACE('',(#825),#13586,.F.);
#14254=ADVANCED_FACE('',(#826),#13587,.F.);
#14255=ADVANCED_FACE('',(#827),#13588,.F.);
#14256=ADVANCED_FACE('',(#828),#13589,.F.);
#14257=ADVANCED_FACE('',(#829),#13590,.F.);
#14258=ADVANCED_FACE('',(#830),#13591,.F.);
#14259=ADVANCED_FACE('',(#831),#13592,.F.);
#14260=ADVANCED_FACE('',(#832),#13593,.F.);
#14261=ADVANCED_FACE('',(#833),#13594,.F.);
#14262=ADVANCED_FACE('',(#834),#13595,.F.);
#14263=ADVANCED_FACE('',(#835),#13596,.F.);
#14264=ADVANCED_FACE('',(#836),#13597,.F.);
#14265=ADVANCED_FACE('',(#837),#13598,.F.);
#14266=ADVANCED_FACE('',(#838),#13599,.F.);
#14267=ADVANCED_FACE('',(#839),#13600,.F.);
#14268=ADVANCED_FACE('',(#840),#13601,.F.);
#14269=ADVANCED_FACE('',(#841),#13602,.F.);
#14270=ADVANCED_FACE('',(#842),#13603,.F.);
#14271=ADVANCED_FACE('',(#843),#13604,.F.);
#14272=ADVANCED_FACE('',(#844),#13605,.F.);
#14273=ADVANCED_FACE('',(#845),#13606,.F.);
#14274=ADVANCED_FACE('',(#846),#13607,.F.);
#14275=ADVANCED_FACE('',(#847),#13608,.F.);
#14276=ADVANCED_FACE('',(#848),#13609,.F.);
#14277=ADVANCED_FACE('',(#849),#13610,.F.);
#14278=ADVANCED_FACE('',(#850),#13611,.F.);
#14279=ADVANCED_FACE('',(#851),#13612,.F.);
#14280=ADVANCED_FACE('',(#852),#13613,.F.);
#14281=ADVANCED_FACE('',(#853),#13614,.F.);
#14282=ADVANCED_FACE('',(#854),#13615,.F.);
#14283=ADVANCED_FACE('',(#855),#13616,.F.);
#14284=ADVANCED_FACE('',(#856),#13617,.F.);
#14285=ADVANCED_FACE('',(#857),#13618,.F.);
#14286=ADVANCED_FACE('',(#858),#13619,.F.);
#14287=ADVANCED_FACE('',(#859),#13620,.F.);
#14288=ADVANCED_FACE('',(#860),#13621,.F.);
#14289=ADVANCED_FACE('',(#861),#13622,.F.);
#14290=ADVANCED_FACE('',(#862),#13623,.F.);
#14291=ADVANCED_FACE('',(#863),#13624,.F.);
#14292=ADVANCED_FACE('',(#864),#13625,.F.);
#14293=ADVANCED_FACE('',(#865),#13626,.F.);
#14294=ADVANCED_FACE('',(#866),#13627,.F.);
#14295=ADVANCED_FACE('',(#867),#13628,.F.);
#14296=ADVANCED_FACE('',(#868),#13629,.F.);
#14297=ADVANCED_FACE('',(#869),#13630,.F.);
#14298=ADVANCED_FACE('',(#870),#13631,.F.);
#14299=ADVANCED_FACE('',(#871),#435,.F.);
#14300=ADVANCED_FACE('',(#872),#13632,.F.);
#14301=ADVANCED_FACE('',(#873),#274,.F.);
#14302=ADVANCED_FACE('',(#874),#275,.F.);
#14303=ADVANCED_FACE('',(#875),#13633,.F.);
#14304=ADVANCED_FACE('',(#876),#436,.F.);
#14305=ADVANCED_FACE('',(#877),#13634,.F.);
#14306=ADVANCED_FACE('',(#878),#276,.F.);
#14307=ADVANCED_FACE('',(#879),#277,.F.);
#14308=ADVANCED_FACE('',(#880),#13635,.F.);
#14309=ADVANCED_FACE('',(#881),#437,.F.);
#14310=ADVANCED_FACE('',(#882),#13636,.F.);
#14311=ADVANCED_FACE('',(#883),#278,.F.);
#14312=ADVANCED_FACE('',(#884),#279,.F.);
#14313=ADVANCED_FACE('',(#885),#13637,.F.);
#14314=ADVANCED_FACE('',(#886),#438,.F.);
#14315=ADVANCED_FACE('',(#887),#13638,.F.);
#14316=ADVANCED_FACE('',(#888),#280,.F.);
#14317=ADVANCED_FACE('',(#889),#281,.F.);
#14318=ADVANCED_FACE('',(#890),#13639,.F.);
#14319=ADVANCED_FACE('',(#891),#439,.F.);
#14320=ADVANCED_FACE('',(#892),#440,.F.);
#14321=ADVANCED_FACE('',(#893),#441,.F.);
#14322=ADVANCED_FACE('',(#894),#442,.F.);
#14323=ADVANCED_FACE('',(#895),#443,.T.);
#14324=ADVANCED_FACE('',(#896),#13640,.F.);
#14325=ADVANCED_FACE('',(#897),#282,.F.);
#14326=ADVANCED_FACE('',(#898),#283,.F.);
#14327=ADVANCED_FACE('',(#899),#13641,.F.);
#14328=ADVANCED_FACE('',(#900),#444,.T.);
#14329=ADVANCED_FACE('',(#901),#13642,.F.);
#14330=ADVANCED_FACE('',(#902),#284,.F.);
#14331=ADVANCED_FACE('',(#903),#285,.F.);
#14332=ADVANCED_FACE('',(#904),#13643,.F.);
#14333=ADVANCED_FACE('',(#905),#445,.T.);
#14334=ADVANCED_FACE('',(#906),#13644,.F.);
#14335=ADVANCED_FACE('',(#907),#286,.F.);
#14336=ADVANCED_FACE('',(#908),#287,.F.);
#14337=ADVANCED_FACE('',(#909),#13645,.F.);
#14338=ADVANCED_FACE('',(#910),#446,.T.);
#14339=ADVANCED_FACE('',(#911),#13646,.F.);
#14340=ADVANCED_FACE('',(#912),#288,.F.);
#14341=ADVANCED_FACE('',(#913),#289,.F.);
#14342=ADVANCED_FACE('',(#914),#13647,.F.);
#14343=ADVANCED_FACE('',(#915),#13648,.T.);
#14344=ADVANCED_FACE('',(#916,#328),#447,.T.);
#14345=ADVANCED_FACE('',(#917),#13649,.F.);
#14346=ADVANCED_FACE('',(#918),#13650,.T.);
#14347=ADVANCED_FACE('',(#919,#329,#330,#331,#332,#333),#448,.T.);
#14348=ADVANCED_FACE('',(#920,#334,#335,#336,#337,#338,#339,#340,#341,#342),
#449,.F.);
#14349=ADVANCED_FACE('',(#921),#13651,.F.);
#14350=ADVANCED_FACE('',(#922),#13652,.F.);
#14351=ADVANCED_FACE('',(#923),#13653,.F.);
#14352=ADVANCED_FACE('',(#924),#13654,.F.);
#14353=ADVANCED_FACE('',(#925),#13655,.F.);
#14354=ADVANCED_FACE('',(#926),#13656,.F.);
#14355=ADVANCED_FACE('',(#927),#13657,.F.);
#14356=ADVANCED_FACE('',(#928),#13658,.F.);
#14357=ADVANCED_FACE('',(#929),#13659,.F.);
#14358=ADVANCED_FACE('',(#930),#13660,.F.);
#14359=ADVANCED_FACE('',(#931),#13661,.F.);
#14360=ADVANCED_FACE('',(#932),#13662,.F.);
#14361=ADVANCED_FACE('',(#933),#13663,.F.);
#14362=ADVANCED_FACE('',(#934),#13664,.F.);
#14363=ADVANCED_FACE('',(#935),#13665,.F.);
#14364=ADVANCED_FACE('',(#936),#13666,.F.);
#14365=ADVANCED_FACE('',(#937),#13667,.F.);
#14366=ADVANCED_FACE('',(#938),#13668,.F.);
#14367=ADVANCED_FACE('',(#939),#13669,.F.);
#14368=ADVANCED_FACE('',(#940),#13670,.F.);
#14369=ADVANCED_FACE('',(#941),#13671,.F.);
#14370=ADVANCED_FACE('',(#942),#13672,.F.);
#14371=ADVANCED_FACE('',(#943),#13673,.F.);
#14372=ADVANCED_FACE('',(#944),#13674,.F.);
#14373=ADVANCED_FACE('',(#945),#13675,.F.);
#14374=ADVANCED_FACE('',(#946),#13676,.F.);
#14375=ADVANCED_FACE('',(#947),#13677,.F.);
#14376=ADVANCED_FACE('',(#948),#13678,.F.);
#14377=ADVANCED_FACE('',(#949),#13679,.F.);
#14378=ADVANCED_FACE('',(#950),#13680,.F.);
#14379=ADVANCED_FACE('',(#951),#13681,.F.);
#14380=ADVANCED_FACE('',(#952),#13682,.F.);
#14381=ADVANCED_FACE('',(#953),#13683,.F.);
#14382=ADVANCED_FACE('',(#954),#13684,.F.);
#14383=ADVANCED_FACE('',(#955),#13685,.F.);
#14384=ADVANCED_FACE('',(#956),#13686,.F.);
#14385=ADVANCED_FACE('',(#957),#13687,.F.);
#14386=ADVANCED_FACE('',(#958),#13688,.F.);
#14387=ADVANCED_FACE('',(#959),#13689,.F.);
#14388=ADVANCED_FACE('',(#960),#13690,.F.);
#14389=ADVANCED_FACE('',(#961),#13691,.F.);
#14390=ADVANCED_FACE('',(#962),#13692,.F.);
#14391=ADVANCED_FACE('',(#963),#13693,.F.);
#14392=ADVANCED_FACE('',(#964),#13694,.F.);
#14393=ADVANCED_FACE('',(#965),#13695,.F.);
#14394=ADVANCED_FACE('',(#966),#13696,.F.);
#14395=ADVANCED_FACE('',(#967),#13697,.F.);
#14396=ADVANCED_FACE('',(#968),#13698,.F.);
#14397=ADVANCED_FACE('',(#969),#13699,.F.);
#14398=ADVANCED_FACE('',(#970),#13700,.F.);
#14399=ADVANCED_FACE('',(#971),#13701,.F.);
#14400=ADVANCED_FACE('',(#972),#13702,.F.);
#14401=ADVANCED_FACE('',(#973),#13703,.F.);
#14402=ADVANCED_FACE('',(#974),#13704,.F.);
#14403=ADVANCED_FACE('',(#975),#13705,.F.);
#14404=ADVANCED_FACE('',(#976),#13706,.F.);
#14405=ADVANCED_FACE('',(#977),#13707,.F.);
#14406=ADVANCED_FACE('',(#978),#13708,.F.);
#14407=ADVANCED_FACE('',(#979),#290,.F.);
#14408=ADVANCED_FACE('',(#980),#291,.F.);
#14409=ADVANCED_FACE('',(#981,#343),#450,.T.);
#14410=ADVANCED_FACE('',(#982),#13709,.F.);
#14411=ADVANCED_FACE('',(#983),#451,.T.);
#14412=ADVANCED_FACE('',(#984),#452,.T.);
#14413=ADVANCED_FACE('',(#985),#453,.T.);
#14414=ADVANCED_FACE('',(#986),#454,.T.);
#14415=ADVANCED_FACE('',(#987),#455,.T.);
#14416=ADVANCED_FACE('',(#988),#456,.T.);
#14417=ADVANCED_FACE('',(#989),#457,.T.);
#14418=ADVANCED_FACE('',(#990),#458,.T.);
#14419=ADVANCED_FACE('',(#991),#459,.T.);
#14420=ADVANCED_FACE('',(#992,#344),#460,.T.);
#14421=ADVANCED_FACE('',(#993),#461,.F.);
#14422=ADVANCED_FACE('',(#994),#13710,.F.);
#14423=ADVANCED_FACE('',(#995),#13711,.F.);
#14424=ADVANCED_FACE('',(#996),#13712,.F.);
#14425=ADVANCED_FACE('',(#997),#13713,.F.);
#14426=ADVANCED_FACE('',(#998,#345),#462,.F.);
#14427=ADVANCED_FACE('',(#999),#463,.T.);
#14428=ADVANCED_FACE('',(#1000),#464,.T.);
#14429=ADVANCED_FACE('',(#1001),#465,.F.);
#14430=ADVANCED_FACE('',(#1002,#346),#466,.F.);
#14431=ADVANCED_FACE('',(#1003),#13714,.F.);
#14432=ADVANCED_FACE('',(#1004,#347,#348),#467,.F.);
#14433=ADVANCED_FACE('',(#1005),#13715,.F.);
#14434=ADVANCED_FACE('',(#1006),#468,.F.);
#14435=ADVANCED_FACE('',(#1007),#469,.F.);
#14436=ADVANCED_FACE('',(#1008),#470,.F.);
#14437=ADVANCED_FACE('',(#1009),#471,.F.);
#14438=ADVANCED_FACE('',(#1010),#472,.F.);
#14439=ADVANCED_FACE('',(#1011),#473,.F.);
#14440=ADVANCED_FACE('',(#1012),#474,.F.);
#14441=ADVANCED_FACE('',(#1013),#475,.T.);
#14442=ADVANCED_FACE('',(#1014),#476,.T.);
#14443=ADVANCED_FACE('',(#1015),#477,.T.);
#14444=ADVANCED_FACE('',(#1016,#349,#350),#478,.T.);
#14445=ADVANCED_FACE('',(#1017),#13716,.T.);
#14446=ADVANCED_FACE('',(#1018),#13717,.T.);
#14447=ADVANCED_FACE('',(#1019),#13718,.T.);
#14448=ADVANCED_FACE('',(#1020),#13719,.T.);
#14449=ADVANCED_FACE('',(#1021),#13720,.T.);
#14450=ADVANCED_FACE('',(#1022),#13721,.T.);
#14451=ADVANCED_FACE('',(#1023),#13722,.T.);
#14452=ADVANCED_FACE('',(#1024),#13723,.T.);
#14453=ADVANCED_FACE('',(#1025),#13724,.T.);
#14454=ADVANCED_FACE('',(#1026),#13725,.T.);
#14455=ADVANCED_FACE('',(#1027),#13726,.T.);
#14456=ADVANCED_FACE('',(#1028),#13727,.T.);
#14457=ADVANCED_FACE('',(#1029),#13728,.T.);
#14458=ADVANCED_FACE('',(#1030),#13729,.T.);
#14459=ADVANCED_FACE('',(#1031),#13730,.T.);
#14460=ADVANCED_FACE('',(#1032),#13731,.T.);
#14461=ADVANCED_FACE('',(#1033),#13732,.T.);
#14462=ADVANCED_FACE('',(#1034),#13733,.T.);
#14463=ADVANCED_FACE('',(#1035),#13734,.T.);
#14464=ADVANCED_FACE('',(#1036),#13735,.T.);
#14465=ADVANCED_FACE('',(#1037),#13736,.T.);
#14466=ADVANCED_FACE('',(#1038),#13737,.T.);
#14467=ADVANCED_FACE('',(#1039),#13738,.T.);
#14468=ADVANCED_FACE('',(#1040),#13739,.T.);
#14469=ADVANCED_FACE('',(#1041),#13740,.T.);
#14470=ADVANCED_FACE('',(#1042),#13741,.T.);
#14471=ADVANCED_FACE('',(#1043),#13742,.T.);
#14472=ADVANCED_FACE('',(#1044),#13743,.T.);
#14473=ADVANCED_FACE('',(#1045),#13744,.T.);
#14474=ADVANCED_FACE('',(#1046),#13745,.T.);
#14475=ADVANCED_FACE('',(#1047),#13746,.T.);
#14476=ADVANCED_FACE('',(#1048),#13747,.T.);
#14477=ADVANCED_FACE('',(#1049),#13748,.T.);
#14478=ADVANCED_FACE('',(#1050),#13749,.T.);
#14479=ADVANCED_FACE('',(#1051),#13750,.T.);
#14480=ADVANCED_FACE('',(#1052),#13751,.T.);
#14481=ADVANCED_FACE('',(#1053),#13752,.T.);
#14482=ADVANCED_FACE('',(#1054),#13753,.T.);
#14483=ADVANCED_FACE('',(#1055),#13754,.T.);
#14484=ADVANCED_FACE('',(#1056),#13755,.T.);
#14485=ADVANCED_FACE('',(#1057),#13756,.T.);
#14486=ADVANCED_FACE('',(#1058),#13757,.T.);
#14487=ADVANCED_FACE('',(#1059),#13758,.T.);
#14488=ADVANCED_FACE('',(#1060),#13759,.T.);
#14489=ADVANCED_FACE('',(#1061),#13760,.T.);
#14490=ADVANCED_FACE('',(#1062),#13761,.T.);
#14491=ADVANCED_FACE('',(#1063),#13762,.T.);
#14492=ADVANCED_FACE('',(#1064),#13763,.T.);
#14493=ADVANCED_FACE('',(#1065),#13764,.T.);
#14494=ADVANCED_FACE('',(#1066),#13765,.T.);
#14495=ADVANCED_FACE('',(#1067),#13766,.T.);
#14496=ADVANCED_FACE('',(#1068),#13767,.T.);
#14497=ADVANCED_FACE('',(#1069),#13768,.T.);
#14498=ADVANCED_FACE('',(#1070),#13769,.T.);
#14499=ADVANCED_FACE('',(#1071),#13770,.T.);
#14500=ADVANCED_FACE('',(#1072),#13771,.T.);
#14501=ADVANCED_FACE('',(#1073),#13772,.T.);
#14502=ADVANCED_FACE('',(#1074),#13773,.T.);
#14503=ADVANCED_FACE('',(#1075),#13774,.T.);
#14504=ADVANCED_FACE('',(#1076),#13775,.T.);
#14505=ADVANCED_FACE('',(#1077),#13776,.T.);
#14506=ADVANCED_FACE('',(#1078),#13777,.T.);
#14507=ADVANCED_FACE('',(#1079),#13778,.T.);
#14508=ADVANCED_FACE('',(#1080),#13779,.T.);
#14509=ADVANCED_FACE('',(#1081),#13780,.T.);
#14510=ADVANCED_FACE('',(#1082),#13781,.T.);
#14511=ADVANCED_FACE('',(#1083),#13782,.T.);
#14512=ADVANCED_FACE('',(#1084),#13783,.T.);
#14513=ADVANCED_FACE('',(#1085),#13784,.T.);
#14514=ADVANCED_FACE('',(#1086),#13785,.T.);
#14515=ADVANCED_FACE('',(#1087),#13786,.T.);
#14516=ADVANCED_FACE('',(#1088),#13787,.T.);
#14517=ADVANCED_FACE('',(#1089),#13788,.T.);
#14518=ADVANCED_FACE('',(#1090),#479,.F.);
#14519=ADVANCED_FACE('',(#1091),#480,.F.);
#14520=ADVANCED_FACE('',(#1092),#481,.F.);
#14521=ADVANCED_FACE('',(#1093),#482,.F.);
#14522=ADVANCED_FACE('',(#1094),#483,.F.);
#14523=ADVANCED_FACE('',(#1095),#484,.F.);
#14524=ADVANCED_FACE('',(#1096),#485,.F.);
#14525=ADVANCED_FACE('',(#1097),#13789,.T.);
#14526=ADVANCED_FACE('',(#1098,#351),#486,.F.);
#14527=ADVANCED_FACE('',(#1099,#352),#487,.F.);
#14528=ADVANCED_FACE('',(#1100),#13790,.T.);
#14529=ADVANCED_FACE('',(#1101),#488,.F.);
#14530=ADVANCED_FACE('',(#1102),#292,.F.);
#14531=ADVANCED_FACE('',(#1103),#13791,.T.);
#14532=ADVANCED_FACE('',(#1104),#293,.F.);
#14533=ADVANCED_FACE('',(#1105),#13792,.T.);
#14534=ADVANCED_FACE('',(#1106,#353),#489,.F.);
#14535=ADVANCED_FACE('',(#1107),#13793,.T.);
#14536=ADVANCED_FACE('',(#1108,#354),#490,.T.);
#14537=ADVANCED_FACE('',(#1109),#491,.F.);
#14538=ADVANCED_FACE('',(#1110),#492,.F.);
#14539=ADVANCED_FACE('',(#1111),#493,.F.);
#14540=ADVANCED_FACE('',(#1112),#494,.F.);
#14541=ADVANCED_FACE('',(#1113),#13794,.F.);
#14542=ADVANCED_FACE('',(#1114),#13795,.T.);
#14543=ADVANCED_FACE('',(#1115),#495,.T.);
#14544=ADVANCED_FACE('',(#1116),#13796,.F.);
#14545=ADVANCED_FACE('',(#1117),#13797,.T.);
#14546=ADVANCED_FACE('',(#1118,#355),#496,.T.);
#14547=ADVANCED_FACE('',(#1119,#356),#497,.F.);
#14548=ADVANCED_FACE('',(#1120),#13798,.F.);
#14549=ADVANCED_FACE('',(#1121),#13799,.T.);
#14550=ADVANCED_FACE('',(#1122,#357),#498,.T.);
#14551=ADVANCED_FACE('',(#1123,#358),#499,.F.);
#14552=ADVANCED_FACE('',(#1124),#13800,.T.);
#14553=ADVANCED_FACE('',(#1125),#13801,.T.);
#14554=ADVANCED_FACE('',(#1126),#13802,.T.);
#14555=ADVANCED_FACE('',(#1127),#13803,.T.);
#14556=ADVANCED_FACE('',(#1128),#13804,.T.);
#14557=ADVANCED_FACE('',(#1129),#13805,.T.);
#14558=ADVANCED_FACE('',(#1130),#13806,.T.);
#14559=ADVANCED_FACE('',(#1131),#13807,.T.);
#14560=ADVANCED_FACE('',(#1132),#13808,.T.);
#14561=ADVANCED_FACE('',(#1133),#13809,.T.);
#14562=ADVANCED_FACE('',(#1134),#13810,.T.);
#14563=ADVANCED_FACE('',(#1135),#13811,.T.);
#14564=ADVANCED_FACE('',(#1136),#13812,.T.);
#14565=ADVANCED_FACE('',(#1137),#13813,.T.);
#14566=ADVANCED_FACE('',(#1138),#13814,.T.);
#14567=ADVANCED_FACE('',(#1139),#13815,.T.);
#14568=ADVANCED_FACE('',(#1140),#13816,.T.);
#14569=ADVANCED_FACE('',(#1141),#13817,.T.);
#14570=ADVANCED_FACE('',(#1142),#13818,.T.);
#14571=ADVANCED_FACE('',(#1143),#13819,.T.);
#14572=ADVANCED_FACE('',(#1144),#13820,.T.);
#14573=ADVANCED_FACE('',(#1145),#13821,.T.);
#14574=ADVANCED_FACE('',(#1146),#13822,.T.);
#14575=ADVANCED_FACE('',(#1147),#13823,.T.);
#14576=ADVANCED_FACE('',(#1148),#13824,.T.);
#14577=ADVANCED_FACE('',(#1149),#13825,.T.);
#14578=ADVANCED_FACE('',(#1150),#13826,.T.);
#14579=ADVANCED_FACE('',(#1151),#13827,.T.);
#14580=ADVANCED_FACE('',(#1152),#13828,.T.);
#14581=ADVANCED_FACE('',(#1153),#13829,.T.);
#14582=ADVANCED_FACE('',(#1154),#13830,.T.);
#14583=ADVANCED_FACE('',(#1155),#13831,.T.);
#14584=ADVANCED_FACE('',(#1156),#13832,.T.);
#14585=ADVANCED_FACE('',(#1157),#13833,.T.);
#14586=ADVANCED_FACE('',(#1158),#13834,.T.);
#14587=ADVANCED_FACE('',(#1159),#13835,.T.);
#14588=ADVANCED_FACE('',(#1160),#13836,.T.);
#14589=ADVANCED_FACE('',(#1161),#13837,.T.);
#14590=ADVANCED_FACE('',(#1162),#13838,.T.);
#14591=ADVANCED_FACE('',(#1163),#13839,.T.);
#14592=ADVANCED_FACE('',(#1164),#13840,.T.);
#14593=ADVANCED_FACE('',(#1165),#13841,.T.);
#14594=ADVANCED_FACE('',(#1166),#13842,.T.);
#14595=ADVANCED_FACE('',(#1167),#13843,.T.);
#14596=ADVANCED_FACE('',(#1168),#13844,.T.);
#14597=ADVANCED_FACE('',(#1169),#13845,.T.);
#14598=ADVANCED_FACE('',(#1170),#13846,.T.);
#14599=ADVANCED_FACE('',(#1171),#13847,.T.);
#14600=ADVANCED_FACE('',(#1172),#13848,.T.);
#14601=ADVANCED_FACE('',(#1173),#13849,.T.);
#14602=ADVANCED_FACE('',(#1174),#13850,.T.);
#14603=ADVANCED_FACE('',(#1175),#13851,.T.);
#14604=ADVANCED_FACE('',(#1176),#13852,.T.);
#14605=ADVANCED_FACE('',(#1177),#13853,.T.);
#14606=ADVANCED_FACE('',(#1178),#13854,.T.);
#14607=ADVANCED_FACE('',(#1179),#13855,.T.);
#14608=ADVANCED_FACE('',(#1180),#13856,.T.);
#14609=ADVANCED_FACE('',(#1181),#13857,.T.);
#14610=ADVANCED_FACE('',(#1182),#13858,.T.);
#14611=ADVANCED_FACE('',(#1183),#13859,.T.);
#14612=ADVANCED_FACE('',(#1184),#13860,.T.);
#14613=ADVANCED_FACE('',(#1185),#13861,.T.);
#14614=ADVANCED_FACE('',(#1186),#13862,.T.);
#14615=ADVANCED_FACE('',(#1187),#13863,.T.);
#14616=ADVANCED_FACE('',(#1188),#13864,.T.);
#14617=ADVANCED_FACE('',(#1189),#13865,.T.);
#14618=ADVANCED_FACE('',(#1190),#13866,.T.);
#14619=ADVANCED_FACE('',(#1191),#13867,.T.);
#14620=ADVANCED_FACE('',(#1192),#13868,.T.);
#14621=ADVANCED_FACE('',(#1193),#13869,.T.);
#14622=ADVANCED_FACE('',(#1194),#13870,.T.);
#14623=ADVANCED_FACE('',(#1195),#13871,.T.);
#14624=ADVANCED_FACE('',(#1196),#13872,.T.);
#14625=ADVANCED_FACE('',(#1197),#13873,.T.);
#14626=ADVANCED_FACE('',(#1198),#13874,.T.);
#14627=ADVANCED_FACE('',(#1199),#13875,.T.);
#14628=ADVANCED_FACE('',(#1200),#13876,.T.);
#14629=ADVANCED_FACE('',(#1201),#13877,.T.);
#14630=ADVANCED_FACE('',(#1202),#211,.T.);
#14631=ADVANCED_FACE('',(#1203),#294,.F.);
#14632=ADVANCED_FACE('',(#1204),#13878,.T.);
#14633=ADVANCED_FACE('',(#1205),#295,.F.);
#14634=ADVANCED_FACE('',(#1206),#13879,.T.);
#14635=ADVANCED_FACE('',(#1207),#500,.F.);
#14636=ADVANCED_FACE('',(#1208),#501,.F.);
#14637=ADVANCED_FACE('',(#1209),#502,.F.);
#14638=ADVANCED_FACE('',(#1210),#503,.F.);
#14639=ADVANCED_FACE('',(#1211),#504,.F.);
#14640=ADVANCED_FACE('',(#1212),#505,.F.);
#14641=ADVANCED_FACE('',(#1213),#506,.F.);
#14642=ADVANCED_FACE('',(#1214,#359),#507,.T.);
#14643=ADVANCED_FACE('',(#1215),#13880,.T.);
#14644=ADVANCED_FACE('',(#1216,#360),#508,.F.);
#14645=ADVANCED_FACE('',(#1217),#509,.T.);
#14646=ADVANCED_FACE('',(#1218),#13881,.F.);
#14647=ADVANCED_FACE('',(#1219),#13882,.T.);
#14648=ADVANCED_FACE('',(#1220,#361),#510,.T.);
#14649=ADVANCED_FACE('',(#1221,#362),#511,.F.);
#14650=ADVANCED_FACE('',(#1222),#13883,.T.);
#14651=ADVANCED_FACE('',(#1223),#13884,.T.);
#14652=ADVANCED_FACE('',(#1224),#13885,.T.);
#14653=ADVANCED_FACE('',(#1225),#13886,.T.);
#14654=ADVANCED_FACE('',(#1226),#13887,.T.);
#14655=ADVANCED_FACE('',(#1227),#13888,.T.);
#14656=ADVANCED_FACE('',(#1228),#13889,.T.);
#14657=ADVANCED_FACE('',(#1229),#13890,.T.);
#14658=ADVANCED_FACE('',(#1230),#13891,.T.);
#14659=ADVANCED_FACE('',(#1231),#13892,.T.);
#14660=ADVANCED_FACE('',(#1232),#13893,.T.);
#14661=ADVANCED_FACE('',(#1233),#13894,.T.);
#14662=ADVANCED_FACE('',(#1234),#13895,.T.);
#14663=ADVANCED_FACE('',(#1235),#13896,.T.);
#14664=ADVANCED_FACE('',(#1236),#13897,.T.);
#14665=ADVANCED_FACE('',(#1237),#13898,.T.);
#14666=ADVANCED_FACE('',(#1238),#13899,.T.);
#14667=ADVANCED_FACE('',(#1239),#13900,.T.);
#14668=ADVANCED_FACE('',(#1240),#13901,.T.);
#14669=ADVANCED_FACE('',(#1241),#13902,.T.);
#14670=ADVANCED_FACE('',(#1242),#13903,.T.);
#14671=ADVANCED_FACE('',(#1243),#13904,.T.);
#14672=ADVANCED_FACE('',(#1244),#13905,.T.);
#14673=ADVANCED_FACE('',(#1245),#13906,.T.);
#14674=ADVANCED_FACE('',(#1246),#13907,.T.);
#14675=ADVANCED_FACE('',(#1247),#13908,.T.);
#14676=ADVANCED_FACE('',(#1248),#13909,.T.);
#14677=ADVANCED_FACE('',(#1249),#13910,.T.);
#14678=ADVANCED_FACE('',(#1250),#13911,.T.);
#14679=ADVANCED_FACE('',(#1251),#13912,.T.);
#14680=ADVANCED_FACE('',(#1252),#13913,.T.);
#14681=ADVANCED_FACE('',(#1253),#13914,.T.);
#14682=ADVANCED_FACE('',(#1254),#13915,.T.);
#14683=ADVANCED_FACE('',(#1255),#13916,.T.);
#14684=ADVANCED_FACE('',(#1256),#13917,.T.);
#14685=ADVANCED_FACE('',(#1257),#13918,.T.);
#14686=ADVANCED_FACE('',(#1258),#13919,.T.);
#14687=ADVANCED_FACE('',(#1259),#13920,.T.);
#14688=ADVANCED_FACE('',(#1260),#13921,.T.);
#14689=ADVANCED_FACE('',(#1261),#13922,.T.);
#14690=ADVANCED_FACE('',(#1262),#13923,.T.);
#14691=ADVANCED_FACE('',(#1263),#13924,.T.);
#14692=ADVANCED_FACE('',(#1264),#13925,.T.);
#14693=ADVANCED_FACE('',(#1265),#13926,.T.);
#14694=ADVANCED_FACE('',(#1266),#13927,.T.);
#14695=ADVANCED_FACE('',(#1267),#13928,.T.);
#14696=ADVANCED_FACE('',(#1268),#13929,.T.);
#14697=ADVANCED_FACE('',(#1269),#13930,.T.);
#14698=ADVANCED_FACE('',(#1270),#13931,.T.);
#14699=ADVANCED_FACE('',(#1271),#13932,.T.);
#14700=ADVANCED_FACE('',(#1272),#13933,.T.);
#14701=ADVANCED_FACE('',(#1273),#13934,.T.);
#14702=ADVANCED_FACE('',(#1274),#13935,.T.);
#14703=ADVANCED_FACE('',(#1275),#13936,.T.);
#14704=ADVANCED_FACE('',(#1276),#13937,.T.);
#14705=ADVANCED_FACE('',(#1277),#13938,.T.);
#14706=ADVANCED_FACE('',(#1278),#13939,.T.);
#14707=ADVANCED_FACE('',(#1279),#13940,.T.);
#14708=ADVANCED_FACE('',(#1280),#13941,.T.);
#14709=ADVANCED_FACE('',(#1281),#13942,.T.);
#14710=ADVANCED_FACE('',(#1282),#13943,.T.);
#14711=ADVANCED_FACE('',(#1283),#13944,.T.);
#14712=ADVANCED_FACE('',(#1284),#13945,.T.);
#14713=ADVANCED_FACE('',(#1285),#13946,.T.);
#14714=ADVANCED_FACE('',(#1286),#212,.T.);
#14715=ADVANCED_FACE('',(#1287),#213,.T.);
#14716=ADVANCED_FACE('',(#1288),#296,.F.);
#14717=ADVANCED_FACE('',(#1289),#13947,.T.);
#14718=ADVANCED_FACE('',(#1290),#297,.F.);
#14719=ADVANCED_FACE('',(#1291),#13948,.T.);
#14720=ADVANCED_FACE('',(#1292),#512,.F.);
#14721=ADVANCED_FACE('',(#1293),#513,.F.);
#14722=ADVANCED_FACE('',(#1294),#514,.F.);
#14723=ADVANCED_FACE('',(#1295),#515,.F.);
#14724=ADVANCED_FACE('',(#1296),#516,.F.);
#14725=ADVANCED_FACE('',(#1297),#517,.F.);
#14726=ADVANCED_FACE('',(#1298),#518,.F.);
#14727=ADVANCED_FACE('',(#1299,#363),#519,.T.);
#14728=ADVANCED_FACE('',(#1300),#13949,.T.);
#14729=ADVANCED_FACE('',(#1301,#364),#520,.F.);
#14730=ADVANCED_FACE('',(#1302),#521,.T.);
#14731=CLOSED_SHELL('',(#13950,#13951,#13952,#13953,#13954,#13955,#13956,
#13957,#13958,#13959,#13960,#13961,#13962,#13963,#13964,#13965,#13966,#13967,
#13968,#13969,#13970,#13971,#13972,#13973,#13974,#13975,#13976,#13977,#13978,
#13979,#13980,#13981,#13982,#13983,#13984,#13985,#13986,#13987,#13988,#13989,
#13990,#13991,#13992,#13993,#13994,#13995,#13996,#13997,#13998,#13999,#14000,
#14001,#14002,#14003,#14004,#14005,#14006,#14007,#14008,#14009,#14010,#14011,
#14012,#14013,#14014,#14015,#14016,#14017,#14018,#14019,#14020,#14021,#14022,
#14023,#14024,#14025,#14026,#14027,#14028,#14029,#14030,#14031,#14032,#14033,
#14034,#14035,#14036,#14037,#14038,#14039,#14040,#14041,#14042,#14043,#14044,
#14045,#14046,#14047,#14048,#14049,#14050,#14051,#14052,#14053,#14054,#14055,
#14056,#14057,#14058,#14059,#14060,#14061,#14062,#14063,#14064,#14065,#14066,
#14067,#14068,#14069,#14070,#14071,#14072,#14073,#14074,#14075,#14076,#14077,
#14078,#14079,#14080,#14081,#14082,#14083,#14084,#14085,#14086,#14087,#14088,
#14089,#14090,#14091,#14092,#14093,#14094,#14095,#14096,#14097,#14098,#14099,
#14100,#14101,#14102,#14103,#14104,#14105,#14106,#14107,#14108,#14109,#14110,
#14111,#14112,#14113,#14114,#14115,#14116,#14117,#14118,#14119,#14120,#14121,
#14122,#14123,#14124,#14125,#14126,#14127,#14128,#14129,#14130,#14131,#14132,
#14133,#14134,#14135,#14136,#14137,#14138,#14139,#14140,#14141,#14142,#14143,
#14144,#14145,#14146,#14147,#14148,#14149,#14150,#14151,#14152,#14153,#14154,
#14155,#14156,#14157,#14158,#14159,#14160,#14161,#14162,#14163,#14164,#14165,
#14166,#14167,#14168,#14169,#14170,#14171,#14172,#14173,#14174,#14175,#14176,
#14177,#14178,#14179,#14180,#14181,#14182,#14183,#14184,#14185,#14186,#14187,
#14188,#14189,#14190,#14191,#14192,#14193,#14194,#14195,#14196,#14197,#14198,
#14199,#14200,#14201,#14202,#14203,#14204,#14205,#14206));
#14732=CLOSED_SHELL('',(#14207,#14208,#14209,#14210,#14211,#14212,#14213,
#14214,#14215,#14216,#14217,#14218,#14219,#14220,#14221,#14222,#14223,#14224,
#14225,#14226,#14227,#14228,#14229,#14230,#14231,#14232,#14233,#14234,#14235,
#14236,#14237,#14238,#14239,#14240,#14241,#14242,#14243,#14244,#14245,#14246,
#14247,#14248,#14249,#14250,#14251,#14252,#14253,#14254,#14255,#14256,#14257,
#14258,#14259,#14260,#14261,#14262,#14263,#14264,#14265,#14266,#14267,#14268,
#14269,#14270,#14271,#14272,#14273,#14274,#14275,#14276,#14277,#14278,#14279,
#14280,#14281,#14282,#14283,#14284,#14285,#14286,#14287,#14288,#14289,#14290,
#14291,#14292,#14293,#14294,#14295,#14296,#14297,#14298,#14299,#14300,#14301,
#14302,#14303,#14304,#14305,#14306,#14307,#14308,#14309,#14310,#14311,#14312,
#14313,#14314,#14315,#14316,#14317,#14318,#14319,#14320,#14321,#14322,#14323,
#14324,#14325,#14326,#14327,#14328,#14329,#14330,#14331,#14332,#14333,#14334,
#14335,#14336,#14337,#14338,#14339,#14340,#14341,#14342,#14343,#14344,#14345,
#14346,#14347,#14348));
#14733=CLOSED_SHELL('',(#14349,#14350,#14351,#14352,#14353,#14354,#14355,
#14356,#14357,#14358,#14359,#14360,#14361,#14362,#14363,#14364,#14365,#14366,
#14367,#14368,#14369,#14370,#14371,#14372,#14373,#14374,#14375,#14376,#14377,
#14378,#14379,#14380,#14381,#14382,#14383,#14384,#14385,#14386,#14387,#14388,
#14389,#14390,#14391,#14392,#14393,#14394,#14395,#14396,#14397,#14398,#14399,
#14400,#14401,#14402,#14403,#14404,#14405,#14406,#14407,#14408,#14409,#14410,
#14411,#14412,#14413,#14414,#14415,#14416,#14417,#14418,#14419,#14420,#14421));
#14734=CLOSED_SHELL('',(#14422,#14423,#14424,#14425,#14426,#14427,#14428,
#14429,#14430,#14431,#14432,#14433,#14434,#14435,#14436,#14437,#14438,#14439,
#14440,#14441,#14442,#14443,#14444));
#14735=CLOSED_SHELL('',(#14445,#14446,#14447,#14448,#14449,#14450,#14451,
#14452,#14453,#14454,#14455,#14456,#14457,#14458,#14459,#14460,#14461,#14462,
#14463,#14464,#14465,#14466,#14467,#14468,#14469,#14470,#14471,#14472,#14473,
#14474,#14475,#14476,#14477,#14478,#14479,#14480,#14481,#14482,#14483,#14484,
#14485,#14486,#14487,#14488,#14489,#14490,#14491,#14492,#14493,#14494,#14495,
#14496,#14497,#14498,#14499,#14500,#14501,#14502,#14503,#14504,#14505,#14506,
#14507,#14508,#14509,#14510,#14511,#14512,#14513,#14514,#14515,#14516,#14517,
#14518,#14519,#14520,#14521,#14522,#14523,#14524,#14525,#14526,#14527,#14528,
#14529,#14530,#14531,#14532,#14533,#14534,#14535,#14536,#14537));
#14736=CLOSED_SHELL('',(#14538,#14539,#14540,#14541,#14542,#14543));
#14737=CLOSED_SHELL('',(#14544,#14545,#14546,#14547));
#14738=CLOSED_SHELL('',(#14548,#14549,#14550,#14551));
#14739=CLOSED_SHELL('',(#14552,#14553,#14554,#14555,#14556,#14557,#14558,
#14559,#14560,#14561,#14562,#14563,#14564,#14565,#14566,#14567,#14568,#14569,
#14570,#14571,#14572,#14573,#14574,#14575,#14576,#14577,#14578,#14579,#14580,
#14581,#14582,#14583,#14584,#14585,#14586,#14587,#14588,#14589,#14590,#14591,
#14592,#14593,#14594,#14595,#14596,#14597,#14598,#14599,#14600,#14601,#14602,
#14603,#14604,#14605,#14606,#14607,#14608,#14609,#14610,#14611,#14612,#14613,
#14614,#14615,#14616,#14617,#14618,#14619,#14620,#14621,#14622,#14623,#14624,
#14625,#14626,#14627,#14628,#14629,#14630,#14631,#14632,#14633,#14634,#14635,
#14636,#14637,#14638,#14639,#14640,#14641,#14642,#14643,#14644,#14645));
#14740=CLOSED_SHELL('',(#14646,#14647,#14648,#14649));
#14741=CLOSED_SHELL('',(#14650,#14651,#14652,#14653,#14654,#14655,#14656,
#14657,#14658,#14659,#14660,#14661,#14662,#14663,#14664,#14665,#14666,#14667,
#14668,#14669,#14670,#14671,#14672,#14673,#14674,#14675,#14676,#14677,#14678,
#14679,#14680,#14681,#14682,#14683,#14684,#14685,#14686,#14687,#14688,#14689,
#14690,#14691,#14692,#14693,#14694,#14695,#14696,#14697,#14698,#14699,#14700,
#14701,#14702,#14703,#14704,#14705,#14706,#14707,#14708,#14709,#14710,#14711,
#14712,#14713,#14714,#14715,#14716,#14717,#14718,#14719,#14720,#14721,#14722,
#14723,#14724,#14725,#14726,#14727,#14728,#14729,#14730));
#14742=DERIVED_UNIT_ELEMENT(#14764,1.);
#14743=DERIVED_UNIT_ELEMENT(#69493,-3.);
#14744=DERIVED_UNIT_ELEMENT(#14764,1.);
#14745=DERIVED_UNIT_ELEMENT(#69493,-3.);
#14746=DERIVED_UNIT_ELEMENT(#14764,1.);
#14747=DERIVED_UNIT_ELEMENT(#69493,-3.);
#14748=DERIVED_UNIT_ELEMENT(#14764,1.);
#14749=DERIVED_UNIT_ELEMENT(#69493,-3.);
#14750=DERIVED_UNIT_ELEMENT(#14764,1.);
#14751=DERIVED_UNIT_ELEMENT(#69493,-3.);
#14752=DERIVED_UNIT_ELEMENT(#14764,1.);
#14753=DERIVED_UNIT_ELEMENT(#69493,-3.);
#14754=DERIVED_UNIT_ELEMENT(#14764,1.);
#14755=DERIVED_UNIT_ELEMENT(#69493,-3.);
#14756=DERIVED_UNIT_ELEMENT(#14764,1.);
#14757=DERIVED_UNIT_ELEMENT(#69493,-3.);
#14758=DERIVED_UNIT_ELEMENT(#14764,1.);
#14759=DERIVED_UNIT_ELEMENT(#69493,-3.);
#14760=DERIVED_UNIT_ELEMENT(#14764,1.);
#14761=DERIVED_UNIT_ELEMENT(#69493,-3.);
#14762=DERIVED_UNIT_ELEMENT(#14764,1.);
#14763=DERIVED_UNIT_ELEMENT(#69493,-3.);
#14764=(
MASS_UNIT()
NAMED_UNIT(*)
SI_UNIT(.KILO.,.GRAM.)
);
#14765=DERIVED_UNIT((#14742,#14743));
#14766=DERIVED_UNIT((#14744,#14745));
#14767=DERIVED_UNIT((#14746,#14747));
#14768=DERIVED_UNIT((#14748,#14749));
#14769=DERIVED_UNIT((#14750,#14751));
#14770=DERIVED_UNIT((#14752,#14753));
#14771=DERIVED_UNIT((#14754,#14755));
#14772=DERIVED_UNIT((#14756,#14757));
#14773=DERIVED_UNIT((#14758,#14759));
#14774=DERIVED_UNIT((#14760,#14761));
#14775=DERIVED_UNIT((#14762,#14763));
#14776=MEASURE_REPRESENTATION_ITEM('density measure',
POSITIVE_RATIO_MEASURE(7850.),#14765);
#14777=MEASURE_REPRESENTATION_ITEM('density measure',
POSITIVE_RATIO_MEASURE(7850.),#14766);
#14778=MEASURE_REPRESENTATION_ITEM('density measure',
POSITIVE_RATIO_MEASURE(7850.),#14767);
#14779=MEASURE_REPRESENTATION_ITEM('density measure',
POSITIVE_RATIO_MEASURE(7850.),#14768);
#14780=MEASURE_REPRESENTATION_ITEM('density measure',
POSITIVE_RATIO_MEASURE(7850.),#14769);
#14781=MEASURE_REPRESENTATION_ITEM('density measure',
POSITIVE_RATIO_MEASURE(7850.),#14770);
#14782=MEASURE_REPRESENTATION_ITEM('density measure',
POSITIVE_RATIO_MEASURE(8920.),#14771);
#14783=MEASURE_REPRESENTATION_ITEM('density measure',
POSITIVE_RATIO_MEASURE(8920.),#14772);
#14784=MEASURE_REPRESENTATION_ITEM('density measure',
POSITIVE_RATIO_MEASURE(7850.),#14773);
#14785=MEASURE_REPRESENTATION_ITEM('density measure',
POSITIVE_RATIO_MEASURE(7850.),#14774);
#14786=MEASURE_REPRESENTATION_ITEM('density measure',
POSITIVE_RATIO_MEASURE(7850.),#14775);
#14787=PROPERTY_DEFINITION_REPRESENTATION(#14842,#14809);
#14788=PROPERTY_DEFINITION_REPRESENTATION(#14843,#14810);
#14789=PROPERTY_DEFINITION_REPRESENTATION(#14844,#14811);
#14790=PROPERTY_DEFINITION_REPRESENTATION(#14845,#14812);
#14791=PROPERTY_DEFINITION_REPRESENTATION(#14846,#14813);
#14792=PROPERTY_DEFINITION_REPRESENTATION(#14847,#14814);
#14793=PROPERTY_DEFINITION_REPRESENTATION(#14848,#14815);
#14794=PROPERTY_DEFINITION_REPRESENTATION(#14849,#14816);
#14795=PROPERTY_DEFINITION_REPRESENTATION(#14850,#14817);
#14796=PROPERTY_DEFINITION_REPRESENTATION(#14851,#14818);
#14797=PROPERTY_DEFINITION_REPRESENTATION(#14852,#14819);
#14798=PROPERTY_DEFINITION_REPRESENTATION(#14853,#14820);
#14799=PROPERTY_DEFINITION_REPRESENTATION(#14854,#14821);
#14800=PROPERTY_DEFINITION_REPRESENTATION(#14855,#14822);
#14801=PROPERTY_DEFINITION_REPRESENTATION(#14856,#14823);
#14802=PROPERTY_DEFINITION_REPRESENTATION(#14857,#14824);
#14803=PROPERTY_DEFINITION_REPRESENTATION(#14858,#14825);
#14804=PROPERTY_DEFINITION_REPRESENTATION(#14859,#14826);
#14805=PROPERTY_DEFINITION_REPRESENTATION(#14860,#14827);
#14806=PROPERTY_DEFINITION_REPRESENTATION(#14861,#14828);
#14807=PROPERTY_DEFINITION_REPRESENTATION(#14862,#14829);
#14808=PROPERTY_DEFINITION_REPRESENTATION(#14863,#14830);
#14809=REPRESENTATION('material name',(#14831),#69480);
#14810=REPRESENTATION('density',(#14776),#69480);
#14811=REPRESENTATION('material name',(#14832),#69481);
#14812=REPRESENTATION('density',(#14777),#69481);
#14813=REPRESENTATION('material name',(#14833),#69482);
#14814=REPRESENTATION('density',(#14778),#69482);
#14815=REPRESENTATION('material name',(#14834),#69483);
#14816=REPRESENTATION('density',(#14779),#69483);
#14817=REPRESENTATION('material name',(#14835),#69484);
#14818=REPRESENTATION('density',(#14780),#69484);
#14819=REPRESENTATION('material name',(#14836),#69485);
#14820=REPRESENTATION('density',(#14781),#69485);
#14821=REPRESENTATION('material name',(#14837),#69486);
#14822=REPRESENTATION('density',(#14782),#69486);
#14823=REPRESENTATION('material name',(#14838),#69487);
#14824=REPRESENTATION('density',(#14783),#69487);
#14825=REPRESENTATION('material name',(#14839),#69488);
#14826=REPRESENTATION('density',(#14784),#69488);
#14827=REPRESENTATION('material name',(#14840),#69489);
#14828=REPRESENTATION('density',(#14785),#69489);
#14829=REPRESENTATION('material name',(#14841),#69490);
#14830=REPRESENTATION('density',(#14786),#69490);
#14831=DESCRIPTIVE_REPRESENTATION_ITEM('Steel','Steel');
#14832=DESCRIPTIVE_REPRESENTATION_ITEM('Steel','Steel');
#14833=DESCRIPTIVE_REPRESENTATION_ITEM('Steel','Steel');
#14834=DESCRIPTIVE_REPRESENTATION_ITEM('Steel','Steel');
#14835=DESCRIPTIVE_REPRESENTATION_ITEM('Steel','Steel');
#14836=DESCRIPTIVE_REPRESENTATION_ITEM('Steel','Steel');
#14837=DESCRIPTIVE_REPRESENTATION_ITEM('Copper, Alloy','Copper, Alloy');
#14838=DESCRIPTIVE_REPRESENTATION_ITEM('Copper, Alloy','Copper, Alloy');
#14839=DESCRIPTIVE_REPRESENTATION_ITEM('Steel','Steel');
#14840=DESCRIPTIVE_REPRESENTATION_ITEM('Steel','Steel');
#14841=DESCRIPTIVE_REPRESENTATION_ITEM('Steel','Steel');
#14842=PROPERTY_DEFINITION('material property','material name',#69584);
#14843=PROPERTY_DEFINITION('material property','density of part',#69584);
#14844=PROPERTY_DEFINITION('material property','material name',#69585);
#14845=PROPERTY_DEFINITION('material property','density of part',#69585);
#14846=PROPERTY_DEFINITION('material property','material name',#69586);
#14847=PROPERTY_DEFINITION('material property','density of part',#69586);
#14848=PROPERTY_DEFINITION('material property','material name',#69587);
#14849=PROPERTY_DEFINITION('material property','density of part',#69587);
#14850=PROPERTY_DEFINITION('material property','material name',#69588);
#14851=PROPERTY_DEFINITION('material property','density of part',#69588);
#14852=PROPERTY_DEFINITION('material property','material name',#69589);
#14853=PROPERTY_DEFINITION('material property','density of part',#69589);
#14854=PROPERTY_DEFINITION('material property','material name',#69590);
#14855=PROPERTY_DEFINITION('material property','density of part',#69590);
#14856=PROPERTY_DEFINITION('material property','material name',#69591);
#14857=PROPERTY_DEFINITION('material property','density of part',#69591);
#14858=PROPERTY_DEFINITION('material property','material name',#69592);
#14859=PROPERTY_DEFINITION('material property','density of part',#69592);
#14860=PROPERTY_DEFINITION('material property','material name',#69593);
#14861=PROPERTY_DEFINITION('material property','density of part',#69593);
#14862=PROPERTY_DEFINITION('material property','material name',#69594);
#14863=PROPERTY_DEFINITION('material property','density of part',#69594);
#14864=AXIS2_PLACEMENT_3D('',#18709,#15863,#15864);
#14865=AXIS2_PLACEMENT_3D('',#18710,#15865,#15866);
#14866=AXIS2_PLACEMENT_3D('',#18711,#15867,#15868);
#14867=AXIS2_PLACEMENT_3D('',#18721,#15870,#15871);
#14868=AXIS2_PLACEMENT_3D('',#18724,#15873,#15874);
#14869=AXIS2_PLACEMENT_3D('',#18726,#15875,#15876);
#14870=AXIS2_PLACEMENT_3D('',#18737,#15877,#15878);
#14871=AXIS2_PLACEMENT_3D('',#18788,#15880,#15881);
#14872=AXIS2_PLACEMENT_3D('',#18839,#15883,#15884);
#14873=AXIS2_PLACEMENT_3D('',#18887,#15886,#15887);
#14874=AXIS2_PLACEMENT_3D('',#18938,#15889,#15890);
#14875=AXIS2_PLACEMENT_3D('',#18989,#15892,#15893);
#14876=AXIS2_PLACEMENT_3D('',#19037,#15895,#15896);
#14877=AXIS2_PLACEMENT_3D('',#19088,#15898,#15899);
#14878=AXIS2_PLACEMENT_3D('',#19107,#15901,#15902);
#14879=AXIS2_PLACEMENT_3D('',#19127,#15903,#15904);
#14880=AXIS2_PLACEMENT_3D('',#19141,#15906,#15907);
#14881=AXIS2_PLACEMENT_3D('',#19151,#15908,#15909);
#14882=AXIS2_PLACEMENT_3D('',#19175,#15911,#15912);
#14883=AXIS2_PLACEMENT_3D('',#19200,#15914,#15915);
#14884=AXIS2_PLACEMENT_3D('',#19225,#15917,#15918);
#14885=AXIS2_PLACEMENT_3D('',#19249,#15920,#15921);
#14886=AXIS2_PLACEMENT_3D('',#19274,#15923,#15924);
#14887=AXIS2_PLACEMENT_3D('',#19299,#15926,#15927);
#14888=AXIS2_PLACEMENT_3D('',#19323,#15929,#15930);
#14889=AXIS2_PLACEMENT_3D('',#19334,#15932,#15933);
#14890=AXIS2_PLACEMENT_3D('',#19340,#15934,#15935);
#14891=AXIS2_PLACEMENT_3D('',#19350,#15937,#15938);
#14892=AXIS2_PLACEMENT_3D('',#19353,#15940,#15941);
#14893=AXIS2_PLACEMENT_3D('',#19355,#15942,#15943);
#14894=AXIS2_PLACEMENT_3D('',#19366,#15944,#15945);
#14895=AXIS2_PLACEMENT_3D('',#19417,#15947,#15948);
#14896=AXIS2_PLACEMENT_3D('',#19468,#15950,#15951);
#14897=AXIS2_PLACEMENT_3D('',#19516,#15953,#15954);
#14898=AXIS2_PLACEMENT_3D('',#19567,#15956,#15957);
#14899=AXIS2_PLACEMENT_3D('',#19618,#15959,#15960);
#14900=AXIS2_PLACEMENT_3D('',#19666,#15962,#15963);
#14901=AXIS2_PLACEMENT_3D('',#19717,#15965,#15966);
#14902=AXIS2_PLACEMENT_3D('',#19736,#15968,#15969);
#14903=AXIS2_PLACEMENT_3D('',#19756,#15970,#15971);
#14904=AXIS2_PLACEMENT_3D('',#19770,#15973,#15974);
#14905=AXIS2_PLACEMENT_3D('',#19780,#15975,#15976);
#14906=AXIS2_PLACEMENT_3D('',#19804,#15978,#15979);
#14907=AXIS2_PLACEMENT_3D('',#19829,#15981,#15982);
#14908=AXIS2_PLACEMENT_3D('',#19854,#15984,#15985);
#14909=AXIS2_PLACEMENT_3D('',#19878,#15987,#15988);
#14910=AXIS2_PLACEMENT_3D('',#19903,#15990,#15991);
#14911=AXIS2_PLACEMENT_3D('',#19928,#15993,#15994);
#14912=AXIS2_PLACEMENT_3D('',#19952,#15996,#15997);
#14913=AXIS2_PLACEMENT_3D('',#19963,#15999,#16000);
#14914=AXIS2_PLACEMENT_3D('',#19969,#16001,#16002);
#14915=AXIS2_PLACEMENT_3D('',#19979,#16004,#16005);
#14916=AXIS2_PLACEMENT_3D('',#19982,#16007,#16008);
#14917=AXIS2_PLACEMENT_3D('',#19984,#16009,#16010);
#14918=AXIS2_PLACEMENT_3D('',#19995,#16011,#16012);
#14919=AXIS2_PLACEMENT_3D('',#20046,#16014,#16015);
#14920=AXIS2_PLACEMENT_3D('',#20097,#16017,#16018);
#14921=AXIS2_PLACEMENT_3D('',#20145,#16020,#16021);
#14922=AXIS2_PLACEMENT_3D('',#20196,#16023,#16024);
#14923=AXIS2_PLACEMENT_3D('',#20247,#16026,#16027);
#14924=AXIS2_PLACEMENT_3D('',#20295,#16029,#16030);
#14925=AXIS2_PLACEMENT_3D('',#20346,#16032,#16033);
#14926=AXIS2_PLACEMENT_3D('',#20365,#16035,#16036);
#14927=AXIS2_PLACEMENT_3D('',#20385,#16037,#16038);
#14928=AXIS2_PLACEMENT_3D('',#20399,#16040,#16041);
#14929=AXIS2_PLACEMENT_3D('',#20409,#16042,#16043);
#14930=AXIS2_PLACEMENT_3D('',#20433,#16045,#16046);
#14931=AXIS2_PLACEMENT_3D('',#20458,#16048,#16049);
#14932=AXIS2_PLACEMENT_3D('',#20483,#16051,#16052);
#14933=AXIS2_PLACEMENT_3D('',#20507,#16054,#16055);
#14934=AXIS2_PLACEMENT_3D('',#20532,#16057,#16058);
#14935=AXIS2_PLACEMENT_3D('',#20557,#16060,#16061);
#14936=AXIS2_PLACEMENT_3D('',#20581,#16063,#16064);
#14937=AXIS2_PLACEMENT_3D('',#20592,#16066,#16067);
#14938=AXIS2_PLACEMENT_3D('',#20598,#16068,#16069);
#14939=AXIS2_PLACEMENT_3D('',#20608,#16071,#16072);
#14940=AXIS2_PLACEMENT_3D('',#20611,#16074,#16075);
#14941=AXIS2_PLACEMENT_3D('',#20613,#16076,#16077);
#14942=AXIS2_PLACEMENT_3D('',#20624,#16078,#16079);
#14943=AXIS2_PLACEMENT_3D('',#20675,#16081,#16082);
#14944=AXIS2_PLACEMENT_3D('',#20726,#16084,#16085);
#14945=AXIS2_PLACEMENT_3D('',#20774,#16087,#16088);
#14946=AXIS2_PLACEMENT_3D('',#20825,#16090,#16091);
#14947=AXIS2_PLACEMENT_3D('',#20876,#16093,#16094);
#14948=AXIS2_PLACEMENT_3D('',#20924,#16096,#16097);
#14949=AXIS2_PLACEMENT_3D('',#20975,#16099,#16100);
#14950=AXIS2_PLACEMENT_3D('',#20994,#16102,#16103);
#14951=AXIS2_PLACEMENT_3D('',#21014,#16104,#16105);
#14952=AXIS2_PLACEMENT_3D('',#21028,#16107,#16108);
#14953=AXIS2_PLACEMENT_3D('',#21038,#16109,#16110);
#14954=AXIS2_PLACEMENT_3D('',#21062,#16112,#16113);
#14955=AXIS2_PLACEMENT_3D('',#21087,#16115,#16116);
#14956=AXIS2_PLACEMENT_3D('',#21112,#16118,#16119);
#14957=AXIS2_PLACEMENT_3D('',#21136,#16121,#16122);
#14958=AXIS2_PLACEMENT_3D('',#21161,#16124,#16125);
#14959=AXIS2_PLACEMENT_3D('',#21186,#16127,#16128);
#14960=AXIS2_PLACEMENT_3D('',#21210,#16130,#16131);
#14961=AXIS2_PLACEMENT_3D('',#21221,#16133,#16134);
#14962=AXIS2_PLACEMENT_3D('',#21227,#16135,#16136);
#14963=AXIS2_PLACEMENT_3D('',#21237,#16138,#16139);
#14964=AXIS2_PLACEMENT_3D('',#21240,#16141,#16142);
#14965=AXIS2_PLACEMENT_3D('',#21242,#16143,#16144);
#14966=AXIS2_PLACEMENT_3D('',#21253,#16145,#16146);
#14967=AXIS2_PLACEMENT_3D('',#21304,#16148,#16149);
#14968=AXIS2_PLACEMENT_3D('',#21355,#16151,#16152);
#14969=AXIS2_PLACEMENT_3D('',#21403,#16154,#16155);
#14970=AXIS2_PLACEMENT_3D('',#21454,#16157,#16158);
#14971=AXIS2_PLACEMENT_3D('',#21505,#16160,#16161);
#14972=AXIS2_PLACEMENT_3D('',#21553,#16163,#16164);
#14973=AXIS2_PLACEMENT_3D('',#21604,#16166,#16167);
#14974=AXIS2_PLACEMENT_3D('',#21623,#16169,#16170);
#14975=AXIS2_PLACEMENT_3D('',#21643,#16171,#16172);
#14976=AXIS2_PLACEMENT_3D('',#21657,#16174,#16175);
#14977=AXIS2_PLACEMENT_3D('',#21667,#16176,#16177);
#14978=AXIS2_PLACEMENT_3D('',#21691,#16179,#16180);
#14979=AXIS2_PLACEMENT_3D('',#21716,#16182,#16183);
#14980=AXIS2_PLACEMENT_3D('',#21741,#16185,#16186);
#14981=AXIS2_PLACEMENT_3D('',#21765,#16188,#16189);
#14982=AXIS2_PLACEMENT_3D('',#21790,#16191,#16192);
#14983=AXIS2_PLACEMENT_3D('',#21815,#16194,#16195);
#14984=AXIS2_PLACEMENT_3D('',#21839,#16197,#16198);
#14985=AXIS2_PLACEMENT_3D('',#21850,#16200,#16201);
#14986=AXIS2_PLACEMENT_3D('',#21856,#16202,#16203);
#14987=AXIS2_PLACEMENT_3D('',#21866,#16205,#16206);
#14988=AXIS2_PLACEMENT_3D('',#21869,#16208,#16209);
#14989=AXIS2_PLACEMENT_3D('',#21871,#16210,#16211);
#14990=AXIS2_PLACEMENT_3D('',#21882,#16212,#16213);
#14991=AXIS2_PLACEMENT_3D('',#21933,#16215,#16216);
#14992=AXIS2_PLACEMENT_3D('',#21984,#16218,#16219);
#14993=AXIS2_PLACEMENT_3D('',#22032,#16221,#16222);
#14994=AXIS2_PLACEMENT_3D('',#22083,#16224,#16225);
#14995=AXIS2_PLACEMENT_3D('',#22134,#16227,#16228);
#14996=AXIS2_PLACEMENT_3D('',#22182,#16230,#16231);
#14997=AXIS2_PLACEMENT_3D('',#22233,#16233,#16234);
#14998=AXIS2_PLACEMENT_3D('',#22252,#16236,#16237);
#14999=AXIS2_PLACEMENT_3D('',#22272,#16238,#16239);
#15000=AXIS2_PLACEMENT_3D('',#22286,#16241,#16242);
#15001=AXIS2_PLACEMENT_3D('',#22296,#16243,#16244);
#15002=AXIS2_PLACEMENT_3D('',#22320,#16246,#16247);
#15003=AXIS2_PLACEMENT_3D('',#22345,#16249,#16250);
#15004=AXIS2_PLACEMENT_3D('',#22370,#16252,#16253);
#15005=AXIS2_PLACEMENT_3D('',#22394,#16255,#16256);
#15006=AXIS2_PLACEMENT_3D('',#22419,#16258,#16259);
#15007=AXIS2_PLACEMENT_3D('',#22444,#16261,#16262);
#15008=AXIS2_PLACEMENT_3D('',#22468,#16264,#16265);
#15009=AXIS2_PLACEMENT_3D('',#22479,#16267,#16268);
#15010=AXIS2_PLACEMENT_3D('',#22485,#16269,#16270);
#15011=AXIS2_PLACEMENT_3D('',#22495,#16272,#16273);
#15012=AXIS2_PLACEMENT_3D('',#22498,#16275,#16276);
#15013=AXIS2_PLACEMENT_3D('',#22500,#16277,#16278);
#15014=AXIS2_PLACEMENT_3D('',#22511,#16279,#16280);
#15015=AXIS2_PLACEMENT_3D('',#22562,#16282,#16283);
#15016=AXIS2_PLACEMENT_3D('',#22613,#16285,#16286);
#15017=AXIS2_PLACEMENT_3D('',#22661,#16288,#16289);
#15018=AXIS2_PLACEMENT_3D('',#22712,#16291,#16292);
#15019=AXIS2_PLACEMENT_3D('',#22763,#16294,#16295);
#15020=AXIS2_PLACEMENT_3D('',#22811,#16297,#16298);
#15021=AXIS2_PLACEMENT_3D('',#22862,#16300,#16301);
#15022=AXIS2_PLACEMENT_3D('',#22881,#16303,#16304);
#15023=AXIS2_PLACEMENT_3D('',#22901,#16305,#16306);
#15024=AXIS2_PLACEMENT_3D('',#22915,#16308,#16309);
#15025=AXIS2_PLACEMENT_3D('',#22925,#16310,#16311);
#15026=AXIS2_PLACEMENT_3D('',#22949,#16313,#16314);
#15027=AXIS2_PLACEMENT_3D('',#22974,#16316,#16317);
#15028=AXIS2_PLACEMENT_3D('',#22999,#16319,#16320);
#15029=AXIS2_PLACEMENT_3D('',#23023,#16322,#16323);
#15030=AXIS2_PLACEMENT_3D('',#23048,#16325,#16326);
#15031=AXIS2_PLACEMENT_3D('',#23073,#16328,#16329);
#15032=AXIS2_PLACEMENT_3D('',#23097,#16331,#16332);
#15033=AXIS2_PLACEMENT_3D('',#23108,#16334,#16335);
#15034=AXIS2_PLACEMENT_3D('',#23114,#16336,#16337);
#15035=AXIS2_PLACEMENT_3D('',#23124,#16339,#16340);
#15036=AXIS2_PLACEMENT_3D('',#23127,#16342,#16343);
#15037=AXIS2_PLACEMENT_3D('',#23129,#16344,#16345);
#15038=AXIS2_PLACEMENT_3D('',#23140,#16346,#16347);
#15039=AXIS2_PLACEMENT_3D('',#23191,#16349,#16350);
#15040=AXIS2_PLACEMENT_3D('',#23242,#16352,#16353);
#15041=AXIS2_PLACEMENT_3D('',#23290,#16355,#16356);
#15042=AXIS2_PLACEMENT_3D('',#23341,#16358,#16359);
#15043=AXIS2_PLACEMENT_3D('',#23392,#16361,#16362);
#15044=AXIS2_PLACEMENT_3D('',#23440,#16364,#16365);
#15045=AXIS2_PLACEMENT_3D('',#23491,#16367,#16368);
#15046=AXIS2_PLACEMENT_3D('',#23510,#16370,#16371);
#15047=AXIS2_PLACEMENT_3D('',#23530,#16372,#16373);
#15048=AXIS2_PLACEMENT_3D('',#23544,#16375,#16376);
#15049=AXIS2_PLACEMENT_3D('',#23554,#16377,#16378);
#15050=AXIS2_PLACEMENT_3D('',#23578,#16380,#16381);
#15051=AXIS2_PLACEMENT_3D('',#23603,#16383,#16384);
#15052=AXIS2_PLACEMENT_3D('',#23628,#16386,#16387);
#15053=AXIS2_PLACEMENT_3D('',#23652,#16389,#16390);
#15054=AXIS2_PLACEMENT_3D('',#23677,#16392,#16393);
#15055=AXIS2_PLACEMENT_3D('',#23702,#16395,#16396);
#15056=AXIS2_PLACEMENT_3D('',#23726,#16398,#16399);
#15057=AXIS2_PLACEMENT_3D('',#23737,#16401,#16402);
#15058=AXIS2_PLACEMENT_3D('',#23743,#16403,#16404);
#15059=AXIS2_PLACEMENT_3D('',#23745,#16405,#16406);
#15060=AXIS2_PLACEMENT_3D('',#23748,#16408,#16409);
#15061=AXIS2_PLACEMENT_3D('',#23749,#16410,#16411);
#15062=AXIS2_PLACEMENT_3D('',#23751,#16412,#16413);
#15063=AXIS2_PLACEMENT_3D('',#23752,#16414,#16415);
#15064=AXIS2_PLACEMENT_3D('',#23754,#16416,#16417);
#15065=AXIS2_PLACEMENT_3D('',#23757,#16419,#16420);
#15066=AXIS2_PLACEMENT_3D('',#23758,#16421,#16422);
#15067=AXIS2_PLACEMENT_3D('',#23760,#16423,#16424);
#15068=AXIS2_PLACEMENT_3D('',#23761,#16425,#16426);
#15069=AXIS2_PLACEMENT_3D('',#23763,#16427,#16428);
#15070=AXIS2_PLACEMENT_3D('',#23766,#16430,#16431);
#15071=AXIS2_PLACEMENT_3D('',#23767,#16432,#16433);
#15072=AXIS2_PLACEMENT_3D('',#23769,#16434,#16435);
#15073=AXIS2_PLACEMENT_3D('',#23770,#16436,#16437);
#15074=AXIS2_PLACEMENT_3D('',#23772,#16438,#16439);
#15075=AXIS2_PLACEMENT_3D('',#23775,#16441,#16442);
#15076=AXIS2_PLACEMENT_3D('',#23776,#16443,#16444);
#15077=AXIS2_PLACEMENT_3D('',#23778,#16445,#16446);
#15078=AXIS2_PLACEMENT_3D('',#23779,#16447,#16448);
#15079=AXIS2_PLACEMENT_3D('',#23782,#16450,#16451);
#15080=AXIS2_PLACEMENT_3D('',#23783,#16452,#16453);
#15081=AXIS2_PLACEMENT_3D('',#23786,#16455,#16456);
#15082=AXIS2_PLACEMENT_3D('',#23787,#16457,#16458);
#15083=AXIS2_PLACEMENT_3D('',#23790,#16460,#16461);
#15084=AXIS2_PLACEMENT_3D('',#23791,#16462,#16463);
#15085=AXIS2_PLACEMENT_3D('',#23794,#16465,#16466);
#15086=AXIS2_PLACEMENT_3D('',#23795,#16467,#16468);
#15087=AXIS2_PLACEMENT_3D('',#23984,#16469,#16470);
#15088=AXIS2_PLACEMENT_3D('',#24731,#16471,#16472);
#15089=AXIS2_PLACEMENT_3D('',#24732,#16473,#16474);
#15090=AXIS2_PLACEMENT_3D('',#24921,#16475,#16476);
#15091=AXIS2_PLACEMENT_3D('',#25668,#16477,#16478);
#15092=AXIS2_PLACEMENT_3D('',#25669,#16479,#16480);
#15093=AXIS2_PLACEMENT_3D('',#25858,#16481,#16482);
#15094=AXIS2_PLACEMENT_3D('',#26605,#16483,#16484);
#15095=AXIS2_PLACEMENT_3D('',#26606,#16485,#16486);
#15096=AXIS2_PLACEMENT_3D('',#26795,#16487,#16488);
#15097=AXIS2_PLACEMENT_3D('',#27542,#16489,#16490);
#15098=AXIS2_PLACEMENT_3D('',#27543,#16491,#16492);
#15099=AXIS2_PLACEMENT_3D('',#27732,#16493,#16494);
#15100=AXIS2_PLACEMENT_3D('',#28479,#16495,#16496);
#15101=AXIS2_PLACEMENT_3D('',#28480,#16497,#16498);
#15102=AXIS2_PLACEMENT_3D('',#28669,#16499,#16500);
#15103=AXIS2_PLACEMENT_3D('',#29416,#16501,#16502);
#15104=AXIS2_PLACEMENT_3D('',#29417,#16503,#16504);
#15105=AXIS2_PLACEMENT_3D('',#29606,#16505,#16506);
#15106=AXIS2_PLACEMENT_3D('',#30353,#16507,#16508);
#15107=AXIS2_PLACEMENT_3D('',#30354,#16509,#16510);
#15108=AXIS2_PLACEMENT_3D('',#30543,#16511,#16512);
#15109=AXIS2_PLACEMENT_3D('',#31290,#16513,#16514);
#15110=AXIS2_PLACEMENT_3D('',#31291,#16515,#16516);
#15111=AXIS2_PLACEMENT_3D('',#31300,#16521,#16522);
#15112=AXIS2_PLACEMENT_3D('',#31322,#16534,#16535);
#15113=AXIS2_PLACEMENT_3D('',#31328,#16539,#16540);
#15114=AXIS2_PLACEMENT_3D('',#31329,#16541,#16542);
#15115=AXIS2_PLACEMENT_3D('',#31330,#16543,#16544);
#15116=AXIS2_PLACEMENT_3D('',#31355,#16557,#16558);
#15117=AXIS2_PLACEMENT_3D('',#31361,#16562,#16563);
#15118=AXIS2_PLACEMENT_3D('',#31367,#16567,#16568);
#15119=AXIS2_PLACEMENT_3D('',#31368,#16569,#16570);
#15120=AXIS2_PLACEMENT_3D('',#31369,#16571,#16572);
#15121=AXIS2_PLACEMENT_3D('',#31375,#16575,#16576);
#15122=AXIS2_PLACEMENT_3D('',#31379,#16579,#16580);
#15123=AXIS2_PLACEMENT_3D('',#31383,#16583,#16584);
#15124=AXIS2_PLACEMENT_3D('',#31385,#16585,#16586);
#15125=AXIS2_PLACEMENT_3D('',#31395,#16591,#16592);
#15126=AXIS2_PLACEMENT_3D('',#31399,#16595,#16596);
#15127=AXIS2_PLACEMENT_3D('',#31405,#16599,#16600);
#15128=AXIS2_PLACEMENT_3D('',#31414,#16605,#16606);
#15129=AXIS2_PLACEMENT_3D('',#31415,#16607,#16608);
#15130=AXIS2_PLACEMENT_3D('',#31419,#16611,#16612);
#15131=AXIS2_PLACEMENT_3D('',#31421,#16614,#16615);
#15132=AXIS2_PLACEMENT_3D('',#31427,#16618,#16619);
#15133=AXIS2_PLACEMENT_3D('',#31431,#16622,#16623);
#15134=AXIS2_PLACEMENT_3D('',#31435,#16626,#16627);
#15135=AXIS2_PLACEMENT_3D('',#31439,#16630,#16631);
#15136=AXIS2_PLACEMENT_3D('',#31443,#16634,#16635);
#15137=AXIS2_PLACEMENT_3D('',#31445,#16636,#16637);
#15138=AXIS2_PLACEMENT_3D('',#31455,#16642,#16643);
#15139=AXIS2_PLACEMENT_3D('',#31457,#16645,#16646);
#15140=AXIS2_PLACEMENT_3D('',#31461,#16649,#16650);
#15141=AXIS2_PLACEMENT_3D('',#31465,#16653,#16654);
#15142=AXIS2_PLACEMENT_3D('',#31471,#16658,#16659);
#15143=AXIS2_PLACEMENT_3D('',#31473,#16661,#16662);
#15144=AXIS2_PLACEMENT_3D('',#31479,#16666,#16667);
#15145=AXIS2_PLACEMENT_3D('',#31483,#16669,#16670);
#15146=AXIS2_PLACEMENT_3D('',#31489,#16674,#16675);
#15147=AXIS2_PLACEMENT_3D('',#31492,#16677,#16678);
#15148=AXIS2_PLACEMENT_3D('',#31494,#16679,#16680);
#15149=AXIS2_PLACEMENT_3D('',#31496,#16682,#16683);
#15150=AXIS2_PLACEMENT_3D('',#31499,#16686,#16687);
#15151=AXIS2_PLACEMENT_3D('',#31501,#16689,#16690);
#15152=AXIS2_PLACEMENT_3D('',#31502,#16691,#16692);
#15153=AXIS2_PLACEMENT_3D('',#31504,#16694,#16695);
#15154=AXIS2_PLACEMENT_3D('',#31509,#16699,#16700);
#15155=AXIS2_PLACEMENT_3D('',#31511,#16702,#16703);
#15156=AXIS2_PLACEMENT_3D('',#31517,#16707,#16708);
#15157=AXIS2_PLACEMENT_3D('',#31519,#16709,#16710);
#15158=AXIS2_PLACEMENT_3D('',#31524,#16713,#16714);
#15159=AXIS2_PLACEMENT_3D('',#31525,#16715,#16716);
#15160=AXIS2_PLACEMENT_3D('',#31540,#16725,#16726);
#15161=AXIS2_PLACEMENT_3D('',#31542,#16728,#16729);
#15162=AXIS2_PLACEMENT_3D('',#31548,#16733,#16734);
#15163=AXIS2_PLACEMENT_3D('',#31568,#16745,#16746);
#15164=AXIS2_PLACEMENT_3D('',#31574,#16750,#16751);
#15165=AXIS2_PLACEMENT_3D('',#31575,#16752,#16753);
#15166=AXIS2_PLACEMENT_3D('',#31576,#16754,#16755);
#15167=AXIS2_PLACEMENT_3D('',#31579,#16758,#16759);
#15168=AXIS2_PLACEMENT_3D('',#31583,#16762,#16763);
#15169=AXIS2_PLACEMENT_3D('',#31585,#16765,#16766);
#15170=AXIS2_PLACEMENT_3D('',#31588,#16768,#16769);
#15171=AXIS2_PLACEMENT_3D('',#31589,#16770,#16771);
#15172=AXIS2_PLACEMENT_3D('',#31590,#16772,#16773);
#15173=AXIS2_PLACEMENT_3D('',#31594,#16776,#16777);
#15174=AXIS2_PLACEMENT_3D('',#31597,#16780,#16781);
#15175=AXIS2_PLACEMENT_3D('',#31601,#16784,#16785);
#15176=AXIS2_PLACEMENT_3D('',#31603,#16787,#16788);
#15177=AXIS2_PLACEMENT_3D('',#31607,#16792,#16793);
#15178=AXIS2_PLACEMENT_3D('',#31609,#16795,#16796);
#15179=AXIS2_PLACEMENT_3D('',#31613,#16800,#16801);
#15180=AXIS2_PLACEMENT_3D('',#31618,#16805,#16806);
#15181=AXIS2_PLACEMENT_3D('',#31619,#16807,#16808);
#15182=AXIS2_PLACEMENT_3D('',#31623,#16811,#16812);
#15183=AXIS2_PLACEMENT_3D('',#31624,#16813,#16814);
#15184=AXIS2_PLACEMENT_3D('',#31626,#16816,#16817);
#15185=AXIS2_PLACEMENT_3D('',#31627,#16818,#16819);
#15186=AXIS2_PLACEMENT_3D('',#31628,#16820,#16821);
#15187=AXIS2_PLACEMENT_3D('',#31630,#16823,#16824);
#15188=AXIS2_PLACEMENT_3D('',#31631,#16825,#16826);
#15189=AXIS2_PLACEMENT_3D('',#31633,#16827,#16828);
#15190=AXIS2_PLACEMENT_3D('',#31636,#16830,#16831);
#15191=AXIS2_PLACEMENT_3D('',#31637,#16832,#16833);
#15192=AXIS2_PLACEMENT_3D('',#31638,#16834,#16835);
#15193=AXIS2_PLACEMENT_3D('',#31639,#16836,#16837);
#15194=AXIS2_PLACEMENT_3D('',#31640,#16838,#16839);
#15195=AXIS2_PLACEMENT_3D('',#31653,#16841,#16842);
#15196=AXIS2_PLACEMENT_3D('',#31656,#16844,#16845);
#15197=AXIS2_PLACEMENT_3D('',#31658,#16846,#16847);
#15198=AXIS2_PLACEMENT_3D('',#31672,#16848,#16849);
#15199=AXIS2_PLACEMENT_3D('',#31726,#16851,#16852);
#15200=AXIS2_PLACEMENT_3D('',#31774,#16854,#16855);
#15201=AXIS2_PLACEMENT_3D('',#31825,#16857,#16858);
#15202=AXIS2_PLACEMENT_3D('',#31876,#16860,#16861);
#15203=AXIS2_PLACEMENT_3D('',#31924,#16863,#16864);
#15204=AXIS2_PLACEMENT_3D('',#31943,#16866,#16867);
#15205=AXIS2_PLACEMENT_3D('',#31963,#16868,#16869);
#15206=AXIS2_PLACEMENT_3D('',#31978,#16871,#16872);
#15207=AXIS2_PLACEMENT_3D('',#31989,#16873,#16874);
#15208=AXIS2_PLACEMENT_3D('',#32014,#16876,#16877);
#15209=AXIS2_PLACEMENT_3D('',#32039,#16879,#16880);
#15210=AXIS2_PLACEMENT_3D('',#32063,#16882,#16883);
#15211=AXIS2_PLACEMENT_3D('',#32088,#16885,#16886);
#15212=AXIS2_PLACEMENT_3D('',#32113,#16888,#16889);
#15213=AXIS2_PLACEMENT_3D('',#32124,#16891,#16892);
#15214=AXIS2_PLACEMENT_3D('',#32130,#16893,#16894);
#15215=AXIS2_PLACEMENT_3D('',#32143,#16896,#16897);
#15216=AXIS2_PLACEMENT_3D('',#32146,#16899,#16900);
#15217=AXIS2_PLACEMENT_3D('',#32148,#16901,#16902);
#15218=AXIS2_PLACEMENT_3D('',#32162,#16903,#16904);
#15219=AXIS2_PLACEMENT_3D('',#32216,#16906,#16907);
#15220=AXIS2_PLACEMENT_3D('',#32264,#16909,#16910);
#15221=AXIS2_PLACEMENT_3D('',#32315,#16912,#16913);
#15222=AXIS2_PLACEMENT_3D('',#32366,#16915,#16916);
#15223=AXIS2_PLACEMENT_3D('',#32414,#16918,#16919);
#15224=AXIS2_PLACEMENT_3D('',#32433,#16921,#16922);
#15225=AXIS2_PLACEMENT_3D('',#32453,#16923,#16924);
#15226=AXIS2_PLACEMENT_3D('',#32468,#16926,#16927);
#15227=AXIS2_PLACEMENT_3D('',#32479,#16928,#16929);
#15228=AXIS2_PLACEMENT_3D('',#32504,#16931,#16932);
#15229=AXIS2_PLACEMENT_3D('',#32529,#16934,#16935);
#15230=AXIS2_PLACEMENT_3D('',#32553,#16937,#16938);
#15231=AXIS2_PLACEMENT_3D('',#32578,#16940,#16941);
#15232=AXIS2_PLACEMENT_3D('',#32603,#16943,#16944);
#15233=AXIS2_PLACEMENT_3D('',#32614,#16946,#16947);
#15234=AXIS2_PLACEMENT_3D('',#32620,#16948,#16949);
#15235=AXIS2_PLACEMENT_3D('',#32633,#16951,#16952);
#15236=AXIS2_PLACEMENT_3D('',#32636,#16954,#16955);
#15237=AXIS2_PLACEMENT_3D('',#32638,#16956,#16957);
#15238=AXIS2_PLACEMENT_3D('',#32652,#16958,#16959);
#15239=AXIS2_PLACEMENT_3D('',#32706,#16961,#16962);
#15240=AXIS2_PLACEMENT_3D('',#32754,#16964,#16965);
#15241=AXIS2_PLACEMENT_3D('',#32805,#16967,#16968);
#15242=AXIS2_PLACEMENT_3D('',#32856,#16970,#16971);
#15243=AXIS2_PLACEMENT_3D('',#32904,#16973,#16974);
#15244=AXIS2_PLACEMENT_3D('',#32923,#16976,#16977);
#15245=AXIS2_PLACEMENT_3D('',#32943,#16978,#16979);
#15246=AXIS2_PLACEMENT_3D('',#32958,#16981,#16982);
#15247=AXIS2_PLACEMENT_3D('',#32969,#16983,#16984);
#15248=AXIS2_PLACEMENT_3D('',#32994,#16986,#16987);
#15249=AXIS2_PLACEMENT_3D('',#33019,#16989,#16990);
#15250=AXIS2_PLACEMENT_3D('',#33043,#16992,#16993);
#15251=AXIS2_PLACEMENT_3D('',#33068,#16995,#16996);
#15252=AXIS2_PLACEMENT_3D('',#33093,#16998,#16999);
#15253=AXIS2_PLACEMENT_3D('',#33104,#17001,#17002);
#15254=AXIS2_PLACEMENT_3D('',#33110,#17003,#17004);
#15255=AXIS2_PLACEMENT_3D('',#33123,#17006,#17007);
#15256=AXIS2_PLACEMENT_3D('',#33126,#17009,#17010);
#15257=AXIS2_PLACEMENT_3D('',#33128,#17011,#17012);
#15258=AXIS2_PLACEMENT_3D('',#33142,#17013,#17014);
#15259=AXIS2_PLACEMENT_3D('',#33196,#17016,#17017);
#15260=AXIS2_PLACEMENT_3D('',#33244,#17019,#17020);
#15261=AXIS2_PLACEMENT_3D('',#33295,#17022,#17023);
#15262=AXIS2_PLACEMENT_3D('',#33346,#17025,#17026);
#15263=AXIS2_PLACEMENT_3D('',#33394,#17028,#17029);
#15264=AXIS2_PLACEMENT_3D('',#33413,#17031,#17032);
#15265=AXIS2_PLACEMENT_3D('',#33433,#17033,#17034);
#15266=AXIS2_PLACEMENT_3D('',#33448,#17036,#17037);
#15267=AXIS2_PLACEMENT_3D('',#33459,#17038,#17039);
#15268=AXIS2_PLACEMENT_3D('',#33484,#17041,#17042);
#15269=AXIS2_PLACEMENT_3D('',#33509,#17044,#17045);
#15270=AXIS2_PLACEMENT_3D('',#33533,#17047,#17048);
#15271=AXIS2_PLACEMENT_3D('',#33558,#17050,#17051);
#15272=AXIS2_PLACEMENT_3D('',#33583,#17053,#17054);
#15273=AXIS2_PLACEMENT_3D('',#33594,#17056,#17057);
#15274=AXIS2_PLACEMENT_3D('',#33600,#17058,#17059);
#15275=AXIS2_PLACEMENT_3D('',#33640,#17061,#17062);
#15276=AXIS2_PLACEMENT_3D('',#33648,#17064,#17065);
#15277=AXIS2_PLACEMENT_3D('',#33692,#17066,#17067);
#15278=AXIS2_PLACEMENT_3D('',#33776,#17069,#17070);
#15279=AXIS2_PLACEMENT_3D('',#33851,#17072,#17073);
#15280=AXIS2_PLACEMENT_3D('',#33882,#17075,#17076);
#15281=AXIS2_PLACEMENT_3D('',#33920,#17077,#17078);
#15282=AXIS2_PLACEMENT_3D('',#33934,#17080,#17081);
#15283=AXIS2_PLACEMENT_3D('',#33945,#17082,#17083);
#15284=AXIS2_PLACEMENT_3D('',#33982,#17085,#17086);
#15285=AXIS2_PLACEMENT_3D('',#34016,#17088,#17089);
#15286=AXIS2_PLACEMENT_3D('',#34052,#17091,#17092);
#15287=AXIS2_PLACEMENT_3D('',#34064,#17094,#17095);
#15288=AXIS2_PLACEMENT_3D('',#34072,#17096,#17097);
#15289=AXIS2_PLACEMENT_3D('',#34112,#17099,#17100);
#15290=AXIS2_PLACEMENT_3D('',#34120,#17102,#17103);
#15291=AXIS2_PLACEMENT_3D('',#34164,#17104,#17105);
#15292=AXIS2_PLACEMENT_3D('',#34248,#17107,#17108);
#15293=AXIS2_PLACEMENT_3D('',#34323,#17110,#17111);
#15294=AXIS2_PLACEMENT_3D('',#34354,#17113,#17114);
#15295=AXIS2_PLACEMENT_3D('',#34392,#17115,#17116);
#15296=AXIS2_PLACEMENT_3D('',#34406,#17118,#17119);
#15297=AXIS2_PLACEMENT_3D('',#34417,#17120,#17121);
#15298=AXIS2_PLACEMENT_3D('',#34454,#17123,#17124);
#15299=AXIS2_PLACEMENT_3D('',#34488,#17126,#17127);
#15300=AXIS2_PLACEMENT_3D('',#34524,#17129,#17130);
#15301=AXIS2_PLACEMENT_3D('',#34536,#17132,#17133);
#15302=AXIS2_PLACEMENT_3D('',#34544,#17134,#17135);
#15303=AXIS2_PLACEMENT_3D('',#34584,#17137,#17138);
#15304=AXIS2_PLACEMENT_3D('',#34592,#17140,#17141);
#15305=AXIS2_PLACEMENT_3D('',#34636,#17142,#17143);
#15306=AXIS2_PLACEMENT_3D('',#34720,#17145,#17146);
#15307=AXIS2_PLACEMENT_3D('',#34795,#17148,#17149);
#15308=AXIS2_PLACEMENT_3D('',#34826,#17151,#17152);
#15309=AXIS2_PLACEMENT_3D('',#34864,#17153,#17154);
#15310=AXIS2_PLACEMENT_3D('',#34878,#17156,#17157);
#15311=AXIS2_PLACEMENT_3D('',#34889,#17158,#17159);
#15312=AXIS2_PLACEMENT_3D('',#34926,#17161,#17162);
#15313=AXIS2_PLACEMENT_3D('',#34960,#17164,#17165);
#15314=AXIS2_PLACEMENT_3D('',#34996,#17167,#17168);
#15315=AXIS2_PLACEMENT_3D('',#35008,#17170,#17171);
#15316=AXIS2_PLACEMENT_3D('',#35016,#17172,#17173);
#15317=AXIS2_PLACEMENT_3D('',#35056,#17175,#17176);
#15318=AXIS2_PLACEMENT_3D('',#35064,#17178,#17179);
#15319=AXIS2_PLACEMENT_3D('',#35108,#17180,#17181);
#15320=AXIS2_PLACEMENT_3D('',#35192,#17183,#17184);
#15321=AXIS2_PLACEMENT_3D('',#35267,#17186,#17187);
#15322=AXIS2_PLACEMENT_3D('',#35298,#17189,#17190);
#15323=AXIS2_PLACEMENT_3D('',#35336,#17191,#17192);
#15324=AXIS2_PLACEMENT_3D('',#35350,#17194,#17195);
#15325=AXIS2_PLACEMENT_3D('',#35361,#17196,#17197);
#15326=AXIS2_PLACEMENT_3D('',#35398,#17199,#17200);
#15327=AXIS2_PLACEMENT_3D('',#35432,#17202,#17203);
#15328=AXIS2_PLACEMENT_3D('',#35468,#17205,#17206);
#15329=AXIS2_PLACEMENT_3D('',#35480,#17208,#17209);
#15330=AXIS2_PLACEMENT_3D('',#35488,#17210,#17211);
#15331=AXIS2_PLACEMENT_3D('',#35710,#17212,#17213);
#15332=AXIS2_PLACEMENT_3D('',#36552,#17214,#17215);
#15333=AXIS2_PLACEMENT_3D('',#36553,#17216,#17217);
#15334=AXIS2_PLACEMENT_3D('',#36775,#17218,#17219);
#15335=AXIS2_PLACEMENT_3D('',#37617,#17220,#17221);
#15336=AXIS2_PLACEMENT_3D('',#37618,#17222,#17223);
#15337=AXIS2_PLACEMENT_3D('',#37840,#17224,#17225);
#15338=AXIS2_PLACEMENT_3D('',#38682,#17226,#17227);
#15339=AXIS2_PLACEMENT_3D('',#38683,#17228,#17229);
#15340=AXIS2_PLACEMENT_3D('',#38905,#17230,#17231);
#15341=AXIS2_PLACEMENT_3D('',#39747,#17232,#17233);
#15342=AXIS2_PLACEMENT_3D('',#39748,#17234,#17235);
#15343=AXIS2_PLACEMENT_3D('',#39749,#17236,#17237);
#15344=AXIS2_PLACEMENT_3D('',#39750,#17238,#17239);
#15345=AXIS2_PLACEMENT_3D('',#39751,#17240,#17241);
#15346=AXIS2_PLACEMENT_3D('',#39752,#17242,#17243);
#15347=AXIS2_PLACEMENT_3D('',#39953,#17244,#17245);
#15348=AXIS2_PLACEMENT_3D('',#40624,#17246,#17247);
#15349=AXIS2_PLACEMENT_3D('',#40625,#17248,#17249);
#15350=AXIS2_PLACEMENT_3D('',#40826,#17250,#17251);
#15351=AXIS2_PLACEMENT_3D('',#41497,#17252,#17253);
#15352=AXIS2_PLACEMENT_3D('',#41498,#17254,#17255);
#15353=AXIS2_PLACEMENT_3D('',#41699,#17256,#17257);
#15354=AXIS2_PLACEMENT_3D('',#42370,#17258,#17259);
#15355=AXIS2_PLACEMENT_3D('',#42371,#17260,#17261);
#15356=AXIS2_PLACEMENT_3D('',#42572,#17262,#17263);
#15357=AXIS2_PLACEMENT_3D('',#43243,#17264,#17265);
#15358=AXIS2_PLACEMENT_3D('',#43244,#17266,#17267);
#15359=AXIS2_PLACEMENT_3D('',#43246,#17268,#17269);
#15360=AXIS2_PLACEMENT_3D('',#43249,#17271,#17272);
#15361=AXIS2_PLACEMENT_3D('',#43250,#17273,#17274);
#15362=AXIS2_PLACEMENT_3D('',#43252,#17275,#17276);
#15363=AXIS2_PLACEMENT_3D('',#43253,#17277,#17278);
#15364=AXIS2_PLACEMENT_3D('',#43256,#17280,#17281);
#15365=AXIS2_PLACEMENT_3D('',#43257,#17282,#17283);
#15366=AXIS2_PLACEMENT_3D('',#43259,#17284,#17285);
#15367=AXIS2_PLACEMENT_3D('',#43262,#17287,#17288);
#15368=AXIS2_PLACEMENT_3D('',#43263,#17289,#17290);
#15369=AXIS2_PLACEMENT_3D('',#43264,#17291,#17292);
#15370=AXIS2_PLACEMENT_3D('',#43265,#17293,#17294);
#15371=AXIS2_PLACEMENT_3D('',#43266,#17295,#17296);
#15372=AXIS2_PLACEMENT_3D('',#43300,#17298,#17299);
#15373=AXIS2_PLACEMENT_3D('',#43341,#17300,#17301);
#15374=AXIS2_PLACEMENT_3D('',#43428,#17303,#17304);
#15375=AXIS2_PLACEMENT_3D('',#43515,#17306,#17307);
#15376=AXIS2_PLACEMENT_3D('',#43602,#17309,#17310);
#15377=AXIS2_PLACEMENT_3D('',#43692,#17312,#17313);
#15378=AXIS2_PLACEMENT_3D('',#43779,#17315,#17316);
#15379=AXIS2_PLACEMENT_3D('',#43866,#17318,#17319);
#15380=AXIS2_PLACEMENT_3D('',#43953,#17321,#17322);
#15381=AXIS2_PLACEMENT_3D('',#44040,#17324,#17325);
#15382=AXIS2_PLACEMENT_3D('',#44130,#17327,#17328);
#15383=AXIS2_PLACEMENT_3D('',#44217,#17330,#17331);
#15384=AXIS2_PLACEMENT_3D('',#44304,#17333,#17334);
#15385=AXIS2_PLACEMENT_3D('',#44391,#17336,#17337);
#15386=AXIS2_PLACEMENT_3D('',#44478,#17339,#17340);
#15387=AXIS2_PLACEMENT_3D('',#44565,#17342,#17343);
#15388=AXIS2_PLACEMENT_3D('',#44652,#17345,#17346);
#15389=AXIS2_PLACEMENT_3D('',#44739,#17348,#17349);
#15390=AXIS2_PLACEMENT_3D('',#44826,#17351,#17352);
#15391=AXIS2_PLACEMENT_3D('',#44913,#17354,#17355);
#15392=AXIS2_PLACEMENT_3D('',#45000,#17357,#17358);
#15393=AXIS2_PLACEMENT_3D('',#45090,#17360,#17361);
#15394=AXIS2_PLACEMENT_3D('',#45177,#17363,#17364);
#15395=AXIS2_PLACEMENT_3D('',#45264,#17366,#17367);
#15396=AXIS2_PLACEMENT_3D('',#45351,#17369,#17370);
#15397=AXIS2_PLACEMENT_3D('',#45438,#17372,#17373);
#15398=AXIS2_PLACEMENT_3D('',#45528,#17375,#17376);
#15399=AXIS2_PLACEMENT_3D('',#45615,#17378,#17379);
#15400=AXIS2_PLACEMENT_3D('',#45646,#17381,#17382);
#15401=AXIS2_PLACEMENT_3D('',#45684,#17383,#17384);
#15402=AXIS2_PLACEMENT_3D('',#45697,#17386,#17387);
#15403=AXIS2_PLACEMENT_3D('',#45706,#17388,#17389);
#15404=AXIS2_PLACEMENT_3D('',#45744,#17391,#17392);
#15405=AXIS2_PLACEMENT_3D('',#45780,#17394,#17395);
#15406=AXIS2_PLACEMENT_3D('',#45818,#17397,#17398);
#15407=AXIS2_PLACEMENT_3D('',#45855,#17400,#17401);
#15408=AXIS2_PLACEMENT_3D('',#45892,#17403,#17404);
#15409=AXIS2_PLACEMENT_3D('',#45930,#17406,#17407);
#15410=AXIS2_PLACEMENT_3D('',#45966,#17409,#17410);
#15411=AXIS2_PLACEMENT_3D('',#46004,#17412,#17413);
#15412=AXIS2_PLACEMENT_3D('',#46041,#17415,#17416);
#15413=AXIS2_PLACEMENT_3D('',#46078,#17418,#17419);
#15414=AXIS2_PLACEMENT_3D('',#46116,#17421,#17422);
#15415=AXIS2_PLACEMENT_3D('',#46152,#17424,#17425);
#15416=AXIS2_PLACEMENT_3D('',#46190,#17427,#17428);
#15417=AXIS2_PLACEMENT_3D('',#46227,#17430,#17431);
#15418=AXIS2_PLACEMENT_3D('',#46264,#17433,#17434);
#15419=AXIS2_PLACEMENT_3D('',#46302,#17436,#17437);
#15420=AXIS2_PLACEMENT_3D('',#46338,#17439,#17440);
#15421=AXIS2_PLACEMENT_3D('',#46376,#17442,#17443);
#15422=AXIS2_PLACEMENT_3D('',#46412,#17445,#17446);
#15423=AXIS2_PLACEMENT_3D('',#46450,#17448,#17449);
#15424=AXIS2_PLACEMENT_3D('',#46488,#17451,#17452);
#15425=AXIS2_PLACEMENT_3D('',#46524,#17454,#17455);
#15426=AXIS2_PLACEMENT_3D('',#46562,#17457,#17458);
#15427=AXIS2_PLACEMENT_3D('',#46598,#17460,#17461);
#15428=AXIS2_PLACEMENT_3D('',#46636,#17463,#17464);
#15429=AXIS2_PLACEMENT_3D('',#46674,#17466,#17467);
#15430=AXIS2_PLACEMENT_3D('',#46710,#17469,#17470);
#15431=AXIS2_PLACEMENT_3D('',#46722,#17472,#17473);
#15432=AXIS2_PLACEMENT_3D('',#46730,#17474,#17475);
#15433=AXIS2_PLACEMENT_3D('',#50232,#17476,#17477);
#15434=AXIS2_PLACEMENT_3D('',#50249,#17486,#17487);
#15435=AXIS2_PLACEMENT_3D('',#50250,#17488,#17489);
#15436=AXIS2_PLACEMENT_3D('',#50259,#17494,#17495);
#15437=AXIS2_PLACEMENT_3D('',#50265,#17499,#17500);
#15438=AXIS2_PLACEMENT_3D('',#50268,#17503,#17504);
#15439=AXIS2_PLACEMENT_3D('',#50272,#17507,#17508);
#15440=AXIS2_PLACEMENT_3D('',#50276,#17511,#17512);
#15441=AXIS2_PLACEMENT_3D('',#50280,#17515,#17516);
#15442=AXIS2_PLACEMENT_3D('',#50284,#17519,#17520);
#15443=AXIS2_PLACEMENT_3D('',#50288,#17523,#17524);
#15444=AXIS2_PLACEMENT_3D('',#50292,#17527,#17528);
#15445=AXIS2_PLACEMENT_3D('',#50294,#17530,#17531);
#15446=AXIS2_PLACEMENT_3D('',#50295,#17532,#17533);
#15447=AXIS2_PLACEMENT_3D('',#50296,#17534,#17535);
#15448=AXIS2_PLACEMENT_3D('',#50298,#17536,#17537);
#15449=AXIS2_PLACEMENT_3D('',#50301,#17539,#17540);
#15450=AXIS2_PLACEMENT_3D('',#50302,#17541,#17542);
#15451=AXIS2_PLACEMENT_3D('',#50304,#17543,#17544);
#15452=AXIS2_PLACEMENT_3D('',#50307,#17546,#17547);
#15453=AXIS2_PLACEMENT_3D('',#50308,#17548,#17549);
#15454=AXIS2_PLACEMENT_3D('',#50313,#17551,#17552);
#15455=AXIS2_PLACEMENT_3D('',#50316,#17554,#17555);
#15456=AXIS2_PLACEMENT_3D('',#50317,#17556,#17557);
#15457=AXIS2_PLACEMENT_3D('',#50322,#17559,#17560);
#15458=AXIS2_PLACEMENT_3D('',#50325,#17562,#17563);
#15459=AXIS2_PLACEMENT_3D('',#50326,#17564,#17565);
#15460=AXIS2_PLACEMENT_3D('',#50346,#17576,#17577);
#15461=AXIS2_PLACEMENT_3D('',#50347,#17578,#17579);
#15462=AXIS2_PLACEMENT_3D('',#50361,#17587,#17588);
#15463=AXIS2_PLACEMENT_3D('',#50375,#17596,#17597);
#15464=AXIS2_PLACEMENT_3D('',#50377,#17599,#17600);
#15465=AXIS2_PLACEMENT_3D('',#50381,#17602,#17603);
#15466=AXIS2_PLACEMENT_3D('',#50383,#17604,#17605);
#15467=AXIS2_PLACEMENT_3D('',#50384,#17606,#17607);
#15468=AXIS2_PLACEMENT_3D('',#50388,#17609,#17610);
#15469=AXIS2_PLACEMENT_3D('',#50390,#17612,#17613);
#15470=AXIS2_PLACEMENT_3D('',#50397,#17618,#17619);
#15471=AXIS2_PLACEMENT_3D('',#50399,#17621,#17622);
#15472=AXIS2_PLACEMENT_3D('',#50402,#17625,#17626);
#15473=AXIS2_PLACEMENT_3D('',#50403,#17627,#17628);
#15474=AXIS2_PLACEMENT_3D('',#50406,#17631,#17632);
#15475=AXIS2_PLACEMENT_3D('',#50408,#17634,#17635);
#15476=AXIS2_PLACEMENT_3D('',#50409,#17636,#17637);
#15477=AXIS2_PLACEMENT_3D('',#50411,#17639,#17640);
#15478=AXIS2_PLACEMENT_3D('',#50413,#17642,#17643);
#15479=AXIS2_PLACEMENT_3D('',#50417,#17646,#17647);
#15480=AXIS2_PLACEMENT_3D('',#50421,#17650,#17651);
#15481=AXIS2_PLACEMENT_3D('',#50423,#17653,#17654);
#15482=AXIS2_PLACEMENT_3D('',#50424,#17655,#17656);
#15483=AXIS2_PLACEMENT_3D('',#50425,#17657,#17658);
#15484=AXIS2_PLACEMENT_3D('',#50447,#17660,#17661);
#15485=AXIS2_PLACEMENT_3D('',#50458,#17662,#17663);
#15486=AXIS2_PLACEMENT_3D('',#50542,#17665,#17666);
#15487=AXIS2_PLACEMENT_3D('',#50632,#17668,#17669);
#15488=AXIS2_PLACEMENT_3D('',#50716,#17671,#17672);
#15489=AXIS2_PLACEMENT_3D('',#50806,#17674,#17675);
#15490=AXIS2_PLACEMENT_3D('',#50896,#17677,#17678);
#15491=AXIS2_PLACEMENT_3D('',#50980,#17680,#17681);
#15492=AXIS2_PLACEMENT_3D('',#51070,#17683,#17684);
#15493=AXIS2_PLACEMENT_3D('',#51154,#17686,#17687);
#15494=AXIS2_PLACEMENT_3D('',#51244,#17689,#17690);
#15495=AXIS2_PLACEMENT_3D('',#51328,#17692,#17693);
#15496=AXIS2_PLACEMENT_3D('',#51418,#17695,#17696);
#15497=AXIS2_PLACEMENT_3D('',#51508,#17698,#17699);
#15498=AXIS2_PLACEMENT_3D('',#51592,#17701,#17702);
#15499=AXIS2_PLACEMENT_3D('',#51682,#17704,#17705);
#15500=AXIS2_PLACEMENT_3D('',#51766,#17707,#17708);
#15501=AXIS2_PLACEMENT_3D('',#51856,#17710,#17711);
#15502=AXIS2_PLACEMENT_3D('',#51940,#17713,#17714);
#15503=AXIS2_PLACEMENT_3D('',#52027,#17716,#17717);
#15504=AXIS2_PLACEMENT_3D('',#52117,#17719,#17720);
#15505=AXIS2_PLACEMENT_3D('',#52201,#17722,#17723);
#15506=AXIS2_PLACEMENT_3D('',#52291,#17725,#17726);
#15507=AXIS2_PLACEMENT_3D('',#52375,#17728,#17729);
#15508=AXIS2_PLACEMENT_3D('',#52465,#17731,#17732);
#15509=AXIS2_PLACEMENT_3D('',#52552,#17734,#17735);
#15510=AXIS2_PLACEMENT_3D('',#52639,#17737,#17738);
#15511=AXIS2_PLACEMENT_3D('',#52729,#17740,#17741);
#15512=AXIS2_PLACEMENT_3D('',#52813,#17743,#17744);
#15513=AXIS2_PLACEMENT_3D('',#52903,#17746,#17747);
#15514=AXIS2_PLACEMENT_3D('',#52987,#17749,#17750);
#15515=AXIS2_PLACEMENT_3D('',#53077,#17752,#17753);
#15516=AXIS2_PLACEMENT_3D('',#53164,#17755,#17756);
#15517=AXIS2_PLACEMENT_3D('',#53251,#17758,#17759);
#15518=AXIS2_PLACEMENT_3D('',#53341,#17761,#17762);
#15519=AXIS2_PLACEMENT_3D('',#53425,#17764,#17765);
#15520=AXIS2_PLACEMENT_3D('',#53515,#17767,#17768);
#15521=AXIS2_PLACEMENT_3D('',#53517,#17769,#17770);
#15522=AXIS2_PLACEMENT_3D('',#53521,#17772,#17773);
#15523=AXIS2_PLACEMENT_3D('',#53558,#17775,#17776);
#15524=AXIS2_PLACEMENT_3D('',#53559,#17777,#17778);
#15525=AXIS2_PLACEMENT_3D('',#53580,#17780,#17781);
#15526=AXIS2_PLACEMENT_3D('',#53594,#17782,#17783);
#15527=AXIS2_PLACEMENT_3D('',#53631,#17785,#17786);
#15528=AXIS2_PLACEMENT_3D('',#53668,#17788,#17789);
#15529=AXIS2_PLACEMENT_3D('',#53705,#17791,#17792);
#15530=AXIS2_PLACEMENT_3D('',#53743,#17794,#17795);
#15531=AXIS2_PLACEMENT_3D('',#53779,#17797,#17798);
#15532=AXIS2_PLACEMENT_3D('',#53817,#17800,#17801);
#15533=AXIS2_PLACEMENT_3D('',#53854,#17803,#17804);
#15534=AXIS2_PLACEMENT_3D('',#53891,#17806,#17807);
#15535=AXIS2_PLACEMENT_3D('',#53928,#17809,#17810);
#15536=AXIS2_PLACEMENT_3D('',#53965,#17812,#17813);
#15537=AXIS2_PLACEMENT_3D('',#54003,#17815,#17816);
#15538=AXIS2_PLACEMENT_3D('',#54039,#17818,#17819);
#15539=AXIS2_PLACEMENT_3D('',#54077,#17821,#17822);
#15540=AXIS2_PLACEMENT_3D('',#54114,#17824,#17825);
#15541=AXIS2_PLACEMENT_3D('',#54151,#17827,#17828);
#15542=AXIS2_PLACEMENT_3D('',#54188,#17830,#17831);
#15543=AXIS2_PLACEMENT_3D('',#54225,#17833,#17834);
#15544=AXIS2_PLACEMENT_3D('',#54263,#17836,#17837);
#15545=AXIS2_PLACEMENT_3D('',#54299,#17839,#17840);
#15546=AXIS2_PLACEMENT_3D('',#54337,#17842,#17843);
#15547=AXIS2_PLACEMENT_3D('',#54374,#17845,#17846);
#15548=AXIS2_PLACEMENT_3D('',#54411,#17848,#17849);
#15549=AXIS2_PLACEMENT_3D('',#54448,#17851,#17852);
#15550=AXIS2_PLACEMENT_3D('',#54485,#17854,#17855);
#15551=AXIS2_PLACEMENT_3D('',#54523,#17857,#17858);
#15552=AXIS2_PLACEMENT_3D('',#54560,#17860,#17861);
#15553=AXIS2_PLACEMENT_3D('',#54597,#17863,#17864);
#15554=AXIS2_PLACEMENT_3D('',#54634,#17866,#17867);
#15555=AXIS2_PLACEMENT_3D('',#54671,#17869,#17870);
#15556=AXIS2_PLACEMENT_3D('',#54708,#17872,#17873);
#15557=AXIS2_PLACEMENT_3D('',#54745,#17875,#17876);
#15558=AXIS2_PLACEMENT_3D('',#54783,#17878,#17879);
#15559=AXIS2_PLACEMENT_3D('',#54820,#17881,#17882);
#15560=AXIS2_PLACEMENT_3D('',#54857,#17884,#17885);
#15561=AXIS2_PLACEMENT_3D('',#54894,#17887,#17888);
#15562=AXIS2_PLACEMENT_3D('',#54903,#17893,#17894);
#15563=AXIS2_PLACEMENT_3D('',#54909,#17898,#17899);
#15564=AXIS2_PLACEMENT_3D('',#54915,#17903,#17904);
#15565=AXIS2_PLACEMENT_3D('',#54921,#17908,#17909);
#15566=AXIS2_PLACEMENT_3D('',#54927,#17913,#17914);
#15567=AXIS2_PLACEMENT_3D('',#54930,#17917,#17918);
#15568=AXIS2_PLACEMENT_3D('',#54931,#17919,#17920);
#15569=AXIS2_PLACEMENT_3D('',#54933,#17921,#17922);
#15570=AXIS2_PLACEMENT_3D('',#54936,#17924,#17925);
#15571=AXIS2_PLACEMENT_3D('',#54937,#17926,#17927);
#15572=AXIS2_PLACEMENT_3D('',#54938,#17928,#17929);
#15573=AXIS2_PLACEMENT_3D('',#54940,#17930,#17931);
#15574=AXIS2_PLACEMENT_3D('',#54941,#17932,#17933);
#15575=AXIS2_PLACEMENT_3D('',#54943,#17934,#17935);
#15576=AXIS2_PLACEMENT_3D('',#54945,#17937,#17938);
#15577=AXIS2_PLACEMENT_3D('',#57196,#17939,#17940);
#15578=AXIS2_PLACEMENT_3D('',#57198,#17941,#17942);
#15579=AXIS2_PLACEMENT_3D('',#59225,#17943,#17944);
#15580=AXIS2_PLACEMENT_3D('',#59226,#17945,#17946);
#15581=AXIS2_PLACEMENT_3D('',#59228,#17947,#17948);
#15582=AXIS2_PLACEMENT_3D('',#59229,#17949,#17950);
#15583=AXIS2_PLACEMENT_3D('',#59231,#17951,#17952);
#15584=AXIS2_PLACEMENT_3D('',#59233,#17954,#17955);
#15585=AXIS2_PLACEMENT_3D('',#59234,#17956,#17957);
#15586=AXIS2_PLACEMENT_3D('',#59235,#17958,#17959);
#15587=AXIS2_PLACEMENT_3D('',#59236,#17960,#17961);
#15588=AXIS2_PLACEMENT_3D('',#59245,#17966,#17967);
#15589=AXIS2_PLACEMENT_3D('',#59254,#17972,#17973);
#15590=AXIS2_PLACEMENT_3D('',#59255,#17974,#17975);
#15591=AXIS2_PLACEMENT_3D('',#59256,#17976,#17977);
#15592=AXIS2_PLACEMENT_3D('',#59257,#17978,#17979);
#15593=AXIS2_PLACEMENT_3D('',#59258,#17980,#17981);
#15594=AXIS2_PLACEMENT_3D('',#59259,#17982,#17983);
#15595=AXIS2_PLACEMENT_3D('',#59260,#17984,#17985);
#15596=AXIS2_PLACEMENT_3D('',#59261,#17986,#17987);
#15597=AXIS2_PLACEMENT_3D('',#59262,#17988,#17989);
#15598=AXIS2_PLACEMENT_3D('',#59263,#17990,#17991);
#15599=AXIS2_PLACEMENT_3D('',#59265,#17992,#17993);
#15600=AXIS2_PLACEMENT_3D('',#59268,#17995,#17996);
#15601=AXIS2_PLACEMENT_3D('',#59269,#17997,#17998);
#15602=AXIS2_PLACEMENT_3D('',#59271,#17999,#18000);
#15603=AXIS2_PLACEMENT_3D('',#59274,#18002,#18003);
#15604=AXIS2_PLACEMENT_3D('',#59275,#18004,#18005);
#15605=AXIS2_PLACEMENT_3D('',#59276,#18006,#18007);
#15606=AXIS2_PLACEMENT_3D('',#59277,#18008,#18009);
#15607=AXIS2_PLACEMENT_3D('',#59278,#18010,#18011);
#15608=AXIS2_PLACEMENT_3D('',#59280,#18012,#18013);
#15609=AXIS2_PLACEMENT_3D('',#59283,#18015,#18016);
#15610=AXIS2_PLACEMENT_3D('',#59284,#18017,#18018);
#15611=AXIS2_PLACEMENT_3D('',#59286,#18019,#18020);
#15612=AXIS2_PLACEMENT_3D('',#59289,#18022,#18023);
#15613=AXIS2_PLACEMENT_3D('',#59290,#18024,#18025);
#15614=AXIS2_PLACEMENT_3D('',#59291,#18026,#18027);
#15615=AXIS2_PLACEMENT_3D('',#59292,#18028,#18029);
#15616=AXIS2_PLACEMENT_3D('',#59293,#18030,#18031);
#15617=AXIS2_PLACEMENT_3D('',#59309,#18033,#18034);
#15618=AXIS2_PLACEMENT_3D('',#59317,#18035,#18036);
#15619=AXIS2_PLACEMENT_3D('',#59365,#18038,#18039);
#15620=AXIS2_PLACEMENT_3D('',#59413,#18041,#18042);
#15621=AXIS2_PLACEMENT_3D('',#59464,#18044,#18045);
#15622=AXIS2_PLACEMENT_3D('',#59515,#18047,#18048);
#15623=AXIS2_PLACEMENT_3D('',#59563,#18050,#18051);
#15624=AXIS2_PLACEMENT_3D('',#59611,#18053,#18054);
#15625=AXIS2_PLACEMENT_3D('',#59665,#18056,#18057);
#15626=AXIS2_PLACEMENT_3D('',#59713,#18059,#18060);
#15627=AXIS2_PLACEMENT_3D('',#59761,#18062,#18063);
#15628=AXIS2_PLACEMENT_3D('',#59812,#18065,#18066);
#15629=AXIS2_PLACEMENT_3D('',#59863,#18068,#18069);
#15630=AXIS2_PLACEMENT_3D('',#59911,#18071,#18072);
#15631=AXIS2_PLACEMENT_3D('',#59962,#18074,#18075);
#15632=AXIS2_PLACEMENT_3D('',#60013,#18077,#18078);
#15633=AXIS2_PLACEMENT_3D('',#60061,#18080,#18081);
#15634=AXIS2_PLACEMENT_3D('',#60112,#18083,#18084);
#15635=AXIS2_PLACEMENT_3D('',#60160,#18086,#18087);
#15636=AXIS2_PLACEMENT_3D('',#60211,#18089,#18090);
#15637=AXIS2_PLACEMENT_3D('',#60259,#18092,#18093);
#15638=AXIS2_PLACEMENT_3D('',#60310,#18095,#18096);
#15639=AXIS2_PLACEMENT_3D('',#60361,#18098,#18099);
#15640=AXIS2_PLACEMENT_3D('',#60409,#18101,#18102);
#15641=AXIS2_PLACEMENT_3D('',#60460,#18104,#18105);
#15642=AXIS2_PLACEMENT_3D('',#60508,#18107,#18108);
#15643=AXIS2_PLACEMENT_3D('',#60559,#18110,#18111);
#15644=AXIS2_PLACEMENT_3D('',#60610,#18113,#18114);
#15645=AXIS2_PLACEMENT_3D('',#60658,#18116,#18117);
#15646=AXIS2_PLACEMENT_3D('',#60709,#18119,#18120);
#15647=AXIS2_PLACEMENT_3D('',#60760,#18122,#18123);
#15648=AXIS2_PLACEMENT_3D('',#60808,#18125,#18126);
#15649=AXIS2_PLACEMENT_3D('',#60856,#18128,#18129);
#15650=AXIS2_PLACEMENT_3D('',#60907,#18131,#18132);
#15651=AXIS2_PLACEMENT_3D('',#60958,#18134,#18135);
#15652=AXIS2_PLACEMENT_3D('',#61006,#18137,#18138);
#15653=AXIS2_PLACEMENT_3D('',#61057,#18140,#18141);
#15654=AXIS2_PLACEMENT_3D('',#61108,#18143,#18144);
#15655=AXIS2_PLACEMENT_3D('',#61156,#18146,#18147);
#15656=AXIS2_PLACEMENT_3D('',#61204,#18149,#18150);
#15657=AXIS2_PLACEMENT_3D('',#61220,#18152,#18153);
#15658=AXIS2_PLACEMENT_3D('',#61229,#18154,#18155);
#15659=AXIS2_PLACEMENT_3D('',#61254,#18157,#18158);
#15660=AXIS2_PLACEMENT_3D('',#61278,#18160,#18161);
#15661=AXIS2_PLACEMENT_3D('',#61302,#18163,#18164);
#15662=AXIS2_PLACEMENT_3D('',#61328,#18166,#18167);
#15663=AXIS2_PLACEMENT_3D('',#61352,#18169,#18170);
#15664=AXIS2_PLACEMENT_3D('',#61376,#18172,#18173);
#15665=AXIS2_PLACEMENT_3D('',#61402,#18175,#18176);
#15666=AXIS2_PLACEMENT_3D('',#61426,#18178,#18179);
#15667=AXIS2_PLACEMENT_3D('',#61450,#18181,#18182);
#15668=AXIS2_PLACEMENT_3D('',#61474,#18184,#18185);
#15669=AXIS2_PLACEMENT_3D('',#61500,#18187,#18188);
#15670=AXIS2_PLACEMENT_3D('',#61524,#18190,#18191);
#15671=AXIS2_PLACEMENT_3D('',#61548,#18193,#18194);
#15672=AXIS2_PLACEMENT_3D('',#61574,#18196,#18197);
#15673=AXIS2_PLACEMENT_3D('',#61598,#18199,#18200);
#15674=AXIS2_PLACEMENT_3D('',#61622,#18202,#18203);
#15675=AXIS2_PLACEMENT_3D('',#61647,#18205,#18206);
#15676=AXIS2_PLACEMENT_3D('',#61672,#18208,#18209);
#15677=AXIS2_PLACEMENT_3D('',#61696,#18211,#18212);
#15678=AXIS2_PLACEMENT_3D('',#61721,#18214,#18215);
#15679=AXIS2_PLACEMENT_3D('',#61746,#18217,#18218);
#15680=AXIS2_PLACEMENT_3D('',#61770,#18220,#18221);
#15681=AXIS2_PLACEMENT_3D('',#61794,#18223,#18224);
#15682=AXIS2_PLACEMENT_3D('',#61819,#18226,#18227);
#15683=AXIS2_PLACEMENT_3D('',#61844,#18229,#18230);
#15684=AXIS2_PLACEMENT_3D('',#61868,#18232,#18233);
#15685=AXIS2_PLACEMENT_3D('',#61893,#18235,#18236);
#15686=AXIS2_PLACEMENT_3D('',#61918,#18238,#18239);
#15687=AXIS2_PLACEMENT_3D('',#61942,#18241,#18242);
#15688=AXIS2_PLACEMENT_3D('',#61967,#18244,#18245);
#15689=AXIS2_PLACEMENT_3D('',#61991,#18247,#18248);
#15690=AXIS2_PLACEMENT_3D('',#62016,#18250,#18251);
#15691=AXIS2_PLACEMENT_3D('',#62041,#18253,#18254);
#15692=AXIS2_PLACEMENT_3D('',#62065,#18256,#18257);
#15693=AXIS2_PLACEMENT_3D('',#62090,#18259,#18260);
#15694=AXIS2_PLACEMENT_3D('',#62114,#18262,#18263);
#15695=AXIS2_PLACEMENT_3D('',#62139,#18265,#18266);
#15696=AXIS2_PLACEMENT_3D('',#62163,#18268,#18269);
#15697=AXIS2_PLACEMENT_3D('',#62457,#18270,#18271);
#15698=AXIS2_PLACEMENT_3D('',#62491,#18273,#18274);
#15699=AXIS2_PLACEMENT_3D('',#63622,#18275,#18276);
#15700=AXIS2_PLACEMENT_3D('',#63633,#18277,#18278);
#15701=AXIS2_PLACEMENT_3D('',#64767,#18279,#18280);
#15702=AXIS2_PLACEMENT_3D('',#64768,#18281,#18282);
#15703=AXIS2_PLACEMENT_3D('',#64777,#18287,#18288);
#15704=AXIS2_PLACEMENT_3D('',#64783,#18292,#18293);
#15705=AXIS2_PLACEMENT_3D('',#64789,#18297,#18298);
#15706=AXIS2_PLACEMENT_3D('',#64795,#18302,#18303);
#15707=AXIS2_PLACEMENT_3D('',#64801,#18307,#18308);
#15708=AXIS2_PLACEMENT_3D('',#64804,#18311,#18312);
#15709=AXIS2_PLACEMENT_3D('',#64805,#18313,#18314);
#15710=AXIS2_PLACEMENT_3D('',#64807,#18315,#18316);
#15711=AXIS2_PLACEMENT_3D('',#64808,#18317,#18318);
#15712=AXIS2_PLACEMENT_3D('',#64811,#18320,#18321);
#15713=AXIS2_PLACEMENT_3D('',#64812,#18322,#18323);
#15714=AXIS2_PLACEMENT_3D('',#64813,#18324,#18325);
#15715=AXIS2_PLACEMENT_3D('',#64814,#18326,#18327);
#15716=AXIS2_PLACEMENT_3D('',#64815,#18328,#18329);
#15717=AXIS2_PLACEMENT_3D('',#64817,#18330,#18331);
#15718=AXIS2_PLACEMENT_3D('',#64820,#18333,#18334);
#15719=AXIS2_PLACEMENT_3D('',#64821,#18335,#18336);
#15720=AXIS2_PLACEMENT_3D('',#64823,#18337,#18338);
#15721=AXIS2_PLACEMENT_3D('',#64826,#18340,#18341);
#15722=AXIS2_PLACEMENT_3D('',#64827,#18342,#18343);
#15723=AXIS2_PLACEMENT_3D('',#64828,#18344,#18345);
#15724=AXIS2_PLACEMENT_3D('',#64829,#18346,#18347);
#15725=AXIS2_PLACEMENT_3D('',#64830,#18348,#18349);
#15726=AXIS2_PLACEMENT_3D('',#64846,#18351,#18352);
#15727=AXIS2_PLACEMENT_3D('',#64854,#18353,#18354);
#15728=AXIS2_PLACEMENT_3D('',#64902,#18356,#18357);
#15729=AXIS2_PLACEMENT_3D('',#64950,#18359,#18360);
#15730=AXIS2_PLACEMENT_3D('',#65001,#18362,#18363);
#15731=AXIS2_PLACEMENT_3D('',#65052,#18365,#18366);
#15732=AXIS2_PLACEMENT_3D('',#65100,#18368,#18369);
#15733=AXIS2_PLACEMENT_3D('',#65148,#18371,#18372);
#15734=AXIS2_PLACEMENT_3D('',#65199,#18374,#18375);
#15735=AXIS2_PLACEMENT_3D('',#65247,#18377,#18378);
#15736=AXIS2_PLACEMENT_3D('',#65295,#18380,#18381);
#15737=AXIS2_PLACEMENT_3D('',#65346,#18383,#18384);
#15738=AXIS2_PLACEMENT_3D('',#65397,#18386,#18387);
#15739=AXIS2_PLACEMENT_3D('',#65445,#18389,#18390);
#15740=AXIS2_PLACEMENT_3D('',#65496,#18392,#18393);
#15741=AXIS2_PLACEMENT_3D('',#65547,#18395,#18396);
#15742=AXIS2_PLACEMENT_3D('',#65595,#18398,#18399);
#15743=AXIS2_PLACEMENT_3D('',#65646,#18401,#18402);
#15744=AXIS2_PLACEMENT_3D('',#65694,#18404,#18405);
#15745=AXIS2_PLACEMENT_3D('',#65745,#18407,#18408);
#15746=AXIS2_PLACEMENT_3D('',#65796,#18410,#18411);
#15747=AXIS2_PLACEMENT_3D('',#65844,#18413,#18414);
#15748=AXIS2_PLACEMENT_3D('',#65895,#18416,#18417);
#15749=AXIS2_PLACEMENT_3D('',#65946,#18419,#18420);
#15750=AXIS2_PLACEMENT_3D('',#65994,#18422,#18423);
#15751=AXIS2_PLACEMENT_3D('',#66042,#18425,#18426);
#15752=AXIS2_PLACEMENT_3D('',#66093,#18428,#18429);
#15753=AXIS2_PLACEMENT_3D('',#66144,#18431,#18432);
#15754=AXIS2_PLACEMENT_3D('',#66192,#18434,#18435);
#15755=AXIS2_PLACEMENT_3D('',#66243,#18437,#18438);
#15756=AXIS2_PLACEMENT_3D('',#66294,#18440,#18441);
#15757=AXIS2_PLACEMENT_3D('',#66342,#18443,#18444);
#15758=AXIS2_PLACEMENT_3D('',#66347,#18446,#18447);
#15759=AXIS2_PLACEMENT_3D('',#66392,#18448,#18449);
#15760=AXIS2_PLACEMENT_3D('',#66402,#18451,#18452);
#15761=AXIS2_PLACEMENT_3D('',#66403,#18453,#18454);
#15762=AXIS2_PLACEMENT_3D('',#66418,#18456,#18457);
#15763=AXIS2_PLACEMENT_3D('',#66429,#18458,#18459);
#15764=AXIS2_PLACEMENT_3D('',#66453,#18461,#18462);
#15765=AXIS2_PLACEMENT_3D('',#66477,#18464,#18465);
#15766=AXIS2_PLACEMENT_3D('',#66503,#18467,#18468);
#15767=AXIS2_PLACEMENT_3D('',#66527,#18470,#18471);
#15768=AXIS2_PLACEMENT_3D('',#66551,#18473,#18474);
#15769=AXIS2_PLACEMENT_3D('',#66577,#18476,#18477);
#15770=AXIS2_PLACEMENT_3D('',#66601,#18479,#18480);
#15771=AXIS2_PLACEMENT_3D('',#66625,#18482,#18483);
#15772=AXIS2_PLACEMENT_3D('',#66649,#18485,#18486);
#15773=AXIS2_PLACEMENT_3D('',#66675,#18488,#18489);
#15774=AXIS2_PLACEMENT_3D('',#66699,#18491,#18492);
#15775=AXIS2_PLACEMENT_3D('',#66723,#18494,#18495);
#15776=AXIS2_PLACEMENT_3D('',#66749,#18497,#18498);
#15777=AXIS2_PLACEMENT_3D('',#66773,#18500,#18501);
#15778=AXIS2_PLACEMENT_3D('',#66797,#18503,#18504);
#15779=AXIS2_PLACEMENT_3D('',#66822,#18506,#18507);
#15780=AXIS2_PLACEMENT_3D('',#66847,#18509,#18510);
#15781=AXIS2_PLACEMENT_3D('',#66871,#18512,#18513);
#15782=AXIS2_PLACEMENT_3D('',#66896,#18515,#18516);
#15783=AXIS2_PLACEMENT_3D('',#66921,#18518,#18519);
#15784=AXIS2_PLACEMENT_3D('',#66945,#18521,#18522);
#15785=AXIS2_PLACEMENT_3D('',#66970,#18524,#18525);
#15786=AXIS2_PLACEMENT_3D('',#66994,#18527,#18528);
#15787=AXIS2_PLACEMENT_3D('',#67019,#18530,#18531);
#15788=AXIS2_PLACEMENT_3D('',#67043,#18533,#18534);
#15789=AXIS2_PLACEMENT_3D('',#67068,#18536,#18537);
#15790=AXIS2_PLACEMENT_3D('',#67093,#18539,#18540);
#15791=AXIS2_PLACEMENT_3D('',#67117,#18542,#18543);
#15792=AXIS2_PLACEMENT_3D('',#67142,#18545,#18546);
#15793=AXIS2_PLACEMENT_3D('',#67166,#18548,#18549);
#15794=AXIS2_PLACEMENT_3D('',#67170,#18551,#18552);
#15795=AXIS2_PLACEMENT_3D('',#67432,#18554,#18555);
#15796=AXIS2_PLACEMENT_3D('',#67482,#18556,#18557);
#15797=AXIS2_PLACEMENT_3D('',#68426,#18558,#18559);
#15798=AXIS2_PLACEMENT_3D('',#68437,#18560,#18561);
#15799=AXIS2_PLACEMENT_3D('',#69369,#18562,#18563);
#15800=AXIS2_PLACEMENT_3D('',#69370,#18564,#18565);
#15801=AXIS2_PLACEMENT_3D('',#69379,#18570,#18571);
#15802=AXIS2_PLACEMENT_3D('',#69385,#18575,#18576);
#15803=AXIS2_PLACEMENT_3D('',#69391,#18580,#18581);
#15804=AXIS2_PLACEMENT_3D('',#69397,#18585,#18586);
#15805=AXIS2_PLACEMENT_3D('',#69403,#18590,#18591);
#15806=AXIS2_PLACEMENT_3D('',#69406,#18594,#18595);
#15807=AXIS2_PLACEMENT_3D('',#69407,#18596,#18597);
#15808=AXIS2_PLACEMENT_3D('',#69409,#18598,#18599);
#15809=AXIS2_PLACEMENT_3D('',#69410,#18600,#18601);
#15810=AXIS2_PLACEMENT_3D('',#69413,#18603,#18604);
#15811=AXIS2_PLACEMENT_3D('',#69414,#18605,#18606);
#15812=AXIS2_PLACEMENT_3D('',#69415,#18607,#18608);
#15813=AXIS2_PLACEMENT_3D('',#69416,#18609,#18610);
#15814=AXIS2_PLACEMENT_3D('',#69417,#18611,#18612);
#15815=AXIS2_PLACEMENT_3D('',#69418,#18613,#18614);
#15816=AXIS2_PLACEMENT_3D('',#69419,#18615,#18616);
#15817=AXIS2_PLACEMENT_3D('',#69420,#18617,#18618);
#15818=AXIS2_PLACEMENT_3D('',#69421,#18619,#18620);
#15819=AXIS2_PLACEMENT_3D('',#69422,#18621,#18622);
#15820=AXIS2_PLACEMENT_3D('',#69423,#18623,#18624);
#15821=AXIS2_PLACEMENT_3D('',#69424,#18625,#18626);
#15822=AXIS2_PLACEMENT_3D('',#69425,#18627,#18628);
#15823=AXIS2_PLACEMENT_3D('',#69426,#18629,#18630);
#15824=AXIS2_PLACEMENT_3D('',#69427,#18631,#18632);
#15825=AXIS2_PLACEMENT_3D('',#69428,#18633,#18634);
#15826=AXIS2_PLACEMENT_3D('',#69429,#18635,#18636);
#15827=AXIS2_PLACEMENT_3D('',#69430,#18637,#18638);
#15828=AXIS2_PLACEMENT_3D('',#69431,#18639,#18640);
#15829=AXIS2_PLACEMENT_3D('',#69432,#18641,#18642);
#15830=AXIS2_PLACEMENT_3D('',#69433,#18643,#18644);
#15831=AXIS2_PLACEMENT_3D('',#69434,#18645,#18646);
#15832=AXIS2_PLACEMENT_3D('',#69435,#18647,#18648);
#15833=AXIS2_PLACEMENT_3D('',#69436,#18649,#18650);
#15834=AXIS2_PLACEMENT_3D('',#69437,#18651,#18652);
#15835=AXIS2_PLACEMENT_3D('',#69438,#18653,#18654);
#15836=AXIS2_PLACEMENT_3D('',#69439,#18655,#18656);
#15837=AXIS2_PLACEMENT_3D('',#69440,#18657,#18658);
#15838=AXIS2_PLACEMENT_3D('',#69441,#18659,#18660);
#15839=AXIS2_PLACEMENT_3D('',#69442,#18661,#18662);
#15840=AXIS2_PLACEMENT_3D('',#69443,#18663,#18664);
#15841=AXIS2_PLACEMENT_3D('',#69444,#18665,#18666);
#15842=AXIS2_PLACEMENT_3D('',#69445,#18667,#18668);
#15843=AXIS2_PLACEMENT_3D('',#69446,#18669,#18670);
#15844=AXIS2_PLACEMENT_3D('',#69447,#18671,#18672);
#15845=AXIS2_PLACEMENT_3D('',#69448,#18673,#18674);
#15846=AXIS2_PLACEMENT_3D('',#69449,#18675,#18676);
#15847=AXIS2_PLACEMENT_3D('',#69450,#18677,#18678);
#15848=AXIS2_PLACEMENT_3D('',#69451,#18679,#18680);
#15849=AXIS2_PLACEMENT_3D('',#69452,#18681,#18682);
#15850=AXIS2_PLACEMENT_3D('',#69453,#18683,#18684);
#15851=AXIS2_PLACEMENT_3D('',#69454,#18685,#18686);
#15852=AXIS2_PLACEMENT_3D('',#69455,#18687,#18688);
#15853=AXIS2_PLACEMENT_3D('',#69456,#18689,#18690);
#15854=AXIS2_PLACEMENT_3D('',#69457,#18691,#18692);
#15855=AXIS2_PLACEMENT_3D('',#69458,#18693,#18694);
#15856=AXIS2_PLACEMENT_3D('',#69459,#18695,#18696);
#15857=AXIS2_PLACEMENT_3D('',#69460,#18697,#18698);
#15858=AXIS2_PLACEMENT_3D('',#69461,#18699,#18700);
#15859=AXIS2_PLACEMENT_3D('',#69462,#18701,#18702);
#15860=AXIS2_PLACEMENT_3D('',#69463,#18703,#18704);
#15861=AXIS2_PLACEMENT_3D('',#69464,#18705,#18706);
#15862=AXIS2_PLACEMENT_3D('',#69465,#18707,#18708);
#15863=DIRECTION('axis',(0.,0.,1.));
#15864=DIRECTION('refdir',(1.,0.,0.));
#15865=DIRECTION('axis',(0.,0.,1.));
#15866=DIRECTION('refdir',(1.,0.,0.));
#15867=DIRECTION('center_axis',(0.,0.,-1.));
#15868=DIRECTION('ref_axis',(1.,0.,0.));
#15869=DIRECTION('',(0.,0.,-1.));
#15870=DIRECTION('center_axis',(0.,0.,1.));
#15871=DIRECTION('ref_axis',(1.,0.,0.));
#15872=DIRECTION('',(0.,0.,-1.));
#15873=DIRECTION('center_axis',(0.,0.,-1.));
#15874=DIRECTION('ref_axis',(1.,0.,0.));
#15875=DIRECTION('center_axis',(0.,0.,1.));
#15876=DIRECTION('ref_axis',(1.,0.,0.));
#15877=DIRECTION('center_axis',(0.,0.,-1.));
#15878=DIRECTION('ref_axis',(1.,0.,0.));
#15879=DIRECTION('',(0.,0.,-1.));
#15880=DIRECTION('center_axis',(0.,0.,-1.));
#15881=DIRECTION('ref_axis',(1.,0.,0.));
#15882=DIRECTION('',(0.,0.,-1.));
#15883=DIRECTION('center_axis',(0.,0.,-1.));
#15884=DIRECTION('ref_axis',(1.,0.,0.));
#15885=DIRECTION('',(0.,0.,-1.));
#15886=DIRECTION('center_axis',(0.,0.,-1.));
#15887=DIRECTION('ref_axis',(1.,0.,0.));
#15888=DIRECTION('',(0.,0.,-1.));
#15889=DIRECTION('center_axis',(0.,0.,-1.));
#15890=DIRECTION('ref_axis',(1.,0.,0.));
#15891=DIRECTION('',(0.,0.,-1.));
#15892=DIRECTION('center_axis',(0.,0.,-1.));
#15893=DIRECTION('ref_axis',(1.,0.,0.));
#15894=DIRECTION('',(0.,0.,-1.));
#15895=DIRECTION('center_axis',(0.,0.,-1.));
#15896=DIRECTION('ref_axis',(1.,0.,0.));
#15897=DIRECTION('',(0.,0.,-1.));
#15898=DIRECTION('center_axis',(0.,0.,-1.));
#15899=DIRECTION('ref_axis',(0.938009665675859,-0.346609098407217,0.));
#15900=DIRECTION('',(0.,0.,-1.));
#15901=DIRECTION('center_axis',(0.,0.,1.));
#15902=DIRECTION('ref_axis',(1.,0.,0.));
#15903=DIRECTION('center_axis',(0.,0.,-1.));
#15904=DIRECTION('ref_axis',(1.,-3.61224345087086E-14,0.));
#15905=DIRECTION('',(1.22464679914735E-16,-4.4387199776766E-30,-1.));
#15906=DIRECTION('center_axis',(0.,0.,1.));
#15907=DIRECTION('ref_axis',(1.,-3.61224345087086E-14,0.));
#15908=DIRECTION('center_axis',(0.,0.,-1.));
#15909=DIRECTION('ref_axis',(1.,-3.61224345087086E-14,0.));
#15910=DIRECTION('',(1.22464679914735E-16,-4.4387199776766E-30,-1.));
#15911=DIRECTION('center_axis',(0.,0.,-1.));
#15912=DIRECTION('ref_axis',(1.,-3.61224345087086E-14,0.));
#15913=DIRECTION('',(1.22464679914735E-16,-4.4387199776766E-30,-1.));
#15914=DIRECTION('center_axis',(0.,0.,-1.));
#15915=DIRECTION('ref_axis',(1.,-3.61224345087086E-14,0.));
#15916=DIRECTION('',(1.22464679914735E-16,-4.4387199776766E-30,-1.));
#15917=DIRECTION('center_axis',(0.,0.,-1.));
#15918=DIRECTION('ref_axis',(1.,-3.61224345087086E-14,0.));
#15919=DIRECTION('',(1.22464679914735E-16,-4.4387199776766E-30,-1.));
#15920=DIRECTION('center_axis',(0.,0.,-1.));
#15921=DIRECTION('ref_axis',(1.,-3.61224345087086E-14,0.));
#15922=DIRECTION('',(1.22464679914735E-16,-4.4387199776766E-30,-1.));
#15923=DIRECTION('center_axis',(0.,0.,-1.));
#15924=DIRECTION('ref_axis',(1.,-3.61224345087086E-14,0.));
#15925=DIRECTION('',(1.22464679914735E-16,-4.4387199776766E-30,-1.));
#15926=DIRECTION('center_axis',(0.,0.,-1.));
#15927=DIRECTION('ref_axis',(1.,-3.61224345087086E-14,0.));
#15928=DIRECTION('',(1.22464679914735E-16,-4.4387199776766E-30,-1.));
#15929=DIRECTION('center_axis',(0.,0.,-1.));
#15930=DIRECTION('ref_axis',(-0.609168291270311,-0.793040978077936,0.));
#15931=DIRECTION('',(1.22464679914735E-16,-4.4387199776766E-30,-1.));
#15932=DIRECTION('center_axis',(0.,0.,-1.));
#15933=DIRECTION('ref_axis',(1.,-3.61224345087086E-14,0.));
#15934=DIRECTION('center_axis',(0.,0.,-1.));
#15935=DIRECTION('ref_axis',(1.,0.,0.));
#15936=DIRECTION('',(0.,0.,-1.));
#15937=DIRECTION('center_axis',(0.,0.,1.));
#15938=DIRECTION('ref_axis',(1.,0.,0.));
#15939=DIRECTION('',(0.,0.,-1.));
#15940=DIRECTION('center_axis',(0.,0.,-1.));
#15941=DIRECTION('ref_axis',(1.,0.,0.));
#15942=DIRECTION('center_axis',(0.,0.,1.));
#15943=DIRECTION('ref_axis',(1.,0.,0.));
#15944=DIRECTION('center_axis',(0.,0.,-1.));
#15945=DIRECTION('ref_axis',(1.,0.,0.));
#15946=DIRECTION('',(0.,0.,-1.));
#15947=DIRECTION('center_axis',(0.,0.,-1.));
#15948=DIRECTION('ref_axis',(1.,0.,0.));
#15949=DIRECTION('',(0.,0.,-1.));
#15950=DIRECTION('center_axis',(0.,0.,-1.));
#15951=DIRECTION('ref_axis',(1.,0.,0.));
#15952=DIRECTION('',(0.,0.,-1.));
#15953=DIRECTION('center_axis',(0.,0.,-1.));
#15954=DIRECTION('ref_axis',(1.,0.,0.));
#15955=DIRECTION('',(0.,0.,-1.));
#15956=DIRECTION('center_axis',(0.,0.,-1.));
#15957=DIRECTION('ref_axis',(1.,0.,0.));
#15958=DIRECTION('',(0.,0.,-1.));
#15959=DIRECTION('center_axis',(0.,0.,-1.));
#15960=DIRECTION('ref_axis',(1.,0.,0.));
#15961=DIRECTION('',(0.,0.,-1.));
#15962=DIRECTION('center_axis',(0.,0.,-1.));
#15963=DIRECTION('ref_axis',(1.,0.,0.));
#15964=DIRECTION('',(0.,0.,-1.));
#15965=DIRECTION('center_axis',(0.,0.,-1.));
#15966=DIRECTION('ref_axis',(0.938009657291012,-0.346609121098678,0.));
#15967=DIRECTION('',(0.,0.,-1.));
#15968=DIRECTION('center_axis',(0.,0.,1.));
#15969=DIRECTION('ref_axis',(1.,0.,0.));
#15970=DIRECTION('center_axis',(0.,0.,-1.));
#15971=DIRECTION('ref_axis',(1.,-3.46775371283602E-14,0.));
#15972=DIRECTION('',(1.22464679914735E-16,-4.2617710824826E-30,-1.));
#15973=DIRECTION('center_axis',(0.,0.,1.));
#15974=DIRECTION('ref_axis',(1.,-3.46775371283602E-14,0.));
#15975=DIRECTION('center_axis',(0.,0.,-1.));
#15976=DIRECTION('ref_axis',(1.,-3.46775371283602E-14,0.));
#15977=DIRECTION('',(1.22464679914735E-16,-4.2617710824826E-30,-1.));
#15978=DIRECTION('center_axis',(0.,0.,-1.));
#15979=DIRECTION('ref_axis',(1.,-3.46775371283602E-14,0.));
#15980=DIRECTION('',(1.22464679914735E-16,-4.2617710824826E-30,-1.));
#15981=DIRECTION('center_axis',(0.,0.,-1.));
#15982=DIRECTION('ref_axis',(1.,-3.46775371283602E-14,0.));
#15983=DIRECTION('',(1.22464679914735E-16,-4.2617710824826E-30,-1.));
#15984=DIRECTION('center_axis',(0.,0.,-1.));
#15985=DIRECTION('ref_axis',(1.,-3.46775371283602E-14,0.));
#15986=DIRECTION('',(1.22464679914735E-16,-4.2617710824826E-30,-1.));
#15987=DIRECTION('center_axis',(0.,0.,-1.));
#15988=DIRECTION('ref_axis',(1.,-3.46775371283602E-14,0.));
#15989=DIRECTION('',(1.22464679914735E-16,-4.2617710824826E-30,-1.));
#15990=DIRECTION('center_axis',(0.,0.,-1.));
#15991=DIRECTION('ref_axis',(1.,-3.46775371283602E-14,0.));
#15992=DIRECTION('',(1.22464679914735E-16,-4.2617710824826E-30,-1.));
#15993=DIRECTION('center_axis',(0.,0.,-1.));
#15994=DIRECTION('ref_axis',(1.,-3.46775371283602E-14,0.));
#15995=DIRECTION('',(1.22464679914735E-16,-4.2617710824826E-30,-1.));
#15996=DIRECTION('center_axis',(0.,0.,-1.));
#15997=DIRECTION('ref_axis',(-0.609168284311007,-0.793040983423672,0.));
#15998=DIRECTION('',(1.22464679914735E-16,-4.2617710824826E-30,-1.));
#15999=DIRECTION('center_axis',(0.,0.,-1.));
#16000=DIRECTION('ref_axis',(1.,-3.46775371283602E-14,0.));
#16001=DIRECTION('center_axis',(0.,0.,-1.));
#16002=DIRECTION('ref_axis',(1.,0.,0.));
#16003=DIRECTION('',(0.,0.,-1.));
#16004=DIRECTION('center_axis',(0.,0.,1.));
#16005=DIRECTION('ref_axis',(1.,0.,0.));
#16006=DIRECTION('',(0.,0.,-1.));
#16007=DIRECTION('center_axis',(0.,0.,-1.));
#16008=DIRECTION('ref_axis',(1.,0.,0.));
#16009=DIRECTION('center_axis',(0.,0.,1.));
#16010=DIRECTION('ref_axis',(1.,0.,0.));
#16011=DIRECTION('center_axis',(0.,0.,-1.));
#16012=DIRECTION('ref_axis',(1.,0.,0.));
#16013=DIRECTION('',(0.,0.,-1.));
#16014=DIRECTION('center_axis',(0.,0.,-1.));
#16015=DIRECTION('ref_axis',(1.,0.,0.));
#16016=DIRECTION('',(0.,0.,-1.));
#16017=DIRECTION('center_axis',(0.,0.,-1.));
#16018=DIRECTION('ref_axis',(1.,0.,0.));
#16019=DIRECTION('',(0.,0.,-1.));
#16020=DIRECTION('center_axis',(0.,0.,-1.));
#16021=DIRECTION('ref_axis',(1.,0.,0.));
#16022=DIRECTION('',(0.,0.,-1.));
#16023=DIRECTION('center_axis',(0.,0.,-1.));
#16024=DIRECTION('ref_axis',(1.,0.,0.));
#16025=DIRECTION('',(0.,0.,-1.));
#16026=DIRECTION('center_axis',(0.,0.,-1.));
#16027=DIRECTION('ref_axis',(1.,0.,0.));
#16028=DIRECTION('',(0.,0.,-1.));
#16029=DIRECTION('center_axis',(0.,0.,-1.));
#16030=DIRECTION('ref_axis',(1.,0.,0.));
#16031=DIRECTION('',(0.,0.,-1.));
#16032=DIRECTION('center_axis',(0.,0.,-1.));
#16033=DIRECTION('ref_axis',(0.938009661722287,-0.346609109106558,0.));
#16034=DIRECTION('',(0.,0.,-1.));
#16035=DIRECTION('center_axis',(0.,0.,1.));
#16036=DIRECTION('ref_axis',(1.,0.,0.));
#16037=DIRECTION('center_axis',(0.,0.,-1.));
#16038=DIRECTION('ref_axis',(1.,-3.46775371283602E-14,0.));
#16039=DIRECTION('',(1.22464679914735E-16,-4.2617710824826E-30,-1.));
#16040=DIRECTION('center_axis',(0.,0.,1.));
#16041=DIRECTION('ref_axis',(1.,-3.46775371283602E-14,0.));
#16042=DIRECTION('center_axis',(0.,0.,-1.));
#16043=DIRECTION('ref_axis',(1.,-3.46775371283602E-14,0.));
#16044=DIRECTION('',(1.22464679914735E-16,-4.2617710824826E-30,-1.));
#16045=DIRECTION('center_axis',(0.,0.,-1.));
#16046=DIRECTION('ref_axis',(1.,-3.46775371283602E-14,0.));
#16047=DIRECTION('',(1.22464679914735E-16,-4.2617710824826E-30,-1.));
#16048=DIRECTION('center_axis',(0.,0.,-1.));
#16049=DIRECTION('ref_axis',(1.,-3.46775371283602E-14,0.));
#16050=DIRECTION('',(1.22464679914735E-16,-4.2617710824826E-30,-1.));
#16051=DIRECTION('center_axis',(0.,0.,-1.));
#16052=DIRECTION('ref_axis',(1.,-3.46775371283602E-14,0.));
#16053=DIRECTION('',(1.22464679914735E-16,-4.2617710824826E-30,-1.));
#16054=DIRECTION('center_axis',(0.,0.,-1.));
#16055=DIRECTION('ref_axis',(1.,-3.46775371283602E-14,0.));
#16056=DIRECTION('',(1.22464679914735E-16,-4.2617710824826E-30,-1.));
#16057=DIRECTION('center_axis',(0.,0.,-1.));
#16058=DIRECTION('ref_axis',(1.,-3.46775371283602E-14,0.));
#16059=DIRECTION('',(1.22464679914735E-16,-4.2617710824826E-30,-1.));
#16060=DIRECTION('center_axis',(0.,0.,-1.));
#16061=DIRECTION('ref_axis',(1.,-3.46775371283602E-14,0.));
#16062=DIRECTION('',(1.22464679914735E-16,-4.2617710824826E-30,-1.));
#16063=DIRECTION('center_axis',(0.,0.,-1.));
#16064=DIRECTION('ref_axis',(-0.609168295488507,-0.793040974837761,0.));
#16065=DIRECTION('',(1.22464679914735E-16,-4.2617710824826E-30,-1.));
#16066=DIRECTION('center_axis',(0.,0.,-1.));
#16067=DIRECTION('ref_axis',(1.,-3.46775371283602E-14,0.));
#16068=DIRECTION('center_axis',(0.,0.,-1.));
#16069=DIRECTION('ref_axis',(1.,0.,0.));
#16070=DIRECTION('',(0.,0.,-1.));
#16071=DIRECTION('center_axis',(0.,0.,1.));
#16072=DIRECTION('ref_axis',(1.,0.,0.));
#16073=DIRECTION('',(0.,0.,-1.));
#16074=DIRECTION('center_axis',(0.,0.,-1.));
#16075=DIRECTION('ref_axis',(1.,0.,0.));
#16076=DIRECTION('center_axis',(0.,0.,1.));
#16077=DIRECTION('ref_axis',(1.,0.,0.));
#16078=DIRECTION('center_axis',(0.,0.,-1.));
#16079=DIRECTION('ref_axis',(1.,0.,0.));
#16080=DIRECTION('',(0.,0.,-1.));
#16081=DIRECTION('center_axis',(0.,0.,-1.));
#16082=DIRECTION('ref_axis',(1.,0.,0.));
#16083=DIRECTION('',(0.,0.,-1.));
#16084=DIRECTION('center_axis',(0.,0.,-1.));
#16085=DIRECTION('ref_axis',(1.,0.,0.));
#16086=DIRECTION('',(0.,0.,-1.));
#16087=DIRECTION('center_axis',(0.,0.,-1.));
#16088=DIRECTION('ref_axis',(1.,0.,0.));
#16089=DIRECTION('',(0.,0.,-1.));
#16090=DIRECTION('center_axis',(0.,0.,-1.));
#16091=DIRECTION('ref_axis',(1.,0.,0.));
#16092=DIRECTION('',(0.,0.,-1.));
#16093=DIRECTION('center_axis',(0.,0.,-1.));
#16094=DIRECTION('ref_axis',(1.,0.,0.));
#16095=DIRECTION('',(0.,0.,-1.));
#16096=DIRECTION('center_axis',(0.,0.,-1.));
#16097=DIRECTION('ref_axis',(1.,0.,0.));
#16098=DIRECTION('',(0.,0.,-1.));
#16099=DIRECTION('center_axis',(0.,0.,-1.));
#16100=DIRECTION('ref_axis',(0.938009665675849,-0.346609098407243,0.));
#16101=DIRECTION('',(0.,0.,-1.));
#16102=DIRECTION('center_axis',(0.,0.,1.));
#16103=DIRECTION('ref_axis',(1.,0.,0.));
#16104=DIRECTION('center_axis',(0.,0.,-1.));
#16105=DIRECTION('ref_axis',(1.,-3.46775371283602E-14,0.));
#16106=DIRECTION('',(1.22464679914735E-16,-4.2617710824826E-30,-1.));
#16107=DIRECTION('center_axis',(0.,0.,1.));
#16108=DIRECTION('ref_axis',(1.,-3.46775371283602E-14,0.));
#16109=DIRECTION('center_axis',(0.,0.,-1.));
#16110=DIRECTION('ref_axis',(1.,-3.46775371283602E-14,0.));
#16111=DIRECTION('',(1.22464679914735E-16,-4.2617710824826E-30,-1.));
#16112=DIRECTION('center_axis',(0.,0.,-1.));
#16113=DIRECTION('ref_axis',(1.,-3.46775371283602E-14,0.));
#16114=DIRECTION('',(1.22464679914735E-16,-4.2617710824826E-30,-1.));
#16115=DIRECTION('center_axis',(0.,0.,-1.));
#16116=DIRECTION('ref_axis',(1.,-3.46775371283602E-14,0.));
#16117=DIRECTION('',(1.22464679914735E-16,-4.2617710824826E-30,-1.));
#16118=DIRECTION('center_axis',(0.,0.,-1.));
#16119=DIRECTION('ref_axis',(1.,-3.46775371283602E-14,0.));
#16120=DIRECTION('',(1.22464679914735E-16,-4.2617710824826E-30,-1.));
#16121=DIRECTION('center_axis',(0.,0.,-1.));
#16122=DIRECTION('ref_axis',(1.,-3.46775371283602E-14,0.));
#16123=DIRECTION('',(1.22464679914735E-16,-4.2617710824826E-30,-1.));
#16124=DIRECTION('center_axis',(0.,0.,-1.));
#16125=DIRECTION('ref_axis',(1.,-3.46775371283602E-14,0.));
#16126=DIRECTION('',(1.22464679914735E-16,-4.2617710824826E-30,-1.));
#16127=DIRECTION('center_axis',(0.,0.,-1.));
#16128=DIRECTION('ref_axis',(1.,-3.46775371283602E-14,0.));
#16129=DIRECTION('',(1.22464679914735E-16,-4.2617710824826E-30,-1.));
#16130=DIRECTION('center_axis',(0.,0.,-1.));
#16131=DIRECTION('ref_axis',(-0.609168291270306,-0.79304097807794,0.));
#16132=DIRECTION('',(1.22464679914735E-16,-4.2617710824826E-30,-1.));
#16133=DIRECTION('center_axis',(0.,0.,-1.));
#16134=DIRECTION('ref_axis',(1.,-3.46775371283602E-14,0.));
#16135=DIRECTION('center_axis',(0.,0.,-1.));
#16136=DIRECTION('ref_axis',(1.,0.,0.));
#16137=DIRECTION('',(0.,0.,-1.));
#16138=DIRECTION('center_axis',(0.,0.,1.));
#16139=DIRECTION('ref_axis',(1.,0.,0.));
#16140=DIRECTION('',(0.,0.,-1.));
#16141=DIRECTION('center_axis',(0.,0.,-1.));
#16142=DIRECTION('ref_axis',(1.,0.,0.));
#16143=DIRECTION('center_axis',(0.,0.,1.));
#16144=DIRECTION('ref_axis',(1.,0.,0.));
#16145=DIRECTION('center_axis',(0.,0.,-1.));
#16146=DIRECTION('ref_axis',(1.,0.,0.));
#16147=DIRECTION('',(0.,0.,-1.));
#16148=DIRECTION('center_axis',(0.,0.,-1.));
#16149=DIRECTION('ref_axis',(1.,0.,0.));
#16150=DIRECTION('',(0.,0.,-1.));
#16151=DIRECTION('center_axis',(0.,0.,-1.));
#16152=DIRECTION('ref_axis',(1.,0.,0.));
#16153=DIRECTION('',(0.,0.,-1.));
#16154=DIRECTION('center_axis',(0.,0.,-1.));
#16155=DIRECTION('ref_axis',(1.,0.,0.));
#16156=DIRECTION('',(0.,0.,-1.));
#16157=DIRECTION('center_axis',(0.,0.,-1.));
#16158=DIRECTION('ref_axis',(1.,0.,0.));
#16159=DIRECTION('',(0.,0.,-1.));
#16160=DIRECTION('center_axis',(0.,0.,-1.));
#16161=DIRECTION('ref_axis',(1.,0.,0.));
#16162=DIRECTION('',(0.,0.,-1.));
#16163=DIRECTION('center_axis',(0.,0.,-1.));
#16164=DIRECTION('ref_axis',(1.,0.,0.));
#16165=DIRECTION('',(0.,0.,-1.));
#16166=DIRECTION('center_axis',(0.,0.,-1.));
#16167=DIRECTION('ref_axis',(0.938009652374732,-0.346609134403343,0.));
#16168=DIRECTION('',(0.,0.,-1.));
#16169=DIRECTION('center_axis',(0.,0.,1.));
#16170=DIRECTION('ref_axis',(1.,0.,0.));
#16171=DIRECTION('center_axis',(0.,0.,-1.));
#16172=DIRECTION('ref_axis',(1.,-3.46775371283602E-14,0.));
#16173=DIRECTION('',(1.22464679914735E-16,-4.2617710824826E-30,-1.));
#16174=DIRECTION('center_axis',(0.,0.,1.));
#16175=DIRECTION('ref_axis',(1.,-3.46775371283602E-14,0.));
#16176=DIRECTION('center_axis',(0.,0.,-1.));
#16177=DIRECTION('ref_axis',(1.,-3.46775371283602E-14,0.));
#16178=DIRECTION('',(1.22464679914735E-16,-4.2617710824826E-30,-1.));
#16179=DIRECTION('center_axis',(0.,0.,-1.));
#16180=DIRECTION('ref_axis',(1.,-3.46775371283602E-14,0.));
#16181=DIRECTION('',(1.22464679914735E-16,-4.2617710824826E-30,-1.));
#16182=DIRECTION('center_axis',(0.,0.,-1.));
#16183=DIRECTION('ref_axis',(1.,-3.46775371283602E-14,0.));
#16184=DIRECTION('',(1.22464679914735E-16,-4.2617710824826E-30,-1.));
#16185=DIRECTION('center_axis',(0.,0.,-1.));
#16186=DIRECTION('ref_axis',(1.,-3.46775371283602E-14,0.));
#16187=DIRECTION('',(1.22464679914735E-16,-4.2617710824826E-30,-1.));
#16188=DIRECTION('center_axis',(0.,0.,-1.));
#16189=DIRECTION('ref_axis',(1.,-3.46775371283602E-14,0.));
#16190=DIRECTION('',(1.22464679914735E-16,-4.2617710824826E-30,-1.));
#16191=DIRECTION('center_axis',(0.,0.,-1.));
#16192=DIRECTION('ref_axis',(1.,-3.46775371283602E-14,0.));
#16193=DIRECTION('',(1.22464679914735E-16,-4.2617710824826E-30,-1.));
#16194=DIRECTION('center_axis',(0.,0.,-1.));
#16195=DIRECTION('ref_axis',(1.,-3.46775371283602E-14,0.));
#16196=DIRECTION('',(1.22464679914735E-16,-4.2617710824826E-30,-1.));
#16197=DIRECTION('center_axis',(0.,0.,-1.));
#16198=DIRECTION('ref_axis',(-0.609168287551074,-0.793040980934839,0.));
#16199=DIRECTION('',(1.22464679914735E-16,-4.2617710824826E-30,-1.));
#16200=DIRECTION('center_axis',(0.,0.,-1.));
#16201=DIRECTION('ref_axis',(1.,-3.46775371283602E-14,0.));
#16202=DIRECTION('center_axis',(0.,0.,-1.));
#16203=DIRECTION('ref_axis',(1.,0.,0.));
#16204=DIRECTION('',(0.,0.,-1.));
#16205=DIRECTION('center_axis',(0.,0.,1.));
#16206=DIRECTION('ref_axis',(1.,0.,0.));
#16207=DIRECTION('',(0.,0.,-1.));
#16208=DIRECTION('center_axis',(0.,0.,-1.));
#16209=DIRECTION('ref_axis',(1.,0.,0.));
#16210=DIRECTION('center_axis',(0.,0.,1.));
#16211=DIRECTION('ref_axis',(1.,0.,0.));
#16212=DIRECTION('center_axis',(0.,0.,-1.));
#16213=DIRECTION('ref_axis',(1.,0.,0.));
#16214=DIRECTION('',(0.,0.,-1.));
#16215=DIRECTION('center_axis',(0.,0.,-1.));
#16216=DIRECTION('ref_axis',(1.,0.,0.));
#16217=DIRECTION('',(0.,0.,-1.));
#16218=DIRECTION('center_axis',(0.,0.,-1.));
#16219=DIRECTION('ref_axis',(1.,0.,0.));
#16220=DIRECTION('',(0.,0.,-1.));
#16221=DIRECTION('center_axis',(0.,0.,-1.));
#16222=DIRECTION('ref_axis',(1.,0.,0.));
#16223=DIRECTION('',(0.,0.,-1.));
#16224=DIRECTION('center_axis',(0.,0.,-1.));
#16225=DIRECTION('ref_axis',(1.,0.,0.));
#16226=DIRECTION('',(0.,0.,-1.));
#16227=DIRECTION('center_axis',(0.,0.,-1.));
#16228=DIRECTION('ref_axis',(1.,0.,0.));
#16229=DIRECTION('',(0.,0.,-1.));
#16230=DIRECTION('center_axis',(0.,0.,-1.));
#16231=DIRECTION('ref_axis',(1.,0.,0.));
#16232=DIRECTION('',(0.,0.,-1.));
#16233=DIRECTION('center_axis',(0.,0.,-1.));
#16234=DIRECTION('ref_axis',(0.938009657291017,-0.346609121098665,0.));
#16235=DIRECTION('',(0.,0.,-1.));
#16236=DIRECTION('center_axis',(0.,0.,1.));
#16237=DIRECTION('ref_axis',(1.,0.,0.));
#16238=DIRECTION('center_axis',(0.,0.,-1.));
#16239=DIRECTION('ref_axis',(1.,-4.04571266497535E-14,0.));
#16240=DIRECTION('',(1.22464679914735E-16,-4.9695666632586E-30,-1.));
#16241=DIRECTION('center_axis',(0.,0.,1.));
#16242=DIRECTION('ref_axis',(1.,-4.04571266497535E-14,0.));
#16243=DIRECTION('center_axis',(0.,0.,-1.));
#16244=DIRECTION('ref_axis',(1.,-4.04571266497535E-14,0.));
#16245=DIRECTION('',(1.22464679914735E-16,-4.9695666632586E-30,-1.));
#16246=DIRECTION('center_axis',(0.,0.,-1.));
#16247=DIRECTION('ref_axis',(1.,-4.04571266497535E-14,0.));
#16248=DIRECTION('',(1.22464679914735E-16,-4.9695666632586E-30,-1.));
#16249=DIRECTION('center_axis',(0.,0.,-1.));
#16250=DIRECTION('ref_axis',(1.,-4.04571266497535E-14,0.));
#16251=DIRECTION('',(1.22464679914735E-16,-4.9695666632586E-30,-1.));
#16252=DIRECTION('center_axis',(0.,0.,-1.));
#16253=DIRECTION('ref_axis',(1.,-4.04571266497535E-14,0.));
#16254=DIRECTION('',(1.22464679914735E-16,-4.9695666632586E-30,-1.));
#16255=DIRECTION('center_axis',(0.,0.,-1.));
#16256=DIRECTION('ref_axis',(1.,-4.04571266497535E-14,0.));
#16257=DIRECTION('',(1.22464679914735E-16,-4.9695666632586E-30,-1.));
#16258=DIRECTION('center_axis',(0.,0.,-1.));
#16259=DIRECTION('ref_axis',(1.,-4.04571266497535E-14,0.));
#16260=DIRECTION('',(1.22464679914735E-16,-4.9695666632586E-30,-1.));
#16261=DIRECTION('center_axis',(0.,0.,-1.));
#16262=DIRECTION('ref_axis',(1.,-4.04571266497535E-14,0.));
#16263=DIRECTION('',(1.22464679914735E-16,-4.9695666632586E-30,-1.));
#16264=DIRECTION('center_axis',(0.,0.,-1.));
#16265=DIRECTION('ref_axis',(-0.609168284311011,-0.793040983423669,0.));
#16266=DIRECTION('',(1.22464679914735E-16,-4.9695666632586E-30,-1.));
#16267=DIRECTION('center_axis',(0.,0.,-1.));
#16268=DIRECTION('ref_axis',(1.,-4.04571266497535E-14,0.));
#16269=DIRECTION('center_axis',(0.,0.,-1.));
#16270=DIRECTION('ref_axis',(1.,0.,0.));
#16271=DIRECTION('',(0.,0.,-1.));
#16272=DIRECTION('center_axis',(0.,0.,1.));
#16273=DIRECTION('ref_axis',(1.,0.,0.));
#16274=DIRECTION('',(0.,0.,-1.));
#16275=DIRECTION('center_axis',(0.,0.,-1.));
#16276=DIRECTION('ref_axis',(1.,0.,0.));
#16277=DIRECTION('center_axis',(0.,0.,1.));
#16278=DIRECTION('ref_axis',(1.,0.,0.));
#16279=DIRECTION('center_axis',(0.,0.,-1.));
#16280=DIRECTION('ref_axis',(1.,0.,0.));
#16281=DIRECTION('',(0.,0.,-1.));
#16282=DIRECTION('center_axis',(0.,0.,-1.));
#16283=DIRECTION('ref_axis',(1.,0.,0.));
#16284=DIRECTION('',(0.,0.,-1.));
#16285=DIRECTION('center_axis',(0.,0.,-1.));
#16286=DIRECTION('ref_axis',(1.,0.,0.));
#16287=DIRECTION('',(0.,0.,-1.));
#16288=DIRECTION('center_axis',(0.,0.,-1.));
#16289=DIRECTION('ref_axis',(1.,0.,0.));
#16290=DIRECTION('',(0.,0.,-1.));
#16291=DIRECTION('center_axis',(0.,0.,-1.));
#16292=DIRECTION('ref_axis',(1.,0.,0.));
#16293=DIRECTION('',(0.,0.,-1.));
#16294=DIRECTION('center_axis',(0.,0.,-1.));
#16295=DIRECTION('ref_axis',(1.,0.,0.));
#16296=DIRECTION('',(0.,0.,-1.));
#16297=DIRECTION('center_axis',(0.,0.,-1.));
#16298=DIRECTION('ref_axis',(1.,0.,0.));
#16299=DIRECTION('',(0.,0.,-1.));
#16300=DIRECTION('center_axis',(0.,0.,-1.));
#16301=DIRECTION('ref_axis',(0.938009652374729,-0.346609134403351,0.));
#16302=DIRECTION('',(0.,0.,-1.));
#16303=DIRECTION('center_axis',(0.,0.,1.));
#16304=DIRECTION('ref_axis',(1.,0.,0.));
#16305=DIRECTION('center_axis',(0.,0.,-1.));
#16306=DIRECTION('ref_axis',(1.,-2.88979476069668E-14,0.));
#16307=DIRECTION('',(1.22464679914735E-16,-3.5539755017066E-30,-1.));
#16308=DIRECTION('center_axis',(0.,0.,1.));
#16309=DIRECTION('ref_axis',(1.,-2.88979476069668E-14,0.));
#16310=DIRECTION('center_axis',(0.,0.,-1.));
#16311=DIRECTION('ref_axis',(1.,-2.88979476069668E-14,0.));
#16312=DIRECTION('',(1.22464679914735E-16,-3.5539755017066E-30,-1.));
#16313=DIRECTION('center_axis',(0.,0.,-1.));
#16314=DIRECTION('ref_axis',(1.,-2.88979476069668E-14,0.));
#16315=DIRECTION('',(1.22464679914735E-16,-3.5539755017066E-30,-1.));
#16316=DIRECTION('center_axis',(0.,0.,-1.));
#16317=DIRECTION('ref_axis',(1.,-2.88979476069668E-14,0.));
#16318=DIRECTION('',(1.22464679914735E-16,-3.5539755017066E-30,-1.));
#16319=DIRECTION('center_axis',(0.,0.,-1.));
#16320=DIRECTION('ref_axis',(1.,-2.88979476069668E-14,0.));
#16321=DIRECTION('',(1.22464679914735E-16,-3.5539755017066E-30,-1.));
#16322=DIRECTION('center_axis',(0.,0.,-1.));
#16323=DIRECTION('ref_axis',(1.,-2.88979476069668E-14,0.));
#16324=DIRECTION('',(1.22464679914735E-16,-3.5539755017066E-30,-1.));
#16325=DIRECTION('center_axis',(0.,0.,-1.));
#16326=DIRECTION('ref_axis',(1.,-2.88979476069668E-14,0.));
#16327=DIRECTION('',(1.22464679914735E-16,-3.5539755017066E-30,-1.));
#16328=DIRECTION('center_axis',(0.,0.,-1.));
#16329=DIRECTION('ref_axis',(1.,-2.88979476069668E-14,0.));
#16330=DIRECTION('',(1.22464679914735E-16,-3.5539755017066E-30,-1.));
#16331=DIRECTION('center_axis',(0.,0.,-1.));
#16332=DIRECTION('ref_axis',(-0.609168287551063,-0.793040980934848,0.));
#16333=DIRECTION('',(1.22464679914735E-16,-3.5539755017066E-30,-1.));
#16334=DIRECTION('center_axis',(0.,0.,-1.));
#16335=DIRECTION('ref_axis',(1.,-2.88979476069668E-14,0.));
#16336=DIRECTION('center_axis',(0.,0.,-1.));
#16337=DIRECTION('ref_axis',(1.,0.,0.));
#16338=DIRECTION('',(0.,0.,-1.));
#16339=DIRECTION('center_axis',(0.,0.,1.));
#16340=DIRECTION('ref_axis',(1.,0.,0.));
#16341=DIRECTION('',(0.,0.,-1.));
#16342=DIRECTION('center_axis',(0.,0.,-1.));
#16343=DIRECTION('ref_axis',(1.,0.,0.));
#16344=DIRECTION('center_axis',(0.,0.,1.));
#16345=DIRECTION('ref_axis',(1.,0.,0.));
#16346=DIRECTION('center_axis',(0.,0.,-1.));
#16347=DIRECTION('ref_axis',(1.,0.,0.));
#16348=DIRECTION('',(0.,0.,-1.));
#16349=DIRECTION('center_axis',(0.,0.,-1.));
#16350=DIRECTION('ref_axis',(1.,0.,0.));
#16351=DIRECTION('',(0.,0.,-1.));
#16352=DIRECTION('center_axis',(0.,0.,-1.));
#16353=DIRECTION('ref_axis',(1.,0.,0.));
#16354=DIRECTION('',(0.,0.,-1.));
#16355=DIRECTION('center_axis',(0.,0.,-1.));
#16356=DIRECTION('ref_axis',(1.,0.,0.));
#16357=DIRECTION('',(0.,0.,-1.));
#16358=DIRECTION('center_axis',(0.,0.,-1.));
#16359=DIRECTION('ref_axis',(1.,0.,0.));
#16360=DIRECTION('',(0.,0.,-1.));
#16361=DIRECTION('center_axis',(0.,0.,-1.));
#16362=DIRECTION('ref_axis',(1.,0.,0.));
#16363=DIRECTION('',(0.,0.,-1.));
#16364=DIRECTION('center_axis',(0.,0.,-1.));
#16365=DIRECTION('ref_axis',(1.,0.,0.));
#16366=DIRECTION('',(0.,0.,-1.));
#16367=DIRECTION('center_axis',(0.,0.,-1.));
#16368=DIRECTION('ref_axis',(0.93800966172229,-0.346609109106549,0.));
#16369=DIRECTION('',(0.,0.,-1.));
#16370=DIRECTION('center_axis',(0.,0.,1.));
#16371=DIRECTION('ref_axis',(1.,0.,0.));
#16372=DIRECTION('center_axis',(0.,0.,-1.));
#16373=DIRECTION('ref_axis',(1.,-3.32326397480119E-14,0.));
#16374=DIRECTION('',(1.22464679914735E-16,-4.0848221872886E-30,-1.));
#16375=DIRECTION('center_axis',(0.,0.,1.));
#16376=DIRECTION('ref_axis',(1.,-3.32326397480119E-14,0.));
#16377=DIRECTION('center_axis',(0.,0.,-1.));
#16378=DIRECTION('ref_axis',(1.,-3.32326397480119E-14,0.));
#16379=DIRECTION('',(1.22464679914735E-16,-4.0848221872886E-30,-1.));
#16380=DIRECTION('center_axis',(0.,0.,-1.));
#16381=DIRECTION('ref_axis',(1.,-3.32326397480119E-14,0.));
#16382=DIRECTION('',(1.22464679914735E-16,-4.0848221872886E-30,-1.));
#16383=DIRECTION('center_axis',(0.,0.,-1.));
#16384=DIRECTION('ref_axis',(1.,-3.32326397480119E-14,0.));
#16385=DIRECTION('',(1.22464679914735E-16,-4.0848221872886E-30,-1.));
#16386=DIRECTION('center_axis',(0.,0.,-1.));
#16387=DIRECTION('ref_axis',(1.,-3.32326397480119E-14,0.));
#16388=DIRECTION('',(1.22464679914735E-16,-4.0848221872886E-30,-1.));
#16389=DIRECTION('center_axis',(0.,0.,-1.));
#16390=DIRECTION('ref_axis',(1.,-3.32326397480119E-14,0.));
#16391=DIRECTION('',(1.22464679914735E-16,-4.0848221872886E-30,-1.));
#16392=DIRECTION('center_axis',(0.,0.,-1.));
#16393=DIRECTION('ref_axis',(1.,-3.32326397480119E-14,0.));
#16394=DIRECTION('',(1.22464679914735E-16,-4.0848221872886E-30,-1.));
#16395=DIRECTION('center_axis',(0.,0.,-1.));
#16396=DIRECTION('ref_axis',(1.,-3.32326397480119E-14,0.));
#16397=DIRECTION('',(1.22464679914735E-16,-4.0848221872886E-30,-1.));
#16398=DIRECTION('center_axis',(0.,0.,-1.));
#16399=DIRECTION('ref_axis',(-0.609168295488513,-0.793040974837757,0.));
#16400=DIRECTION('',(1.22464679914735E-16,-4.0848221872886E-30,-1.));
#16401=DIRECTION('center_axis',(0.,0.,-1.));
#16402=DIRECTION('ref_axis',(1.,-3.32326397480119E-14,0.));
#16403=DIRECTION('center_axis',(0.,0.,-1.));
#16404=DIRECTION('ref_axis',(1.,0.,0.));
#16405=DIRECTION('center_axis',(0.,0.,-1.));
#16406=DIRECTION('ref_axis',(1.,0.,0.));
#16407=DIRECTION('',(0.,0.,-1.));
#16408=DIRECTION('center_axis',(0.,0.,-1.));
#16409=DIRECTION('ref_axis',(1.,0.,0.));
#16410=DIRECTION('center_axis',(0.,0.,-1.));
#16411=DIRECTION('ref_axis',(1.,0.,0.));
#16412=DIRECTION('center_axis',(0.,0.,1.));
#16413=DIRECTION('ref_axis',(1.,0.,0.));
#16414=DIRECTION('center_axis',(0.,0.,-1.));
#16415=DIRECTION('ref_axis',(1.,0.,0.));
#16416=DIRECTION('center_axis',(0.,0.,-1.));
#16417=DIRECTION('ref_axis',(1.,0.,0.));
#16418=DIRECTION('',(0.,0.,-1.));
#16419=DIRECTION('center_axis',(0.,0.,-1.));
#16420=DIRECTION('ref_axis',(1.,0.,0.));
#16421=DIRECTION('center_axis',(0.,0.,-1.));
#16422=DIRECTION('ref_axis',(1.,0.,0.));
#16423=DIRECTION('center_axis',(0.,0.,1.));
#16424=DIRECTION('ref_axis',(1.,0.,0.));
#16425=DIRECTION('center_axis',(0.,0.,-1.));
#16426=DIRECTION('ref_axis',(1.,0.,0.));
#16427=DIRECTION('center_axis',(0.,0.,-1.));
#16428=DIRECTION('ref_axis',(1.,0.,0.));
#16429=DIRECTION('',(0.,0.,-1.));
#16430=DIRECTION('center_axis',(0.,0.,-1.));
#16431=DIRECTION('ref_axis',(1.,0.,0.));
#16432=DIRECTION('center_axis',(0.,0.,-1.));
#16433=DIRECTION('ref_axis',(1.,0.,0.));
#16434=DIRECTION('center_axis',(0.,0.,1.));
#16435=DIRECTION('ref_axis',(1.,0.,0.));
#16436=DIRECTION('center_axis',(0.,0.,-1.));
#16437=DIRECTION('ref_axis',(1.,0.,0.));
#16438=DIRECTION('center_axis',(0.,0.,-1.));
#16439=DIRECTION('ref_axis',(1.,0.,0.));
#16440=DIRECTION('',(0.,0.,-1.));
#16441=DIRECTION('center_axis',(0.,0.,-1.));
#16442=DIRECTION('ref_axis',(1.,0.,0.));
#16443=DIRECTION('center_axis',(0.,0.,-1.));
#16444=DIRECTION('ref_axis',(1.,0.,0.));
#16445=DIRECTION('center_axis',(0.,0.,1.));
#16446=DIRECTION('ref_axis',(1.,0.,0.));
#16447=DIRECTION('center_axis',(0.,0.,-1.));
#16448=DIRECTION('ref_axis',(1.,0.,0.));
#16449=DIRECTION('',(0.,0.,-1.));
#16450=DIRECTION('center_axis',(0.,0.,1.));
#16451=DIRECTION('ref_axis',(1.,0.,0.));
#16452=DIRECTION('center_axis',(0.,0.,-1.));
#16453=DIRECTION('ref_axis',(1.,0.,0.));
#16454=DIRECTION('',(0.,0.,-1.));
#16455=DIRECTION('center_axis',(0.,0.,1.));
#16456=DIRECTION('ref_axis',(1.,0.,0.));
#16457=DIRECTION('center_axis',(0.,0.,-1.));
#16458=DIRECTION('ref_axis',(1.,0.,0.));
#16459=DIRECTION('',(0.,0.,-1.));
#16460=DIRECTION('center_axis',(0.,0.,1.));
#16461=DIRECTION('ref_axis',(1.,0.,0.));
#16462=DIRECTION('center_axis',(0.,0.,-1.));
#16463=DIRECTION('ref_axis',(1.,0.,0.));
#16464=DIRECTION('',(0.,0.,-1.));
#16465=DIRECTION('center_axis',(0.,0.,1.));
#16466=DIRECTION('ref_axis',(1.,0.,0.));
#16467=DIRECTION('center_axis',(0.,0.,1.));
#16468=DIRECTION('ref_axis',(1.,0.,0.));
#16469=DIRECTION('center_axis',(0.,0.,-1.));
#16470=DIRECTION('ref_axis',(1.,-3.32326397480119E-14,0.));
#16471=DIRECTION('center_axis',(0.,0.,-1.));
#16472=DIRECTION('ref_axis',(1.,0.,0.));
#16473=DIRECTION('center_axis',(0.,0.,1.));
#16474=DIRECTION('ref_axis',(1.,0.,0.));
#16475=DIRECTION('center_axis',(0.,0.,-1.));
#16476=DIRECTION('ref_axis',(1.,-2.88979476069668E-14,0.));
#16477=DIRECTION('center_axis',(0.,0.,-1.));
#16478=DIRECTION('ref_axis',(1.,0.,0.));
#16479=DIRECTION('center_axis',(0.,0.,1.));
#16480=DIRECTION('ref_axis',(1.,0.,0.));
#16481=DIRECTION('center_axis',(0.,0.,-1.));
#16482=DIRECTION('ref_axis',(1.,-4.04571266497535E-14,0.));
#16483=DIRECTION('center_axis',(0.,0.,-1.));
#16484=DIRECTION('ref_axis',(1.,0.,0.));
#16485=DIRECTION('center_axis',(0.,0.,1.));
#16486=DIRECTION('ref_axis',(1.,0.,0.));
#16487=DIRECTION('center_axis',(0.,0.,-1.));
#16488=DIRECTION('ref_axis',(1.,-3.46775371283602E-14,0.));
#16489=DIRECTION('center_axis',(0.,0.,-1.));
#16490=DIRECTION('ref_axis',(1.,0.,0.));
#16491=DIRECTION('center_axis',(0.,0.,1.));
#16492=DIRECTION('ref_axis',(1.,0.,0.));
#16493=DIRECTION('center_axis',(0.,0.,-1.));
#16494=DIRECTION('ref_axis',(1.,-3.46775371283602E-14,0.));
#16495=DIRECTION('center_axis',(0.,0.,-1.));
#16496=DIRECTION('ref_axis',(1.,0.,0.));
#16497=DIRECTION('center_axis',(0.,0.,1.));
#16498=DIRECTION('ref_axis',(1.,0.,0.));
#16499=DIRECTION('center_axis',(0.,0.,-1.));
#16500=DIRECTION('ref_axis',(1.,-3.46775371283602E-14,0.));
#16501=DIRECTION('center_axis',(0.,0.,-1.));
#16502=DIRECTION('ref_axis',(1.,0.,0.));
#16503=DIRECTION('center_axis',(0.,0.,1.));
#16504=DIRECTION('ref_axis',(1.,0.,0.));
#16505=DIRECTION('center_axis',(0.,0.,-1.));
#16506=DIRECTION('ref_axis',(1.,-3.46775371283602E-14,0.));
#16507=DIRECTION('center_axis',(0.,0.,-1.));
#16508=DIRECTION('ref_axis',(1.,0.,0.));
#16509=DIRECTION('center_axis',(0.,0.,1.));
#16510=DIRECTION('ref_axis',(1.,0.,0.));
#16511=DIRECTION('center_axis',(0.,0.,-1.));
#16512=DIRECTION('ref_axis',(1.,-3.61224345087086E-14,0.));
#16513=DIRECTION('center_axis',(0.,0.,-1.));
#16514=DIRECTION('ref_axis',(1.,0.,0.));
#16515=DIRECTION('center_axis',(-1.,0.,0.));
#16516=DIRECTION('ref_axis',(0.,1.,0.));
#16517=DIRECTION('',(0.,0.,1.));
#16518=DIRECTION('',(0.,1.,0.));
#16519=DIRECTION('',(0.,0.,-1.));
#16520=DIRECTION('',(0.,1.,0.));
#16521=DIRECTION('center_axis',(0.,1.,0.));
#16522=DIRECTION('ref_axis',(1.,0.,0.));
#16523=DIRECTION('',(0.,0.,-1.));
#16524=DIRECTION('',(1.,0.,0.));
#16525=DIRECTION('',(1.,0.,0.));
#16526=DIRECTION('',(0.,0.,-1.));
#16527=DIRECTION('',(1.,0.,0.));
#16528=DIRECTION('',(0.,0.,1.));
#16529=DIRECTION('',(-1.,0.,0.));
#16530=DIRECTION('',(0.,0.,1.));
#16531=DIRECTION('',(1.,0.,0.));
#16532=DIRECTION('',(0.,0.,-1.));
#16533=DIRECTION('',(-1.,0.,0.));
#16534=DIRECTION('center_axis',(1.,0.,0.));
#16535=DIRECTION('ref_axis',(0.,-1.,0.));
#16536=DIRECTION('',(0.,0.,-1.));
#16537=DIRECTION('',(0.,-1.,0.));
#16538=DIRECTION('',(0.,-1.,0.));
#16539=DIRECTION('center_axis',(0.,0.,-1.));
#16540=DIRECTION('ref_axis',(-1.,0.,0.));
#16541=DIRECTION('center_axis',(0.,0.,-1.));
#16542=DIRECTION('ref_axis',(1.,0.,0.));
#16543=DIRECTION('center_axis',(0.,-1.,0.));
#16544=DIRECTION('ref_axis',(-1.,0.,0.));
#16545=DIRECTION('',(0.,0.,-1.));
#16546=DIRECTION('',(-1.,0.,0.));
#16547=DIRECTION('',(0.,0.,-1.));
#16548=DIRECTION('',(-1.,0.,0.));
#16549=DIRECTION('',(0.,0.,-1.));
#16550=DIRECTION('',(-1.,0.,0.));
#16551=DIRECTION('',(0.,0.,1.));
#16552=DIRECTION('',(1.,0.,0.));
#16553=DIRECTION('',(0.,0.,1.));
#16554=DIRECTION('',(-1.,0.,0.));
#16555=DIRECTION('',(0.,0.,-1.));
#16556=DIRECTION('',(1.,0.,0.));
#16557=DIRECTION('center_axis',(1.,0.,0.));
#16558=DIRECTION('ref_axis',(0.,-1.,0.));
#16559=DIRECTION('',(0.,0.,1.));
#16560=DIRECTION('',(0.,-1.,0.));
#16561=DIRECTION('',(0.,-1.,0.));
#16562=DIRECTION('center_axis',(-1.,0.,0.));
#16563=DIRECTION('ref_axis',(0.,1.,0.));
#16564=DIRECTION('',(0.,0.,-1.));
#16565=DIRECTION('',(0.,1.,0.));
#16566=DIRECTION('',(0.,1.,0.));
#16567=DIRECTION('center_axis',(0.,0.,-1.));
#16568=DIRECTION('ref_axis',(-1.,0.,0.));
#16569=DIRECTION('center_axis',(0.,0.,-1.));
#16570=DIRECTION('ref_axis',(1.,0.,0.));
#16571=DIRECTION('center_axis',(0.,0.,-1.));
#16572=DIRECTION('ref_axis',(-1.,0.,0.));
#16573=DIRECTION('',(0.,-1.,0.));
#16574=DIRECTION('',(1.,0.,0.));
#16575=DIRECTION('center_axis',(0.,0.,1.));
#16576=DIRECTION('ref_axis',(1.,0.,0.));
#16577=DIRECTION('',(1.,0.,0.));
#16578=DIRECTION('',(0.,1.,0.));
#16579=DIRECTION('center_axis',(1.,0.,0.));
#16580=DIRECTION('ref_axis',(0.,-1.,0.));
#16581=DIRECTION('',(0.,1.,0.));
#16582=DIRECTION('',(0.,0.,-1.));
#16583=DIRECTION('center_axis',(0.,0.,1.));
#16584=DIRECTION('ref_axis',(1.,0.,0.));
#16585=DIRECTION('center_axis',(0.,0.,1.));
#16586=DIRECTION('ref_axis',(1.,0.,0.));
#16587=DIRECTION('',(-1.,0.,0.));
#16588=DIRECTION('',(0.,1.,0.));
#16589=DIRECTION('',(-1.,0.,0.));
#16590=DIRECTION('',(0.,1.,0.));
#16591=DIRECTION('center_axis',(0.,0.,-1.));
#16592=DIRECTION('ref_axis',(1.,0.,0.));
#16593=DIRECTION('',(1.,0.,0.));
#16594=DIRECTION('',(0.,-1.,0.));
#16595=DIRECTION('center_axis',(0.,0.,1.));
#16596=DIRECTION('ref_axis',(1.,0.,0.));
#16597=DIRECTION('',(0.,1.,0.));
#16598=DIRECTION('',(1.,0.,0.));
#16599=DIRECTION('center_axis',(0.,0.,-1.));
#16600=DIRECTION('ref_axis',(1.,0.,0.));
#16601=DIRECTION('',(0.,-1.,0.));
#16602=DIRECTION('',(-1.,0.,0.));
#16603=DIRECTION('',(0.,-1.,0.));
#16604=DIRECTION('',(-1.,0.,0.));
#16605=DIRECTION('center_axis',(0.,0.,1.));
#16606=DIRECTION('ref_axis',(1.,0.,0.));
#16607=DIRECTION('center_axis',(0.,0.,1.));
#16608=DIRECTION('ref_axis',(1.,0.,0.));
#16609=DIRECTION('',(0.,-1.,0.));
#16610=DIRECTION('',(-1.,0.,0.));
#16611=DIRECTION('center_axis',(1.,0.,0.));
#16612=DIRECTION('ref_axis',(0.,-1.,0.));
#16613=DIRECTION('',(0.,0.,-1.));
#16614=DIRECTION('center_axis',(0.,0.,-1.));
#16615=DIRECTION('ref_axis',(-1.,0.,0.));
#16616=DIRECTION('',(0.,1.,0.));
#16617=DIRECTION('',(-1.,0.,0.));
#16618=DIRECTION('center_axis',(0.,0.,1.));
#16619=DIRECTION('ref_axis',(1.,0.,0.));
#16620=DIRECTION('',(-1.,0.,0.));
#16621=DIRECTION('',(0.,-1.,0.));
#16622=DIRECTION('center_axis',(-1.,0.,0.));
#16623=DIRECTION('ref_axis',(0.,1.,0.));
#16624=DIRECTION('',(0.,-1.,0.));
#16625=DIRECTION('',(0.,0.,-1.));
#16626=DIRECTION('center_axis',(0.,0.,1.));
#16627=DIRECTION('ref_axis',(1.,0.,0.));
#16628=DIRECTION('',(0.,1.,0.));
#16629=DIRECTION('',(1.,0.,0.));
#16630=DIRECTION('center_axis',(-1.,0.,0.));
#16631=DIRECTION('ref_axis',(0.,1.,0.));
#16632=DIRECTION('',(0.,1.,0.));
#16633=DIRECTION('',(0.,0.,-1.));
#16634=DIRECTION('center_axis',(0.,0.,1.));
#16635=DIRECTION('ref_axis',(1.,0.,0.));
#16636=DIRECTION('center_axis',(0.,0.,1.));
#16637=DIRECTION('ref_axis',(1.,0.,0.));
#16638=DIRECTION('',(1.,0.,0.));
#16639=DIRECTION('',(0.,-1.,0.));
#16640=DIRECTION('',(1.,0.,0.));
#16641=DIRECTION('',(0.,-1.,0.));
#16642=DIRECTION('center_axis',(0.,0.,-1.));
#16643=DIRECTION('ref_axis',(1.,0.,0.));
#16644=DIRECTION('',(-1.,0.,0.));
#16645=DIRECTION('center_axis',(-1.,0.,0.));
#16646=DIRECTION('ref_axis',(0.,1.,0.));
#16647=DIRECTION('',(0.,0.,-1.));
#16648=DIRECTION('',(0.,-1.,0.));
#16649=DIRECTION('center_axis',(0.,0.,1.));
#16650=DIRECTION('ref_axis',(1.,0.,0.));
#16651=DIRECTION('',(-1.,0.,0.));
#16652=DIRECTION('',(0.,1.,0.));
#16653=DIRECTION('center_axis',(0.,0.,1.));
#16654=DIRECTION('ref_axis',(1.,0.,0.));
#16655=DIRECTION('',(0.,1.,0.));
#16656=DIRECTION('',(1.,0.,0.));
#16657=DIRECTION('',(0.,-1.,0.));
#16658=DIRECTION('center_axis',(1.,0.,0.));
#16659=DIRECTION('ref_axis',(0.,-1.,0.));
#16660=DIRECTION('',(0.,0.,-1.));
#16661=DIRECTION('center_axis',(0.,0.,1.));
#16662=DIRECTION('ref_axis',(1.,0.,0.));
#16663=DIRECTION('',(0.,0.,-1.));
#16664=DIRECTION('',(0.,0.,1.));
#16665=DIRECTION('',(0.,0.,-1.));
#16666=DIRECTION('center_axis',(0.,0.,1.));
#16667=DIRECTION('ref_axis',(1.,0.,0.));
#16668=DIRECTION('',(0.,0.,1.));
#16669=DIRECTION('center_axis',(0.,0.,-1.));
#16670=DIRECTION('ref_axis',(1.,0.,0.));
#16671=DIRECTION('',(0.,0.,-1.));
#16672=DIRECTION('',(0.,0.,1.));
#16673=DIRECTION('',(0.,0.,-1.));
#16674=DIRECTION('center_axis',(0.,0.,1.));
#16675=DIRECTION('ref_axis',(1.,0.,0.));
#16676=DIRECTION('',(0.,0.,-1.));
#16677=DIRECTION('center_axis',(0.,0.,-1.));
#16678=DIRECTION('ref_axis',(1.,0.,0.));
#16679=DIRECTION('center_axis',(0.,0.,1.));
#16680=DIRECTION('ref_axis',(1.,0.,0.));
#16681=DIRECTION('',(0.,0.,1.));
#16682=DIRECTION('center_axis',(0.,1.,0.));
#16683=DIRECTION('ref_axis',(1.,0.,0.));
#16684=DIRECTION('',(0.,0.,-1.));
#16685=DIRECTION('',(0.,0.,-1.));
#16686=DIRECTION('center_axis',(0.,1.,0.));
#16687=DIRECTION('ref_axis',(1.,0.,0.));
#16688=DIRECTION('',(0.,0.,-1.));
#16689=DIRECTION('center_axis',(-1.,0.,0.));
#16690=DIRECTION('ref_axis',(0.,1.,0.));
#16691=DIRECTION('center_axis',(0.,-1.,0.));
#16692=DIRECTION('ref_axis',(-1.,0.,0.));
#16693=DIRECTION('',(0.,0.,-1.));
#16694=DIRECTION('center_axis',(0.,-1.,0.));
#16695=DIRECTION('ref_axis',(-1.,0.,0.));
#16696=DIRECTION('',(-1.,0.,0.));
#16697=DIRECTION('',(0.,0.,-1.));
#16698=DIRECTION('',(0.,0.,-1.));
#16699=DIRECTION('center_axis',(1.,0.,0.));
#16700=DIRECTION('ref_axis',(0.,-1.,0.));
#16701=DIRECTION('',(0.,-1.,0.));
#16702=DIRECTION('center_axis',(0.,-1.,0.));
#16703=DIRECTION('ref_axis',(-1.,0.,0.));
#16704=DIRECTION('',(0.,0.,-1.));
#16705=DIRECTION('',(0.,0.,-1.));
#16706=DIRECTION('',(-1.,0.,0.));
#16707=DIRECTION('center_axis',(0.,0.,-1.));
#16708=DIRECTION('ref_axis',(-1.,0.,0.));
#16709=DIRECTION('center_axis',(0.,0.,-1.));
#16710=DIRECTION('ref_axis',(1.,0.,0.));
#16711=DIRECTION('',(0.,-1.,0.));
#16712=DIRECTION('',(1.,0.,0.));
#16713=DIRECTION('center_axis',(0.,0.,-1.));
#16714=DIRECTION('ref_axis',(1.,0.,0.));
#16715=DIRECTION('center_axis',(1.,0.,0.));
#16716=DIRECTION('ref_axis',(0.,-1.,0.));
#16717=DIRECTION('',(0.,0.,1.));
#16718=DIRECTION('',(0.,1.,0.));
#16719=DIRECTION('',(0.,0.,1.));
#16720=DIRECTION('',(0.,-1.,0.));
#16721=DIRECTION('',(0.,0.,-1.));
#16722=DIRECTION('',(0.,1.,0.));
#16723=DIRECTION('',(0.,0.,-1.));
#16724=DIRECTION('',(0.,0.,-1.));
#16725=DIRECTION('center_axis',(0.,1.,0.));
#16726=DIRECTION('ref_axis',(1.,0.,0.));
#16727=DIRECTION('',(0.,0.,1.));
#16728=DIRECTION('center_axis',(0.,-1.,0.));
#16729=DIRECTION('ref_axis',(-1.,0.,0.));
#16730=DIRECTION('',(0.,0.,1.));
#16731=DIRECTION('',(-1.,0.,0.));
#16732=DIRECTION('',(0.,0.,-1.));
#16733=DIRECTION('center_axis',(-1.,0.,0.));
#16734=DIRECTION('ref_axis',(0.,1.,0.));
#16735=DIRECTION('',(0.,0.,-1.));
#16736=DIRECTION('',(0.,1.,0.));
#16737=DIRECTION('',(0.,0.,-1.));
#16738=DIRECTION('',(0.,1.,0.));
#16739=DIRECTION('',(0.,0.,1.));
#16740=DIRECTION('',(0.,-1.,0.));
#16741=DIRECTION('',(0.,0.,1.));
#16742=DIRECTION('',(0.,1.,0.));
#16743=DIRECTION('',(0.,0.,-1.));
#16744=DIRECTION('',(0.,-1.,0.));
#16745=DIRECTION('center_axis',(0.,1.,0.));
#16746=DIRECTION('ref_axis',(1.,0.,0.));
#16747=DIRECTION('',(0.,0.,-1.));
#16748=DIRECTION('',(1.,0.,0.));
#16749=DIRECTION('',(1.,0.,0.));
#16750=DIRECTION('center_axis',(0.,0.,-1.));
#16751=DIRECTION('ref_axis',(-1.,0.,0.));
#16752=DIRECTION('center_axis',(0.,0.,-1.));
#16753=DIRECTION('ref_axis',(1.,0.,0.));
#16754=DIRECTION('center_axis',(0.,-1.,0.));
#16755=DIRECTION('ref_axis',(-1.,0.,0.));
#16756=DIRECTION('',(1.,0.,0.));
#16757=DIRECTION('',(-1.,0.,0.));
#16758=DIRECTION('center_axis',(0.,0.,1.));
#16759=DIRECTION('ref_axis',(1.,0.,0.));
#16760=DIRECTION('',(-1.,0.,0.));
#16761=DIRECTION('',(0.,1.,0.));
#16762=DIRECTION('center_axis',(0.,-1.,0.));
#16763=DIRECTION('ref_axis',(-1.,0.,0.));
#16764=DIRECTION('',(0.,0.,-1.));
#16765=DIRECTION('center_axis',(0.,0.,1.));
#16766=DIRECTION('ref_axis',(1.,0.,0.));
#16767=DIRECTION('',(0.,0.,-1.));
#16768=DIRECTION('center_axis',(0.,0.,1.));
#16769=DIRECTION('ref_axis',(1.,0.,0.));
#16770=DIRECTION('center_axis',(0.,0.,1.));
#16771=DIRECTION('ref_axis',(1.,0.,0.));
#16772=DIRECTION('center_axis',(0.,-1.,0.));
#16773=DIRECTION('ref_axis',(-1.,0.,0.));
#16774=DIRECTION('',(-1.,0.,0.));
#16775=DIRECTION('',(0.,0.,-1.));
#16776=DIRECTION('center_axis',(0.,0.,1.));
#16777=DIRECTION('ref_axis',(1.,0.,0.));
#16778=DIRECTION('',(1.,0.,0.));
#16779=DIRECTION('',(0.,-1.,0.));
#16780=DIRECTION('center_axis',(0.,0.,1.));
#16781=DIRECTION('ref_axis',(1.,0.,0.));
#16782=DIRECTION('',(0.,1.,0.));
#16783=DIRECTION('',(1.,0.,0.));
#16784=DIRECTION('center_axis',(0.,-1.,0.));
#16785=DIRECTION('ref_axis',(-1.,0.,0.));
#16786=DIRECTION('',(-1.,0.,0.));
#16787=DIRECTION('center_axis',(0.,0.,-1.));
#16788=DIRECTION('ref_axis',(-1.,0.,0.));
#16789=DIRECTION('',(1.,0.,0.));
#16790=DIRECTION('',(0.,1.,0.));
#16791=DIRECTION('',(0.,1.,0.));
#16792=DIRECTION('center_axis',(0.,1.,0.));
#16793=DIRECTION('ref_axis',(1.,0.,0.));
#16794=DIRECTION('',(-1.,0.,0.));
#16795=DIRECTION('center_axis',(0.,0.,-1.));
#16796=DIRECTION('ref_axis',(-1.,0.,0.));
#16797=DIRECTION('',(0.,-1.,0.));
#16798=DIRECTION('',(0.,-1.,0.));
#16799=DIRECTION('',(1.,0.,0.));
#16800=DIRECTION('center_axis',(0.,0.,1.));
#16801=DIRECTION('ref_axis',(1.,0.,0.));
#16802=DIRECTION('',(-1.,0.,0.));
#16803=DIRECTION('',(0.,1.,0.));
#16804=DIRECTION('',(1.,0.,0.));
#16805=DIRECTION('center_axis',(0.,1.,0.));
#16806=DIRECTION('ref_axis',(1.,0.,0.));
#16807=DIRECTION('center_axis',(0.,0.,1.));
#16808=DIRECTION('ref_axis',(1.,0.,0.));
#16809=DIRECTION('',(1.,0.,0.));
#16810=DIRECTION('',(0.,-1.,0.));
#16811=DIRECTION('center_axis',(1.,0.,0.));
#16812=DIRECTION('ref_axis',(0.,-1.,0.));
#16813=DIRECTION('center_axis',(1.,0.,0.));
#16814=DIRECTION('ref_axis',(0.,-1.,0.));
#16815=DIRECTION('',(0.,0.,-1.));
#16816=DIRECTION('center_axis',(0.,1.,0.));
#16817=DIRECTION('ref_axis',(1.,0.,0.));
#16818=DIRECTION('center_axis',(-1.,0.,0.));
#16819=DIRECTION('ref_axis',(0.,1.,0.));
#16820=DIRECTION('center_axis',(0.,1.,0.));
#16821=DIRECTION('ref_axis',(1.,0.,0.));
#16822=DIRECTION('',(0.,0.,-1.));
#16823=DIRECTION('center_axis',(-1.,0.,0.));
#16824=DIRECTION('ref_axis',(0.,1.,0.));
#16825=DIRECTION('center_axis',(0.,0.,1.));
#16826=DIRECTION('ref_axis',(-1.,0.,0.));
#16827=DIRECTION('center_axis',(0.,0.,1.));
#16828=DIRECTION('ref_axis',(-1.,0.,0.));
#16829=DIRECTION('',(0.,0.,1.));
#16830=DIRECTION('center_axis',(0.,0.,1.));
#16831=DIRECTION('ref_axis',(-1.,0.,0.));
#16832=DIRECTION('center_axis',(0.,0.,1.));
#16833=DIRECTION('ref_axis',(-1.,0.,0.));
#16834=DIRECTION('center_axis',(0.,0.,1.));
#16835=DIRECTION('ref_axis',(1.,0.,0.));
#16836=DIRECTION('axis',(0.,0.,1.));
#16837=DIRECTION('refdir',(1.,0.,0.));
#16838=DIRECTION('center_axis',(0.,0.,-1.));
#16839=DIRECTION('ref_axis',(1.,0.,0.));
#16840=DIRECTION('',(0.,0.,-1.));
#16841=DIRECTION('center_axis',(0.,0.,1.));
#16842=DIRECTION('ref_axis',(1.,0.,0.));
#16843=DIRECTION('',(0.,0.,-1.));
#16844=DIRECTION('center_axis',(0.,0.,-1.));
#16845=DIRECTION('ref_axis',(1.,0.,0.));
#16846=DIRECTION('center_axis',(0.,0.,1.));
#16847=DIRECTION('ref_axis',(1.,0.,0.));
#16848=DIRECTION('center_axis',(0.,0.,-1.));
#16849=DIRECTION('ref_axis',(1.,0.,0.));
#16850=DIRECTION('',(0.,0.,-1.));
#16851=DIRECTION('center_axis',(0.,0.,-1.));
#16852=DIRECTION('ref_axis',(1.,0.,0.));
#16853=DIRECTION('',(0.,0.,-1.));
#16854=DIRECTION('center_axis',(0.,0.,-1.));
#16855=DIRECTION('ref_axis',(1.,0.,0.));
#16856=DIRECTION('',(0.,0.,-1.));
#16857=DIRECTION('center_axis',(0.,0.,-1.));
#16858=DIRECTION('ref_axis',(1.,0.,0.));
#16859=DIRECTION('',(0.,0.,-1.));
#16860=DIRECTION('center_axis',(0.,0.,-1.));
#16861=DIRECTION('ref_axis',(1.,0.,0.));
#16862=DIRECTION('',(0.,0.,-1.));
#16863=DIRECTION('center_axis',(0.,0.,-1.));
#16864=DIRECTION('ref_axis',(0.937752260636195,-0.347304905913675,0.));
#16865=DIRECTION('',(0.,0.,-1.));
#16866=DIRECTION('center_axis',(0.,0.,-1.));
#16867=DIRECTION('ref_axis',(1.,0.,0.));
#16868=DIRECTION('center_axis',(0.,0.,-1.));
#16869=DIRECTION('ref_axis',(0.999651918108172,0.0263826197079016,0.));
#16870=DIRECTION('',(1.22464679914735E-16,-1.61260571350473E-30,-1.));
#16871=DIRECTION('center_axis',(0.,0.,1.));
#16872=DIRECTION('ref_axis',(1.,-1.30454602648733E-14,0.));
#16873=DIRECTION('center_axis',(0.,0.,-1.));
#16874=DIRECTION('ref_axis',(1.,-1.30454602648733E-14,0.));
#16875=DIRECTION('',(1.22464679914735E-16,-1.61260571350473E-30,-1.));
#16876=DIRECTION('center_axis',(0.,0.,-1.));
#16877=DIRECTION('ref_axis',(1.,-1.30454602648733E-14,0.));
#16878=DIRECTION('',(1.22464679914735E-16,-1.61260571350473E-30,-1.));
#16879=DIRECTION('center_axis',(0.,0.,-1.));
#16880=DIRECTION('ref_axis',(1.,-1.30454602648733E-14,0.));
#16881=DIRECTION('',(1.22464679914735E-16,-1.61260571350473E-30,-1.));
#16882=DIRECTION('center_axis',(0.,0.,-1.));
#16883=DIRECTION('ref_axis',(1.,-1.30454602648733E-14,0.));
#16884=DIRECTION('',(1.22464679914735E-16,-1.61260571350473E-30,-1.));
#16885=DIRECTION('center_axis',(0.,0.,-1.));
#16886=DIRECTION('ref_axis',(1.,-1.30454602648733E-14,0.));
#16887=DIRECTION('',(1.22464679914735E-16,-1.61260571350473E-30,-1.));
#16888=DIRECTION('center_axis',(0.,0.,-1.));
#16889=DIRECTION('ref_axis',(-0.608776360854994,-0.793341882459353,0.));
#16890=DIRECTION('',(1.22464679914735E-16,-1.61260571350473E-30,-1.));
#16891=DIRECTION('center_axis',(0.,0.,-1.));
#16892=DIRECTION('ref_axis',(1.,-1.30454602648733E-14,0.));
#16893=DIRECTION('center_axis',(0.,0.,-1.));
#16894=DIRECTION('ref_axis',(1.,0.,0.));
#16895=DIRECTION('',(0.,0.,-1.));
#16896=DIRECTION('center_axis',(0.,0.,1.));
#16897=DIRECTION('ref_axis',(1.,0.,0.));
#16898=DIRECTION('',(0.,0.,-1.));
#16899=DIRECTION('center_axis',(0.,0.,-1.));
#16900=DIRECTION('ref_axis',(1.,0.,0.));
#16901=DIRECTION('center_axis',(0.,0.,1.));
#16902=DIRECTION('ref_axis',(1.,0.,0.));
#16903=DIRECTION('center_axis',(0.,0.,-1.));
#16904=DIRECTION('ref_axis',(1.,0.,0.));
#16905=DIRECTION('',(0.,0.,-1.));
#16906=DIRECTION('center_axis',(0.,0.,-1.));
#16907=DIRECTION('ref_axis',(1.,0.,0.));
#16908=DIRECTION('',(0.,0.,-1.));
#16909=DIRECTION('center_axis',(0.,0.,-1.));
#16910=DIRECTION('ref_axis',(1.,0.,0.));
#16911=DIRECTION('',(0.,0.,-1.));
#16912=DIRECTION('center_axis',(0.,0.,-1.));
#16913=DIRECTION('ref_axis',(1.,0.,0.));
#16914=DIRECTION('',(0.,0.,-1.));
#16915=DIRECTION('center_axis',(0.,0.,-1.));
#16916=DIRECTION('ref_axis',(1.,0.,0.));
#16917=DIRECTION('',(0.,0.,-1.));
#16918=DIRECTION('center_axis',(0.,0.,-1.));
#16919=DIRECTION('ref_axis',(0.93775225635851,-0.347304917463781,0.));
#16920=DIRECTION('',(0.,0.,-1.));
#16921=DIRECTION('center_axis',(0.,0.,-1.));
#16922=DIRECTION('ref_axis',(1.,0.,0.));
#16923=DIRECTION('center_axis',(0.,0.,-1.));
#16924=DIRECTION('ref_axis',(0.99965191776215,0.0263826328188801,0.));
#16925=DIRECTION('',(1.22464679914735E-16,-2.1451417520641E-30,-1.));
#16926=DIRECTION('center_axis',(0.,0.,1.));
#16927=DIRECTION('ref_axis',(1.,-1.73939470198311E-14,0.));
#16928=DIRECTION('center_axis',(0.,0.,-1.));
#16929=DIRECTION('ref_axis',(1.,-1.73939470198311E-14,0.));
#16930=DIRECTION('',(1.22464679914735E-16,-2.1451417520641E-30,-1.));
#16931=DIRECTION('center_axis',(0.,0.,-1.));
#16932=DIRECTION('ref_axis',(1.,-1.73939470198311E-14,0.));
#16933=DIRECTION('',(1.22464679914735E-16,-2.1451417520641E-30,-1.));
#16934=DIRECTION('center_axis',(0.,0.,-1.));
#16935=DIRECTION('ref_axis',(1.,-1.73939470198311E-14,0.));
#16936=DIRECTION('',(1.22464679914735E-16,-2.1451417520641E-30,-1.));
#16937=DIRECTION('center_axis',(0.,0.,-1.));
#16938=DIRECTION('ref_axis',(1.,-1.73939470198311E-14,0.));
#16939=DIRECTION('',(1.22464679914735E-16,-2.1451417520641E-30,-1.));
#16940=DIRECTION('center_axis',(0.,0.,-1.));
#16941=DIRECTION('ref_axis',(1.,-1.73939470198311E-14,0.));
#16942=DIRECTION('',(1.22464679914735E-16,-2.1451417520641E-30,-1.));
#16943=DIRECTION('center_axis',(0.,0.,-1.));
#16944=DIRECTION('ref_axis',(-0.608776367541345,-0.793341877328536,0.));
#16945=DIRECTION('',(1.22464679914735E-16,-2.1451417520641E-30,-1.));
#16946=DIRECTION('center_axis',(0.,0.,-1.));
#16947=DIRECTION('ref_axis',(1.,-1.73939470198311E-14,0.));
#16948=DIRECTION('center_axis',(0.,0.,-1.));
#16949=DIRECTION('ref_axis',(1.,0.,0.));
#16950=DIRECTION('',(0.,0.,-1.));
#16951=DIRECTION('center_axis',(0.,0.,1.));
#16952=DIRECTION('ref_axis',(1.,0.,0.));
#16953=DIRECTION('',(0.,0.,-1.));
#16954=DIRECTION('center_axis',(0.,0.,-1.));
#16955=DIRECTION('ref_axis',(1.,0.,0.));
#16956=DIRECTION('center_axis',(0.,0.,1.));
#16957=DIRECTION('ref_axis',(1.,0.,0.));
#16958=DIRECTION('center_axis',(0.,0.,-1.));
#16959=DIRECTION('ref_axis',(1.,0.,0.));
#16960=DIRECTION('',(0.,0.,-1.));
#16961=DIRECTION('center_axis',(0.,0.,-1.));
#16962=DIRECTION('ref_axis',(1.,0.,0.));
#16963=DIRECTION('',(0.,0.,-1.));
#16964=DIRECTION('center_axis',(0.,0.,-1.));
#16965=DIRECTION('ref_axis',(1.,0.,0.));
#16966=DIRECTION('',(0.,0.,-1.));
#16967=DIRECTION('center_axis',(0.,0.,-1.));
#16968=DIRECTION('ref_axis',(1.,0.,0.));
#16969=DIRECTION('',(0.,0.,-1.));
#16970=DIRECTION('center_axis',(0.,0.,-1.));
#16971=DIRECTION('ref_axis',(1.,0.,0.));
#16972=DIRECTION('',(0.,0.,-1.));
#16973=DIRECTION('center_axis',(0.,0.,-1.));
#16974=DIRECTION('ref_axis',(0.937752268704685,-0.347304884128077,0.));
#16975=DIRECTION('',(0.,0.,-1.));
#16976=DIRECTION('center_axis',(0.,0.,-1.));
#16977=DIRECTION('ref_axis',(1.,0.,0.));
#16978=DIRECTION('center_axis',(0.,0.,-1.));
#16979=DIRECTION('ref_axis',(0.999651918695003,0.0263825974725584,0.));
#16980=DIRECTION('',(1.22464679914735E-16,-1.61260571350473E-30,-1.));
#16981=DIRECTION('center_axis',(0.,0.,1.));
#16982=DIRECTION('ref_axis',(1.,-1.30454602648733E-14,0.));
#16983=DIRECTION('center_axis',(0.,0.,-1.));
#16984=DIRECTION('ref_axis',(1.,-1.30454602648733E-14,0.));
#16985=DIRECTION('',(1.22464679914735E-16,-1.61260571350473E-30,-1.));
#16986=DIRECTION('center_axis',(0.,0.,-1.));
#16987=DIRECTION('ref_axis',(1.,-1.30454602648733E-14,0.));
#16988=DIRECTION('',(1.22464679914735E-16,-1.61260571350473E-30,-1.));
#16989=DIRECTION('center_axis',(0.,0.,-1.));
#16990=DIRECTION('ref_axis',(1.,-1.30454602648733E-14,0.));
#16991=DIRECTION('',(1.22464679914735E-16,-1.61260571350473E-30,-1.));
#16992=DIRECTION('center_axis',(0.,0.,-1.));
#16993=DIRECTION('ref_axis',(1.,-1.30454602648733E-14,0.));
#16994=DIRECTION('',(1.22464679914735E-16,-1.61260571350473E-30,-1.));
#16995=DIRECTION('center_axis',(0.,0.,-1.));
#16996=DIRECTION('ref_axis',(1.,-1.30454602648733E-14,0.));
#16997=DIRECTION('',(1.22464679914735E-16,-1.61260571350473E-30,-1.));
#16998=DIRECTION('center_axis',(0.,0.,-1.));
#16999=DIRECTION('ref_axis',(-0.608776376626888,-0.793341870356681,0.));
#17000=DIRECTION('',(1.22464679914735E-16,-1.61260571350473E-30,-1.));
#17001=DIRECTION('center_axis',(0.,0.,-1.));
#17002=DIRECTION('ref_axis',(1.,-1.30454602648733E-14,0.));
#17003=DIRECTION('center_axis',(0.,0.,-1.));
#17004=DIRECTION('ref_axis',(1.,0.,0.));
#17005=DIRECTION('',(0.,0.,-1.));
#17006=DIRECTION('center_axis',(0.,0.,1.));
#17007=DIRECTION('ref_axis',(1.,0.,0.));
#17008=DIRECTION('',(0.,0.,-1.));
#17009=DIRECTION('center_axis',(0.,0.,-1.));
#17010=DIRECTION('ref_axis',(1.,0.,0.));
#17011=DIRECTION('center_axis',(0.,0.,1.));
#17012=DIRECTION('ref_axis',(1.,0.,0.));
#17013=DIRECTION('center_axis',(0.,0.,-1.));
#17014=DIRECTION('ref_axis',(1.,0.,0.));
#17015=DIRECTION('',(0.,0.,-1.));
#17016=DIRECTION('center_axis',(0.,0.,-1.));
#17017=DIRECTION('ref_axis',(1.,0.,0.));
#17018=DIRECTION('',(0.,0.,-1.));
#17019=DIRECTION('center_axis',(0.,0.,-1.));
#17020=DIRECTION('ref_axis',(1.,0.,0.));
#17021=DIRECTION('',(0.,0.,-1.));
#17022=DIRECTION('center_axis',(0.,0.,-1.));
#17023=DIRECTION('ref_axis',(1.,0.,0.));
#17024=DIRECTION('',(0.,0.,-1.));
#17025=DIRECTION('center_axis',(0.,0.,-1.));
#17026=DIRECTION('ref_axis',(1.,0.,0.));
#17027=DIRECTION('',(0.,0.,-1.));
#17028=DIRECTION('center_axis',(0.,0.,-1.));
#17029=DIRECTION('ref_axis',(0.937752266106258,-0.347304891144047,0.));
#17030=DIRECTION('',(0.,0.,-1.));
#17031=DIRECTION('center_axis',(0.,0.,-1.));
#17032=DIRECTION('ref_axis',(1.,0.,0.));
#17033=DIRECTION('center_axis',(0.,0.,-1.));
#17034=DIRECTION('ref_axis',(0.999651918505729,0.026382604644274,0.));
#17035=DIRECTION('',(1.22464679914735E-16,-2.1451417520641E-30,-1.));
#17036=DIRECTION('center_axis',(0.,0.,1.));
#17037=DIRECTION('ref_axis',(1.,-1.73939470198311E-14,0.));
#17038=DIRECTION('center_axis',(0.,0.,-1.));
#17039=DIRECTION('ref_axis',(1.,-1.73939470198311E-14,0.));
#17040=DIRECTION('',(1.22464679914735E-16,-2.1451417520641E-30,-1.));
#17041=DIRECTION('center_axis',(0.,0.,-1.));
#17042=DIRECTION('ref_axis',(1.,-1.73939470198311E-14,0.));
#17043=DIRECTION('',(1.22464679914735E-16,-2.1451417520641E-30,-1.));
#17044=DIRECTION('center_axis',(0.,0.,-1.));
#17045=DIRECTION('ref_axis',(1.,-1.73939470198311E-14,0.));
#17046=DIRECTION('',(1.22464679914735E-16,-2.1451417520641E-30,-1.));
#17047=DIRECTION('center_axis',(0.,0.,-1.));
#17048=DIRECTION('ref_axis',(1.,-1.73939470198311E-14,0.));
#17049=DIRECTION('',(1.22464679914735E-16,-2.1451417520641E-30,-1.));
#17050=DIRECTION('center_axis',(0.,0.,-1.));
#17051=DIRECTION('ref_axis',(1.,-1.73939470198311E-14,0.));
#17052=DIRECTION('',(1.22464679914735E-16,-2.1451417520641E-30,-1.));
#17053=DIRECTION('center_axis',(0.,0.,-1.));
#17054=DIRECTION('ref_axis',(-0.60877637156726,-0.793341874239222,0.));
#17055=DIRECTION('',(1.22464679914735E-16,-2.1451417520641E-30,-1.));
#17056=DIRECTION('center_axis',(0.,0.,-1.));
#17057=DIRECTION('ref_axis',(1.,-1.73939470198311E-14,0.));
#17058=DIRECTION('center_axis',(0.,0.,1.));
#17059=DIRECTION('ref_axis',(-1.,0.,0.));
#17060=DIRECTION('',(0.,0.,1.));
#17061=DIRECTION('center_axis',(0.,0.,-1.));
#17062=DIRECTION('ref_axis',(-1.,0.,0.));
#17063=DIRECTION('',(0.,0.,1.));
#17064=DIRECTION('center_axis',(0.,0.,-1.));
#17065=DIRECTION('ref_axis',(-1.,0.,0.));
#17066=DIRECTION('center_axis',(0.,0.,1.));
#17067=DIRECTION('ref_axis',(-1.,0.,0.));
#17068=DIRECTION('',(0.,0.,1.));
#17069=DIRECTION('center_axis',(0.,0.,1.));
#17070=DIRECTION('ref_axis',(-1.,0.,0.));
#17071=DIRECTION('',(0.,0.,1.));
#17072=DIRECTION('center_axis',(0.,0.,1.));
#17073=DIRECTION('ref_axis',(-0.937049331551953,-0.349197007773604,0.));
#17074=DIRECTION('',(0.,0.,1.));
#17075=DIRECTION('center_axis',(0.,0.,-1.));
#17076=DIRECTION('ref_axis',(-1.,0.,0.));
#17077=DIRECTION('center_axis',(0.,0.,1.));
#17078=DIRECTION('ref_axis',(0.130209904811036,0.991486450078417,0.));
#17079=DIRECTION('',(-1.22464679914735E-16,1.05158884927822E-30,1.));
#17080=DIRECTION('center_axis',(0.,0.,-1.));
#17081=DIRECTION('ref_axis',(-1.,8.70933927927167E-15,0.));
#17082=DIRECTION('center_axis',(0.,0.,1.));
#17083=DIRECTION('ref_axis',(-1.,8.70933927927167E-15,0.));
#17084=DIRECTION('',(-1.22464679914735E-16,1.05158884927822E-30,1.));
#17085=DIRECTION('center_axis',(0.,0.,1.));
#17086=DIRECTION('ref_axis',(-1.,8.70933927927167E-15,0.));
#17087=DIRECTION('',(-1.22464679914735E-16,1.05158884927822E-30,1.));
#17088=DIRECTION('center_axis',(0.,0.,1.));
#17089=DIRECTION('ref_axis',(-1.,8.70933927927167E-15,0.));
#17090=DIRECTION('',(-1.22464679914735E-16,1.05158884927822E-30,1.));
#17091=DIRECTION('center_axis',(0.,0.,1.));
#17092=DIRECTION('ref_axis',(0.608508670823076,-0.793547224513534,0.));
#17093=DIRECTION('',(-1.22464679914735E-16,1.05158884927822E-30,1.));
#17094=DIRECTION('center_axis',(0.,0.,1.));
#17095=DIRECTION('ref_axis',(-1.,8.70933927927167E-15,0.));
#17096=DIRECTION('center_axis',(0.,0.,1.));
#17097=DIRECTION('ref_axis',(-1.,0.,0.));
#17098=DIRECTION('',(0.,0.,1.));
#17099=DIRECTION('center_axis',(0.,0.,-1.));
#17100=DIRECTION('ref_axis',(-1.,0.,0.));
#17101=DIRECTION('',(0.,0.,1.));
#17102=DIRECTION('center_axis',(0.,0.,-1.));
#17103=DIRECTION('ref_axis',(-1.,0.,0.));
#17104=DIRECTION('center_axis',(0.,0.,1.));
#17105=DIRECTION('ref_axis',(-1.,0.,0.));
#17106=DIRECTION('',(0.,0.,1.));
#17107=DIRECTION('center_axis',(0.,0.,1.));
#17108=DIRECTION('ref_axis',(-1.,0.,0.));
#17109=DIRECTION('',(0.,0.,1.));
#17110=DIRECTION('center_axis',(0.,0.,1.));
#17111=DIRECTION('ref_axis',(-0.937049332084929,-0.349197006343393,0.));
#17112=DIRECTION('',(0.,0.,1.));
#17113=DIRECTION('center_axis',(0.,0.,-1.));
#17114=DIRECTION('ref_axis',(-1.,0.,0.));
#17115=DIRECTION('center_axis',(0.,0.,1.));
#17116=DIRECTION('ref_axis',(0.130209903589588,0.991486450238827,0.));
#17117=DIRECTION('',(-1.22464679914735E-16,8.38271559857251E-31,1.));
#17118=DIRECTION('center_axis',(0.,0.,-1.));
#17119=DIRECTION('ref_axis',(-1.,6.96747142341734E-15,0.));
#17120=DIRECTION('center_axis',(0.,0.,1.));
#17121=DIRECTION('ref_axis',(-1.,6.96747142341734E-15,0.));
#17122=DIRECTION('',(-1.22464679914735E-16,8.38271559857251E-31,1.));
#17123=DIRECTION('center_axis',(0.,0.,1.));
#17124=DIRECTION('ref_axis',(-1.,6.96747142341734E-15,0.));
#17125=DIRECTION('',(-1.22464679914735E-16,8.38271559857251E-31,1.));
#17126=DIRECTION('center_axis',(0.,0.,1.));
#17127=DIRECTION('ref_axis',(-1.,6.96747142341734E-15,0.));
#17128=DIRECTION('',(-1.22464679914735E-16,8.38271559857251E-31,1.));
#17129=DIRECTION('center_axis',(0.,0.,1.));
#17130=DIRECTION('ref_axis',(0.608508660191718,-0.793547232665882,0.));
#17131=DIRECTION('',(-1.22464679914735E-16,8.38271559857251E-31,1.));
#17132=DIRECTION('center_axis',(0.,0.,1.));
#17133=DIRECTION('ref_axis',(-1.,6.96747142341734E-15,0.));
#17134=DIRECTION('center_axis',(0.,0.,1.));
#17135=DIRECTION('ref_axis',(-1.,0.,0.));
#17136=DIRECTION('',(0.,0.,1.));
#17137=DIRECTION('center_axis',(0.,0.,-1.));
#17138=DIRECTION('ref_axis',(-1.,0.,0.));
#17139=DIRECTION('',(0.,0.,1.));
#17140=DIRECTION('center_axis',(0.,0.,-1.));
#17141=DIRECTION('ref_axis',(-1.,0.,0.));
#17142=DIRECTION('center_axis',(0.,0.,1.));
#17143=DIRECTION('ref_axis',(-1.,0.,0.));
#17144=DIRECTION('',(0.,0.,1.));
#17145=DIRECTION('center_axis',(0.,0.,1.));
#17146=DIRECTION('ref_axis',(-1.,0.,0.));
#17147=DIRECTION('',(0.,0.,1.));
#17148=DIRECTION('center_axis',(0.,0.,1.));
#17149=DIRECTION('ref_axis',(-0.937049331749067,-0.34919700724466,0.));
#17150=DIRECTION('',(0.,0.,1.));
#17151=DIRECTION('center_axis',(0.,0.,-1.));
#17152=DIRECTION('ref_axis',(-1.,0.,0.));
#17153=DIRECTION('center_axis',(0.,0.,1.));
#17154=DIRECTION('ref_axis',(0.130209904005025,0.991486450184269,0.));
#17155=DIRECTION('',(-1.22464679914735E-16,1.47822342812015E-30,1.));
#17156=DIRECTION('center_axis',(0.,0.,-1.));
#17157=DIRECTION('ref_axis',(-1.,1.21930749909803E-14,0.));
#17158=DIRECTION('center_axis',(0.,0.,1.));
#17159=DIRECTION('ref_axis',(-1.,1.21930749909803E-14,0.));
#17160=DIRECTION('',(-1.22464679914735E-16,1.47822342812015E-30,1.));
#17161=DIRECTION('center_axis',(0.,0.,1.));
#17162=DIRECTION('ref_axis',(-1.,1.21930749909803E-14,0.));
#17163=DIRECTION('',(-1.22464679914735E-16,1.47822342812015E-30,1.));
#17164=DIRECTION('center_axis',(0.,0.,1.));
#17165=DIRECTION('ref_axis',(-1.,1.21930749909803E-14,0.));
#17166=DIRECTION('',(-1.22464679914735E-16,1.47822342812015E-30,1.));
#17167=DIRECTION('center_axis',(0.,0.,1.));
#17168=DIRECTION('ref_axis',(0.608508666431814,-0.793547227880846,0.));
#17169=DIRECTION('',(-1.22464679914735E-16,1.47822342812015E-30,1.));
#17170=DIRECTION('center_axis',(0.,0.,1.));
#17171=DIRECTION('ref_axis',(-1.,1.21930749909803E-14,0.));
#17172=DIRECTION('center_axis',(0.,0.,1.));
#17173=DIRECTION('ref_axis',(-1.,0.,0.));
#17174=DIRECTION('',(0.,0.,1.));
#17175=DIRECTION('center_axis',(0.,0.,-1.));
#17176=DIRECTION('ref_axis',(-1.,0.,0.));
#17177=DIRECTION('',(0.,0.,1.));
#17178=DIRECTION('center_axis',(0.,0.,-1.));
#17179=DIRECTION('ref_axis',(-1.,0.,0.));
#17180=DIRECTION('center_axis',(0.,0.,1.));
#17181=DIRECTION('ref_axis',(-1.,0.,0.));
#17182=DIRECTION('',(0.,0.,1.));
#17183=DIRECTION('center_axis',(0.,0.,1.));
#17184=DIRECTION('ref_axis',(-1.,0.,0.));
#17185=DIRECTION('',(0.,0.,1.));
#17186=DIRECTION('center_axis',(0.,0.,1.));
#17187=DIRECTION('ref_axis',(-0.937049331905873,-0.349197006823879,0.));
#17188=DIRECTION('',(0.,0.,1.));
#17189=DIRECTION('center_axis',(0.,0.,-1.));
#17190=DIRECTION('ref_axis',(-1.,0.,0.));
#17191=DIRECTION('center_axis',(0.,0.,1.));
#17192=DIRECTION('ref_axis',(0.130209904338333,0.991486450140496,0.));
#17193=DIRECTION('',(-1.22464679914735E-16,1.26490613869919E-30,1.));
#17194=DIRECTION('center_axis',(0.,0.,-1.));
#17195=DIRECTION('ref_axis',(-1.,1.0451207135126E-14,0.));
#17196=DIRECTION('center_axis',(0.,0.,1.));
#17197=DIRECTION('ref_axis',(-1.,1.0451207135126E-14,0.));
#17198=DIRECTION('',(-1.22464679914735E-16,1.26490613869919E-30,1.));
#17199=DIRECTION('center_axis',(0.,0.,1.));
#17200=DIRECTION('ref_axis',(-1.,1.0451207135126E-14,0.));
#17201=DIRECTION('',(-1.22464679914735E-16,1.26490613869919E-30,1.));
#17202=DIRECTION('center_axis',(0.,0.,1.));
#17203=DIRECTION('ref_axis',(-1.,1.0451207135126E-14,0.));
#17204=DIRECTION('',(-1.22464679914735E-16,1.26490613869919E-30,1.));
#17205=DIRECTION('center_axis',(0.,0.,1.));
#17206=DIRECTION('ref_axis',(0.608508664268565,-0.79354722953967,0.));
#17207=DIRECTION('',(-1.22464679914735E-16,1.26490613869919E-30,1.));
#17208=DIRECTION('center_axis',(0.,0.,1.));
#17209=DIRECTION('ref_axis',(-1.,1.0451207135126E-14,0.));
#17210=DIRECTION('center_axis',(0.,0.,1.));
#17211=DIRECTION('ref_axis',(1.,0.,0.));
#17212=DIRECTION('center_axis',(0.,0.,1.));
#17213=DIRECTION('ref_axis',(-1.,1.0451207135126E-14,0.));
#17214=DIRECTION('center_axis',(0.,0.,1.));
#17215=DIRECTION('ref_axis',(-1.,0.,0.));
#17216=DIRECTION('center_axis',(0.,0.,1.));
#17217=DIRECTION('ref_axis',(1.,0.,0.));
#17218=DIRECTION('center_axis',(0.,0.,1.));
#17219=DIRECTION('ref_axis',(-1.,1.21930749909803E-14,0.));
#17220=DIRECTION('center_axis',(0.,0.,1.));
#17221=DIRECTION('ref_axis',(-1.,0.,0.));
#17222=DIRECTION('center_axis',(0.,0.,1.));
#17223=DIRECTION('ref_axis',(1.,0.,0.));
#17224=DIRECTION('center_axis',(0.,0.,1.));
#17225=DIRECTION('ref_axis',(-1.,6.96747142341734E-15,0.));
#17226=DIRECTION('center_axis',(0.,0.,1.));
#17227=DIRECTION('ref_axis',(-1.,0.,0.));
#17228=DIRECTION('center_axis',(0.,0.,1.));
#17229=DIRECTION('ref_axis',(1.,0.,0.));
#17230=DIRECTION('center_axis',(0.,0.,1.));
#17231=DIRECTION('ref_axis',(-1.,8.70933927927167E-15,0.));
#17232=DIRECTION('center_axis',(0.,0.,1.));
#17233=DIRECTION('ref_axis',(-1.,0.,0.));
#17234=DIRECTION('center_axis',(0.,0.,1.));
#17235=DIRECTION('ref_axis',(-1.,0.,0.));
#17236=DIRECTION('center_axis',(0.,0.,1.));
#17237=DIRECTION('ref_axis',(-1.,0.,0.));
#17238=DIRECTION('center_axis',(0.,0.,1.));
#17239=DIRECTION('ref_axis',(-1.,0.,0.));
#17240=DIRECTION('center_axis',(0.,0.,1.));
#17241=DIRECTION('ref_axis',(-1.,0.,0.));
#17242=DIRECTION('center_axis',(0.,0.,1.));
#17243=DIRECTION('ref_axis',(1.,0.,0.));
#17244=DIRECTION('center_axis',(0.,0.,-1.));
#17245=DIRECTION('ref_axis',(1.,-1.73939470198311E-14,0.));
#17246=DIRECTION('center_axis',(0.,0.,-1.));
#17247=DIRECTION('ref_axis',(1.,0.,0.));
#17248=DIRECTION('center_axis',(0.,0.,1.));
#17249=DIRECTION('ref_axis',(1.,0.,0.));
#17250=DIRECTION('center_axis',(0.,0.,-1.));
#17251=DIRECTION('ref_axis',(1.,-1.30454602648733E-14,0.));
#17252=DIRECTION('center_axis',(0.,0.,-1.));
#17253=DIRECTION('ref_axis',(1.,0.,0.));
#17254=DIRECTION('center_axis',(0.,0.,1.));
#17255=DIRECTION('ref_axis',(1.,0.,0.));
#17256=DIRECTION('center_axis',(0.,0.,-1.));
#17257=DIRECTION('ref_axis',(1.,-1.73939470198311E-14,0.));
#17258=DIRECTION('center_axis',(0.,0.,-1.));
#17259=DIRECTION('ref_axis',(1.,0.,0.));
#17260=DIRECTION('center_axis',(0.,0.,1.));
#17261=DIRECTION('ref_axis',(1.,0.,0.));
#17262=DIRECTION('center_axis',(0.,0.,-1.));
#17263=DIRECTION('ref_axis',(1.,-1.30454602648733E-14,0.));
#17264=DIRECTION('center_axis',(0.,0.,-1.));
#17265=DIRECTION('ref_axis',(1.,0.,0.));
#17266=DIRECTION('center_axis',(0.,0.,1.));
#17267=DIRECTION('ref_axis',(1.,0.,0.));
#17268=DIRECTION('center_axis',(0.,0.,1.));
#17269=DIRECTION('ref_axis',(1.,0.,0.));
#17270=DIRECTION('',(0.,0.,-1.));
#17271=DIRECTION('center_axis',(0.,0.,-1.));
#17272=DIRECTION('ref_axis',(1.,0.,0.));
#17273=DIRECTION('center_axis',(0.,0.,1.));
#17274=DIRECTION('ref_axis',(1.,0.,0.));
#17275=DIRECTION('center_axis',(0.,0.,-1.));
#17276=DIRECTION('ref_axis',(1.,0.,0.));
#17277=DIRECTION('center_axis',(0.,0.,1.));
#17278=DIRECTION('ref_axis',(1.,0.,0.));
#17279=DIRECTION('',(0.,0.,-1.));
#17280=DIRECTION('center_axis',(0.,0.,-1.));
#17281=DIRECTION('ref_axis',(1.,0.,0.));
#17282=DIRECTION('center_axis',(0.,0.,1.));
#17283=DIRECTION('ref_axis',(1.,0.,0.));
#17284=DIRECTION('center_axis',(0.,0.,-1.));
#17285=DIRECTION('ref_axis',(1.,0.,0.));
#17286=DIRECTION('',(0.,0.,-1.));
#17287=DIRECTION('center_axis',(0.,0.,-1.));
#17288=DIRECTION('ref_axis',(1.,0.,0.));
#17289=DIRECTION('center_axis',(0.,0.,1.));
#17290=DIRECTION('ref_axis',(1.,0.,0.));
#17291=DIRECTION('center_axis',(0.,0.,1.));
#17292=DIRECTION('ref_axis',(1.,0.,0.));
#17293=DIRECTION('axis',(0.,0.,1.));
#17294=DIRECTION('refdir',(1.,0.,0.));
#17295=DIRECTION('center_axis',(-1.,0.,0.));
#17296=DIRECTION('ref_axis',(0.,0.991178642906414,0.13253262936424));
#17297=DIRECTION('',(-1.,0.,0.));
#17298=DIRECTION('center_axis',(1.,0.,0.));
#17299=DIRECTION('ref_axis',(0.,1.,0.));
#17300=DIRECTION('center_axis',(-1.,0.,0.));
#17301=DIRECTION('ref_axis',(0.,1.,0.));
#17302=DIRECTION('',(-1.,0.,0.));
#17303=DIRECTION('center_axis',(-1.,0.,0.));
#17304=DIRECTION('ref_axis',(0.,1.,0.));
#17305=DIRECTION('',(-1.,0.,0.));
#17306=DIRECTION('center_axis',(-1.,0.,0.));
#17307=DIRECTION('ref_axis',(0.,1.,0.));
#17308=DIRECTION('',(-1.,0.,0.));
#17309=DIRECTION('center_axis',(-1.,0.,0.));
#17310=DIRECTION('ref_axis',(0.,1.,0.));
#17311=DIRECTION('',(-1.,0.,0.));
#17312=DIRECTION('center_axis',(-1.,0.,0.));
#17313=DIRECTION('ref_axis',(0.,1.,0.));
#17314=DIRECTION('',(-1.,0.,0.));
#17315=DIRECTION('center_axis',(-1.,0.,0.));
#17316=DIRECTION('ref_axis',(0.,1.,0.));
#17317=DIRECTION('',(-1.,0.,0.));
#17318=DIRECTION('center_axis',(-1.,0.,0.));
#17319=DIRECTION('ref_axis',(0.,1.,0.));
#17320=DIRECTION('',(-1.,0.,0.));
#17321=DIRECTION('center_axis',(-1.,0.,0.));
#17322=DIRECTION('ref_axis',(0.,1.,0.));
#17323=DIRECTION('',(-1.,0.,0.));
#17324=DIRECTION('center_axis',(-1.,0.,0.));
#17325=DIRECTION('ref_axis',(0.,1.,0.));
#17326=DIRECTION('',(-1.,0.,0.));
#17327=DIRECTION('center_axis',(-1.,0.,0.));
#17328=DIRECTION('ref_axis',(0.,1.,0.));
#17329=DIRECTION('',(-1.,0.,0.));
#17330=DIRECTION('center_axis',(-1.,0.,0.));
#17331=DIRECTION('ref_axis',(0.,1.,0.));
#17332=DIRECTION('',(-1.,0.,0.));
#17333=DIRECTION('center_axis',(-1.,0.,0.));
#17334=DIRECTION('ref_axis',(0.,1.,0.));
#17335=DIRECTION('',(-1.,0.,0.));
#17336=DIRECTION('center_axis',(-1.,0.,0.));
#17337=DIRECTION('ref_axis',(0.,1.,0.));
#17338=DIRECTION('',(-1.,0.,0.));
#17339=DIRECTION('center_axis',(-1.,0.,0.));
#17340=DIRECTION('ref_axis',(0.,1.,0.));
#17341=DIRECTION('',(-1.,0.,0.));
#17342=DIRECTION('center_axis',(-1.,0.,0.));
#17343=DIRECTION('ref_axis',(0.,1.,0.));
#17344=DIRECTION('',(-1.,0.,0.));
#17345=DIRECTION('center_axis',(-1.,0.,0.));
#17346=DIRECTION('ref_axis',(0.,1.,0.));
#17347=DIRECTION('',(-1.,0.,0.));
#17348=DIRECTION('center_axis',(-1.,0.,0.));
#17349=DIRECTION('ref_axis',(0.,1.,0.));
#17350=DIRECTION('',(-1.,0.,0.));
#17351=DIRECTION('center_axis',(-1.,0.,0.));
#17352=DIRECTION('ref_axis',(0.,1.,0.));
#17353=DIRECTION('',(-1.,0.,0.));
#17354=DIRECTION('center_axis',(-1.,0.,0.));
#17355=DIRECTION('ref_axis',(0.,1.,0.));
#17356=DIRECTION('',(-1.,0.,0.));
#17357=DIRECTION('center_axis',(-1.,0.,0.));
#17358=DIRECTION('ref_axis',(0.,1.,0.));
#17359=DIRECTION('',(-1.,0.,0.));
#17360=DIRECTION('center_axis',(-1.,0.,0.));
#17361=DIRECTION('ref_axis',(0.,1.,0.));
#17362=DIRECTION('',(-1.,0.,0.));
#17363=DIRECTION('center_axis',(-1.,0.,0.));
#17364=DIRECTION('ref_axis',(0.,1.,0.));
#17365=DIRECTION('',(-1.,0.,0.));
#17366=DIRECTION('center_axis',(-1.,0.,0.));
#17367=DIRECTION('ref_axis',(0.,1.,0.));
#17368=DIRECTION('',(-1.,0.,0.));
#17369=DIRECTION('center_axis',(-1.,0.,0.));
#17370=DIRECTION('ref_axis',(0.,1.,0.));
#17371=DIRECTION('',(-1.,0.,0.));
#17372=DIRECTION('center_axis',(-1.,0.,0.));
#17373=DIRECTION('ref_axis',(0.,1.,0.));
#17374=DIRECTION('',(-1.,0.,0.));
#17375=DIRECTION('center_axis',(-1.,0.,0.));
#17376=DIRECTION('ref_axis',(0.,1.,0.));
#17377=DIRECTION('',(-1.,0.,0.));
#17378=DIRECTION('center_axis',(-1.,0.,0.));
#17379=DIRECTION('ref_axis',(0.,0.936835173124404,-0.349771151464737));
#17380=DIRECTION('',(-1.,0.,0.));
#17381=DIRECTION('center_axis',(-1.,0.,0.));
#17382=DIRECTION('ref_axis',(0.,1.,0.));
#17383=DIRECTION('center_axis',(-1.,0.,0.));
#17384=DIRECTION('ref_axis',(0.,-0.417222372432346,0.908804429974857));
#17385=DIRECTION('',(-1.,1.22464679914735E-16,1.19060305846873E-29));
#17386=DIRECTION('center_axis',(1.,0.,0.));
#17387=DIRECTION('ref_axis',(0.,1.,9.73425822924114E-14));
#17388=DIRECTION('center_axis',(-1.,0.,0.));
#17389=DIRECTION('ref_axis',(0.,1.,9.73425822924114E-14));
#17390=DIRECTION('',(-1.,1.22464679914735E-16,1.19060305846873E-29));
#17391=DIRECTION('center_axis',(-1.,0.,0.));
#17392=DIRECTION('ref_axis',(0.,1.,9.73425822924114E-14));
#17393=DIRECTION('',(-1.,1.22464679914735E-16,1.19060305846873E-29));
#17394=DIRECTION('center_axis',(-1.,0.,0.));
#17395=DIRECTION('ref_axis',(0.,1.,9.73425822924114E-14));
#17396=DIRECTION('',(-1.,1.22464679914735E-16,1.19060305846873E-29));
#17397=DIRECTION('center_axis',(-1.,0.,0.));
#17398=DIRECTION('ref_axis',(0.,1.,9.73425822924114E-14));
#17399=DIRECTION('',(-1.,1.22464679914735E-16,1.19060305846873E-29));
#17400=DIRECTION('center_axis',(-1.,0.,0.));
#17401=DIRECTION('ref_axis',(0.,1.,9.73425822924114E-14));
#17402=DIRECTION('',(-1.,1.22464679914735E-16,1.19060305846873E-29));
#17403=DIRECTION('center_axis',(-1.,0.,0.));
#17404=DIRECTION('ref_axis',(0.,1.,9.73425822924114E-14));
#17405=DIRECTION('',(-1.,1.22464679914735E-16,1.19060305846873E-29));
#17406=DIRECTION('center_axis',(-1.,0.,0.));
#17407=DIRECTION('ref_axis',(0.,1.,9.73425822924114E-14));
#17408=DIRECTION('',(-1.,1.22464679914735E-16,1.19060305846873E-29));
#17409=DIRECTION('center_axis',(-1.,0.,0.));
#17410=DIRECTION('ref_axis',(0.,1.,9.73425822924114E-14));
#17411=DIRECTION('',(-1.,1.22464679914735E-16,1.19060305846873E-29));
#17412=DIRECTION('center_axis',(-1.,0.,0.));
#17413=DIRECTION('ref_axis',(0.,1.,9.73425822924114E-14));
#17414=DIRECTION('',(-1.,1.22464679914735E-16,1.19060305846873E-29));
#17415=DIRECTION('center_axis',(-1.,0.,0.));
#17416=DIRECTION('ref_axis',(0.,1.,9.73425822924114E-14));
#17417=DIRECTION('',(-1.,1.22464679914735E-16,1.19060305846873E-29));
#17418=DIRECTION('center_axis',(-1.,0.,0.));
#17419=DIRECTION('ref_axis',(0.,1.,9.73425822924114E-14));
#17420=DIRECTION('',(-1.,1.22464679914735E-16,1.19060305846873E-29));
#17421=DIRECTION('center_axis',(-1.,0.,0.));
#17422=DIRECTION('ref_axis',(0.,1.,9.73425822924114E-14));
#17423=DIRECTION('',(-1.,1.22464679914735E-16,1.19060305846873E-29));
#17424=DIRECTION('center_axis',(-1.,0.,0.));
#17425=DIRECTION('ref_axis',(0.,1.,9.73425822924114E-14));
#17426=DIRECTION('',(-1.,1.22464679914735E-16,1.19060305846873E-29));
#17427=DIRECTION('center_axis',(-1.,0.,0.));
#17428=DIRECTION('ref_axis',(0.,1.,9.73425822924114E-14));
#17429=DIRECTION('',(-1.,1.22464679914735E-16,1.19060305846873E-29));
#17430=DIRECTION('center_axis',(-1.,0.,0.));
#17431=DIRECTION('ref_axis',(0.,1.,9.73425822924114E-14));
#17432=DIRECTION('',(-1.,1.22464679914735E-16,1.19060305846873E-29));
#17433=DIRECTION('center_axis',(-1.,0.,0.));
#17434=DIRECTION('ref_axis',(0.,1.,9.73425822924114E-14));
#17435=DIRECTION('',(-1.,1.22464679914735E-16,1.19060305846873E-29));
#17436=DIRECTION('center_axis',(-1.,0.,0.));
#17437=DIRECTION('ref_axis',(0.,1.,9.73425822924114E-14));
#17438=DIRECTION('',(-1.,1.22464679914735E-16,1.19060305846873E-29));
#17439=DIRECTION('center_axis',(-1.,0.,0.));
#17440=DIRECTION('ref_axis',(0.,1.,9.73425822924114E-14));
#17441=DIRECTION('',(-1.,1.22464679914735E-16,1.19060305846873E-29));
#17442=DIRECTION('center_axis',(-1.,0.,0.));
#17443=DIRECTION('ref_axis',(0.,1.,9.73425822924114E-14));
#17444=DIRECTION('',(-1.,1.22464679914735E-16,1.19060305846873E-29));
#17445=DIRECTION('center_axis',(-1.,0.,0.));
#17446=DIRECTION('ref_axis',(0.,1.,9.73425822924114E-14));
#17447=DIRECTION('',(-1.,1.22464679914735E-16,1.19060305846873E-29));
#17448=DIRECTION('center_axis',(-1.,0.,0.));
#17449=DIRECTION('ref_axis',(0.,1.,9.73425822924114E-14));
#17450=DIRECTION('',(-1.,1.22464679914735E-16,1.19060305846873E-29));
#17451=DIRECTION('center_axis',(-1.,0.,0.));
#17452=DIRECTION('ref_axis',(0.,1.,9.73425822924114E-14));
#17453=DIRECTION('',(-1.,1.22464679914735E-16,1.19060305846873E-29));
#17454=DIRECTION('center_axis',(-1.,0.,0.));
#17455=DIRECTION('ref_axis',(0.,1.,9.73425822924114E-14));
#17456=DIRECTION('',(-1.,1.22464679914735E-16,1.19060305846873E-29));
#17457=DIRECTION('center_axis',(-1.,0.,0.));
#17458=DIRECTION('ref_axis',(0.,1.,9.73425822924114E-14));
#17459=DIRECTION('',(-1.,1.22464679914735E-16,1.19060305846873E-29));
#17460=DIRECTION('center_axis',(-1.,0.,0.));
#17461=DIRECTION('ref_axis',(0.,1.,9.73425822924114E-14));
#17462=DIRECTION('',(-1.,1.22464679914735E-16,1.19060305846873E-29));
#17463=DIRECTION('center_axis',(-1.,0.,0.));
#17464=DIRECTION('ref_axis',(0.,1.,9.73425822924114E-14));
#17465=DIRECTION('',(-1.,1.22464679914735E-16,1.19060305846873E-29));
#17466=DIRECTION('center_axis',(-1.,0.,0.));
#17467=DIRECTION('ref_axis',(0.,1.,9.73425822924114E-14));
#17468=DIRECTION('',(-1.,1.22464679914735E-16,1.19060305846873E-29));
#17469=DIRECTION('center_axis',(-1.,0.,0.));
#17470=DIRECTION('ref_axis',(0.,-0.608992615770512,-0.79317589092016));
#17471=DIRECTION('',(-1.,1.22464679914735E-16,1.19060305846873E-29));
#17472=DIRECTION('center_axis',(-1.,0.,0.));
#17473=DIRECTION('ref_axis',(0.,1.,9.73425822924114E-14));
#17474=DIRECTION('center_axis',(-1.,0.,0.));
#17475=DIRECTION('ref_axis',(0.,1.,9.73425822924114E-14));
#17476=DIRECTION('center_axis',(1.,0.,0.));
#17477=DIRECTION('ref_axis',(0.,1.,0.));
#17478=DIRECTION('',(0.,1.,0.));
#17479=DIRECTION('',(0.,0.,1.));
#17480=DIRECTION('',(0.,1.,0.));
#17481=DIRECTION('',(0.,0.,1.));
#17482=DIRECTION('',(0.,1.,0.));
#17483=DIRECTION('',(0.,0.,1.));
#17484=DIRECTION('',(0.,1.,0.));
#17485=DIRECTION('',(0.,0.,1.));
#17486=DIRECTION('center_axis',(-1.,0.,0.));
#17487=DIRECTION('ref_axis',(0.,1.,0.));
#17488=DIRECTION('center_axis',(1.,0.,0.));
#17489=DIRECTION('ref_axis',(0.,1.,0.));
#17490=DIRECTION('',(0.,-1.,0.));
#17491=DIRECTION('',(0.,0.,1.));
#17492=DIRECTION('',(0.,1.,0.));
#17493=DIRECTION('',(0.,0.,1.));
#17494=DIRECTION('center_axis',(0.,0.,1.));
#17495=DIRECTION('ref_axis',(1.,0.,0.));
#17496=DIRECTION('',(0.,-1.,0.));
#17497=DIRECTION('',(1.,0.,0.));
#17498=DIRECTION('',(-1.,0.,0.));
#17499=DIRECTION('center_axis',(0.,0.,1.));
#17500=DIRECTION('ref_axis',(1.,0.,0.));
#17501=DIRECTION('',(1.,0.,0.));
#17502=DIRECTION('',(-1.,0.,0.));
#17503=DIRECTION('center_axis',(0.,1.,0.));
#17504=DIRECTION('ref_axis',(-1.,0.,0.));
#17505=DIRECTION('',(1.,0.,0.));
#17506=DIRECTION('',(0.,0.,1.));
#17507=DIRECTION('center_axis',(0.,-1.,0.));
#17508=DIRECTION('ref_axis',(1.,0.,0.));
#17509=DIRECTION('',(-1.,0.,0.));
#17510=DIRECTION('',(0.,0.,1.));
#17511=DIRECTION('center_axis',(0.,0.,1.));
#17512=DIRECTION('ref_axis',(1.,0.,0.));
#17513=DIRECTION('',(-1.,0.,0.));
#17514=DIRECTION('',(0.,-1.,0.));
#17515=DIRECTION('center_axis',(0.,0.,1.));
#17516=DIRECTION('ref_axis',(1.,0.,0.));
#17517=DIRECTION('',(0.,-1.,0.));
#17518=DIRECTION('',(1.,0.,0.));
#17519=DIRECTION('center_axis',(0.,1.,0.));
#17520=DIRECTION('ref_axis',(-1.,0.,0.));
#17521=DIRECTION('',(-1.,0.,0.));
#17522=DIRECTION('',(0.,0.,1.));
#17523=DIRECTION('center_axis',(0.,-1.,0.));
#17524=DIRECTION('ref_axis',(1.,0.,0.));
#17525=DIRECTION('',(1.,0.,0.));
#17526=DIRECTION('',(0.,0.,1.));
#17527=DIRECTION('center_axis',(-1.,0.,0.));
#17528=DIRECTION('ref_axis',(0.,-1.,0.));
#17529=DIRECTION('',(0.,-1.,0.));
#17530=DIRECTION('center_axis',(0.,0.,1.));
#17531=DIRECTION('ref_axis',(1.,0.,0.));
#17532=DIRECTION('axis',(0.,0.,1.));
#17533=DIRECTION('refdir',(1.,0.,0.));
#17534=DIRECTION('center_axis',(0.,0.,-1.));
#17535=DIRECTION('ref_axis',(1.,0.,0.));
#17536=DIRECTION('center_axis',(0.,0.,-1.));
#17537=DIRECTION('ref_axis',(1.,0.,0.));
#17538=DIRECTION('',(0.,0.,-1.));
#17539=DIRECTION('center_axis',(0.,0.,1.));
#17540=DIRECTION('ref_axis',(1.,0.,0.));
#17541=DIRECTION('center_axis',(0.,0.,-1.));
#17542=DIRECTION('ref_axis',(1.,0.,0.));
#17543=DIRECTION('center_axis',(0.,0.,-1.));
#17544=DIRECTION('ref_axis',(1.,0.,0.));
#17545=DIRECTION('',(0.,0.,-1.));
#17546=DIRECTION('center_axis',(0.,0.,1.));
#17547=DIRECTION('ref_axis',(1.,0.,0.));
#17548=DIRECTION('center_axis',(1.,0.,0.));
#17549=DIRECTION('ref_axis',(0.,-1.,0.));
#17550=DIRECTION('',(1.,0.,0.));
#17551=DIRECTION('center_axis',(1.,0.,0.));
#17552=DIRECTION('ref_axis',(0.,-1.,0.));
#17553=DIRECTION('',(-1.,0.,0.));
#17554=DIRECTION('center_axis',(1.,0.,0.));
#17555=DIRECTION('ref_axis',(0.,-1.,0.));
#17556=DIRECTION('center_axis',(1.,0.,0.));
#17557=DIRECTION('ref_axis',(0.,-1.,0.));
#17558=DIRECTION('',(-1.,0.,0.));
#17559=DIRECTION('center_axis',(1.,0.,0.));
#17560=DIRECTION('ref_axis',(0.,-1.,0.));
#17561=DIRECTION('',(1.,0.,0.));
#17562=DIRECTION('center_axis',(1.,0.,0.));
#17563=DIRECTION('ref_axis',(0.,-1.,0.));
#17564=DIRECTION('center_axis',(1.,0.,0.));
#17565=DIRECTION('ref_axis',(0.,-1.,0.));
#17566=DIRECTION('',(0.,-1.,0.));
#17567=DIRECTION('',(0.,0.,-1.));
#17568=DIRECTION('',(0.,1.,0.));
#17569=DIRECTION('',(0.,0.,-1.));
#17570=DIRECTION('',(0.,-1.,0.));
#17571=DIRECTION('',(0.,0.,-1.));
#17572=DIRECTION('',(0.,1.,0.));
#17573=DIRECTION('',(0.,0.,-1.));
#17574=DIRECTION('',(0.,-1.,0.));
#17575=DIRECTION('',(0.,1.,0.));
#17576=DIRECTION('center_axis',(1.,0.,0.));
#17577=DIRECTION('ref_axis',(0.,1.,0.));
#17578=DIRECTION('center_axis',(-1.,0.,0.));
#17579=DIRECTION('ref_axis',(0.,-1.,0.));
#17580=DIRECTION('',(0.,-1.,0.));
#17581=DIRECTION('',(0.,0.,1.));
#17582=DIRECTION('',(0.,-1.,0.));
#17583=DIRECTION('',(0.,0.,-1.));
#17584=DIRECTION('',(0.,-1.,0.));
#17585=DIRECTION('',(0.,0.,-1.));
#17586=DIRECTION('',(0.,1.,0.));
#17587=DIRECTION('center_axis',(-1.,0.,0.));
#17588=DIRECTION('ref_axis',(0.,-1.,0.));
#17589=DIRECTION('',(0.,1.,0.));
#17590=DIRECTION('',(0.,0.,1.));
#17591=DIRECTION('',(0.,-1.,0.));
#17592=DIRECTION('',(0.,0.,1.));
#17593=DIRECTION('',(0.,-1.,0.));
#17594=DIRECTION('',(0.,0.,1.));
#17595=DIRECTION('',(0.,-1.,0.));
#17596=DIRECTION('center_axis',(0.,0.,-1.));
#17597=DIRECTION('ref_axis',(-1.,0.,0.));
#17598=DIRECTION('',(-1.,0.,0.));
#17599=DIRECTION('center_axis',(-1.,0.,0.));
#17600=DIRECTION('ref_axis',(0.,1.,0.));
#17601=DIRECTION('',(0.,-1.,0.));
#17602=DIRECTION('center_axis',(-1.,0.,0.));
#17603=DIRECTION('ref_axis',(0.,1.,0.));
#17604=DIRECTION('center_axis',(1.,0.,0.));
#17605=DIRECTION('ref_axis',(0.,1.,0.));
#17606=DIRECTION('center_axis',(-1.,0.,0.));
#17607=DIRECTION('ref_axis',(0.,6.12323399573677E-17,1.));
#17608=DIRECTION('',(-1.,0.,0.));
#17609=DIRECTION('center_axis',(-1.,0.,0.));
#17610=DIRECTION('ref_axis',(0.,1.,0.));
#17611=DIRECTION('',(1.,0.,0.));
#17612=DIRECTION('center_axis',(0.,0.,1.));
#17613=DIRECTION('ref_axis',(1.,0.,0.));
#17614=DIRECTION('',(-1.,0.,0.));
#17615=DIRECTION('',(0.,1.,0.));
#17616=DIRECTION('',(0.,1.,0.));
#17617=DIRECTION('',(1.,0.,0.));
#17618=DIRECTION('center_axis',(-1.,0.,0.));
#17619=DIRECTION('ref_axis',(0.,1.,0.));
#17620=DIRECTION('',(-1.,0.,0.));
#17621=DIRECTION('center_axis',(0.,0.,1.));
#17622=DIRECTION('ref_axis',(1.,0.,0.));
#17623=DIRECTION('',(-1.,0.,0.));
#17624=DIRECTION('',(1.,0.,0.));
#17625=DIRECTION('center_axis',(0.,-1.,0.));
#17626=DIRECTION('ref_axis',(-1.,0.,0.));
#17627=DIRECTION('center_axis',(0.,1.,0.));
#17628=DIRECTION('ref_axis',(1.,0.,0.));
#17629=DIRECTION('',(-1.,0.,0.));
#17630=DIRECTION('',(1.,0.,0.));
#17631=DIRECTION('center_axis',(0.,0.,1.));
#17632=DIRECTION('ref_axis',(1.,0.,0.));
#17633=DIRECTION('',(1.,0.,0.));
#17634=DIRECTION('center_axis',(0.,0.,-1.));
#17635=DIRECTION('ref_axis',(-1.,0.,0.));
#17636=DIRECTION('center_axis',(0.,-1.,0.));
#17637=DIRECTION('ref_axis',(-1.,0.,0.));
#17638=DIRECTION('',(-1.,0.,0.));
#17639=DIRECTION('center_axis',(0.,1.,0.));
#17640=DIRECTION('ref_axis',(1.,0.,0.));
#17641=DIRECTION('',(1.,0.,0.));
#17642=DIRECTION('center_axis',(0.,1.,0.));
#17643=DIRECTION('ref_axis',(-1.,0.,0.));
#17644=DIRECTION('',(-1.,0.,0.));
#17645=DIRECTION('',(0.,0.,1.));
#17646=DIRECTION('center_axis',(1.,0.,0.));
#17647=DIRECTION('ref_axis',(0.,1.,0.));
#17648=DIRECTION('',(0.,1.,0.));
#17649=DIRECTION('',(0.,0.,1.));
#17650=DIRECTION('center_axis',(0.,-1.,0.));
#17651=DIRECTION('ref_axis',(1.,0.,0.));
#17652=DIRECTION('',(1.,0.,0.));
#17653=DIRECTION('center_axis',(0.,0.,1.));
#17654=DIRECTION('ref_axis',(1.,0.,0.));
#17655=DIRECTION('axis',(0.,0.,1.));
#17656=DIRECTION('refdir',(1.,0.,0.));
#17657=DIRECTION('center_axis',(0.,0.,1.));
#17658=DIRECTION('ref_axis',(1.,0.,0.));
#17659=DIRECTION('',(0.,0.,-1.));
#17660=DIRECTION('center_axis',(0.,0.,-1.));
#17661=DIRECTION('ref_axis',(1.,0.,0.));
#17662=DIRECTION('center_axis',(0.,0.,1.));
#17663=DIRECTION('ref_axis',(1.,0.,0.));
#17664=DIRECTION('',(0.,0.,-1.));
#17665=DIRECTION('center_axis',(0.,0.,1.));
#17666=DIRECTION('ref_axis',(1.,0.,0.));
#17667=DIRECTION('',(0.,0.,-1.));
#17668=DIRECTION('center_axis',(0.,0.,1.));
#17669=DIRECTION('ref_axis',(1.,0.,0.));
#17670=DIRECTION('',(0.,0.,-1.));
#17671=DIRECTION('center_axis',(0.,0.,1.));
#17672=DIRECTION('ref_axis',(1.,0.,0.));
#17673=DIRECTION('',(0.,0.,-1.));
#17674=DIRECTION('center_axis',(0.,0.,1.));
#17675=DIRECTION('ref_axis',(1.,0.,0.));
#17676=DIRECTION('',(0.,0.,-1.));
#17677=DIRECTION('center_axis',(0.,0.,1.));
#17678=DIRECTION('ref_axis',(1.,0.,0.));
#17679=DIRECTION('',(0.,0.,-1.));
#17680=DIRECTION('center_axis',(0.,0.,1.));
#17681=DIRECTION('ref_axis',(1.,0.,0.));
#17682=DIRECTION('',(0.,0.,-1.));
#17683=DIRECTION('center_axis',(0.,0.,1.));
#17684=DIRECTION('ref_axis',(1.,0.,0.));
#17685=DIRECTION('',(0.,0.,-1.));
#17686=DIRECTION('center_axis',(0.,0.,1.));
#17687=DIRECTION('ref_axis',(1.,0.,0.));
#17688=DIRECTION('',(0.,0.,-1.));
#17689=DIRECTION('center_axis',(0.,0.,1.));
#17690=DIRECTION('ref_axis',(1.,0.,0.));
#17691=DIRECTION('',(0.,0.,-1.));
#17692=DIRECTION('center_axis',(0.,0.,1.));
#17693=DIRECTION('ref_axis',(1.,0.,0.));
#17694=DIRECTION('',(0.,0.,-1.));
#17695=DIRECTION('center_axis',(0.,0.,1.));
#17696=DIRECTION('ref_axis',(1.,0.,0.));
#17697=DIRECTION('',(0.,0.,-1.));
#17698=DIRECTION('center_axis',(0.,0.,1.));
#17699=DIRECTION('ref_axis',(1.,0.,0.));
#17700=DIRECTION('',(0.,0.,-1.));
#17701=DIRECTION('center_axis',(0.,0.,1.));
#17702=DIRECTION('ref_axis',(1.,0.,0.));
#17703=DIRECTION('',(0.,0.,-1.));
#17704=DIRECTION('center_axis',(0.,0.,1.));
#17705=DIRECTION('ref_axis',(1.,0.,0.));
#17706=DIRECTION('',(0.,0.,-1.));
#17707=DIRECTION('center_axis',(0.,0.,1.));
#17708=DIRECTION('ref_axis',(1.,0.,0.));
#17709=DIRECTION('',(0.,0.,-1.));
#17710=DIRECTION('center_axis',(0.,0.,1.));
#17711=DIRECTION('ref_axis',(1.,0.,0.));
#17712=DIRECTION('',(0.,0.,-1.));
#17713=DIRECTION('center_axis',(0.,0.,1.));
#17714=DIRECTION('ref_axis',(1.,0.,0.));
#17715=DIRECTION('',(0.,0.,-1.));
#17716=DIRECTION('center_axis',(0.,0.,1.));
#17717=DIRECTION('ref_axis',(1.,0.,0.));
#17718=DIRECTION('',(0.,0.,-1.));
#17719=DIRECTION('center_axis',(0.,0.,1.));
#17720=DIRECTION('ref_axis',(1.,0.,0.));
#17721=DIRECTION('',(0.,0.,-1.));
#17722=DIRECTION('center_axis',(0.,0.,1.));
#17723=DIRECTION('ref_axis',(1.,0.,0.));
#17724=DIRECTION('',(0.,0.,-1.));
#17725=DIRECTION('center_axis',(0.,0.,1.));
#17726=DIRECTION('ref_axis',(1.,0.,0.));
#17727=DIRECTION('',(0.,0.,-1.));
#17728=DIRECTION('center_axis',(0.,0.,1.));
#17729=DIRECTION('ref_axis',(1.,0.,0.));
#17730=DIRECTION('',(0.,0.,-1.));
#17731=DIRECTION('center_axis',(0.,0.,1.));
#17732=DIRECTION('ref_axis',(1.,0.,0.));
#17733=DIRECTION('',(0.,0.,-1.));
#17734=DIRECTION('center_axis',(0.,0.,1.));
#17735=DIRECTION('ref_axis',(1.,0.,0.));
#17736=DIRECTION('',(0.,0.,-1.));
#17737=DIRECTION('center_axis',(0.,0.,1.));
#17738=DIRECTION('ref_axis',(1.,0.,0.));
#17739=DIRECTION('',(0.,0.,-1.));
#17740=DIRECTION('center_axis',(0.,0.,1.));
#17741=DIRECTION('ref_axis',(1.,0.,0.));
#17742=DIRECTION('',(0.,0.,-1.));
#17743=DIRECTION('center_axis',(0.,0.,1.));
#17744=DIRECTION('ref_axis',(1.,0.,0.));
#17745=DIRECTION('',(0.,0.,-1.));
#17746=DIRECTION('center_axis',(0.,0.,1.));
#17747=DIRECTION('ref_axis',(1.,0.,0.));
#17748=DIRECTION('',(0.,0.,-1.));
#17749=DIRECTION('center_axis',(0.,0.,1.));
#17750=DIRECTION('ref_axis',(1.,0.,0.));
#17751=DIRECTION('',(0.,0.,-1.));
#17752=DIRECTION('center_axis',(0.,0.,1.));
#17753=DIRECTION('ref_axis',(1.,0.,0.));
#17754=DIRECTION('',(0.,0.,-1.));
#17755=DIRECTION('center_axis',(0.,0.,1.));
#17756=DIRECTION('ref_axis',(1.,0.,0.));
#17757=DIRECTION('',(0.,0.,-1.));
#17758=DIRECTION('center_axis',(0.,0.,1.));
#17759=DIRECTION('ref_axis',(1.,0.,0.));
#17760=DIRECTION('',(0.,0.,-1.));
#17761=DIRECTION('center_axis',(0.,0.,1.));
#17762=DIRECTION('ref_axis',(1.,0.,0.));
#17763=DIRECTION('',(0.,0.,-1.));
#17764=DIRECTION('center_axis',(0.,0.,1.));
#17765=DIRECTION('ref_axis',(1.,0.,0.));
#17766=DIRECTION('',(0.,0.,-1.));
#17767=DIRECTION('center_axis',(0.,0.,1.));
#17768=DIRECTION('ref_axis',(1.,0.,0.));
#17769=DIRECTION('center_axis',(0.,0.,-1.));
#17770=DIRECTION('ref_axis',(1.,0.,0.));
#17771=DIRECTION('',(0.,0.,-1.));
#17772=DIRECTION('center_axis',(0.,0.,1.));
#17773=DIRECTION('ref_axis',(1.,0.,0.));
#17774=DIRECTION('',(0.,0.,-1.));
#17775=DIRECTION('center_axis',(0.,0.,1.));
#17776=DIRECTION('ref_axis',(1.,0.,0.));
#17777=DIRECTION('center_axis',(0.,0.,1.));
#17778=DIRECTION('ref_axis',(0.968645259382149,-0.248447904954922,0.));
#17779=DIRECTION('',(0.,0.,1.));
#17780=DIRECTION('center_axis',(0.,0.,1.));
#17781=DIRECTION('ref_axis',(1.,-3.01021172098358E-13,0.));
#17782=DIRECTION('center_axis',(0.,0.,1.));
#17783=DIRECTION('ref_axis',(1.,-3.01021172098358E-13,0.));
#17784=DIRECTION('',(0.,0.,1.));
#17785=DIRECTION('center_axis',(0.,0.,1.));
#17786=DIRECTION('ref_axis',(1.,-3.01021172098358E-13,0.));
#17787=DIRECTION('',(0.,0.,1.));
#17788=DIRECTION('center_axis',(0.,0.,1.));
#17789=DIRECTION('ref_axis',(1.,-3.01021172098358E-13,0.));
#17790=DIRECTION('',(0.,0.,1.));
#17791=DIRECTION('center_axis',(0.,0.,1.));
#17792=DIRECTION('ref_axis',(1.,-3.01021172098358E-13,0.));
#17793=DIRECTION('',(0.,0.,1.));
#17794=DIRECTION('center_axis',(0.,0.,1.));
#17795=DIRECTION('ref_axis',(1.,-3.01021172098358E-13,0.));
#17796=DIRECTION('',(0.,0.,1.));
#17797=DIRECTION('center_axis',(0.,0.,1.));
#17798=DIRECTION('ref_axis',(1.,-3.01021172098358E-13,0.));
#17799=DIRECTION('',(0.,0.,1.));
#17800=DIRECTION('center_axis',(0.,0.,1.));
#17801=DIRECTION('ref_axis',(1.,-3.01021172098358E-13,0.));
#17802=DIRECTION('',(0.,0.,1.));
#17803=DIRECTION('center_axis',(0.,0.,1.));
#17804=DIRECTION('ref_axis',(1.,-3.01021172098358E-13,0.));
#17805=DIRECTION('',(0.,0.,1.));
#17806=DIRECTION('center_axis',(0.,0.,1.));
#17807=DIRECTION('ref_axis',(1.,-3.01021172098358E-13,0.));
#17808=DIRECTION('',(0.,0.,1.));
#17809=DIRECTION('center_axis',(0.,0.,1.));
#17810=DIRECTION('ref_axis',(1.,-3.01021172098358E-13,0.));
#17811=DIRECTION('',(0.,0.,1.));
#17812=DIRECTION('center_axis',(0.,0.,1.));
#17813=DIRECTION('ref_axis',(1.,-3.01021172098358E-13,0.));
#17814=DIRECTION('',(0.,0.,1.));
#17815=DIRECTION('center_axis',(0.,0.,1.));
#17816=DIRECTION('ref_axis',(1.,-3.01021172098358E-13,0.));
#17817=DIRECTION('',(0.,0.,1.));
#17818=DIRECTION('center_axis',(0.,0.,1.));
#17819=DIRECTION('ref_axis',(1.,-3.01021172098358E-13,0.));
#17820=DIRECTION('',(0.,0.,1.));
#17821=DIRECTION('center_axis',(0.,0.,1.));
#17822=DIRECTION('ref_axis',(1.,-3.01021172098358E-13,0.));
#17823=DIRECTION('',(0.,0.,1.));
#17824=DIRECTION('center_axis',(0.,0.,1.));
#17825=DIRECTION('ref_axis',(1.,-3.01021172098358E-13,0.));
#17826=DIRECTION('',(0.,0.,1.));
#17827=DIRECTION('center_axis',(0.,0.,1.));
#17828=DIRECTION('ref_axis',(1.,-3.01021172098358E-13,0.));
#17829=DIRECTION('',(0.,0.,1.));
#17830=DIRECTION('center_axis',(0.,0.,1.));
#17831=DIRECTION('ref_axis',(1.,-3.01021172098358E-13,0.));
#17832=DIRECTION('',(0.,0.,1.));
#17833=DIRECTION('center_axis',(0.,0.,1.));
#17834=DIRECTION('ref_axis',(1.,-3.01021172098358E-13,0.));
#17835=DIRECTION('',(0.,0.,1.));
#17836=DIRECTION('center_axis',(0.,0.,1.));
#17837=DIRECTION('ref_axis',(1.,-3.01021172098358E-13,0.));
#17838=DIRECTION('',(0.,0.,1.));
#17839=DIRECTION('center_axis',(0.,0.,1.));
#17840=DIRECTION('ref_axis',(1.,-3.01021172098358E-13,0.));
#17841=DIRECTION('',(0.,0.,1.));
#17842=DIRECTION('center_axis',(0.,0.,1.));
#17843=DIRECTION('ref_axis',(1.,-3.01021172098358E-13,0.));
#17844=DIRECTION('',(0.,0.,1.));
#17845=DIRECTION('center_axis',(0.,0.,1.));
#17846=DIRECTION('ref_axis',(1.,-3.01021172098358E-13,0.));
#17847=DIRECTION('',(0.,0.,1.));
#17848=DIRECTION('center_axis',(0.,0.,1.));
#17849=DIRECTION('ref_axis',(1.,-3.01021172098358E-13,0.));
#17850=DIRECTION('',(0.,0.,1.));
#17851=DIRECTION('center_axis',(0.,0.,1.));
#17852=DIRECTION('ref_axis',(1.,-3.01021172098358E-13,0.));
#17853=DIRECTION('',(0.,0.,1.));
#17854=DIRECTION('center_axis',(0.,0.,1.));
#17855=DIRECTION('ref_axis',(1.,-3.01021172098358E-13,0.));
#17856=DIRECTION('',(0.,0.,1.));
#17857=DIRECTION('center_axis',(0.,0.,1.));
#17858=DIRECTION('ref_axis',(1.,-3.01021172098358E-13,0.));
#17859=DIRECTION('',(0.,0.,1.));
#17860=DIRECTION('center_axis',(0.,0.,1.));
#17861=DIRECTION('ref_axis',(1.,-3.01021172098358E-13,0.));
#17862=DIRECTION('',(0.,0.,1.));
#17863=DIRECTION('center_axis',(0.,0.,1.));
#17864=DIRECTION('ref_axis',(1.,-3.01021172098358E-13,0.));
#17865=DIRECTION('',(0.,0.,1.));
#17866=DIRECTION('center_axis',(0.,0.,1.));
#17867=DIRECTION('ref_axis',(1.,-3.01021172098358E-13,0.));
#17868=DIRECTION('',(0.,0.,1.));
#17869=DIRECTION('center_axis',(0.,0.,1.));
#17870=DIRECTION('ref_axis',(1.,-3.01021172098358E-13,0.));
#17871=DIRECTION('',(0.,0.,1.));
#17872=DIRECTION('center_axis',(0.,0.,1.));
#17873=DIRECTION('ref_axis',(1.,-3.01021172098358E-13,0.));
#17874=DIRECTION('',(0.,0.,1.));
#17875=DIRECTION('center_axis',(0.,0.,1.));
#17876=DIRECTION('ref_axis',(1.,-3.01021172098358E-13,0.));
#17877=DIRECTION('',(0.,0.,1.));
#17878=DIRECTION('center_axis',(0.,0.,1.));
#17879=DIRECTION('ref_axis',(1.,-3.01021172098358E-13,0.));
#17880=DIRECTION('',(0.,0.,1.));
#17881=DIRECTION('center_axis',(0.,0.,1.));
#17882=DIRECTION('ref_axis',(1.,-3.01021172098358E-13,0.));
#17883=DIRECTION('',(0.,0.,1.));
#17884=DIRECTION('center_axis',(0.,0.,1.));
#17885=DIRECTION('ref_axis',(1.,-3.01021172098358E-13,0.));
#17886=DIRECTION('',(0.,0.,1.));
#17887=DIRECTION('center_axis',(0.866025403784439,0.5,0.));
#17888=DIRECTION('ref_axis',(0.5,-0.866025403784439,0.));
#17889=DIRECTION('',(0.5,-0.866025403784439,0.));
#17890=DIRECTION('',(0.,0.,-1.));
#17891=DIRECTION('',(0.5,-0.866025403784439,0.));
#17892=DIRECTION('',(0.,0.,-1.));
#17893=DIRECTION('center_axis',(1.20185167898973E-16,1.,0.));
#17894=DIRECTION('ref_axis',(1.,-1.20185167898973E-16,0.));
#17895=DIRECTION('',(1.,-1.20185167898973E-16,0.));
#17896=DIRECTION('',(0.,0.,-1.));
#17897=DIRECTION('',(1.,-1.20185167898973E-16,0.));
#17898=DIRECTION('center_axis',(-0.866025403784439,0.5,0.));
#17899=DIRECTION('ref_axis',(0.5,0.866025403784439,0.));
#17900=DIRECTION('',(0.5,0.866025403784439,0.));
#17901=DIRECTION('',(0.,0.,-1.));
#17902=DIRECTION('',(0.5,0.866025403784439,0.));
#17903=DIRECTION('center_axis',(-0.866025403784439,-0.5,0.));
#17904=DIRECTION('ref_axis',(-0.5,0.866025403784439,0.));
#17905=DIRECTION('',(-0.5,0.866025403784439,0.));
#17906=DIRECTION('',(0.,0.,-1.));
#17907=DIRECTION('',(-0.5,0.866025403784439,0.));
#17908=DIRECTION('center_axis',(-2.40370335797945E-16,-1.,0.));
#17909=DIRECTION('ref_axis',(-1.,2.40370335797945E-16,0.));
#17910=DIRECTION('',(-1.,2.40370335797945E-16,0.));
#17911=DIRECTION('',(0.,0.,-1.));
#17912=DIRECTION('',(-1.,2.40370335797945E-16,0.));
#17913=DIRECTION('center_axis',(0.866025403784439,-0.5,0.));
#17914=DIRECTION('ref_axis',(-0.5,-0.866025403784439,0.));
#17915=DIRECTION('',(-0.5,-0.866025403784439,0.));
#17916=DIRECTION('',(-0.5,-0.866025403784439,0.));
#17917=DIRECTION('center_axis',(0.,0.,-1.));
#17918=DIRECTION('ref_axis',(-1.,0.,0.));
#17919=DIRECTION('center_axis',(0.,0.,1.));
#17920=DIRECTION('ref_axis',(1.,0.,0.));
#17921=DIRECTION('center_axis',(0.,0.,1.));
#17922=DIRECTION('ref_axis',(1.,0.,0.));
#17923=DIRECTION('',(0.,0.,1.));
#17924=DIRECTION('center_axis',(0.,0.,1.));
#17925=DIRECTION('ref_axis',(1.,0.,0.));
#17926=DIRECTION('center_axis',(0.,0.,-1.));
#17927=DIRECTION('ref_axis',(-1.,0.,0.));
#17928=DIRECTION('center_axis',(0.,0.,1.));
#17929=DIRECTION('ref_axis',(1.,0.,0.));
#17930=DIRECTION('center_axis',(0.,0.,1.));
#17931=DIRECTION('ref_axis',(1.,0.,0.));
#17932=DIRECTION('center_axis',(0.,0.,1.));
#17933=DIRECTION('ref_axis',(1.,0.,0.));
#17934=DIRECTION('center_axis',(0.,0.,-1.));
#17935=DIRECTION('ref_axis',(1.,0.,0.));
#17936=DIRECTION('',(0.,0.,-1.));
#17937=DIRECTION('center_axis',(0.,0.,1.));
#17938=DIRECTION('ref_axis',(1.,0.,0.));
#17939=DIRECTION('center_axis',(0.,0.,1.));
#17940=DIRECTION('ref_axis',(0.889074521506822,0.457762487767855,0.));
#17941=DIRECTION('center_axis',(0.,0.,-1.));
#17942=DIRECTION('ref_axis',(1.,-3.01021172098358E-13,0.));
#17943=DIRECTION('center_axis',(0.,0.,1.));
#17944=DIRECTION('ref_axis',(1.,0.,0.));
#17945=DIRECTION('center_axis',(0.,0.,1.));
#17946=DIRECTION('ref_axis',(1.,0.,0.));
#17947=DIRECTION('center_axis',(0.,0.,1.));
#17948=DIRECTION('ref_axis',(1.,0.,0.));
#17949=DIRECTION('center_axis',(0.,0.,1.));
#17950=DIRECTION('ref_axis',(1.,0.,0.));
#17951=DIRECTION('center_axis',(0.,0.,1.));
#17952=DIRECTION('ref_axis',(1.,0.,0.));
#17953=DIRECTION('',(0.,0.,-1.));
#17954=DIRECTION('center_axis',(0.,0.,1.));
#17955=DIRECTION('ref_axis',(1.,0.,0.));
#17956=DIRECTION('center_axis',(0.,0.,1.));
#17957=DIRECTION('ref_axis',(1.,0.,0.));
#17958=DIRECTION('axis',(0.,0.,1.));
#17959=DIRECTION('refdir',(1.,0.,0.));
#17960=DIRECTION('center_axis',(-1.,0.,0.));
#17961=DIRECTION('ref_axis',(0.,1.,0.));
#17962=DIRECTION('',(0.,0.,1.));
#17963=DIRECTION('',(0.,-1.,0.));
#17964=DIRECTION('',(0.,0.,-1.));
#17965=DIRECTION('',(0.,1.,0.));
#17966=DIRECTION('center_axis',(1.,0.,0.));
#17967=DIRECTION('ref_axis',(0.,-1.,0.));
#17968=DIRECTION('',(0.,0.,-1.));
#17969=DIRECTION('',(0.,-1.,0.));
#17970=DIRECTION('',(0.,0.,1.));
#17971=DIRECTION('',(0.,1.,0.));
#17972=DIRECTION('center_axis',(0.,0.,1.));
#17973=DIRECTION('ref_axis',(1.,0.,0.));
#17974=DIRECTION('center_axis',(0.,0.,1.));
#17975=DIRECTION('ref_axis',(1.,0.,0.));
#17976=DIRECTION('center_axis',(0.,0.,-1.));
#17977=DIRECTION('ref_axis',(1.,0.,0.));
#17978=DIRECTION('center_axis',(0.,0.,1.));
#17979=DIRECTION('ref_axis',(6.12323399573677E-17,-1.,0.));
#17980=DIRECTION('center_axis',(0.,0.,-1.));
#17981=DIRECTION('ref_axis',(1.,0.,0.));
#17982=DIRECTION('center_axis',(0.,0.,1.));
#17983=DIRECTION('ref_axis',(6.12323399573677E-17,-1.,0.));
#17984=DIRECTION('center_axis',(0.,0.,1.));
#17985=DIRECTION('ref_axis',(1.,0.,0.));
#17986=DIRECTION('center_axis',(0.,0.,1.));
#17987=DIRECTION('ref_axis',(1.,0.,0.));
#17988=DIRECTION('axis',(0.,0.,1.));
#17989=DIRECTION('refdir',(1.,0.,0.));
#17990=DIRECTION('center_axis',(0.,0.,1.));
#17991=DIRECTION('ref_axis',(1.,0.,0.));
#17992=DIRECTION('center_axis',(0.,0.,-1.));
#17993=DIRECTION('ref_axis',(1.,0.,0.));
#17994=DIRECTION('',(0.,0.,-1.));
#17995=DIRECTION('center_axis',(0.,0.,-1.));
#17996=DIRECTION('ref_axis',(1.,0.,0.));
#17997=DIRECTION('center_axis',(0.,0.,1.));
#17998=DIRECTION('ref_axis',(1.,0.,0.));
#17999=DIRECTION('center_axis',(0.,0.,1.));
#18000=DIRECTION('ref_axis',(1.,0.,0.));
#18001=DIRECTION('',(0.,0.,-1.));
#18002=DIRECTION('center_axis',(0.,0.,1.));
#18003=DIRECTION('ref_axis',(1.,0.,0.));
#18004=DIRECTION('center_axis',(0.,0.,1.));
#18005=DIRECTION('ref_axis',(1.,0.,0.));
#18006=DIRECTION('center_axis',(0.,0.,1.));
#18007=DIRECTION('ref_axis',(1.,0.,0.));
#18008=DIRECTION('axis',(0.,0.,1.));
#18009=DIRECTION('refdir',(1.,0.,0.));
#18010=DIRECTION('center_axis',(0.,0.,1.));
#18011=DIRECTION('ref_axis',(1.,0.,0.));
#18012=DIRECTION('center_axis',(0.,0.,-1.));
#18013=DIRECTION('ref_axis',(1.,0.,0.));
#18014=DIRECTION('',(0.,0.,-1.));
#18015=DIRECTION('center_axis',(0.,0.,-1.));
#18016=DIRECTION('ref_axis',(1.,0.,0.));
#18017=DIRECTION('center_axis',(0.,0.,1.));
#18018=DIRECTION('ref_axis',(1.,0.,0.));
#18019=DIRECTION('center_axis',(0.,0.,1.));
#18020=DIRECTION('ref_axis',(1.,0.,0.));
#18021=DIRECTION('',(0.,0.,-1.));
#18022=DIRECTION('center_axis',(0.,0.,1.));
#18023=DIRECTION('ref_axis',(1.,0.,0.));
#18024=DIRECTION('center_axis',(0.,0.,1.));
#18025=DIRECTION('ref_axis',(1.,0.,0.));
#18026=DIRECTION('center_axis',(0.,0.,1.));
#18027=DIRECTION('ref_axis',(1.,0.,0.));
#18028=DIRECTION('axis',(0.,0.,1.));
#18029=DIRECTION('refdir',(1.,0.,0.));
#18030=DIRECTION('center_axis',(0.,0.,1.));
#18031=DIRECTION('ref_axis',(1.,0.,0.));
#18032=DIRECTION('',(0.,0.,-1.));
#18033=DIRECTION('center_axis',(0.,0.,-1.));
#18034=DIRECTION('ref_axis',(1.,0.,0.));
#18035=DIRECTION('center_axis',(0.,0.,1.));
#18036=DIRECTION('ref_axis',(1.,0.,0.));
#18037=DIRECTION('',(0.,0.,-1.));
#18038=DIRECTION('center_axis',(0.,0.,1.));
#18039=DIRECTION('ref_axis',(1.,0.,0.));
#18040=DIRECTION('',(0.,0.,-1.));
#18041=DIRECTION('center_axis',(0.,0.,1.));
#18042=DIRECTION('ref_axis',(1.,0.,0.));
#18043=DIRECTION('',(0.,0.,-1.));
#18044=DIRECTION('center_axis',(0.,0.,1.));
#18045=DIRECTION('ref_axis',(1.,0.,0.));
#18046=DIRECTION('',(0.,0.,-1.));
#18047=DIRECTION('center_axis',(0.,0.,1.));
#18048=DIRECTION('ref_axis',(1.,0.,0.));
#18049=DIRECTION('',(0.,0.,-1.));
#18050=DIRECTION('center_axis',(0.,0.,1.));
#18051=DIRECTION('ref_axis',(1.,0.,0.));
#18052=DIRECTION('',(0.,0.,-1.));
#18053=DIRECTION('center_axis',(0.,0.,1.));
#18054=DIRECTION('ref_axis',(1.,0.,0.));
#18055=DIRECTION('',(0.,0.,-1.));
#18056=DIRECTION('center_axis',(0.,0.,1.));
#18057=DIRECTION('ref_axis',(1.,0.,0.));
#18058=DIRECTION('',(0.,0.,-1.));
#18059=DIRECTION('center_axis',(0.,0.,1.));
#18060=DIRECTION('ref_axis',(1.,0.,0.));
#18061=DIRECTION('',(0.,0.,-1.));
#18062=DIRECTION('center_axis',(0.,0.,1.));
#18063=DIRECTION('ref_axis',(1.,0.,0.));
#18064=DIRECTION('',(0.,0.,-1.));
#18065=DIRECTION('center_axis',(0.,0.,1.));
#18066=DIRECTION('ref_axis',(1.,0.,0.));
#18067=DIRECTION('',(0.,0.,-1.));
#18068=DIRECTION('center_axis',(0.,0.,1.));
#18069=DIRECTION('ref_axis',(1.,0.,0.));
#18070=DIRECTION('',(0.,0.,-1.));
#18071=DIRECTION('center_axis',(0.,0.,1.));
#18072=DIRECTION('ref_axis',(1.,0.,0.));
#18073=DIRECTION('',(0.,0.,-1.));
#18074=DIRECTION('center_axis',(0.,0.,1.));
#18075=DIRECTION('ref_axis',(1.,0.,0.));
#18076=DIRECTION('',(0.,0.,-1.));
#18077=DIRECTION('center_axis',(0.,0.,1.));
#18078=DIRECTION('ref_axis',(1.,0.,0.));
#18079=DIRECTION('',(0.,0.,-1.));
#18080=DIRECTION('center_axis',(0.,0.,1.));
#18081=DIRECTION('ref_axis',(1.,0.,0.));
#18082=DIRECTION('',(0.,0.,-1.));
#18083=DIRECTION('center_axis',(0.,0.,1.));
#18084=DIRECTION('ref_axis',(1.,0.,0.));
#18085=DIRECTION('',(0.,0.,-1.));
#18086=DIRECTION('center_axis',(0.,0.,1.));
#18087=DIRECTION('ref_axis',(1.,0.,0.));
#18088=DIRECTION('',(0.,0.,-1.));
#18089=DIRECTION('center_axis',(0.,0.,1.));
#18090=DIRECTION('ref_axis',(1.,0.,0.));
#18091=DIRECTION('',(0.,0.,-1.));
#18092=DIRECTION('center_axis',(0.,0.,1.));
#18093=DIRECTION('ref_axis',(1.,0.,0.));
#18094=DIRECTION('',(0.,0.,-1.));
#18095=DIRECTION('center_axis',(0.,0.,1.));
#18096=DIRECTION('ref_axis',(1.,0.,0.));
#18097=DIRECTION('',(0.,0.,-1.));
#18098=DIRECTION('center_axis',(0.,0.,1.));
#18099=DIRECTION('ref_axis',(1.,0.,0.));
#18100=DIRECTION('',(0.,0.,-1.));
#18101=DIRECTION('center_axis',(0.,0.,1.));
#18102=DIRECTION('ref_axis',(1.,0.,0.));
#18103=DIRECTION('',(0.,0.,-1.));
#18104=DIRECTION('center_axis',(0.,0.,1.));
#18105=DIRECTION('ref_axis',(1.,0.,0.));
#18106=DIRECTION('',(0.,0.,-1.));
#18107=DIRECTION('center_axis',(0.,0.,1.));
#18108=DIRECTION('ref_axis',(1.,0.,0.));
#18109=DIRECTION('',(0.,0.,-1.));
#18110=DIRECTION('center_axis',(0.,0.,1.));
#18111=DIRECTION('ref_axis',(1.,0.,0.));
#18112=DIRECTION('',(0.,0.,-1.));
#18113=DIRECTION('center_axis',(0.,0.,1.));
#18114=DIRECTION('ref_axis',(1.,0.,0.));
#18115=DIRECTION('',(0.,0.,-1.));
#18116=DIRECTION('center_axis',(0.,0.,1.));
#18117=DIRECTION('ref_axis',(1.,0.,0.));
#18118=DIRECTION('',(0.,0.,-1.));
#18119=DIRECTION('center_axis',(0.,0.,1.));
#18120=DIRECTION('ref_axis',(1.,0.,0.));
#18121=DIRECTION('',(0.,0.,-1.));
#18122=DIRECTION('center_axis',(0.,0.,1.));
#18123=DIRECTION('ref_axis',(1.,0.,0.));
#18124=DIRECTION('',(0.,0.,-1.));
#18125=DIRECTION('center_axis',(0.,0.,1.));
#18126=DIRECTION('ref_axis',(1.,0.,0.));
#18127=DIRECTION('',(0.,0.,-1.));
#18128=DIRECTION('center_axis',(0.,0.,1.));
#18129=DIRECTION('ref_axis',(1.,0.,0.));
#18130=DIRECTION('',(0.,0.,-1.));
#18131=DIRECTION('center_axis',(0.,0.,1.));
#18132=DIRECTION('ref_axis',(1.,0.,0.));
#18133=DIRECTION('',(0.,0.,-1.));
#18134=DIRECTION('center_axis',(0.,0.,1.));
#18135=DIRECTION('ref_axis',(1.,0.,0.));
#18136=DIRECTION('',(0.,0.,-1.));
#18137=DIRECTION('center_axis',(0.,0.,1.));
#18138=DIRECTION('ref_axis',(1.,0.,0.));
#18139=DIRECTION('',(0.,0.,-1.));
#18140=DIRECTION('center_axis',(0.,0.,1.));
#18141=DIRECTION('ref_axis',(1.,0.,0.));
#18142=DIRECTION('',(0.,0.,-1.));
#18143=DIRECTION('center_axis',(0.,0.,1.));
#18144=DIRECTION('ref_axis',(1.,0.,0.));
#18145=DIRECTION('',(0.,0.,-1.));
#18146=DIRECTION('center_axis',(0.,0.,1.));
#18147=DIRECTION('ref_axis',(1.,0.,0.));
#18148=DIRECTION('',(0.,0.,-1.));
#18149=DIRECTION('center_axis',(0.,0.,1.));
#18150=DIRECTION('ref_axis',(0.997336311962016,-0.0729402552915997,0.));
#18151=DIRECTION('',(0.,0.,1.));
#18152=DIRECTION('center_axis',(0.,0.,-1.));
#18153=DIRECTION('ref_axis',(1.,-4.53607687595903E-13,0.));
#18154=DIRECTION('center_axis',(0.,0.,1.));
#18155=DIRECTION('ref_axis',(1.,-4.53607687595903E-13,0.));
#18156=DIRECTION('',(0.,0.,1.));
#18157=DIRECTION('center_axis',(0.,0.,1.));
#18158=DIRECTION('ref_axis',(1.,-4.53607687595903E-13,0.));
#18159=DIRECTION('',(0.,0.,1.));
#18160=DIRECTION('center_axis',(0.,0.,1.));
#18161=DIRECTION('ref_axis',(1.,-4.53607687595903E-13,0.));
#18162=DIRECTION('',(0.,0.,1.));
#18163=DIRECTION('center_axis',(0.,0.,1.));
#18164=DIRECTION('ref_axis',(1.,-4.53607687595903E-13,0.));
#18165=DIRECTION('',(0.,0.,1.));
#18166=DIRECTION('center_axis',(0.,0.,1.));
#18167=DIRECTION('ref_axis',(1.,-4.53607687595903E-13,0.));
#18168=DIRECTION('',(0.,0.,1.));
#18169=DIRECTION('center_axis',(0.,0.,1.));
#18170=DIRECTION('ref_axis',(1.,-4.53607687595903E-13,0.));
#18171=DIRECTION('',(0.,0.,1.));
#18172=DIRECTION('center_axis',(0.,0.,1.));
#18173=DIRECTION('ref_axis',(1.,-4.53607687595903E-13,0.));
#18174=DIRECTION('',(0.,0.,1.));
#18175=DIRECTION('center_axis',(0.,0.,1.));
#18176=DIRECTION('ref_axis',(1.,-4.53607687595903E-13,0.));
#18177=DIRECTION('',(0.,0.,1.));
#18178=DIRECTION('center_axis',(0.,0.,1.));
#18179=DIRECTION('ref_axis',(1.,-4.53607687595903E-13,0.));
#18180=DIRECTION('',(0.,0.,1.));
#18181=DIRECTION('center_axis',(0.,0.,1.));
#18182=DIRECTION('ref_axis',(1.,-4.53607687595903E-13,0.));
#18183=DIRECTION('',(0.,0.,1.));
#18184=DIRECTION('center_axis',(0.,0.,1.));
#18185=DIRECTION('ref_axis',(1.,-4.53607687595903E-13,0.));
#18186=DIRECTION('',(0.,0.,1.));
#18187=DIRECTION('center_axis',(0.,0.,1.));
#18188=DIRECTION('ref_axis',(1.,-4.53607687595903E-13,0.));
#18189=DIRECTION('',(0.,0.,1.));
#18190=DIRECTION('center_axis',(0.,0.,1.));
#18191=DIRECTION('ref_axis',(1.,-4.53607687595903E-13,0.));
#18192=DIRECTION('',(0.,0.,1.));
#18193=DIRECTION('center_axis',(0.,0.,1.));
#18194=DIRECTION('ref_axis',(1.,-4.53607687595903E-13,0.));
#18195=DIRECTION('',(0.,0.,1.));
#18196=DIRECTION('center_axis',(0.,0.,1.));
#18197=DIRECTION('ref_axis',(1.,-4.53607687595903E-13,0.));
#18198=DIRECTION('',(0.,0.,1.));
#18199=DIRECTION('center_axis',(0.,0.,1.));
#18200=DIRECTION('ref_axis',(1.,-4.53607687595903E-13,0.));
#18201=DIRECTION('',(0.,0.,1.));
#18202=DIRECTION('center_axis',(0.,0.,1.));
#18203=DIRECTION('ref_axis',(1.,-4.53607687595903E-13,0.));
#18204=DIRECTION('',(0.,0.,1.));
#18205=DIRECTION('center_axis',(0.,0.,1.));
#18206=DIRECTION('ref_axis',(1.,-4.53607687595903E-13,0.));
#18207=DIRECTION('',(0.,0.,1.));
#18208=DIRECTION('center_axis',(0.,0.,1.));
#18209=DIRECTION('ref_axis',(1.,-4.53607687595903E-13,0.));
#18210=DIRECTION('',(0.,0.,1.));
#18211=DIRECTION('center_axis',(0.,0.,1.));
#18212=DIRECTION('ref_axis',(1.,-4.53607687595903E-13,0.));
#18213=DIRECTION('',(0.,0.,1.));
#18214=DIRECTION('center_axis',(0.,0.,1.));
#18215=DIRECTION('ref_axis',(1.,-4.53607687595903E-13,0.));
#18216=DIRECTION('',(0.,0.,1.));
#18217=DIRECTION('center_axis',(0.,0.,1.));
#18218=DIRECTION('ref_axis',(1.,-4.53607687595903E-13,0.));
#18219=DIRECTION('',(0.,0.,1.));
#18220=DIRECTION('center_axis',(0.,0.,1.));
#18221=DIRECTION('ref_axis',(1.,-4.53607687595903E-13,0.));
#18222=DIRECTION('',(0.,0.,1.));
#18223=DIRECTION('center_axis',(0.,0.,1.));
#18224=DIRECTION('ref_axis',(1.,-4.53607687595903E-13,0.));
#18225=DIRECTION('',(0.,0.,1.));
#18226=DIRECTION('center_axis',(0.,0.,1.));
#18227=DIRECTION('ref_axis',(1.,-4.53607687595903E-13,0.));
#18228=DIRECTION('',(0.,0.,1.));
#18229=DIRECTION('center_axis',(0.,0.,1.));
#18230=DIRECTION('ref_axis',(1.,-4.53607687595903E-13,0.));
#18231=DIRECTION('',(0.,0.,1.));
#18232=DIRECTION('center_axis',(0.,0.,1.));
#18233=DIRECTION('ref_axis',(1.,-4.53607687595903E-13,0.));
#18234=DIRECTION('',(0.,0.,1.));
#18235=DIRECTION('center_axis',(0.,0.,1.));
#18236=DIRECTION('ref_axis',(1.,-4.53607687595903E-13,0.));
#18237=DIRECTION('',(0.,0.,1.));
#18238=DIRECTION('center_axis',(0.,0.,1.));
#18239=DIRECTION('ref_axis',(1.,-4.53607687595903E-13,0.));
#18240=DIRECTION('',(0.,0.,1.));
#18241=DIRECTION('center_axis',(0.,0.,1.));
#18242=DIRECTION('ref_axis',(1.,-4.53607687595903E-13,0.));
#18243=DIRECTION('',(0.,0.,1.));
#18244=DIRECTION('center_axis',(0.,0.,1.));
#18245=DIRECTION('ref_axis',(1.,-4.53607687595903E-13,0.));
#18246=DIRECTION('',(0.,0.,1.));
#18247=DIRECTION('center_axis',(0.,0.,1.));
#18248=DIRECTION('ref_axis',(1.,-4.53607687595903E-13,0.));
#18249=DIRECTION('',(0.,0.,1.));
#18250=DIRECTION('center_axis',(0.,0.,1.));
#18251=DIRECTION('ref_axis',(1.,-4.53607687595903E-13,0.));
#18252=DIRECTION('',(0.,0.,1.));
#18253=DIRECTION('center_axis',(0.,0.,1.));
#18254=DIRECTION('ref_axis',(1.,-4.53607687595903E-13,0.));
#18255=DIRECTION('',(0.,0.,1.));
#18256=DIRECTION('center_axis',(0.,0.,1.));
#18257=DIRECTION('ref_axis',(1.,-4.53607687595903E-13,0.));
#18258=DIRECTION('',(0.,0.,1.));
#18259=DIRECTION('center_axis',(0.,0.,1.));
#18260=DIRECTION('ref_axis',(1.,-4.53607687595903E-13,0.));
#18261=DIRECTION('',(0.,0.,1.));
#18262=DIRECTION('center_axis',(0.,0.,1.));
#18263=DIRECTION('ref_axis',(1.,-4.53607687595903E-13,0.));
#18264=DIRECTION('',(0.,0.,1.));
#18265=DIRECTION('center_axis',(0.,0.,1.));
#18266=DIRECTION('ref_axis',(1.,-4.53607687595903E-13,0.));
#18267=DIRECTION('',(0.,0.,1.));
#18268=DIRECTION('center_axis',(0.,0.,-1.));
#18269=DIRECTION('ref_axis',(1.,0.,0.));
#18270=DIRECTION('center_axis',(0.,0.,-1.));
#18271=DIRECTION('ref_axis',(1.,0.,0.));
#18272=DIRECTION('',(0.707106781186547,8.65956056235493E-17,0.707106781186548));
#18273=DIRECTION('center_axis',(0.,0.,1.));
#18274=DIRECTION('ref_axis',(1.,0.,0.));
#18275=DIRECTION('center_axis',(0.,0.,1.));
#18276=DIRECTION('ref_axis',(1.,-4.53607687595903E-13,0.));
#18277=DIRECTION('center_axis',(0.,0.,-1.));
#18278=DIRECTION('ref_axis',(1.,-4.53607687595903E-13,0.));
#18279=DIRECTION('center_axis',(0.,0.,1.));
#18280=DIRECTION('ref_axis',(1.,0.,0.));
#18281=DIRECTION('center_axis',(-1.92296268638356E-16,-1.,0.));
#18282=DIRECTION('ref_axis',(1.,-1.92296268638356E-16,0.));
#18283=DIRECTION('',(1.,-1.92296268638356E-16,0.));
#18284=DIRECTION('',(0.,0.,1.));
#18285=DIRECTION('',(1.,-1.92296268638356E-16,0.));
#18286=DIRECTION('',(0.,0.,1.));
#18287=DIRECTION('center_axis',(-0.866025403784439,-0.5,0.));
#18288=DIRECTION('ref_axis',(0.5,-0.866025403784439,0.));
#18289=DIRECTION('',(0.5,-0.866025403784439,0.));
#18290=DIRECTION('',(0.,0.,1.));
#18291=DIRECTION('',(0.5,-0.866025403784439,0.));
#18292=DIRECTION('center_axis',(-0.866025403784439,0.5,0.));
#18293=DIRECTION('ref_axis',(-0.5,-0.866025403784438,0.));
#18294=DIRECTION('',(-0.5,-0.866025403784438,0.));
#18295=DIRECTION('',(0.,0.,1.));
#18296=DIRECTION('',(-0.5,-0.866025403784439,0.));
#18297=DIRECTION('center_axis',(1.92296268638356E-16,1.,0.));
#18298=DIRECTION('ref_axis',(-1.,1.92296268638356E-16,0.));
#18299=DIRECTION('',(-1.,1.92296268638356E-16,0.));
#18300=DIRECTION('',(0.,0.,1.));
#18301=DIRECTION('',(-1.,1.92296268638356E-16,0.));
#18302=DIRECTION('center_axis',(0.866025403784439,0.5,0.));
#18303=DIRECTION('ref_axis',(-0.5,0.866025403784439,0.));
#18304=DIRECTION('',(-0.5,0.866025403784439,0.));
#18305=DIRECTION('',(0.,0.,1.));
#18306=DIRECTION('',(-0.5,0.866025403784439,0.));
#18307=DIRECTION('center_axis',(0.866025403784439,-0.5,0.));
#18308=DIRECTION('ref_axis',(0.5,0.866025403784439,0.));
#18309=DIRECTION('',(0.5,0.866025403784439,0.));
#18310=DIRECTION('',(0.5,0.866025403784439,0.));
#18311=DIRECTION('center_axis',(0.,0.,1.));
#18312=DIRECTION('ref_axis',(1.,0.,0.));
#18313=DIRECTION('center_axis',(0.,0.,1.));
#18314=DIRECTION('ref_axis',(1.,0.,0.));
#18315=DIRECTION('center_axis',(0.,0.,1.));
#18316=DIRECTION('ref_axis',(1.,0.,0.));
#18317=DIRECTION('center_axis',(0.,0.,1.));
#18318=DIRECTION('ref_axis',(1.,0.,0.));
#18319=DIRECTION('',(0.,0.,-1.));
#18320=DIRECTION('center_axis',(0.,0.,1.));
#18321=DIRECTION('ref_axis',(1.,0.,0.));
#18322=DIRECTION('center_axis',(0.,0.,1.));
#18323=DIRECTION('ref_axis',(1.,0.,0.));
#18324=DIRECTION('center_axis',(0.,0.,1.));
#18325=DIRECTION('ref_axis',(1.,0.,0.));
#18326=DIRECTION('axis',(0.,0.,1.));
#18327=DIRECTION('refdir',(1.,0.,0.));
#18328=DIRECTION('center_axis',(0.,0.,1.));
#18329=DIRECTION('ref_axis',(1.,0.,0.));
#18330=DIRECTION('center_axis',(0.,0.,-1.));
#18331=DIRECTION('ref_axis',(1.,0.,0.));
#18332=DIRECTION('',(0.,0.,-1.));
#18333=DIRECTION('center_axis',(0.,0.,-1.));
#18334=DIRECTION('ref_axis',(1.,0.,0.));
#18335=DIRECTION('center_axis',(0.,0.,1.));
#18336=DIRECTION('ref_axis',(1.,0.,0.));
#18337=DIRECTION('center_axis',(0.,0.,1.));
#18338=DIRECTION('ref_axis',(1.,0.,0.));
#18339=DIRECTION('',(0.,0.,-1.));
#18340=DIRECTION('center_axis',(0.,0.,1.));
#18341=DIRECTION('ref_axis',(1.,0.,0.));
#18342=DIRECTION('center_axis',(0.,0.,1.));
#18343=DIRECTION('ref_axis',(1.,0.,0.));
#18344=DIRECTION('center_axis',(0.,0.,1.));
#18345=DIRECTION('ref_axis',(1.,0.,0.));
#18346=DIRECTION('axis',(0.,0.,1.));
#18347=DIRECTION('refdir',(1.,0.,0.));
#18348=DIRECTION('center_axis',(0.,0.,1.));
#18349=DIRECTION('ref_axis',(1.,0.,0.));
#18350=DIRECTION('',(0.,0.,-1.));
#18351=DIRECTION('center_axis',(0.,0.,-1.));
#18352=DIRECTION('ref_axis',(1.,0.,0.));
#18353=DIRECTION('center_axis',(0.,0.,1.));
#18354=DIRECTION('ref_axis',(1.,0.,0.));
#18355=DIRECTION('',(0.,0.,-1.));
#18356=DIRECTION('center_axis',(0.,0.,1.));
#18357=DIRECTION('ref_axis',(1.,0.,0.));
#18358=DIRECTION('',(0.,0.,-1.));
#18359=DIRECTION('center_axis',(0.,0.,1.));
#18360=DIRECTION('ref_axis',(1.,0.,0.));
#18361=DIRECTION('',(0.,0.,-1.));
#18362=DIRECTION('center_axis',(0.,0.,1.));
#18363=DIRECTION('ref_axis',(1.,0.,0.));
#18364=DIRECTION('',(0.,0.,-1.));
#18365=DIRECTION('center_axis',(0.,0.,1.));
#18366=DIRECTION('ref_axis',(1.,0.,0.));
#18367=DIRECTION('',(0.,0.,-1.));
#18368=DIRECTION('center_axis',(0.,0.,1.));
#18369=DIRECTION('ref_axis',(1.,0.,0.));
#18370=DIRECTION('',(0.,0.,-1.));
#18371=DIRECTION('center_axis',(0.,0.,1.));
#18372=DIRECTION('ref_axis',(1.,0.,0.));
#18373=DIRECTION('',(0.,0.,-1.));
#18374=DIRECTION('center_axis',(0.,0.,1.));
#18375=DIRECTION('ref_axis',(1.,0.,0.));
#18376=DIRECTION('',(0.,0.,-1.));
#18377=DIRECTION('center_axis',(0.,0.,1.));
#18378=DIRECTION('ref_axis',(1.,0.,0.));
#18379=DIRECTION('',(0.,0.,-1.));
#18380=DIRECTION('center_axis',(0.,0.,1.));
#18381=DIRECTION('ref_axis',(1.,0.,0.));
#18382=DIRECTION('',(0.,0.,-1.));
#18383=DIRECTION('center_axis',(0.,0.,1.));
#18384=DIRECTION('ref_axis',(1.,0.,0.));
#18385=DIRECTION('',(0.,0.,-1.));
#18386=DIRECTION('center_axis',(0.,0.,1.));
#18387=DIRECTION('ref_axis',(1.,0.,0.));
#18388=DIRECTION('',(0.,0.,-1.));
#18389=DIRECTION('center_axis',(0.,0.,1.));
#18390=DIRECTION('ref_axis',(1.,0.,0.));
#18391=DIRECTION('',(0.,0.,-1.));
#18392=DIRECTION('center_axis',(0.,0.,1.));
#18393=DIRECTION('ref_axis',(1.,0.,0.));
#18394=DIRECTION('',(0.,0.,-1.));
#18395=DIRECTION('center_axis',(0.,0.,1.));
#18396=DIRECTION('ref_axis',(1.,0.,0.));
#18397=DIRECTION('',(0.,0.,-1.));
#18398=DIRECTION('center_axis',(0.,0.,1.));
#18399=DIRECTION('ref_axis',(1.,0.,0.));
#18400=DIRECTION('',(0.,0.,-1.));
#18401=DIRECTION('center_axis',(0.,0.,1.));
#18402=DIRECTION('ref_axis',(1.,0.,0.));
#18403=DIRECTION('',(0.,0.,-1.));
#18404=DIRECTION('center_axis',(0.,0.,1.));
#18405=DIRECTION('ref_axis',(1.,0.,0.));
#18406=DIRECTION('',(0.,0.,-1.));
#18407=DIRECTION('center_axis',(0.,0.,1.));
#18408=DIRECTION('ref_axis',(1.,0.,0.));
#18409=DIRECTION('',(0.,0.,-1.));
#18410=DIRECTION('center_axis',(0.,0.,1.));
#18411=DIRECTION('ref_axis',(1.,0.,0.));
#18412=DIRECTION('',(0.,0.,-1.));
#18413=DIRECTION('center_axis',(0.,0.,1.));
#18414=DIRECTION('ref_axis',(1.,0.,0.));
#18415=DIRECTION('',(0.,0.,-1.));
#18416=DIRECTION('center_axis',(0.,0.,1.));
#18417=DIRECTION('ref_axis',(1.,0.,0.));
#18418=DIRECTION('',(0.,0.,-1.));
#18419=DIRECTION('center_axis',(0.,0.,1.));
#18420=DIRECTION('ref_axis',(1.,0.,0.));
#18421=DIRECTION('',(0.,0.,-1.));
#18422=DIRECTION('center_axis',(0.,0.,1.));
#18423=DIRECTION('ref_axis',(1.,0.,0.));
#18424=DIRECTION('',(0.,0.,-1.));
#18425=DIRECTION('center_axis',(0.,0.,1.));
#18426=DIRECTION('ref_axis',(1.,0.,0.));
#18427=DIRECTION('',(0.,0.,-1.));
#18428=DIRECTION('center_axis',(0.,0.,1.));
#18429=DIRECTION('ref_axis',(1.,0.,0.));
#18430=DIRECTION('',(0.,0.,-1.));
#18431=DIRECTION('center_axis',(0.,0.,1.));
#18432=DIRECTION('ref_axis',(1.,0.,0.));
#18433=DIRECTION('',(0.,0.,-1.));
#18434=DIRECTION('center_axis',(0.,0.,1.));
#18435=DIRECTION('ref_axis',(1.,0.,0.));
#18436=DIRECTION('',(0.,0.,-1.));
#18437=DIRECTION('center_axis',(0.,0.,1.));
#18438=DIRECTION('ref_axis',(1.,0.,0.));
#18439=DIRECTION('',(0.,0.,-1.));
#18440=DIRECTION('center_axis',(0.,0.,1.));
#18441=DIRECTION('ref_axis',(1.,0.,0.));
#18442=DIRECTION('',(0.,0.,-1.));
#18443=DIRECTION('center_axis',(0.,0.,1.));
#18444=DIRECTION('ref_axis',(1.,0.,0.));
#18445=DIRECTION('',(0.,0.,-1.));
#18446=DIRECTION('center_axis',(0.,0.,-1.));
#18447=DIRECTION('ref_axis',(1.,0.,0.));
#18448=DIRECTION('center_axis',(0.,0.,1.));
#18449=DIRECTION('ref_axis',(1.,-2.38163665272677E-13,0.));
#18450=DIRECTION('',(0.,0.,1.));
#18451=DIRECTION('center_axis',(0.,0.,-1.));
#18452=DIRECTION('ref_axis',(1.,-2.38163665272677E-13,0.));
#18453=DIRECTION('center_axis',(0.,0.,1.));
#18454=DIRECTION('ref_axis',(1.,-2.38163665272677E-13,0.));
#18455=DIRECTION('',(0.,0.,1.));
#18456=DIRECTION('center_axis',(0.,0.,-1.));
#18457=DIRECTION('ref_axis',(1.,-2.38163665272677E-13,0.));
#18458=DIRECTION('center_axis',(0.,0.,1.));
#18459=DIRECTION('ref_axis',(1.,-2.38163665272677E-13,0.));
#18460=DIRECTION('',(0.,0.,1.));
#18461=DIRECTION('center_axis',(0.,0.,1.));
#18462=DIRECTION('ref_axis',(1.,-2.38163665272677E-13,0.));
#18463=DIRECTION('',(0.,0.,1.));
#18464=DIRECTION('center_axis',(0.,0.,1.));
#18465=DIRECTION('ref_axis',(1.,-2.38163665272677E-13,0.));
#18466=DIRECTION('',(0.,0.,1.));
#18467=DIRECTION('center_axis',(0.,0.,1.));
#18468=DIRECTION('ref_axis',(1.,-2.38163665272677E-13,0.));
#18469=DIRECTION('',(0.,0.,1.));
#18470=DIRECTION('center_axis',(0.,0.,1.));
#18471=DIRECTION('ref_axis',(1.,-2.38163665272677E-13,0.));
#18472=DIRECTION('',(0.,0.,1.));
#18473=DIRECTION('center_axis',(0.,0.,1.));
#18474=DIRECTION('ref_axis',(1.,-2.38163665272677E-13,0.));
#18475=DIRECTION('',(0.,0.,1.));
#18476=DIRECTION('center_axis',(0.,0.,1.));
#18477=DIRECTION('ref_axis',(1.,-2.38163665272677E-13,0.));
#18478=DIRECTION('',(0.,0.,1.));
#18479=DIRECTION('center_axis',(0.,0.,1.));
#18480=DIRECTION('ref_axis',(1.,-2.38163665272677E-13,0.));
#18481=DIRECTION('',(0.,0.,1.));
#18482=DIRECTION('center_axis',(0.,0.,1.));
#18483=DIRECTION('ref_axis',(1.,-2.38163665272677E-13,0.));
#18484=DIRECTION('',(0.,0.,1.));
#18485=DIRECTION('center_axis',(0.,0.,1.));
#18486=DIRECTION('ref_axis',(1.,-2.38163665272677E-13,0.));
#18487=DIRECTION('',(0.,0.,1.));
#18488=DIRECTION('center_axis',(0.,0.,1.));
#18489=DIRECTION('ref_axis',(1.,-2.38163665272677E-13,0.));
#18490=DIRECTION('',(0.,0.,1.));
#18491=DIRECTION('center_axis',(0.,0.,1.));
#18492=DIRECTION('ref_axis',(1.,-2.38163665272677E-13,0.));
#18493=DIRECTION('',(0.,0.,1.));
#18494=DIRECTION('center_axis',(0.,0.,1.));
#18495=DIRECTION('ref_axis',(1.,-2.38163665272677E-13,0.));
#18496=DIRECTION('',(0.,0.,1.));
#18497=DIRECTION('center_axis',(0.,0.,1.));
#18498=DIRECTION('ref_axis',(1.,-2.38163665272677E-13,0.));
#18499=DIRECTION('',(0.,0.,1.));
#18500=DIRECTION('center_axis',(0.,0.,1.));
#18501=DIRECTION('ref_axis',(1.,-2.38163665272677E-13,0.));
#18502=DIRECTION('',(0.,0.,1.));
#18503=DIRECTION('center_axis',(0.,0.,1.));
#18504=DIRECTION('ref_axis',(1.,-2.38163665272677E-13,0.));
#18505=DIRECTION('',(0.,0.,1.));
#18506=DIRECTION('center_axis',(0.,0.,1.));
#18507=DIRECTION('ref_axis',(1.,-2.38163665272677E-13,0.));
#18508=DIRECTION('',(0.,0.,1.));
#18509=DIRECTION('center_axis',(0.,0.,1.));
#18510=DIRECTION('ref_axis',(1.,-2.38163665272677E-13,0.));
#18511=DIRECTION('',(0.,0.,1.));
#18512=DIRECTION('center_axis',(0.,0.,1.));
#18513=DIRECTION('ref_axis',(1.,-2.38163665272677E-13,0.));
#18514=DIRECTION('',(0.,0.,1.));
#18515=DIRECTION('center_axis',(0.,0.,1.));
#18516=DIRECTION('ref_axis',(1.,-2.38163665272677E-13,0.));
#18517=DIRECTION('',(0.,0.,1.));
#18518=DIRECTION('center_axis',(0.,0.,1.));
#18519=DIRECTION('ref_axis',(1.,-2.38163665272677E-13,0.));
#18520=DIRECTION('',(0.,0.,1.));
#18521=DIRECTION('center_axis',(0.,0.,1.));
#18522=DIRECTION('ref_axis',(1.,-2.38163665272677E-13,0.));
#18523=DIRECTION('',(0.,0.,1.));
#18524=DIRECTION('center_axis',(0.,0.,1.));
#18525=DIRECTION('ref_axis',(1.,-2.38163665272677E-13,0.));
#18526=DIRECTION('',(0.,0.,1.));
#18527=DIRECTION('center_axis',(0.,0.,1.));
#18528=DIRECTION('ref_axis',(1.,-2.38163665272677E-13,0.));
#18529=DIRECTION('',(0.,0.,1.));
#18530=DIRECTION('center_axis',(0.,0.,1.));
#18531=DIRECTION('ref_axis',(1.,-2.38163665272677E-13,0.));
#18532=DIRECTION('',(0.,0.,1.));
#18533=DIRECTION('center_axis',(0.,0.,1.));
#18534=DIRECTION('ref_axis',(1.,-2.38163665272677E-13,0.));
#18535=DIRECTION('',(0.,0.,1.));
#18536=DIRECTION('center_axis',(0.,0.,1.));
#18537=DIRECTION('ref_axis',(1.,-2.38163665272677E-13,0.));
#18538=DIRECTION('',(0.,0.,1.));
#18539=DIRECTION('center_axis',(0.,0.,1.));
#18540=DIRECTION('ref_axis',(1.,-2.38163665272677E-13,0.));
#18541=DIRECTION('',(0.,0.,1.));
#18542=DIRECTION('center_axis',(0.,0.,1.));
#18543=DIRECTION('ref_axis',(1.,-2.38163665272677E-13,0.));
#18544=DIRECTION('',(0.,0.,1.));
#18545=DIRECTION('center_axis',(0.,0.,1.));
#18546=DIRECTION('ref_axis',(1.,-2.38163665272677E-13,0.));
#18547=DIRECTION('',(0.,0.,1.));
#18548=DIRECTION('center_axis',(0.,0.,-1.));
#18549=DIRECTION('ref_axis',(1.,0.,0.));
#18550=DIRECTION('',(0.707106781186547,8.65956056235493E-17,0.707106781186548));
#18551=DIRECTION('center_axis',(0.,0.,-1.));
#18552=DIRECTION('ref_axis',(1.,0.,0.));
#18553=DIRECTION('',(0.707106781186547,8.65956056235493E-17,0.707106781186548));
#18554=DIRECTION('center_axis',(0.,0.,1.));
#18555=DIRECTION('ref_axis',(1.,0.,0.));
#18556=DIRECTION('center_axis',(0.,0.,-1.));
#18557=DIRECTION('ref_axis',(-0.976187422880467,0.216928825677901,0.));
#18558=DIRECTION('center_axis',(0.,0.,1.));
#18559=DIRECTION('ref_axis',(1.,-2.38163665272677E-13,0.));
#18560=DIRECTION('center_axis',(0.,0.,-1.));
#18561=DIRECTION('ref_axis',(1.,-2.38163665272677E-13,0.));
#18562=DIRECTION('center_axis',(0.,0.,1.));
#18563=DIRECTION('ref_axis',(1.,0.,0.));
#18564=DIRECTION('center_axis',(-1.60246890531964E-16,-1.,0.));
#18565=DIRECTION('ref_axis',(1.,-1.60246890531964E-16,0.));
#18566=DIRECTION('',(1.,-1.60246890531964E-16,0.));
#18567=DIRECTION('',(0.,0.,1.));
#18568=DIRECTION('',(1.,-1.60246890531964E-16,0.));
#18569=DIRECTION('',(0.,0.,1.));
#18570=DIRECTION('center_axis',(-0.866025403784439,-0.5,0.));
#18571=DIRECTION('ref_axis',(0.5,-0.866025403784439,0.));
#18572=DIRECTION('',(0.5,-0.866025403784439,0.));
#18573=DIRECTION('',(0.,0.,1.));
#18574=DIRECTION('',(0.5,-0.866025403784439,0.));
#18575=DIRECTION('center_axis',(-0.866025403784439,0.5,0.));
#18576=DIRECTION('ref_axis',(-0.5,-0.866025403784439,0.));
#18577=DIRECTION('',(-0.5,-0.866025403784439,0.));
#18578=DIRECTION('',(0.,0.,1.));
#18579=DIRECTION('',(-0.5,-0.866025403784439,0.));
#18580=DIRECTION('center_axis',(1.60246890531964E-16,1.,0.));
#18581=DIRECTION('ref_axis',(-1.,1.60246890531964E-16,0.));
#18582=DIRECTION('',(-1.,1.60246890531964E-16,0.));
#18583=DIRECTION('',(0.,0.,1.));
#18584=DIRECTION('',(-1.,1.60246890531964E-16,0.));
#18585=DIRECTION('center_axis',(0.866025403784439,0.5,0.));
#18586=DIRECTION('ref_axis',(-0.5,0.866025403784439,0.));
#18587=DIRECTION('',(-0.5,0.866025403784439,0.));
#18588=DIRECTION('',(0.,0.,1.));
#18589=DIRECTION('',(-0.5,0.866025403784439,0.));
#18590=DIRECTION('center_axis',(0.866025403784439,-0.5,0.));
#18591=DIRECTION('ref_axis',(0.5,0.866025403784439,0.));
#18592=DIRECTION('',(0.5,0.866025403784439,0.));
#18593=DIRECTION('',(0.5,0.866025403784439,0.));
#18594=DIRECTION('center_axis',(0.,0.,1.));
#18595=DIRECTION('ref_axis',(1.,0.,0.));
#18596=DIRECTION('center_axis',(0.,0.,1.));
#18597=DIRECTION('ref_axis',(1.,0.,0.));
#18598=DIRECTION('center_axis',(0.,0.,1.));
#18599=DIRECTION('ref_axis',(1.,0.,0.));
#18600=DIRECTION('center_axis',(0.,0.,1.));
#18601=DIRECTION('ref_axis',(1.,0.,0.));
#18602=DIRECTION('',(0.,0.,-1.));
#18603=DIRECTION('center_axis',(0.,0.,1.));
#18604=DIRECTION('ref_axis',(1.,0.,0.));
#18605=DIRECTION('center_axis',(0.,0.,1.));
#18606=DIRECTION('ref_axis',(1.,0.,0.));
#18607=DIRECTION('center_axis',(0.,0.,1.));
#18608=DIRECTION('ref_axis',(1.,0.,0.));
#18609=DIRECTION('',(0.,0.,1.));
#18610=DIRECTION('',(1.,0.,0.));
#18611=DIRECTION('',(0.,0.,1.));
#18612=DIRECTION('',(1.,0.,0.));
#18613=DIRECTION('',(0.,0.,1.));
#18614=DIRECTION('',(1.,0.,0.));
#18615=DIRECTION('',(1.,0.,0.));
#18616=DIRECTION('',(0.,-0.766044443118978,-0.642787609686539));
#18617=DIRECTION('',(0.,0.,1.));
#18618=DIRECTION('',(1.,0.,0.));
#18619=DIRECTION('',(1.,0.,0.));
#18620=DIRECTION('',(0.,1.,0.));
#18621=DIRECTION('',(1.,0.,0.));
#18622=DIRECTION('',(0.,1.,0.));
#18623=DIRECTION('',(1.,0.,0.));
#18624=DIRECTION('',(0.,1.,0.));
#18625=DIRECTION('',(0.,-1.22464679914735E-16,-1.));
#18626=DIRECTION('',(1.,0.,0.));
#18627=DIRECTION('',(0.,0.,1.));
#18628=DIRECTION('',(1.,0.,0.));
#18629=DIRECTION('',(0.,-1.22464679914735E-16,-1.));
#18630=DIRECTION('',(-0.766044443118978,-0.64278760968654,7.87187788734199E-17));
#18631=DIRECTION('',(1.,0.,0.));
#18632=DIRECTION('',(0.,1.,0.));
#18633=DIRECTION('',(0.,-1.22464679914735E-16,-1.));
#18634=DIRECTION('',(1.,0.,0.));
#18635=DIRECTION('',(0.,0.,1.));
#18636=DIRECTION('',(1.,0.,0.));
#18637=DIRECTION('',(0.,0.,1.));
#18638=DIRECTION('',(2.22044604925031E-16,1.,0.));
#18639=DIRECTION('',(0.,0.,1.));
#18640=DIRECTION('',(2.22044604925031E-16,1.,0.));
#18641=DIRECTION('',(2.22044604925031E-16,1.,0.));
#18642=DIRECTION('',(0.766044443118978,-1.11022302462516E-16,-0.642787609686539));
#18643=DIRECTION('',(2.22044604925031E-16,1.,0.));
#18644=DIRECTION('',(-1.,2.22044604925031E-16,0.));
#18645=DIRECTION('',(2.22044604925031E-16,1.,0.));
#18646=DIRECTION('',(-1.,2.22044604925031E-16,0.));
#18647=DIRECTION('',(2.22044604925031E-16,1.,0.));
#18648=DIRECTION('',(-1.,2.22044604925031E-16,0.));
#18649=DIRECTION('',(2.22044604925031E-16,1.,0.));
#18650=DIRECTION('',(-1.,2.22044604925031E-16,0.));
#18651=DIRECTION('',(1.22464679914735E-16,-2.46519032881566E-32,-1.));
#18652=DIRECTION('',(1.,0.,1.22464679914735E-16));
#18653=DIRECTION('',(0.,0.,1.));
#18654=DIRECTION('',(2.22044604925031E-16,1.,0.));
#18655=DIRECTION('',(1.22464679914735E-16,-2.46519032881566E-32,-1.));
#18656=DIRECTION('',(1.,0.,1.22464679914735E-16));
#18657=DIRECTION('',(0.,0.,1.));
#18658=DIRECTION('',(2.22044604925031E-16,1.,0.));
#18659=DIRECTION('',(0.,0.,1.));
#18660=DIRECTION('',(-1.,1.22464679914735E-16,0.));
#18661=DIRECTION('',(0.,0.,1.));
#18662=DIRECTION('',(-1.,1.22464679914735E-16,0.));
#18663=DIRECTION('',(-1.,1.22464679914735E-16,0.));
#18664=DIRECTION('',(9.38133875270273E-17,0.766044443118978,-0.642787609686539));
#18665=DIRECTION('',(-1.,1.22464679914735E-16,0.));
#18666=DIRECTION('',(-1.22464679914735E-16,-1.,0.));
#18667=DIRECTION('',(-1.,1.22464679914735E-16,0.));
#18668=DIRECTION('',(-1.22464679914735E-16,-1.,0.));
#18669=DIRECTION('',(-1.,1.22464679914735E-16,0.));
#18670=DIRECTION('',(-1.22464679914735E-16,-1.,0.));
#18671=DIRECTION('',(-1.,1.22464679914735E-16,0.));
#18672=DIRECTION('',(-1.22464679914735E-16,-1.,0.));
#18673=DIRECTION('',(1.49975978266186E-32,1.22464679914735E-16,-1.));
#18674=DIRECTION('',(1.,0.,1.49975978266186E-32));
#18675=DIRECTION('',(0.,0.,1.));
#18676=DIRECTION('',(-1.,1.22464679914735E-16,0.));
#18677=DIRECTION('',(1.49975978266186E-32,1.22464679914735E-16,-1.));
#18678=DIRECTION('',(1.,0.,1.49975978266186E-32));
#18679=DIRECTION('',(0.,0.,1.));
#18680=DIRECTION('',(-1.,1.22464679914735E-16,0.));
#18681=DIRECTION('',(0.,0.,1.));
#18682=DIRECTION('',(-2.22044604925031E-16,-1.,0.));
#18683=DIRECTION('',(0.,0.,1.));
#18684=DIRECTION('',(-2.22044604925031E-16,-1.,0.));
#18685=DIRECTION('',(-2.22044604925031E-16,-1.,0.));
#18686=DIRECTION('',(-0.766044443118978,1.66533453693773E-16,-0.642787609686539));
#18687=DIRECTION('',(-2.22044604925031E-16,-1.,0.));
#18688=DIRECTION('',(1.,-2.22044604925031E-16,0.));
#18689=DIRECTION('',(-2.22044604925031E-16,-1.,0.));
#18690=DIRECTION('',(1.,-2.22044604925031E-16,0.));
#18691=DIRECTION('',(-2.22044604925031E-16,-1.,0.));
#18692=DIRECTION('',(1.,-2.22044604925031E-16,0.));
#18693=DIRECTION('',(-2.22044604925031E-16,-1.,0.));
#18694=DIRECTION('',(1.,-2.22044604925031E-16,0.));
#18695=DIRECTION('',(-1.22464679914735E-16,2.46519032881566E-32,-1.));
#18696=DIRECTION('',(1.,0.,-1.22464679914735E-16));
#18697=DIRECTION('',(0.,0.,1.));
#18698=DIRECTION('',(-2.22044604925031E-16,-1.,0.));
#18699=DIRECTION('',(-1.22464679914735E-16,2.46519032881566E-32,-1.));
#18700=DIRECTION('',(1.,0.,-1.22464679914735E-16));
#18701=DIRECTION('',(0.,0.,1.));
#18702=DIRECTION('',(-2.22044604925031E-16,-1.,0.));
#18703=DIRECTION('',(0.,-1.22464679914735E-16,-1.));
#18704=DIRECTION('',(-0.766044443118978,-0.64278760968654,7.87187788734199E-17));
#18705=DIRECTION('',(0.,-1.22464679914735E-16,-1.));
#18706=DIRECTION('',(-0.766044443118978,-0.64278760968654,7.87187788734199E-17));
#18707=DIRECTION('',(0.,-1.22464679914735E-16,-1.));
#18708=DIRECTION('',(-0.766044443118978,-0.64278760968654,7.87187788734199E-17));
#18709=CARTESIAN_POINT('',(0.,0.,0.));
#18710=CARTESIAN_POINT('',(0.,0.,0.));
#18711=CARTESIAN_POINT('Origin',(-92.,-24.,5.));
#18712=CARTESIAN_POINT('',(-94.5134954281454,-23.9997257032743,1.38741669750802));
#18713=CARTESIAN_POINT('',(-94.5156258041287,-24.0035321038279,1.11258330249198));
#18714=CARTESIAN_POINT('',(-94.5175,-24.,5.));
#18715=CARTESIAN_POINT('',(-93.913465996665,-22.364012796625,0.999999999999999));
#18716=CARTESIAN_POINT('Ctrl Pts',(-94.5156258041287,-24.0035321038279,
1.11258330249198));
#18717=CARTESIAN_POINT('Ctrl Pts',(-94.5104632893492,-23.410913677985,1.07505553499465));
#18718=CARTESIAN_POINT('Ctrl Pts',(-94.299221828084,-22.8151964396956,1.03752776749732));
#18719=CARTESIAN_POINT('Ctrl Pts',(-93.913465996665,-22.364012796625,0.999999999999996));
#18720=CARTESIAN_POINT('',(-94.5175,-24.,1.));
#18721=CARTESIAN_POINT('Origin',(-92.,-24.,1.));
#18722=CARTESIAN_POINT('',(-94.5175,-24.,0.));
#18723=CARTESIAN_POINT('',(-94.5175,-24.,5.));
#18724=CARTESIAN_POINT('Origin',(-92.,-24.,0.));
#18725=CARTESIAN_POINT('',(-90.0828967253639,-22.3614656719992,1.));
#18726=CARTESIAN_POINT('Origin',(-92.,-24.,1.));
#18727=CARTESIAN_POINT('Ctrl Pts',(-90.0828882653787,-22.3614597476137,
1.));
#18728=CARTESIAN_POINT('Ctrl Pts',(-90.6060429859409,-21.7523041107177,
1.05098091535882));
#18729=CARTESIAN_POINT('Ctrl Pts',(-91.4465812877835,-21.4121723295192,
1.10196183071765));
#18730=CARTESIAN_POINT('Ctrl Pts',(-92.2457357736239,-21.49051470028,1.15294274607647));
#18731=CARTESIAN_POINT('Ctrl Pts',(-93.0712273934265,-21.5714389416932,
1.20560380115935));
#18732=CARTESIAN_POINT('Ctrl Pts',(-93.8525625390091,-22.0988745222663,
1.25826485624223));
#18733=CARTESIAN_POINT('Ctrl Pts',(-94.2358880111547,-22.8341462678707,
1.31092591132511));
#18734=CARTESIAN_POINT('Ctrl Pts',(-94.4214828919903,-23.1901431476069,
1.33642284005274));
#18735=CARTESIAN_POINT('Ctrl Pts',(-94.5137759227878,-23.5948612017176,
1.36191976878038));
#18736=CARTESIAN_POINT('Ctrl Pts',(-94.5134954281454,-23.9997257032743,
1.38741669750802));
#18737=CARTESIAN_POINT('Origin',(-92.,-24.,5.));
#18738=CARTESIAN_POINT('',(-94.5187355654992,-24.0021096152222,2.38741669750802));
#18739=CARTESIAN_POINT('',(-94.5214126870217,-23.9993544610189,2.11258330249198));
#18740=CARTESIAN_POINT('',(-94.5175,-24.,5.));
#18741=CARTESIAN_POINT('Ctrl Pts',(-94.5214126870217,-23.9993544610189,
2.11258330249198));
#18742=CARTESIAN_POINT('Ctrl Pts',(-94.5215323520691,-23.9641713906795,
2.11034958724147));
#18743=CARTESIAN_POINT('Ctrl Pts',(-94.5208590695048,-23.9289930573579,
2.10811587199095));
#18744=CARTESIAN_POINT('Ctrl Pts',(-94.5193785186672,-23.8938487960073,
2.10588215674044));
#18745=CARTESIAN_POINT('Ctrl Pts',(-94.4844737253228,-23.0653036703884,
2.05322110165756));
#18746=CARTESIAN_POINT('Ctrl Pts',(-94.0008841105951,-22.25569596213,2.00056004657469));
#18747=CARTESIAN_POINT('Ctrl Pts',(-93.2879127216155,-21.8321129915859,
1.94789899149181));
#18748=CARTESIAN_POINT('Ctrl Pts',(-92.5749413326359,-21.4085300210418,
1.89523793640893));
#18749=CARTESIAN_POINT('Ctrl Pts',(-91.6325881694045,-21.3709717882121,
1.84257688132605));
#18750=CARTESIAN_POINT('Ctrl Pts',(-90.8882532181424,-21.7366423255222,
1.78991582624317));
#18751=CARTESIAN_POINT('Ctrl Pts',(-90.1439182668804,-22.1023128628323,
1.73725477116029));
#18752=CARTESIAN_POINT('Ctrl Pts',(-89.5976015275876,-22.8712121702823,
1.68459371607741));
#18753=CARTESIAN_POINT('Ctrl Pts',(-89.4970123488694,-23.6942825335227,
1.63193266099454));
#18754=CARTESIAN_POINT('Ctrl Pts',(-89.3964231701512,-24.5173528967631,
1.57927160591166));
#18755=CARTESIAN_POINT('Ctrl Pts',(-89.7415615520075,-25.3945943157939,
1.52661055082878));
#18756=CARTESIAN_POINT('Ctrl Pts',(-90.3760119861909,-25.9288768514157,
1.4739494957459));
#18757=CARTESIAN_POINT('Ctrl Pts',(-91.0104624203743,-26.4631593870376,
1.42128844066303));
#18758=CARTESIAN_POINT('Ctrl Pts',(-91.9342249068849,-26.6544830392504,
1.36862738558015));
#18759=CARTESIAN_POINT('Ctrl Pts',(-92.7281293260075,-26.4146105531457,
1.31596633049727));
#18760=CARTESIAN_POINT('Ctrl Pts',(-93.52203374513,-26.1747380670411,1.26330527541439));
#18761=CARTESIAN_POINT('Ctrl Pts',(-94.1860800968645,-25.503669442619,1.21064422033151));
#18762=CARTESIAN_POINT('Ctrl Pts',(-94.4192666807451,-24.7092696340464,
1.15798316524863));
#18763=CARTESIAN_POINT('Ctrl Pts',(-94.4862778644254,-24.4809817514334,
1.14284987766308));
#18764=CARTESIAN_POINT('Ctrl Pts',(-94.5177076178372,-24.2425088846187,
1.12771659007753));
#18765=CARTESIAN_POINT('Ctrl Pts',(-94.5156258041287,-24.0035321038279,
1.11258330249198));
#18766=CARTESIAN_POINT('Ctrl Pts',(-94.5134954281454,-23.9997257032743,
1.38741669750802));
#18767=CARTESIAN_POINT('Ctrl Pts',(-94.5131965924704,-24.4310635555512,
1.41458082386326));
#18768=CARTESIAN_POINT('Ctrl Pts',(-94.4078219950606,-24.8625676332891,
1.4417449502185));
#18769=CARTESIAN_POINT('Ctrl Pts',(-94.1982523776868,-25.2354979308672,
1.46890907657374));
#18770=CARTESIAN_POINT('Ctrl Pts',(-93.7919754733646,-25.9584699376238,
1.52157013165662));
#18771=CARTESIAN_POINT('Ctrl Pts',(-92.9941058660117,-26.4613060405014,
1.5742311867395));
#18772=CARTESIAN_POINT('Ctrl Pts',(-92.1666097958722,-26.5160870716528,
1.62689224182237));
#18773=CARTESIAN_POINT('Ctrl Pts',(-91.3391137257328,-26.5708681028041,
1.67955329690525));
#18774=CARTESIAN_POINT('Ctrl Pts',(-90.4819911928069,-26.1775940622292,
1.73221435198813));
#18775=CARTESIAN_POINT('Ctrl Pts',(-89.9839037459974,-25.5145599501885,
1.78487540707101));
#18776=CARTESIAN_POINT('Ctrl Pts',(-89.4858162991878,-24.8515258381478,
1.83753646215389));
#18777=CARTESIAN_POINT('Ctrl Pts',(-89.3467639384946,-23.9187316546413,
1.89019751723676));
#18778=CARTESIAN_POINT('Ctrl Pts',(-89.6298377538243,-23.1392455882325,
1.94285857231964));
#18779=CARTESIAN_POINT('Ctrl Pts',(-89.9129115691541,-22.3597595218238,
1.99551962740252));
#18780=CARTESIAN_POINT('Ctrl Pts',(-90.6181115605066,-21.7335815725127,
2.0481806824854));
#18781=CARTESIAN_POINT('Ctrl Pts',(-91.425603556166,-21.5446793850464,2.10084173756828));
#18782=CARTESIAN_POINT('Ctrl Pts',(-92.2330955518254,-21.35577719758,2.15350279265115));
#18783=CARTESIAN_POINT('Ctrl Pts',(-93.1428795517915,-21.6041507719583,
2.20616384773403));
#18784=CARTESIAN_POINT('Ctrl Pts',(-93.7423598115282,-22.1771656715372,
2.25882490281691));
#18785=CARTESIAN_POINT('Ctrl Pts',(-94.2303120712523,-22.6435762172788,
2.30168883438062));
#18786=CARTESIAN_POINT('Ctrl Pts',(-94.5126791039229,-23.3250710559231,
2.34455276594432));
#18787=CARTESIAN_POINT('Ctrl Pts',(-94.5187355654992,-24.0021096152222,
2.38741669750802));
#18788=CARTESIAN_POINT('Origin',(-92.,-24.,5.));
#18789=CARTESIAN_POINT('',(-94.5197285159004,-23.9981710495135,3.38741669750802));
#18790=CARTESIAN_POINT('',(-94.5145914825341,-23.9984414286209,3.11258330249198));
#18791=CARTESIAN_POINT('',(-94.5175,-24.,5.));
#18792=CARTESIAN_POINT('Ctrl Pts',(-94.5145914825341,-23.9984414286209,
3.11258330249198));
#18793=CARTESIAN_POINT('Ctrl Pts',(-94.5163706169191,-23.687546359978,3.0929825844054));
#18794=CARTESIAN_POINT('Ctrl Pts',(-94.4629229514308,-23.3772412892129,
3.07338186631883));
#18795=CARTESIAN_POINT('Ctrl Pts',(-94.3514583308843,-23.0894032152641,
3.05378114823225));
#18796=CARTESIAN_POINT('Ctrl Pts',(-94.0519874392331,-22.3160715138328,
3.00112009314937));
#18797=CARTESIAN_POINT('Ctrl Pts',(-93.3337325490401,-21.7049134175565,
2.94845903806649));
#18798=CARTESIAN_POINT('Ctrl Pts',(-92.52243433036,-21.5330984014484,2.89579798298361));
#18799=CARTESIAN_POINT('Ctrl Pts',(-91.7111361116799,-21.3612833853403,
2.84313692790073));
#18800=CARTESIAN_POINT('Ctrl Pts',(-90.8067945645125,-21.6288114494004,
2.79047587281786));
#18801=CARTESIAN_POINT('Ctrl Pts',(-90.219544382578,-22.2143564031656,2.73781481773498));
#18802=CARTESIAN_POINT('Ctrl Pts',(-89.6322942006435,-22.7999013569308,
2.6851537626521));
#18803=CARTESIAN_POINT('Ctrl Pts',(-89.3621353839418,-23.703463200401,2.63249270756922));
#18804=CARTESIAN_POINT('Ctrl Pts',(-89.5315888137356,-24.515256413142,2.57983165248635));
#18805=CARTESIAN_POINT('Ctrl Pts',(-89.7010422435293,-25.3270496258829,
2.52717059740347));
#18806=CARTESIAN_POINT('Ctrl Pts',(-90.3101079198185,-26.0470742078947,
2.47450954232059));
#18807=CARTESIAN_POINT('Ctrl Pts',(-91.0825657012674,-26.3487965351803,
2.42184848723771));
#18808=CARTESIAN_POINT('Ctrl Pts',(-91.8550234827163,-26.6505188624658,
2.36918743215483));
#18809=CARTESIAN_POINT('Ctrl Pts',(-92.7908733693248,-26.5339389350252,
2.31652637707195));
#18810=CARTESIAN_POINT('Ctrl Pts',(-93.4656883266487,-26.0519076998153,
2.26386532198908));
#18811=CARTESIAN_POINT('Ctrl Pts',(-94.1118797697061,-25.5903227036642,
2.21343798215671));
#18812=CARTESIAN_POINT('Ctrl Pts',(-94.5187111833227,-24.7936314593702,
2.16301064232435));
#18813=CARTESIAN_POINT('Ctrl Pts',(-94.5214126870217,-23.9993544610189,
2.11258330249198));
#18814=CARTESIAN_POINT('Ctrl Pts',(-94.5187355654992,-24.0021096152222,
2.38741669750802));
#18815=CARTESIAN_POINT('Ctrl Pts',(-94.5201198506077,-24.1568558120997,
2.3972138210272));
#18816=CARTESIAN_POINT('Ctrl Pts',(-94.5070693393431,-24.3113692075874,
2.40701094454637));
#18817=CARTESIAN_POINT('Ctrl Pts',(-94.4787395411231,-24.4630283942082,
2.41680806806555));
#18818=CARTESIAN_POINT('Ctrl Pts',(-94.3264624914741,-25.2782199925207,
2.46946912314842));
#18819=CARTESIAN_POINT('Ctrl Pts',(-93.7327318726689,-26.0109469643662,
2.5221301782313));
#18820=CARTESIAN_POINT('Ctrl Pts',(-92.9668162894688,-26.3289068537565,
2.57479123331418));
#18821=CARTESIAN_POINT('Ctrl Pts',(-92.2009007062687,-26.6468667431468,
2.62745228839706));
#18822=CARTESIAN_POINT('Ctrl Pts',(-91.2628001586737,-26.5500595500819,
2.68011334347994));
#18823=CARTESIAN_POINT('Ctrl Pts',(-90.5779584534227,-26.0823881414071,
2.73277439856282));
#18824=CARTESIAN_POINT('Ctrl Pts',(-89.8931167481717,-25.6147167327323,
2.78543545364569));
#18825=CARTESIAN_POINT('Ctrl Pts',(-89.4615338852647,-24.7761811084476,
2.83809650872857));
#18826=CARTESIAN_POINT('Ctrl Pts',(-89.4789404507956,-23.9470718995605,
2.89075756381145));
#18827=CARTESIAN_POINT('Ctrl Pts',(-89.4963470163265,-23.1179626906734,
2.94341861889433));
#18828=CARTESIAN_POINT('Ctrl Pts',(-89.9627430102955,-22.2982798971839,
2.99607967397721));
#18829=CARTESIAN_POINT('Ctrl Pts',(-90.6666096977841,-21.8597634515608,
3.04874072906008));
#18830=CARTESIAN_POINT('Ctrl Pts',(-91.3704763852727,-21.4212470059377,
3.10140178414296));
#18831=CARTESIAN_POINT('Ctrl Pts',(-92.311813766281,-21.363896908181,3.15406283922584));
#18832=CARTESIAN_POINT('Ctrl Pts',(-93.0637093676529,-21.7137225058316,
3.20672389430872));
#18833=CARTESIAN_POINT('Ctrl Pts',(-93.8156049690249,-22.0635481034822,
3.2593849493916));
#18834=CARTESIAN_POINT('Ctrl Pts',(-94.3780587907605,-22.8205493965401,
3.31204600447447));
#18835=CARTESIAN_POINT('Ctrl Pts',(-94.4959883797686,-23.641413330862,3.36470705955735));
#18836=CARTESIAN_POINT('Ctrl Pts',(-94.5129404282089,-23.7594102245555,
3.37227693887424));
#18837=CARTESIAN_POINT('Ctrl Pts',(-94.5207071577179,-23.8787267284854,
3.37984681819113));
#18838=CARTESIAN_POINT('Ctrl Pts',(-94.5197285159004,-23.9981710495135,
3.38741669750802));
#18839=CARTESIAN_POINT('Origin',(-92.,-24.,5.));
#18840=CARTESIAN_POINT('',(-94.5135839828142,-23.9996457834291,4.38741669750802));
#18841=CARTESIAN_POINT('',(-94.51602550603,-24.0021063693209,4.11258330249198));
#18842=CARTESIAN_POINT('',(-94.5175,-24.,5.));
#18843=CARTESIAN_POINT('Ctrl Pts',(-94.51602550603,-24.0021063693209,4.11258330249198));
#18844=CARTESIAN_POINT('Ctrl Pts',(-94.5113088734142,-23.4165891850021,
4.07561558156934));
#18845=CARTESIAN_POINT('Ctrl Pts',(-94.30740600999,-22.828109419245,4.0386478606467));
#18846=CARTESIAN_POINT('Ctrl Pts',(-93.9337853550358,-22.381662326268,4.00168013972405));
#18847=CARTESIAN_POINT('Ctrl Pts',(-93.4015573085243,-21.7456919616342,
3.94901908464117));
#18848=CARTESIAN_POINT('Ctrl Pts',(-92.5249308580447,-21.3979402061153,
3.8963580295583));
#18849=CARTESIAN_POINT('Ctrl Pts',(-91.7014710569733,-21.4961183997274,
3.84369697447542));
#18850=CARTESIAN_POINT('Ctrl Pts',(-90.8780112559018,-21.5942965933395,
3.79103591939254));
#18851=CARTESIAN_POINT('Ctrl Pts',(-90.1077181042387,-22.1384047360825,
3.73837486430966));
#18852=CARTESIAN_POINT('Ctrl Pts',(-89.7399326972187,-22.8816805318428,
3.68571380922678));
#18853=CARTESIAN_POINT('Ctrl Pts',(-89.3721472901988,-23.624956327603,3.63305275414391));
#18854=CARTESIAN_POINT('Ctrl Pts',(-89.406869627822,-24.5673997763804,3.58039169906103));
#18855=CARTESIAN_POINT('Ctrl Pts',(-89.8283525270324,-25.2815966241557,
3.52773064397815));
#18856=CARTESIAN_POINT('Ctrl Pts',(-90.2498354262427,-25.9957934719311,
3.47506958889527));
#18857=CARTESIAN_POINT('Ctrl Pts',(-91.0580788870401,-26.4817437187043,
3.42240853381239));
#18858=CARTESIAN_POINT('Ctrl Pts',(-91.8865307275916,-26.5190607694894,
3.36974747872952));
#18859=CARTESIAN_POINT('Ctrl Pts',(-92.7149825681431,-26.5563778202744,
3.31708642364664));
#18860=CARTESIAN_POINT('Ctrl Pts',(-93.5636427884488,-26.1450616750713,
3.26442536856376));
#18861=CARTESIAN_POINT('Ctrl Pts',(-94.0476294520469,-25.4716509491765,
3.21176431348088));
#18862=CARTESIAN_POINT('Ctrl Pts',(-94.3514737668842,-25.0488871914059,
3.17870397648458));
#18863=CARTESIAN_POINT('Ctrl Pts',(-94.5115906341944,-24.5228250606093,
3.14564363948828));
#18864=CARTESIAN_POINT('Ctrl Pts',(-94.5145914825341,-23.9984414286209,
3.11258330249198));
#18865=CARTESIAN_POINT('Ctrl Pts',(-94.5197285159004,-23.9981710495135,
3.38741669750802));
#18866=CARTESIAN_POINT('Ctrl Pts',(-94.5138990821199,-24.7096599185249,
3.43250787327401));
#18867=CARTESIAN_POINT('Ctrl Pts',(-94.1977684432012,-25.4256839637041,
3.47759904904));
#18868=CARTESIAN_POINT('Ctrl Pts',(-93.664320715776,-25.8943544806311,3.52269022480599));
#18869=CARTESIAN_POINT('Ctrl Pts',(-93.0413181064947,-26.4417051204924,
3.57535127988887));
#18870=CARTESIAN_POINT('Ctrl Pts',(-92.1219075316514,-26.6516798246292,
3.62801233497174));
#18871=CARTESIAN_POINT('Ctrl Pts',(-91.3230573666226,-26.4290514695956,
3.68067339005462));
#18872=CARTESIAN_POINT('Ctrl Pts',(-90.5242072015938,-26.206423114562,3.7333344451375));
#18873=CARTESIAN_POINT('Ctrl Pts',(-89.8459174463795,-25.5511917003581,
3.78599550022038));
#18874=CARTESIAN_POINT('Ctrl Pts',(-89.5958040861176,-24.7605158612689,
3.83865655530326));
#18875=CARTESIAN_POINT('Ctrl Pts',(-89.3456907258557,-23.9698400221797,
3.89131761038613));
#18876=CARTESIAN_POINT('Ctrl Pts',(-89.5237537605462,-23.0437197582053,
3.94397866546901));
#18877=CARTESIAN_POINT('Ctrl Pts',(-90.0492385624731,-22.4021664114935,
3.99663972055189));
#18878=CARTESIAN_POINT('Ctrl Pts',(-90.5747233644,-21.7606130647817,4.04930077563477));
#18879=CARTESIAN_POINT('Ctrl Pts',(-91.4476299335634,-21.4036266353327,
4.10196183071765));
#18880=CARTESIAN_POINT('Ctrl Pts',(-92.2720802450577,-21.4931065626282,
4.15462288580053));
#18881=CARTESIAN_POINT('Ctrl Pts',(-93.096530556552,-21.5825864899238,4.2072839408834));
#18882=CARTESIAN_POINT('Ctrl Pts',(-93.8725246103771,-22.1185327739639,
4.25994499596628));
#18883=CARTESIAN_POINT('Ctrl Pts',(-94.2481358593184,-22.8578846277675,
4.31260605104916));
#18884=CARTESIAN_POINT('Ctrl Pts',(-94.4260011420294,-23.2079940211105,
4.33754293320211));
#18885=CARTESIAN_POINT('Ctrl Pts',(-94.5140862159014,-23.6037142506574,
4.36247981535507));
#18886=CARTESIAN_POINT('Ctrl Pts',(-94.5135839828142,-23.9996457834291,
4.38741669750802));
#18887=CARTESIAN_POINT('Origin',(-92.,-24.,5.));
#18888=CARTESIAN_POINT('',(-94.5184743499735,-24.0021560918536,5.38741669750802));
#18889=CARTESIAN_POINT('',(-94.5215003759084,-23.999522240299,5.11258330249198));
#18890=CARTESIAN_POINT('',(-94.5175,-24.,5.));
#18891=CARTESIAN_POINT('Ctrl Pts',(-94.5215003759084,-23.999522240299,5.11258330249198));
#18892=CARTESIAN_POINT('Ctrl Pts',(-94.5215696550139,-23.9731625365728,
5.11090963381615));
#18893=CARTESIAN_POINT('Ctrl Pts',(-94.5211916947533,-23.9468048672736,
5.10923596514032));
#18894=CARTESIAN_POINT('Ctrl Pts',(-94.5203603409136,-23.9204615063421,
5.10756229646449));
#18895=CARTESIAN_POINT('Ctrl Pts',(-94.4942022542029,-23.0915822896134,
5.05490124138162));
#18896=CARTESIAN_POINT('Ctrl Pts',(-94.0191794168034,-22.2768685179764,
5.00224018629874));
#18897=CARTESIAN_POINT('Ctrl Pts',(-93.3107227922662,-21.8458067909395,
4.94957913121586));
#18898=CARTESIAN_POINT('Ctrl Pts',(-92.602266167729,-21.4147450639025,4.89691807613299));
#18899=CARTESIAN_POINT('Ctrl Pts',(-91.660375756054,-21.3673353814657,4.84425702105011));
#18900=CARTESIAN_POINT('Ctrl Pts',(-90.9122149332711,-21.7250788434924,
4.79159596596723));
#18901=CARTESIAN_POINT('Ctrl Pts',(-90.1640541104882,-22.0828223055191,
4.73893491088435));
#18902=CARTESIAN_POINT('Ctrl Pts',(-89.6096228765974,-22.8457189120093,
4.68627385580147));
#18903=CARTESIAN_POINT('Ctrl Pts',(-89.5003652582015,-23.667782032718,4.63361280071859));
#18904=CARTESIAN_POINT('Ctrl Pts',(-89.3911076398056,-24.4898451534267,
4.58095174563571));
#18905=CARTESIAN_POINT('Ctrl Pts',(-89.7270236369045,-25.3710747883538,
4.52829069055284));
#18906=CARTESIAN_POINT('Ctrl Pts',(-90.3557696119043,-25.9118182580198,
4.47562963546996));
#18907=CARTESIAN_POINT('Ctrl Pts',(-90.9845155869042,-26.4525617276857,
4.42296858038708));
#18908=CARTESIAN_POINT('Ctrl Pts',(-91.906091539805,-26.6528190320905,4.3703075253042));
#18909=CARTESIAN_POINT('Ctrl Pts',(-92.7025470485768,-26.4217700679435,
4.31764647022132));
#18910=CARTESIAN_POINT('Ctrl Pts',(-93.4990025573485,-26.1907211037965,
4.26498541513844));
#18911=CARTESIAN_POINT('Ctrl Pts',(-94.1703376219912,-25.5283658710978,
4.21232436005557));
#18912=CARTESIAN_POINT('Ctrl Pts',(-94.4120903330409,-24.7350937678741,
4.15966330497269));
#18913=CARTESIAN_POINT('Ctrl Pts',(-94.4841342006139,-24.4986935632772,
4.14396997081245));
#18914=CARTESIAN_POINT('Ctrl Pts',(-94.5180277850427,-24.250666913513,4.12827663665222));
#18915=CARTESIAN_POINT('Ctrl Pts',(-94.51602550603,-24.0021063693209,4.11258330249198));
#18916=CARTESIAN_POINT('Ctrl Pts',(-94.5135839828142,-23.9996457834291,
4.38741669750802));
#18917=CARTESIAN_POINT('Ctrl Pts',(-94.5130256132123,-24.4398320992502,
4.41514087043795));
#18918=CARTESIAN_POINT('Ctrl Pts',(-94.4029696961734,-24.8802795945301,
4.44286504336787));
#18919=CARTESIAN_POINT('Ctrl Pts',(-94.185055515175,-25.2586003180437,4.47058921629779));
#18920=CARTESIAN_POINT('Ctrl Pts',(-93.7711354780326,-25.9772067309494,
4.52325027138067));
#18921=CARTESIAN_POINT('Ctrl Pts',(-92.9680669596902,-26.4716621331935,
4.57591132646355));
#18922=CARTESIAN_POINT('Ctrl Pts',(-92.140055238289,-26.5177225612861,4.62857238154643));
#18923=CARTESIAN_POINT('Ctrl Pts',(-91.3120435168878,-26.5637829893786,
4.68123343662931));
#18924=CARTESIAN_POINT('Ctrl Pts',(-90.4590885924279,-26.1614484433196,
4.73389449171219));
#18925=CARTESIAN_POINT('Ctrl Pts',(-89.9680200798161,-25.493184506096,4.78655554679507));
#18926=CARTESIAN_POINT('Ctrl Pts',(-89.4769515672043,-24.8249205688725,
4.83921660187794));
#18927=CARTESIAN_POINT('Ctrl Pts',(-89.3477694664407,-23.8907272404844,
4.89187765696082));
#18928=CARTESIAN_POINT('Ctrl Pts',(-89.6390600648162,-23.1142771383271,
4.9445387120437));
#18929=CARTESIAN_POINT('Ctrl Pts',(-89.9303506631918,-22.3378270361698,
4.99719976712657));
#18930=CARTESIAN_POINT('Ctrl Pts',(-90.6421139607066,-21.7191201602431,
5.04986082220945));
#18931=CARTESIAN_POINT('Ctrl Pts',(-91.4515531549517,-21.5387506376962,
5.10252187729233));
#18932=CARTESIAN_POINT('Ctrl Pts',(-92.2609923491968,-21.3583811151493,
5.15518293237521));
#18933=CARTESIAN_POINT('Ctrl Pts',(-93.1681074401722,-21.6163489459821,
5.20784398745809));
#18934=CARTESIAN_POINT('Ctrl Pts',(-93.7615062532209,-22.1956613164021,
5.26050504254097));
#18935=CARTESIAN_POINT('Ctrl Pts',(-94.2381977114593,-22.6610367983859,
5.30280892752999));
#18936=CARTESIAN_POINT('Ctrl Pts',(-94.5124388592754,-23.3337853316565,
5.34511281251901));
#18937=CARTESIAN_POINT('Ctrl Pts',(-94.5184743499735,-24.0021560918536,
5.38741669750802));
#18938=CARTESIAN_POINT('Origin',(-92.,-24.,5.));
#18939=CARTESIAN_POINT('',(-94.5199606688991,-23.9982645762516,6.38741669750803));
#18940=CARTESIAN_POINT('',(-94.5147663248015,-23.9983410423439,6.11258330249198));
#18941=CARTESIAN_POINT('',(-94.5175,-24.,5.));
#18942=CARTESIAN_POINT('Ctrl Pts',(-94.5147663248015,-23.9983410423439,
6.11258330249198));
#18943=CARTESIAN_POINT('Ctrl Pts',(-94.5166143414574,-23.6963819206475,
6.09354263098009));
#18944=CARTESIAN_POINT('Ctrl Pts',(-94.4662620027174,-23.3950183934936,
6.0745019594682));
#18945=CARTESIAN_POINT('Ctrl Pts',(-94.3609399824778,-23.1142771205844,
6.0554612879563));
#18946=CARTESIAN_POINT('Ctrl Pts',(-94.0696493782671,-22.3378270028733,
6.00280023287342));
#18947=CARTESIAN_POINT('Ctrl Pts',(-93.3578860664944,-21.7191201145527,
5.95013917779055));
#18948=CARTESIAN_POINT('Ctrl Pts',(-92.5484468560347,-21.5387505883927,
5.89747812270767));
#18949=CARTESIAN_POINT('Ctrl Pts',(-91.739007645575,-21.3583810622326,5.84481706762479));
#18950=CARTESIAN_POINT('Ctrl Pts',(-90.8318925364285,-21.616348898233,5.79215601254191));
#18951=CARTESIAN_POINT('Ctrl Pts',(-90.2384937114928,-22.1956612802578,
5.73949495745903));
#18952=CARTESIAN_POINT('Ctrl Pts',(-89.6450948865571,-22.7749736622827,
5.68683390237615));
#18953=CARTESIAN_POINT('Ctrl Pts',(-89.3654123458324,-23.6756305903319,
5.63417284729328));
#18954=CARTESIAN_POINT('Ctrl Pts',(-89.5262868946163,-24.4891687768701,
5.5815117922104));
#18955=CARTESIAN_POINT('Ctrl Pts',(-89.6871614434003,-25.3027069634083,
5.52885073712752));
#18956=CARTESIAN_POINT('Ctrl Pts',(-90.2885930816928,-26.0291264084354,
5.47618968204464));
#18957=CARTESIAN_POINT('Ctrl Pts',(-91.0578222974529,-26.3389834964905,
5.42352862696176));
#18958=CARTESIAN_POINT('Ctrl Pts',(-91.8270515132129,-26.6488405845455,
5.37086757187889));
#18959=CARTESIAN_POINT('Ctrl Pts',(-92.7640783064405,-26.5421353156285,
5.31820651679601));
#18960=CARTESIAN_POINT('Ctrl Pts',(-93.4439450350434,-26.0672603502598,
5.26554546171313));
#18961=CARTESIAN_POINT('Ctrl Pts',(-94.1022043035296,-25.6074778161617,
5.21455807530608));
#18962=CARTESIAN_POINT('Ctrl Pts',(-94.5193898264468,-24.8025559702574,
5.16357068889903));
#18963=CARTESIAN_POINT('Ctrl Pts',(-94.5215003759084,-23.999522240299,5.11258330249198));
#18964=CARTESIAN_POINT('Ctrl Pts',(-94.5184743499735,-24.0021560918536,
5.38741669750802));
#18965=CARTESIAN_POINT('Ctrl Pts',(-94.5199520063111,-24.1657918820634,
5.39777386760188));
#18966=CARTESIAN_POINT('Ctrl Pts',(-94.5053532314692,-24.3291652655504,
5.40813103769574));
#18967=CARTESIAN_POINT('Ctrl Pts',(-94.4737130558303,-24.4891687670711,
5.4184882077896));
#18968=CARTESIAN_POINT('Ctrl Pts',(-94.3128385102691,-25.3027069373126,
5.47114926287248));
#18969=CARTESIAN_POINT('Ctrl Pts',(-93.7114068840245,-26.0291263677881,
5.52381031795536));
#18970=CARTESIAN_POINT('Ctrl Pts',(-92.9421776836735,-26.3389834496362,
5.57647137303824));
#18971=CARTESIAN_POINT('Ctrl Pts',(-92.1729484833227,-26.6488405314842,
5.62913242812112));
#18972=CARTESIAN_POINT('Ctrl Pts',(-91.2359217088655,-26.5421352647047,
5.68179348320399));
#18973=CARTESIAN_POINT('Ctrl Pts',(-90.5560549938817,-26.0672603088487,
5.73445453828687));
#18974=CARTESIAN_POINT('Ctrl Pts',(-89.8761882788978,-25.5923853529926,
5.78711559336975));
#18975=CARTESIAN_POINT('Ctrl Pts',(-89.4534816233873,-24.7493407080601,
5.83977664845263));
#18976=CARTESIAN_POINT('Ctrl Pts',(-89.479639709574,-23.9204615079354,5.8924377035355));
#18977=CARTESIAN_POINT('Ctrl Pts',(-89.5057977957607,-23.0915823078108,
5.94509875861838));
#18978=CARTESIAN_POINT('Ctrl Pts',(-89.9808206236446,-22.276868552494,5.99775981370126));
#18979=CARTESIAN_POINT('Ctrl Pts',(-90.6892772339901,-21.845806834092,6.05042086878414));
#18980=CARTESIAN_POINT('Ctrl Pts',(-91.3977338443356,-21.4147451156901,
6.10308192386702));
#18981=CARTESIAN_POINT('Ctrl Pts',(-92.3396242371427,-21.3673354342031,
6.15574297894989));
#18982=CARTESIAN_POINT('Ctrl Pts',(-93.0877850449385,-21.7250788890635,
6.20840403403277));
#18983=CARTESIAN_POINT('Ctrl Pts',(-93.8359458527343,-22.0828223439238,
6.26106508911565));
#18984=CARTESIAN_POINT('Ctrl Pts',(-94.3903770755186,-22.8457189351315,
6.31372614419853));
#18985=CARTESIAN_POINT('Ctrl Pts',(-94.499634691726,-23.6677820393728,6.36638719928141));
#18986=CARTESIAN_POINT('Ctrl Pts',(-94.5141782213651,-23.7772087277519,
6.37339703202361));
#18987=CARTESIAN_POINT('Ctrl Pts',(-94.5208337745228,-23.8876837803117,
6.38040686476582));
#18988=CARTESIAN_POINT('Ctrl Pts',(-94.5199606688991,-23.9982645762516,
6.38741669750803));
#18989=CARTESIAN_POINT('Origin',(-92.,-24.,5.));
#18990=CARTESIAN_POINT('',(-94.5136290410546,-23.9995053986546,7.38741669750802));
#18991=CARTESIAN_POINT('',(-94.5157926212741,-24.0020516723221,7.11258330249199));
#18992=CARTESIAN_POINT('',(-94.5175,-24.,5.));
#18993=CARTESIAN_POINT('Ctrl Pts',(-94.5157926212741,-24.0020516723221,
7.11258330249199));
#18994=CARTESIAN_POINT('Ctrl Pts',(-94.511298858366,-23.4252696399995,7.07617562814403));
#18995=CARTESIAN_POINT('Ctrl Pts',(-94.3140599311548,-22.8457098245431,
7.03976795379607));
#18996=CARTESIAN_POINT('Ctrl Pts',(-93.9507614766045,-22.4021663794855,
7.00336027944811));
#18997=CARTESIAN_POINT('Ctrl Pts',(-93.4252766641513,-21.7606130199219,
6.95069922436523));
#18998=CARTESIAN_POINT('Ctrl Pts',(-92.5523700775016,-21.4036265833224,
6.89803816928235));
#18999=CARTESIAN_POINT('Ctrl Pts',(-91.7279197494919,-21.4931065124105,
6.84537711419947));
#19000=CARTESIAN_POINT('Ctrl Pts',(-90.9034694214823,-21.5825864414987,
6.7927160591166));
#19001=CARTESIAN_POINT('Ctrl Pts',(-90.1274753521127,-22.1185327362746,
6.74005500403372));
#19002=CARTESIAN_POINT('Ctrl Pts',(-89.7518640956472,-22.8578846048887,
6.68739394895084));
#19003=CARTESIAN_POINT('Ctrl Pts',(-89.3762528391816,-23.5972364735029,
6.63473289386796));
#19004=CARTESIAN_POINT('Ctrl Pts',(-89.4010243956202,-24.5399939159553,
6.58207183878508));
#19005=CARTESIAN_POINT('Ctrl Pts',(-89.8149444410542,-25.258600343256,6.52941078370221));
#19006=CARTESIAN_POINT('Ctrl Pts',(-90.2288644864881,-25.9772067705567,
6.47674972861933));
#19007=CARTESIAN_POINT('Ctrl Pts',(-91.0319330209175,-26.4716621827057,
6.42408867353645));
#19008=CARTESIAN_POINT('Ctrl Pts',(-91.8599447589054,-26.5177226117209,
6.37142761845357));
#19009=CARTESIAN_POINT('Ctrl Pts',(-92.6879564968933,-26.5637830407361,
6.31876656337069));
#19010=CARTESIAN_POINT('Ctrl Pts',(-93.5409114384396,-26.1614484866175,
6.26610550828782));
#19011=CARTESIAN_POINT('Ctrl Pts',(-94.0319799608884,-25.4931845360073,
6.21344445320494));
#19012=CARTESIAN_POINT('Ctrl Pts',(-94.3454927087508,-25.0665449574646,
6.17982406963395));
#19013=CARTESIAN_POINT('Ctrl Pts',(-94.5115032555984,-24.531514543491,6.14620368606297));
#19014=CARTESIAN_POINT('Ctrl Pts',(-94.5147663248015,-23.9983410423439,
6.11258330249198));
#19015=CARTESIAN_POINT('Ctrl Pts',(-94.5199606688991,-23.9982645762516,
6.38741669750803));
#19016=CARTESIAN_POINT('Ctrl Pts',(-94.5142746075592,-24.7184170660063,
6.4330679198487));
#19017=CARTESIAN_POINT('Ctrl Pts',(-94.1892825133498,-25.44305435182,6.47871914218937));
#19018=CARTESIAN_POINT('Ctrl Pts',(-93.6442303551587,-25.9118182197226,
6.52437036453004));
#19019=CARTESIAN_POINT('Ctrl Pts',(-93.0154843927538,-26.4525616785562,
6.57703141961292));
#19020=CARTESIAN_POINT('Ctrl Pts',(-92.0939084583139,-26.6528189789487,
6.6296924746958));
#19021=CARTESIAN_POINT('Ctrl Pts',(-91.2974529654966,-26.4217700194305,
6.68235352977868));
#19022=CARTESIAN_POINT('Ctrl Pts',(-90.5009974726793,-26.1907210599122,
6.73501458486156));
#19023=CARTESIAN_POINT('Ctrl Pts',(-89.8296624214848,-25.5283658404831,
6.78767563994443));
#19024=CARTESIAN_POINT('Ctrl Pts',(-89.5879097152778,-24.7350937531495,
6.84033669502731));
#19025=CARTESIAN_POINT('Ctrl Pts',(-89.3461570090709,-23.941821665816,6.89299775011019));
#19026=CARTESIAN_POINT('Ctrl Pts',(-89.5339866478515,-23.0176327105779,
6.94565880519307));
#19027=CARTESIAN_POINT('Ctrl Pts',(-90.0662146837015,-22.3816623586851,
6.99831986027595));
#19028=CARTESIAN_POINT('Ctrl Pts',(-90.5984427195515,-21.7456920067922,
7.05098091535882));
#19029=CARTESIAN_POINT('Ctrl Pts',(-91.4750691524708,-21.3979402582445,
7.1036419704417));
#19030=CARTESIAN_POINT('Ctrl Pts',(-92.2985289370466,-21.4961184498875,
7.15630302552458));
#19031=CARTESIAN_POINT('Ctrl Pts',(-93.1219887216224,-21.5942966415305,
7.20896408060745));
#19032=CARTESIAN_POINT('Ctrl Pts',(-93.8922818578547,-22.1384047733641,
7.26162513569033));
#19033=CARTESIAN_POINT('Ctrl Pts',(-94.2600672575076,-22.8816805542397,
7.31428619077321));
#19034=CARTESIAN_POINT('Ctrl Pts',(-94.4303153507392,-23.2257433815264,
7.33866302635148));
#19035=CARTESIAN_POINT('Ctrl Pts',(-94.5143152963871,-23.6124832538171,
7.36303986192975));
#19036=CARTESIAN_POINT('Ctrl Pts',(-94.5136290410546,-23.9995053986546,
7.38741669750802));
#19037=CARTESIAN_POINT('Origin',(-92.,-24.,5.));
#19038=CARTESIAN_POINT('',(-94.5182106813093,-24.0021944371302,8.38741669750803));
#19039=CARTESIAN_POINT('',(-94.5215633824187,-23.9996804087645,8.11258330249198));
#19040=CARTESIAN_POINT('',(-94.5175,-24.,5.));
#19041=CARTESIAN_POINT('Ctrl Pts',(-94.5215633824187,-23.9996804087645,
8.11258330249198));
#19042=CARTESIAN_POINT('Ctrl Pts',(-94.5215950065109,-23.9821424208032,
8.11146968039084));
#19043=CARTESIAN_POINT('Ctrl Pts',(-94.5214276959298,-23.9646050519463,
8.11035605828969));
#19044=CARTESIAN_POINT('Ctrl Pts',(-94.5210595996876,-23.9470718985317,
8.10924243618855));
#19045=CARTESIAN_POINT('Ctrl Pts',(-94.5036530337929,-23.1179626730646,
8.05658138110567));
#19046=CARTESIAN_POINT('Ctrl Pts',(-94.0372570305162,-22.2982798630938,
8.0039203260228));
#19047=CARTESIAN_POINT('Ctrl Pts',(-93.3333903289359,-21.8597634086716,
7.95125927093992));
#19048=CARTESIAN_POINT('Ctrl Pts',(-92.6295236273557,-21.4212469542493,
7.89859821585704));
#19049=CARTESIAN_POINT('Ctrl Pts',(-91.688186227472,-21.3638968553754,7.84593716077416));
#19050=CARTESIAN_POINT('Ctrl Pts',(-90.9362906110337,-21.7137224600414,
7.79327610569128));
#19051=CARTESIAN_POINT('Ctrl Pts',(-90.1843949945955,-22.0635480647074,
7.7406150506084));
#19052=CARTESIAN_POINT('Ctrl Pts',(-89.6219411616028,-22.8205493729132,
7.68795399552553));
#19053=CARTESIAN_POINT('Ctrl Pts',(-89.5040115702347,-23.6414133236746,
7.63529294044265));
#19054=CARTESIAN_POINT('Ctrl Pts',(-89.3860819788666,-24.4622772744359,
7.58263188535977));
#19055=CARTESIAN_POINT('Ctrl Pts',(-89.7126766291231,-25.3470038677529,
7.52997083027689));
#19056=CARTESIAN_POINT('Ctrl Pts',(-90.3356792508831,-25.8943545185808,
7.47730977519401));
#19057=CARTESIAN_POINT('Ctrl Pts',(-90.9586818726431,-26.4417051694086,
7.42464872011113));
#19058=CARTESIAN_POINT('Ctrl Pts',(-91.8780924659066,-26.6516798777473,
7.37198766502825));
#19059=CARTESIAN_POINT('Ctrl Pts',(-92.6769426469386,-26.429051518253,7.31932660994538));
#19060=CARTESIAN_POINT('Ctrl Pts',(-93.4757928279705,-26.2064231587587,
7.2666655548625));
#19061=CARTESIAN_POINT('Ctrl Pts',(-94.1540825967709,-25.5511917314315,
7.21400449977962));
#19062=CARTESIAN_POINT('Ctrl Pts',(-94.4041959620427,-24.760515876504,7.16134344469674));
#19063=CARTESIAN_POINT('Ctrl Pts',(-94.4813912963606,-24.516480589178,7.14509006396182));
#19064=CARTESIAN_POINT('Ctrl Pts',(-94.5177987598365,-24.2595429331701,
7.1288366832269));
#19065=CARTESIAN_POINT('Ctrl Pts',(-94.5157926212741,-24.0020516723221,
7.11258330249199));
#19066=CARTESIAN_POINT('Ctrl Pts',(-94.5136290410546,-23.9995053986546,
7.38741669750802));
#19067=CARTESIAN_POINT('Ctrl Pts',(-94.5128327852651,-24.4485636557274,
7.41570091701263));
#19068=CARTESIAN_POINT('Ctrl Pts',(-94.3980256245316,-24.8980019292388,
7.44398513651724));
#19069=CARTESIAN_POINT('Ctrl Pts',(-94.1716474294659,-25.2815965984927,
7.47226935602185));
#19070=CARTESIAN_POINT('Ctrl Pts',(-93.7501645386979,-25.9957934319524,
7.52493041110473));
#19071=CARTESIAN_POINT('Ctrl Pts',(-92.9419210940886,-26.4817436689545,
7.5775914661876));
#19072=CARTESIAN_POINT('Ctrl Pts',(-92.1134692701342,-26.5190607190089,
7.63025252127048));
#19073=CARTESIAN_POINT('Ctrl Pts',(-91.2850174461799,-26.5563777690633,
7.68291357635336));
#19074=CARTESIAN_POINT('Ctrl Pts',(-90.4363572428804,-26.1450616321701,
7.73557463143624));
#19075=CARTESIAN_POINT('Ctrl Pts',(-89.9523705889737,-25.4716509197329,
7.78823568651912));
#19076=CARTESIAN_POINT('Ctrl Pts',(-89.468383935067,-24.7982402072957,7.840896741602));
#19077=CARTESIAN_POINT('Ctrl Pts',(-89.3490708305531,-23.8627349193145,
7.89355779668488));
#19078=CARTESIAN_POINT('Ctrl Pts',(-89.6485417162137,-23.0894032334354,
7.94621885176776));
#19079=CARTESIAN_POINT('Ctrl Pts',(-89.9480126018744,-22.3160715475563,
7.99887990685064));
#19080=CARTESIAN_POINT('Ctrl Pts',(-90.6662674777097,-21.7049134637795,
8.05154096193351));
#19081=CARTESIAN_POINT('Ctrl Pts',(-91.4775656801192,-21.5330984509984,
8.10420201701639));
#19082=CARTESIAN_POINT('Ctrl Pts',(-92.2888638825287,-21.3612834382173,
8.15686307209926));
#19083=CARTESIAN_POINT('Ctrl Pts',(-93.1932054115124,-21.628811496432,8.20952412718214));
#19084=CARTESIAN_POINT('Ctrl Pts',(-93.7804555817247,-22.2143564386821,
8.26218518226502));
#19085=CARTESIAN_POINT('Ctrl Pts',(-94.2459623243365,-22.6785114658678,
8.30392902067935));
#19086=CARTESIAN_POINT('Ctrl Pts',(-94.5122228629259,-23.3424942562717,
8.34567285909369));
#19087=CARTESIAN_POINT('Ctrl Pts',(-94.5182106813093,-24.0021944371302,
8.38741669750803));
#19088=CARTESIAN_POINT('Origin',(-92.,-24.,5.));
#19089=CARTESIAN_POINT('',(-94.5201759878003,-23.9984131478585,9.38741669750803));
#19090=CARTESIAN_POINT('',(-94.5149492652116,-23.9982505980887,9.11258330249199));
#19091=CARTESIAN_POINT('',(-94.5175,-24.,5.));
#19092=CARTESIAN_POINT('',(-90.0865340033349,-22.3640127966251,10.));
#19093=CARTESIAN_POINT('Ctrl Pts',(-94.5201759878003,-23.9984131478585,
9.38741669750803));
#19094=CARTESIAN_POINT('Ctrl Pts',(-94.5146936217042,-24.7270926513296,
9.43362796642338));
#19095=CARTESIAN_POINT('Ctrl Pts',(-94.1807325653029,-25.4600317456745,
9.47983923533874));
#19096=CARTESIAN_POINT('Ctrl Pts',(-93.6239879633604,-25.9288767806186,
9.5260505042541));
#19097=CARTESIAN_POINT('Ctrl Pts',(-92.9895375611503,-26.4631593223022,
9.57871155933697));
#19098=CARTESIAN_POINT('Ctrl Pts',(-92.0657751669118,-26.6544830596339,
9.63137261441985));
#19099=CARTESIAN_POINT('Ctrl Pts',(-91.2718706971314,-26.4146105241973,
9.68403366950273));
#19100=CARTESIAN_POINT('Ctrl Pts',(-90.4779662273509,-26.1747379887606,
9.73669472458561));
#19101=CARTESIAN_POINT('Ctrl Pts',(-89.8139196820286,-25.5036691805558,
9.78935577966849));
#19102=CARTESIAN_POINT('Ctrl Pts',(-89.5807331050278,-24.7092693915533,
9.84201683475137));
#19103=CARTESIAN_POINT('Ctrl Pts',(-89.347546528027,-23.9148696025509,9.89467788983425));
#19104=CARTESIAN_POINT('Ctrl Pts',(-89.5452199193478,-22.9971388327508,
9.94733894491712));
#19105=CARTESIAN_POINT('Ctrl Pts',(-90.0865340033349,-22.3640127966251,
10.));
#19106=CARTESIAN_POINT('',(-93.9171033105362,-22.361465667796,10.));
#19107=CARTESIAN_POINT('Origin',(-92.,-24.,10.));
#19108=CARTESIAN_POINT('Ctrl Pts',(-93.9171117712833,-22.3614597429257,
10.));
#19109=CARTESIAN_POINT('Ctrl Pts',(-93.3939570615584,-21.7523041616072,
9.94901908464118));
#19110=CARTESIAN_POINT('Ctrl Pts',(-92.5534187329286,-21.4121722649682,
9.89803816928236));
#19111=CARTESIAN_POINT('Ctrl Pts',(-91.7542642249036,-21.4905146133598,
9.84705725392353));
#19112=CARTESIAN_POINT('Ctrl Pts',(-90.9287725821855,-21.5714388316664,
9.79439619884065));
#19113=CARTESIAN_POINT('Ctrl Pts',(-90.1474374185984,-22.0988744884398,
9.74173514375777));
#19114=CARTESIAN_POINT('Ctrl Pts',(-89.7641119401365,-22.8341462635555,
9.68907408867489));
#19115=CARTESIAN_POINT('Ctrl Pts',(-89.3807864616747,-23.5694180386713,
9.63641303359201));
#19116=CARTESIAN_POINT('Ctrl Pts',(-89.3954706683381,-24.5125259321295,
9.58375197850913));
#19117=CARTESIAN_POINT('Ctrl Pts',(-89.8017475811355,-25.2354979451803,
9.53109092342626));
#19118=CARTESIAN_POINT('Ctrl Pts',(-90.2080244939329,-25.9584699582311,
9.47842986834338));
#19119=CARTESIAN_POINT('Ctrl Pts',(-91.0058941128642,-26.4613060908746,
9.4257688132605));
#19120=CARTESIAN_POINT('Ctrl Pts',(-91.8333901989263,-26.5160871276519,
9.37310775817762));
#19121=CARTESIAN_POINT('Ctrl Pts',(-92.6608862849884,-26.5708681644292,
9.32044670309475));
#19122=CARTESIAN_POINT('Ctrl Pts',(-93.5180088381812,-26.1775941053403,
9.26778564801187));
#19123=CARTESIAN_POINT('Ctrl Pts',(-94.0160962955284,-25.5145599775471,
9.21512459292899));
#19124=CARTESIAN_POINT('Ctrl Pts',(-94.339387264832,-25.0842079526291,9.18094416278332));
#19125=CARTESIAN_POINT('Ctrl Pts',(-94.5114221549398,-24.5402100730638,
9.14676373263765));
#19126=CARTESIAN_POINT('Ctrl Pts',(-94.5149492652116,-23.9982505980887,
9.11258330249199));
#19127=CARTESIAN_POINT('Origin',(-92.,-24.,12.2084234471775));
#19128=CARTESIAN_POINT('',(-95.0782768196867,-23.9992118911386,1.79157655282254));
#19129=CARTESIAN_POINT('',(-95.0686110023456,-23.9996651237392,1.70842344717745));
#19130=CARTESIAN_POINT('',(-95.0735,-23.9999999999999,12.2084234471775));
#19131=CARTESIAN_POINT('',(-91.2062007174672,-26.9692229537457,0.999999999999999));
#19132=CARTESIAN_POINT('Ctrl Pts',(-95.0686110023456,-23.9996651237392,
1.70842344717745));
#19133=CARTESIAN_POINT('Ctrl Pts',(-95.0689534453578,-23.5053846687107,
1.68292651844982));
#19134=CARTESIAN_POINT('Ctrl Pts',(-94.7235567931003,-21.9907712706008,
1.6047685346393));
#19135=CARTESIAN_POINT('Ctrl Pts',(-92.3539161166825,-20.3911596148569,
1.4739494957459));
#19136=CARTESIAN_POINT('Ctrl Pts',(-89.1687759971456,-21.7301450507159,
1.31596633049727));
#19137=CARTESIAN_POINT('Ctrl Pts',(-88.5566856051374,-25.1332975040883,
1.15798316524863));
#19138=CARTESIAN_POINT('Ctrl Pts',(-90.2237466982397,-26.7065713079336,
1.05266105508288));
#19139=CARTESIAN_POINT('Ctrl Pts',(-91.2062007174672,-26.9692229537457,
0.999999999999999));
#19140=CARTESIAN_POINT('',(-92.7937992825329,-26.9692229537457,1.));
#19141=CARTESIAN_POINT('Origin',(-92.,-24.,0.999999999999999));
#19142=CARTESIAN_POINT('Ctrl Pts',(-95.0782768196867,-23.9992118911386,
1.79157655282254));
#19143=CARTESIAN_POINT('Ctrl Pts',(-95.0784229132411,-23.9562584982139,
1.78934283757203));
#19144=CARTESIAN_POINT('Ctrl Pts',(-95.058222313234,-22.9007975699364,1.73444806723864));
#19145=CARTESIAN_POINT('Ctrl Pts',(-93.8523950876059,-20.8820465732966,
1.62689224182237));
#19146=CARTESIAN_POINT('Ctrl Pts',(-90.400968139612,-20.7444872144857,1.46890907657374));
#19147=CARTESIAN_POINT('Ctrl Pts',(-88.4000491745082,-23.5606286501727,
1.31092591132511));
#19148=CARTESIAN_POINT('Ctrl Pts',(-89.6506964041097,-26.7394102869818,
1.15462288580053));
#19149=CARTESIAN_POINT('Ctrl Pts',(-91.8480946426715,-27.2254055619768,
1.05098091535883));
#19150=CARTESIAN_POINT('Ctrl Pts',(-92.7957017813267,-26.9743128096467,
1.));
#19151=CARTESIAN_POINT('Origin',(-92.,-24.,12.2084234471775));
#19152=CARTESIAN_POINT('',(-95.0699491247542,-23.9980972118633,2.79157655282254));
#19153=CARTESIAN_POINT('',(-95.075008445109,-24.0025755322285,2.70842344717745));
#19154=CARTESIAN_POINT('',(-95.0735,-23.9999999999999,12.2084234471775));
#19155=CARTESIAN_POINT('Ctrl Pts',(-95.075008445109,-24.0025755322285,2.70842344717745));
#19156=CARTESIAN_POINT('Ctrl Pts',(-95.0676143896354,-23.1760102841626,
2.66555951561375));
#19157=CARTESIAN_POINT('Ctrl Pts',(-94.2993641383816,-21.3218328468575,
2.57003452896717));
#19158=CARTESIAN_POINT('Ctrl Pts',(-91.1738621865499,-20.4685620798055,
2.42184848723771));
#19159=CARTESIAN_POINT('Ctrl Pts',(-88.5910234496018,-22.7619776832305,
2.26386532198907));
#19160=CARTESIAN_POINT('Ctrl Pts',(-89.1003113510008,-26.1783942746989,
2.10588215674044));
#19161=CARTESIAN_POINT('Ctrl Pts',(-92.2395758256157,-27.6187848570707,
1.94789899149181));
#19162=CARTESIAN_POINT('Ctrl Pts',(-94.690200871183,-26.074343589762,1.81541275497081));
#19163=CARTESIAN_POINT('Ctrl Pts',(-95.0682461676098,-24.5262656754664,
1.73558757353269));
#19164=CARTESIAN_POINT('Ctrl Pts',(-95.0686110023456,-23.9996651237392,
1.70842344717745));
#19165=CARTESIAN_POINT('Ctrl Pts',(-95.0699491247542,-23.9980972118633,
2.79157655282254));
#19166=CARTESIAN_POINT('Ctrl Pts',(-95.0721211881234,-23.6185397169383,
2.77197583473597));
#19167=CARTESIAN_POINT('Ctrl Pts',(-94.8315580332634,-22.2218843885843,
2.69971406156651));
#19168=CARTESIAN_POINT('Ctrl Pts',(-92.7514083751607,-20.4518994955132,
2.57479123331418));
#19169=CARTESIAN_POINT('Ctrl Pts',(-89.4392013302128,-21.4317376344076,
2.41680806806554));
#19170=CARTESIAN_POINT('Ctrl Pts',(-88.4497278964895,-24.7410889661721,
2.25882490281691));
#19171=CARTESIAN_POINT('Ctrl Pts',(-90.6804687378896,-27.3782236865054,
2.10084173756828));
#19172=CARTESIAN_POINT('Ctrl Pts',(-94.0596142672113,-26.9572795305498,
1.94509228757015));
#19173=CARTESIAN_POINT('Ctrl Pts',(-95.0749786780308,-24.9689081590363,
1.84200389265491));
#19174=CARTESIAN_POINT('Ctrl Pts',(-95.0782768196867,-23.9992118911386,
1.79157655282254));
#19175=CARTESIAN_POINT('Origin',(-92.,-24.,12.2084234471775));
#19176=CARTESIAN_POINT('',(-95.0716998581065,-24.0025715694568,3.79157655282254));
#19177=CARTESIAN_POINT('',(-95.0762206925999,-23.9977671184427,3.70842344717745));
#19178=CARTESIAN_POINT('',(-95.0735,-23.9999999999999,12.2084234471775));
#19179=CARTESIAN_POINT('Ctrl Pts',(-95.0762206925998,-23.9977671184427,
3.70842344717745));
#19180=CARTESIAN_POINT('Ctrl Pts',(-95.0774154713987,-23.8519430387288,
3.70085356786056));
#19181=CARTESIAN_POINT('Ctrl Pts',(-95.0019701064919,-22.6929124367374,
3.6406226334608));
#19182=CARTESIAN_POINT('Ctrl Pts',(-93.5299146181504,-20.7116868408496,
3.52773064397815));
#19183=CARTESIAN_POINT('Ctrl Pts',(-90.0822080355936,-20.9217351333484,
3.36974747872952));
#19184=CARTESIAN_POINT('Ctrl Pts',(-88.3740037605625,-23.92387423856,3.21176431348088));
#19185=CARTESIAN_POINT('Ctrl Pts',(-89.9547027823836,-26.99506300667,3.05378114823225));
#19186=CARTESIAN_POINT('Ctrl Pts',(-93.3905542616683,-27.349625359661,2.89579798298362));
#19187=CARTESIAN_POINT('Ctrl Pts',(-94.9751245860296,-25.3940964065108,
2.78067874929868));
#19188=CARTESIAN_POINT('Ctrl Pts',(-95.076698455151,-24.1914980490519,2.71822057069663));
#19189=CARTESIAN_POINT('Ctrl Pts',(-95.075008445109,-24.0025755322285,2.70842344717745));
#19190=CARTESIAN_POINT('Ctrl Pts',(-95.0716998581065,-24.0025715694568,
3.79157655282254));
#19191=CARTESIAN_POINT('Ctrl Pts',(-95.0659415382079,-23.2877405601207,
3.7546088318999));
#19192=CARTESIAN_POINT('Ctrl Pts',(-94.4623934875611,-21.5458532246353,
3.66498005589439));
#19193=CARTESIAN_POINT('Ctrl Pts',(-91.5706310215098,-20.3987107062197,
3.52269022480599));
#19194=CARTESIAN_POINT('Ctrl Pts',(-88.7493845448822,-22.3915405493825,
3.36470705955735));
#19195=CARTESIAN_POINT('Ctrl Pts',(-88.8765572614881,-25.8432981737925,
3.20672389430872));
#19196=CARTESIAN_POINT('Ctrl Pts',(-91.8367991007263,-27.6231211133645,
3.04874072906008));
#19197=CARTESIAN_POINT('Ctrl Pts',(-94.5594316628929,-26.3035556341772,
2.91035828189803));
#19198=CARTESIAN_POINT('Ctrl Pts',(-95.0662855269897,-24.6382930779672,
2.82463688981884));
#19199=CARTESIAN_POINT('Ctrl Pts',(-95.0699491247542,-23.9980972118633,
2.79157655282254));
#19200=CARTESIAN_POINT('Origin',(-92.,-24.,12.2084234471775));
#19201=CARTESIAN_POINT('',(-95.0783838750166,-23.9994167251475,4.79157655282254));
#19202=CARTESIAN_POINT('',(-95.0687191146691,-23.9995675532748,4.70842344717746));
#19203=CARTESIAN_POINT('',(-95.0735,-23.9999999999999,12.2084234471775));
#19204=CARTESIAN_POINT('Ctrl Pts',(-95.0687191146691,-23.9995675532748,
4.70842344717746));
#19205=CARTESIAN_POINT('Ctrl Pts',(-95.0693322679534,-23.5161929491143,
4.6834865650245));
#19206=CARTESIAN_POINT('Ctrl Pts',(-94.7346951702921,-22.0128432522753,
4.60588862778867));
#19207=CARTESIAN_POINT('Ctrl Pts',(-92.3913282785029,-20.3943788173916,
4.47562963546995));
#19208=CARTESIAN_POINT('Ctrl Pts',(-89.1942537915232,-21.7018637718047,
4.31764647022133));
#19209=CARTESIAN_POINT('Ctrl Pts',(-88.5420868753907,-25.0938367187666,
4.15966330497269));
#19210=CARTESIAN_POINT('Ctrl Pts',(-91.0263652022841,-27.4936624405808,
4.00168013972406));
#19211=CARTESIAN_POINT('Ctrl Pts',(-94.2324121355514,-26.7614664286127,
3.85126685379231));
#19212=CARTESIAN_POINT('Ctrl Pts',(-95.0691038049237,-24.8663911656747,
3.75351462294344));
#19213=CARTESIAN_POINT('Ctrl Pts',(-95.0762206925998,-23.9977671184427,
3.70842344717745));
#19214=CARTESIAN_POINT('Ctrl Pts',(-95.0783838750166,-23.9994167251475,
4.79157655282255));
#19215=CARTESIAN_POINT('Ctrl Pts',(-95.0784684546912,-23.9672353748386,
4.78990288414672));
#19216=CARTESIAN_POINT('Ctrl Pts',(-95.0634882463523,-22.9225663485135,
4.73556816038801));
#19217=CARTESIAN_POINT('Ctrl Pts',(-93.885189770327,-20.9016614152429,4.62857238154643));
#19218=CARTESIAN_POINT('Ctrl Pts',(-90.435457678629,-20.7280205108105,4.47058921629779));
#19219=CARTESIAN_POINT('Ctrl Pts',(-88.4048188734298,-23.5221766816715,
4.31260605104916));
#19220=CARTESIAN_POINT('Ctrl Pts',(-89.6351320616122,-26.7497349135866,
4.15462288580052));
#19221=CARTESIAN_POINT('Ctrl Pts',(-93.0104611872221,-27.4831897200468,
3.99663972055189));
#19222=CARTESIAN_POINT('Ctrl Pts',(-94.8939121321551,-25.6249319667866,
3.8756242762259));
#19223=CARTESIAN_POINT('Ctrl Pts',(-95.0741443484921,-24.3060277095063,
3.80726988698278));
#19224=CARTESIAN_POINT('Ctrl Pts',(-95.0716998581065,-24.0025715694568,
3.79157655282254));
#19225=CARTESIAN_POINT('Origin',(-92.,-24.,12.2084234471775));
#19226=CARTESIAN_POINT('',(-95.0701625816395,-23.9979746548734,5.79157655282255));
#19227=CARTESIAN_POINT('',(-95.0746895390838,-24.0026322734109,5.70842344717746));
#19228=CARTESIAN_POINT('',(-95.0735,-23.9999999999999,12.2084234471775));
#19229=CARTESIAN_POINT('Ctrl Pts',(-95.0746895390839,-24.0026322734109,
5.70842344717746));
#19230=CARTESIAN_POINT('Ctrl Pts',(-95.0673210859913,-23.1866491427393,
5.66611956218844));
#19231=CARTESIAN_POINT('Ctrl Pts',(-94.3157338396919,-21.3429097126816,
5.57115462211654));
#19232=CARTESIAN_POINT('Ctrl Pts',(-91.2111784520928,-20.4600278964634,
5.42352862696177));
#19233=CARTESIAN_POINT('Ctrl Pts',(-88.6043011989707,-22.7260802299219,
5.26554546171313));
#19234=CARTESIAN_POINT('Ctrl Pts',(-89.0774386607742,-26.1476212763575,
5.1075622964645));
#19235=CARTESIAN_POINT('Ctrl Pts',(-92.201439010718,-27.6211965224103,4.94957913121586));
#19236=CARTESIAN_POINT('Ctrl Pts',(-94.6784591036876,-26.0960763882475,
4.81653284812018));
#19237=CARTESIAN_POINT('Ctrl Pts',(-95.068037426895,-24.536970787307,4.73614762010738));
#19238=CARTESIAN_POINT('Ctrl Pts',(-95.0687191146691,-23.9995675532748,
4.70842344717746));
#19239=CARTESIAN_POINT('Ctrl Pts',(-95.0701625816395,-23.9979746548734,
5.79157655282255));
#19240=CARTESIAN_POINT('Ctrl Pts',(-95.0724187402062,-23.629326646717,5.77253588131065));
#19241=CARTESIAN_POINT('Ctrl Pts',(-94.8409295378372,-22.2438417959684,
5.70083415471588));
#19242=CARTESIAN_POINT('Ctrl Pts',(-92.7888215637087,-20.460027825551,5.57647137303824));
#19243=CARTESIAN_POINT('Ctrl Pts',(-89.4664561758693,-21.4048510358159,
5.4184882077896));
#19244=CARTESIAN_POINT('Ctrl Pts',(-88.4421015118167,-24.7035629345559,
5.26050504254097));
#19245=CARTESIAN_POINT('Ctrl Pts',(-90.6448822152433,-27.3641192375838,
5.10252187729233));
#19246=CARTESIAN_POINT('Ctrl Pts',(-94.0404433629951,-26.9774448457588,
4.94621238071953));
#19247=CARTESIAN_POINT('Ctrl Pts',(-95.0758072022182,-24.9798036840461,
4.8425639392296));
#19248=CARTESIAN_POINT('Ctrl Pts',(-95.0783838750166,-23.9994167251475,
4.79157655282255));
#19249=CARTESIAN_POINT('Origin',(-92.,-24.,12.2084234471775));
#19250=CARTESIAN_POINT('',(-95.0714155398157,-24.0025047924058,6.79157655282255));
#19251=CARTESIAN_POINT('',(-95.0765041175219,-23.9978813009372,6.70842344717745));
#19252=CARTESIAN_POINT('',(-95.0735,-23.9999999999999,12.2084234471775));
#19253=CARTESIAN_POINT('Ctrl Pts',(-95.0765041175219,-23.9978813009372,
6.70842344717746));
#19254=CARTESIAN_POINT('Ctrl Pts',(-95.077570052034,-23.8628782914748,6.70141361443525));
#19255=CARTESIAN_POINT('Ctrl Pts',(-95.008402446927,-22.7147701434973,6.64174272661016));
#19256=CARTESIAN_POINT('Ctrl Pts',(-93.5645422900301,-20.7280205763547,
6.52941078370221));
#19257=CARTESIAN_POINT('Ctrl Pts',(-90.1148102674372,-20.9016614773084,
6.37142761845357));
#19258=CARTESIAN_POINT('Ctrl Pts',(-88.3750096777633,-23.8856011718064,
6.21344445320494));
#19259=CARTESIAN_POINT('Ctrl Pts',(-89.9231990390881,-26.973304507894,6.0554612879563));
#19260=CARTESIAN_POINT('Ctrl Pts',(-93.3551177576112,-27.364119170194,5.89747812270767));
#19261=CARTESIAN_POINT('Ctrl Pts',(-94.9680496218174,-25.4159924088721,
5.78179884244805));
#19262=CARTESIAN_POINT('Ctrl Pts',(-95.0764935417666,-24.2024076860067,
5.71878061727132));
#19263=CARTESIAN_POINT('Ctrl Pts',(-95.0746895390839,-24.0026322734109,
5.70842344717746));
#19264=CARTESIAN_POINT('Ctrl Pts',(-95.0714155398157,-24.0025047924058,
6.79157655282255));
#19265=CARTESIAN_POINT('Ctrl Pts',(-95.0659293112961,-23.2983381285158,
6.75516887847459));
#19266=CARTESIAN_POINT('Ctrl Pts',(-94.4768297637754,-21.5673490693386,
6.66610014904376));
#19267=CARTESIAN_POINT('Ctrl Pts',(-91.6086717136577,-20.3943787451648,
6.52437036453004));
#19268=CARTESIAN_POINT('Ctrl Pts',(-88.7665452720996,-22.3573153135784,
6.36638719928141));
#19269=CARTESIAN_POINT('Ctrl Pts',(-88.8572726350159,-25.8102229593112,
6.20840403403277));
#19270=CARTESIAN_POINT('Ctrl Pts',(-91.7985609852469,-27.6211965949497,
6.05042086878414));
#19271=CARTESIAN_POINT('Ctrl Pts',(-94.5460461813276,-26.3252216524648,
5.9114783750474));
#19272=CARTESIAN_POINT('Ctrl Pts',(-95.0661788504793,-24.6489016680912,
5.82519693639353));
#19273=CARTESIAN_POINT('Ctrl Pts',(-95.0701625816395,-23.9979746548734,
5.79157655282255));
#19274=CARTESIAN_POINT('Origin',(-92.,-24.,12.2084234471775));
#19275=CARTESIAN_POINT('',(-95.0784607967682,-23.9996098257547,7.79157655282255));
#19276=CARTESIAN_POINT('',(-95.0687741242031,-23.9993961639582,7.70842344717745));
#19277=CARTESIAN_POINT('',(-95.0735,-23.9999999999999,12.2084234471775));
#19278=CARTESIAN_POINT('Ctrl Pts',(-95.0687741242031,-23.9993961639582,
7.70842344717745));
#19279=CARTESIAN_POINT('Ctrl Pts',(-95.0696119417857,-23.5268986218895,
7.68404661159918));
#19280=CARTESIAN_POINT('Ctrl Pts',(-94.7455188317854,-22.034758037689,7.60700872093803));
#19281=CARTESIAN_POINT('Ctrl Pts',(-92.4293689698895,-20.3987107783727,
7.47730977519402));
#19282=CARTESIAN_POINT('Ctrl Pts',(-89.2186702510282,-21.6723731408291,
7.31932660994537));
#19283=CARTESIAN_POINT('Ctrl Pts',(-88.5307325412461,-25.0572725496761,
7.16134344469675));
#19284=CARTESIAN_POINT('Ctrl Pts',(-90.9895388330194,-27.4831896502702,
7.0033602794481));
#19285=CARTESIAN_POINT('Ctrl Pts',(-94.2151019833044,-26.782278803337,6.85238694694169));
#19286=CARTESIAN_POINT('Ctrl Pts',(-95.0695622666666,-24.8770823643973,
6.75407466951813));
#19287=CARTESIAN_POINT('Ctrl Pts',(-95.0765041175219,-23.9978813009372,
6.70842344717746));
#19288=CARTESIAN_POINT('Ctrl Pts',(-95.0784607967682,-23.9996098257547,
7.79157655282255));
#19289=CARTESIAN_POINT('Ctrl Pts',(-95.0784994051683,-23.978198502617,7.7904629307214));
#19290=CARTESIAN_POINT('Ctrl Pts',(-95.0686359944837,-22.944323237583,7.73668825353738));
#19291=CARTESIAN_POINT('Ctrl Pts',(-93.9177920028682,-20.9217350716083,
7.63025252127049));
#19292=CARTESIAN_POINT('Ctrl Pts',(-90.4700853511787,-20.7116867750179,
7.47226935602185));
#19293=CARTESIAN_POINT('Ctrl Pts',(-88.4100632788413,-23.4842510500175,
7.31428619077322));
#19294=CARTESIAN_POINT('Ctrl Pts',(-89.6062364556796,-26.7246171090759,
7.15630302552458));
#19295=CARTESIAN_POINT('Ctrl Pts',(-92.9736348172232,-27.4936625105602,
6.99831986027594));
#19296=CARTESIAN_POINT('Ctrl Pts',(-94.8854041041608,-25.6468834845165,
6.87674436937527));
#19297=CARTESIAN_POINT('Ctrl Pts',(-95.073864742148,-24.3168640338026,6.80782993355747));
#19298=CARTESIAN_POINT('Ctrl Pts',(-95.0714155398157,-24.0025047924058,
6.79157655282255));
#19299=CARTESIAN_POINT('Origin',(-92.,-24.,12.2084234471775));
#19300=CARTESIAN_POINT('',(-95.0703859251749,-23.9978642356407,8.79157655282255));
#19301=CARTESIAN_POINT('',(-95.0743676381347,-24.0026790873961,8.70842344717746));
#19302=CARTESIAN_POINT('',(-95.0735,-23.9999999999999,12.2084234471775));
#19303=CARTESIAN_POINT('Ctrl Pts',(-95.0743676381347,-24.0026790873961,
8.70842344717746));
#19304=CARTESIAN_POINT('Ctrl Pts',(-95.0670573859793,-23.1972814683818,
8.66667960876313));
#19305=CARTESIAN_POINT('Ctrl Pts',(-94.3319129571347,-21.3640272738251,
8.57227471526591));
#19306=CARTESIAN_POINT('Ctrl Pts',(-91.2485916399685,-20.4518995672047,
8.42520876668582));
#19307=CARTESIAN_POINT('Ctrl Pts',(-88.6179385783441,-22.6903039808949,
8.26722560143718));
#19308=CARTESIAN_POINT('Ctrl Pts',(-89.0549302288588,-26.1166501607681,
8.10924243618856));
#19309=CARTESIAN_POINT('Ctrl Pts',(-92.1632008959979,-27.623121040698,7.95125927093991));
#19310=CARTESIAN_POINT('Ctrl Pts',(-94.6666767475757,-26.1179251847747,
7.81765294126956));
#19311=CARTESIAN_POINT('Ctrl Pts',(-95.0678020121201,-24.5476307431492,
7.73670766668206));
#19312=CARTESIAN_POINT('Ctrl Pts',(-95.0687741242031,-23.9993961639582,
7.70842344717745));
#19313=CARTESIAN_POINT('Ctrl Pts',(-95.0703859251749,-23.9978642356407,
8.79157655282255));
#19314=CARTESIAN_POINT('Ctrl Pts',(-95.0727141338614,-23.6401224413272,
8.77309592788534));
#19315=CARTESIAN_POINT('Ctrl Pts',(-94.8501668180301,-22.265785975548,8.70195424786526));
#19316=CARTESIAN_POINT('Ctrl Pts',(-92.8261378316182,-20.4685620052276,
8.57815151276229));
#19317=CARTESIAN_POINT('Ctrl Pts',(-89.493997396212,-21.3782456609066,8.42016834751365));
#19318=CARTESIAN_POINT('Ctrl Pts',(-88.4348704258472,-24.6659673604642,
8.26218518226502));
#19319=CARTESIAN_POINT('Ctrl Pts',(-90.6094457101907,-27.3496254273118,
8.10420201701639));
#19320=CARTESIAN_POINT('Ctrl Pts',(-94.0210779679427,-26.9975623737005,
7.94733247386889));
#19321=CARTESIAN_POINT('Ctrl Pts',(-95.0766736879126,-24.9906989423899,
7.84312398580428));
#19322=CARTESIAN_POINT('Ctrl Pts',(-95.0784607967682,-23.9996098257547,
7.79157655282255));
#19323=CARTESIAN_POINT('Origin',(-92.,-24.,12.2084234471775));
#19324=CARTESIAN_POINT('',(-95.0702887490762,-24.0031018432153,9.79157655282255));
#19325=CARTESIAN_POINT('',(-95.0767669904684,-23.998062685181,9.70842344717746));
#19326=CARTESIAN_POINT('',(-95.0735,-23.9999999999999,12.2084234471775));
#19327=CARTESIAN_POINT('',(-92.7937992825329,-26.9692229537457,10.));
#19328=CARTESIAN_POINT('Ctrl Pts',(-92.7937992825329,-26.9692229537457,
10.));
#19329=CARTESIAN_POINT('Ctrl Pts',(-93.7762533017603,-26.7065713079336,
9.94733894491712));
#19330=CARTESIAN_POINT('Ctrl Pts',(-94.875910333047,-25.6687793941585,9.87786446252464));
#19331=CARTESIAN_POINT('Ctrl Pts',(-95.0726354893275,-24.3283627763233,
9.80838998013215));
#19332=CARTESIAN_POINT('Ctrl Pts',(-95.0702887490763,-24.0031018432153,
9.79157655282255));
#19333=CARTESIAN_POINT('',(-91.2043026670138,-26.9743009685655,10.));
#19334=CARTESIAN_POINT('Origin',(-92.,-24.,10.));
#19335=CARTESIAN_POINT('Ctrl Pts',(-91.2042982523172,-26.9743127795766,
10.));
#19336=CARTESIAN_POINT('Ctrl Pts',(-92.1519054403102,-27.2254055803294,
9.94901908464118));
#19337=CARTESIAN_POINT('Ctrl Pts',(-94.2125562800898,-26.7696542914347,
9.851826900367));
#19338=CARTESIAN_POINT('Ctrl Pts',(-95.0700738217707,-24.8876739876312,
9.75463471609281));
#19339=CARTESIAN_POINT('Ctrl Pts',(-95.0767669904684,-23.998062685181,9.70842344717746));
#19340=CARTESIAN_POINT('Origin',(92.,24.,5.));
#19341=CARTESIAN_POINT('',(89.4865042982783,24.0002742229179,1.38741669750802));
#19342=CARTESIAN_POINT('',(89.4843731420168,23.9964690566784,1.11258330249198));
#19343=CARTESIAN_POINT('',(89.4825,24.,5.));
#19344=CARTESIAN_POINT('',(90.086534003335,25.635987203375,0.999999999999999));
#19345=CARTESIAN_POINT('Ctrl Pts',(89.4843731420168,23.9964690566784,1.11258330249198));
#19346=CARTESIAN_POINT('Ctrl Pts',(89.4895360512898,24.5890870308543,1.07505553499465));
#19347=CARTESIAN_POINT('Ctrl Pts',(89.7007781719159,25.1848035603044,1.03752776749733));
#19348=CARTESIAN_POINT('Ctrl Pts',(90.0865340033349,25.635987203375,0.999999999999998));
#19349=CARTESIAN_POINT('',(89.4825,24.,1.));
#19350=CARTESIAN_POINT('Origin',(92.,24.,1.));
#19351=CARTESIAN_POINT('',(89.4825,24.,0.));
#19352=CARTESIAN_POINT('',(89.4825,24.,5.));
#19353=CARTESIAN_POINT('Origin',(92.,24.,0.));
#19354=CARTESIAN_POINT('',(93.9171034684659,25.6385343514563,0.999999999999999));
#19355=CARTESIAN_POINT('Origin',(92.,24.,1.));
#19356=CARTESIAN_POINT('Ctrl Pts',(93.9171119325403,25.6385402784441,0.999999999999999));
#19357=CARTESIAN_POINT('Ctrl Pts',(93.3939572704879,26.2476956151711,1.05098091535882));
#19358=CARTESIAN_POINT('Ctrl Pts',(92.5534188240449,26.5878280192362,1.10196183071765));
#19359=CARTESIAN_POINT('Ctrl Pts',(91.7542642184068,26.50948576913,1.15294274607647));
#19360=CARTESIAN_POINT('Ctrl Pts',(90.9287724748586,26.4285616523478,1.20560380115935));
#19361=CARTESIAN_POINT('Ctrl Pts',(90.1474372319947,25.9011256605461,1.25826485624223));
#19362=CARTESIAN_POINT('Ctrl Pts',(89.7641117257107,25.1658537555941,1.31092591132511));
#19363=CARTESIAN_POINT('Ctrl Pts',(89.5785168283464,24.8098567987064,1.33642284005274));
#19364=CARTESIAN_POINT('Ctrl Pts',(89.4862237958222,24.4051387264905,1.36191976878038));
#19365=CARTESIAN_POINT('Ctrl Pts',(89.4865042982783,24.0002742229179,1.38741669750802));
#19366=CARTESIAN_POINT('Origin',(92.,24.,5.));
#19367=CARTESIAN_POINT('',(89.4812641621455,23.9978903848741,2.38741669750802));
#19368=CARTESIAN_POINT('',(89.4785876236681,24.0006455599548,2.11258330249198));
#19369=CARTESIAN_POINT('',(89.4825,24.,5.));
#19370=CARTESIAN_POINT('Ctrl Pts',(89.4785876236681,24.0006455599548,2.11258330249198));
#19371=CARTESIAN_POINT('Ctrl Pts',(89.4784679588298,24.0358286254365,2.11034958724147));
#19372=CARTESIAN_POINT('Ctrl Pts',(89.4791412415306,24.071006953815,2.10811587199096));
#19373=CARTESIAN_POINT('Ctrl Pts',(89.480621792432,24.1061512101346,2.10588215674044));
#19374=CARTESIAN_POINT('Ctrl Pts',(89.5155265872823,24.9346962171462,2.05322110165756));
#19375=CARTESIAN_POINT('Ctrl Pts',(89.9991161631697,25.7443037579803,2.00056004657469));
#19376=CARTESIAN_POINT('Ctrl Pts',(90.7120874500747,26.1678867011383,1.94789899149181));
#19377=CARTESIAN_POINT('Ctrl Pts',(91.4250587369798,26.5914696442962,1.89523793640893));
#19378=CARTESIAN_POINT('Ctrl Pts',(92.3674117349025,26.6290279897781,1.84257688132605));
#19379=CARTESIAN_POINT('Ctrl Pts',(93.1117466201966,26.2633574548232,1.78991582624318));
#19380=CARTESIAN_POINT('Ctrl Pts',(93.8560815054908,25.8976869198683,1.7372547711603));
#19381=CARTESIAN_POINT('Ctrl Pts',(94.4023982781564,25.1287875044768,1.68459371607742));
#19382=CARTESIAN_POINT('Ctrl Pts',(94.5029873847571,24.3057173158974,1.63193266099454));
#19383=CARTESIAN_POINT('Ctrl Pts',(94.6035764913578,23.4826471273179,1.57927160591166));
#19384=CARTESIAN_POINT('Ctrl Pts',(94.2584379318934,22.6054061655506,1.52661055082878));
#19385=CARTESIAN_POINT('Ctrl Pts',(93.6239876980049,22.0711235918099,1.4739494957459));
#19386=CARTESIAN_POINT('Ctrl Pts',(92.9895374641164,21.5368410180693,1.42128844066303));
#19387=CARTESIAN_POINT('Ctrl Pts',(92.0657755558037,21.3455168323553,1.36862738558015));
#19388=CARTESIAN_POINT('Ctrl Pts',(91.2718708195105,21.5853896272901,1.31596633049727));
#19389=CARTESIAN_POINT('Ctrl Pts',(90.4779660832174,21.8252624222249,1.26330527541439));
#19390=CARTESIAN_POINT('Ctrl Pts',(89.8139185189439,22.4963321978085,1.21064422033151));
#19391=CARTESIAN_POINT('Ctrl Pts',(89.5807319779765,23.2907318840645,1.15798316524864));
#19392=CARTESIAN_POINT('Ctrl Pts',(89.5137208066282,23.5190197315272,1.14284987766308));
#19393=CARTESIAN_POINT('Ctrl Pts',(89.4822911692266,23.7574924580249,1.12771659007753));
#19394=CARTESIAN_POINT('Ctrl Pts',(89.4843731420168,23.9964690566784,1.11258330249198));
#19395=CARTESIAN_POINT('Ctrl Pts',(89.4865042982783,24.0002742229179,1.38741669750802));
#19396=CARTESIAN_POINT('Ctrl Pts',(89.4868031422779,23.5689363684933,1.41458082386326));
#19397=CARTESIAN_POINT('Ctrl Pts',(89.5921777588412,23.1374323068698,1.4417449502185));
#19398=CARTESIAN_POINT('Ctrl Pts',(89.8017473998347,22.764501991722,1.46890907657374));
#19399=CARTESIAN_POINT('Ctrl Pts',(90.2080243499466,22.0415299509043,1.52157013165662));
#19400=CARTESIAN_POINT('Ctrl Pts',(91.0058940198741,21.5386936873713,1.57423118673949));
#19401=CARTESIAN_POINT('Ctrl Pts',(91.833390176038,21.4839126258589,1.62689224182237));
#19402=CARTESIAN_POINT('Ctrl Pts',(92.6608863322019,21.4291315643466,1.67955329690525));
#19403=CARTESIAN_POINT('Ctrl Pts',(93.5180089746021,21.8224057048548,1.73221435198813));
#19404=CARTESIAN_POINT('Ctrl Pts',(94.0160964783391,22.4854399019793,1.78487540707101));
#19405=CARTESIAN_POINT('Ctrl Pts',(94.5141839820761,23.1484740991037,1.83753646215389));
#19406=CARTESIAN_POINT('Ctrl Pts',(94.65323634715,24.0812683528445,1.89019751723676));
#19407=CARTESIAN_POINT('Ctrl Pts',(94.3701624990711,24.8607544964156,1.94285857231964));
#19408=CARTESIAN_POINT('Ctrl Pts',(94.0870886509922,25.6402406399868,1.99551962740252));
#19409=CARTESIAN_POINT('Ctrl Pts',(93.3818885897606,26.2664186733884,2.0481806824854));
#19410=CARTESIAN_POINT('Ctrl Pts',(92.5743965080578,26.4553208851494,2.10084173756828));
#19411=CARTESIAN_POINT('Ctrl Pts',(91.766904426355,26.6442230969105,2.15350279265116));
#19412=CARTESIAN_POINT('Ctrl Pts',(90.857120324181,26.3958494870309,2.20616384773403));
#19413=CARTESIAN_POINT('Ctrl Pts',(90.2576399987561,25.8228345233925,2.25882490281691));
#19414=CARTESIAN_POINT('Ctrl Pts',(89.7696876855645,25.3564239255092,2.30168883438061));
#19415=CARTESIAN_POINT('Ctrl Pts',(89.4873206236216,24.6749290158026,2.34455276594432));
#19416=CARTESIAN_POINT('Ctrl Pts',(89.4812641621455,23.9978903848741,2.38741669750802));
#19417=CARTESIAN_POINT('Origin',(92.,24.,5.));
#19418=CARTESIAN_POINT('',(89.4802712114252,24.0018289507128,3.38741669750802));
#19419=CARTESIAN_POINT('',(89.4854088326162,24.0015585716341,3.11258330249198));
#19420=CARTESIAN_POINT('',(89.4825,24.,5.));
#19421=CARTESIAN_POINT('Ctrl Pts',(89.4854088326162,24.0015585716341,3.11258330249198));
#19422=CARTESIAN_POINT('Ctrl Pts',(89.4836296984461,24.3124536014081,3.09298258440541));
#19423=CARTESIAN_POINT('Ctrl Pts',(89.5370773572355,24.6227586333045,3.07338186631883));
#19424=CARTESIAN_POINT('Ctrl Pts',(89.6485419638298,24.9105966710309,3.05378114823225));
#19425=CARTESIAN_POINT('Ctrl Pts',(89.9480128179958,25.6839282751438,3.00112009314937));
#19426=CARTESIAN_POINT('Ctrl Pts',(90.6662676183469,26.2950862932019,2.94845903806649));
#19427=CARTESIAN_POINT('Ctrl Pts',(91.4775657352138,26.466901288493,2.89579798298361));
#19428=CARTESIAN_POINT('Ctrl Pts',(92.2888638520807,26.638716283784,2.84313692790074));
#19429=CARTESIAN_POINT('Ctrl Pts',(93.1932052854633,26.371188256308,2.79047587281786));
#19430=CARTESIAN_POINT('Ctrl Pts',(93.7804553940471,25.7856433745947,2.73781481773498));
#19431=CARTESIAN_POINT('Ctrl Pts',(94.3677055026309,25.2000984928813,2.6851537626521));
#19432=CARTESIAN_POINT('Ctrl Pts',(94.6378642864158,24.2965367569306,2.63249270756922));
#19433=CARTESIAN_POINT('Ctrl Pts',(94.4684108772915,23.4847436484408,2.57983165248635));
#19434=CARTESIAN_POINT('Ctrl Pts',(94.2989574681671,22.672950539951,2.52717059740347));
#19435=CARTESIAN_POINT('Ctrl Pts',(93.6898918661335,21.952926058922,2.47450954232059));
#19436=CARTESIAN_POINT('Ctrl Pts',(92.9174341827593,21.6512037648828,2.42184848723771));
#19437=CARTESIAN_POINT('Ctrl Pts',(92.1449764993851,21.3494814708436,2.36918743215483));
#19438=CARTESIAN_POINT('Ctrl Pts',(91.2091267346702,21.4660613637942,2.31652637707196));
#19439=CARTESIAN_POINT('Ctrl Pts',(90.5343118592194,21.9480925468641,2.26386532198908));
#19440=CARTESIAN_POINT('Ctrl Pts',(89.8881204945621,22.4096774930868,2.21343798215671));
#19441=CARTESIAN_POINT('Ctrl Pts',(89.4812891226481,23.2063686712678,2.16301064232435));
#19442=CARTESIAN_POINT('Ctrl Pts',(89.4785876236681,24.0006455599548,2.11258330249198));
#19443=CARTESIAN_POINT('Ctrl Pts',(89.4812641621455,23.9978903848741,2.38741669750802));
#19444=CARTESIAN_POINT('Ctrl Pts',(89.47987987706,23.8431441716248,2.3972138210272));
#19445=CARTESIAN_POINT('Ctrl Pts',(89.4929303898819,23.6886307597355,2.40701094454637));
#19446=CARTESIAN_POINT('Ctrl Pts',(89.5212601912555,23.5369715569028,2.41680806806555));
#19447=CARTESIAN_POINT('Ctrl Pts',(89.6735372578558,22.7217798714484,2.46946912314842));
#19448=CARTESIAN_POINT('Ctrl Pts',(90.2672679397321,21.9890528179368,2.5221301782313));
#19449=CARTESIAN_POINT('Ctrl Pts',(91.0331836055545,21.6710928935685,2.57479123331418));
#19450=CARTESIAN_POINT('Ctrl Pts',(91.7990992713769,21.3531329692002,2.62745228839706));
#19451=CARTESIAN_POINT('Ctrl Pts',(92.7371999211453,21.4499401739753,2.68011334347994));
#19452=CARTESIAN_POINT('Ctrl Pts',(93.4220417006604,21.9176116335595,2.73277439856282));
#19453=CARTESIAN_POINT('Ctrl Pts',(94.1068834801755,22.3852830931437,2.78543545364569));
#19454=CARTESIAN_POINT('Ctrl Pts',(94.5384663894373,23.2238188075369,2.83809650872857));
#19455=CARTESIAN_POINT('Ctrl Pts',(94.5210598219411,24.052928105998,2.89075756381145));
#19456=CARTESIAN_POINT('Ctrl Pts',(94.5036532544448,24.8820374044591,2.94341861889433));
#19457=CARTESIAN_POINT('Ctrl Pts',(94.0372572101906,25.701720286988,2.99607967397721));
#19458=CARTESIAN_POINT('Ctrl Pts',(93.3333904465718,26.1402367801488,3.04874072906008));
#19459=CARTESIAN_POINT('Ctrl Pts',(92.629523682953,26.5787532733095,3.10140178414296));
#19460=CARTESIAN_POINT('Ctrl Pts',(91.6881861999696,26.636103377102,3.15406283922584));
#19461=CARTESIAN_POINT('Ctrl Pts',(90.9362905172017,26.2862777415508,3.20672389430872));
#19462=CARTESIAN_POINT('Ctrl Pts',(90.1843948344338,25.9364521059997,3.2593849493916));
#19463=CARTESIAN_POINT('Ctrl Pts',(89.6219409518814,25.1794507311049,3.31204600447447));
#19464=CARTESIAN_POINT('Ctrl Pts',(89.5040113501232,24.3585867079682,3.36470705955735));
#19465=CARTESIAN_POINT('Ctrl Pts',(89.4870592998501,24.2405898015078,3.37227693887424));
#19466=CARTESIAN_POINT('Ctrl Pts',(89.4792925695015,24.1212732846669,3.37984681819113));
#19467=CARTESIAN_POINT('Ctrl Pts',(89.4802712114252,24.0018289507128,3.38741669750802));
#19468=CARTESIAN_POINT('Origin',(92.,24.,5.));
#19469=CARTESIAN_POINT('',(89.4864157451591,24.0003542166096,4.38741669750802));
#19470=CARTESIAN_POINT('',(89.4839748093507,23.9978936309447,4.11258330249198));
#19471=CARTESIAN_POINT('',(89.4825,24.,5.));
#19472=CARTESIAN_POINT('Ctrl Pts',(89.4839748093507,23.9978936309447,4.11258330249198));
#19473=CARTESIAN_POINT('Ctrl Pts',(89.4886914413751,24.5834107418753,4.07561558156934));
#19474=CARTESIAN_POINT('Ctrl Pts',(89.6925942792401,25.1718904338737,4.0386478606467));
#19475=CARTESIAN_POINT('Ctrl Pts',(90.0662148873616,25.6183374708836,4.00168013972405));
#19476=CARTESIAN_POINT('Ctrl Pts',(90.5984428671593,26.2543077557916,3.94901908464118));
#19477=CARTESIAN_POINT('Ctrl Pts',(91.475069207756,26.6020594676883,3.8963580295583));
#19478=CARTESIAN_POINT('Ctrl Pts',(92.2985289056069,26.5038812863978,3.84369697447542));
#19479=CARTESIAN_POINT('Ctrl Pts',(93.1219886034578,26.4057031051072,3.79103591939255));
#19480=CARTESIAN_POINT('Ctrl Pts',(93.8922816585628,25.8615950306292,3.73837486430966));
#19481=CARTESIAN_POINT('Ctrl Pts',(94.2600670194833,25.1183193280089,3.68571380922678));
#19482=CARTESIAN_POINT('Ctrl Pts',(94.6278523804038,24.3750436253885,3.63305275414391));
#19483=CARTESIAN_POINT('Ctrl Pts',(94.5931300471397,23.4326002946258,3.58039169906103));
#19484=CARTESIAN_POINT('Ctrl Pts',(94.1716472007572,22.7184035364296,3.52773064397815));
#19485=CARTESIAN_POINT('Ctrl Pts',(93.7501643543746,22.0042067782334,3.47506958889527));
#19486=CARTESIAN_POINT('Ctrl Pts',(92.9419209948736,21.5182565926037,3.4224085338124));
#19487=CARTESIAN_POINT('Ctrl Pts',(92.113469258178,21.4809395463903,3.36974747872952));
#19488=CARTESIAN_POINT('Ctrl Pts',(91.2850175214825,21.4436225001769,3.31708642364664));
#19489=CARTESIAN_POINT('Ctrl Pts',(90.4363574075924,21.8549385933799,3.26442536856376));
#19490=CARTESIAN_POINT('Ctrl Pts',(89.9523708046377,22.5283492350652,3.21176431348088));
#19491=CARTESIAN_POINT('Ctrl Pts',(89.648526527872,22.9511129399696,3.17870397648458));
#19492=CARTESIAN_POINT('Ctrl Pts',(89.4884096805934,23.4771750052054,3.14564363948828));
#19493=CARTESIAN_POINT('Ctrl Pts',(89.4854088326162,24.0015585716341,3.11258330249198));
#19494=CARTESIAN_POINT('Ctrl Pts',(89.4802712114252,24.0018289507128,3.38741669750802));
#19495=CARTESIAN_POINT('Ctrl Pts',(89.4861006458386,23.2903400047058,3.43250787327401));
#19496=CARTESIAN_POINT('Ctrl Pts',(89.8022313189484,22.5743158820022,3.47759904904));
#19497=CARTESIAN_POINT('Ctrl Pts',(90.335679104099,22.105645314345,3.52269022480599));
#19498=CARTESIAN_POINT('Ctrl Pts',(90.9586817807967,21.5582946152368,3.57535127988887));
#19499=CARTESIAN_POINT('Ctrl Pts',(91.8780924551559,21.3483198883991,3.62801233497174));
#19500=CARTESIAN_POINT('Ctrl Pts',(92.6769427066419,21.5709482675317,3.68067339005462));
#19501=CARTESIAN_POINT('Ctrl Pts',(93.475792958128,21.7935766466644,3.7333344451375));
#19502=CARTESIAN_POINT('Ctrl Pts',(94.1540827867411,22.4488081317675,3.78599550022038));
#19503=CARTESIAN_POINT('Ctrl Pts',(94.4041961740691,23.2394840564229,3.83865655530326));
#19504=CARTESIAN_POINT('Ctrl Pts',(94.6543095613971,24.0301599810783,3.89131761038613));
#19505=CARTESIAN_POINT('Ctrl Pts',(94.4762465074402,24.9562803452861,3.94397866546901));
#19506=CARTESIAN_POINT('Ctrl Pts',(93.9507616486448,25.59783376143,3.99663972055189));
#19507=CARTESIAN_POINT('Ctrl Pts',(93.4252767898494,26.2393871775739,4.04930077563477));
#19508=CARTESIAN_POINT('Ctrl Pts',(92.5523701262155,26.596373645654,4.10196183071765));
#19509=CARTESIAN_POINT('Ctrl Pts',(91.7279197254964,26.5068937086739,4.15462288580053));
#19510=CARTESIAN_POINT('Ctrl Pts',(90.9034693247774,26.4174137716938,4.2072839408834));
#19511=CARTESIAN_POINT('Ctrl Pts',(90.1274751869731,25.8814674296536,4.25994499596628));
#19512=CARTESIAN_POINT('Ctrl Pts',(89.7518638973824,25.1421154958357,4.31260605104916));
#19513=CARTESIAN_POINT('Ctrl Pts',(89.5739985954225,24.7920060646031,4.33754293320211));
#19514=CARTESIAN_POINT('Ctrl Pts',(89.4859135120177,24.3962857922303,4.36247981535507));
#19515=CARTESIAN_POINT('Ctrl Pts',(89.4864157451591,24.0003542166096,4.38741669750802));
#19516=CARTESIAN_POINT('Origin',(92.,24.,5.));
#19517=CARTESIAN_POINT('',(89.4815253774702,23.997843907913,5.38741669750803));
#19518=CARTESIAN_POINT('',(89.4784999401586,24.000477759641,5.11258330249198));
#19519=CARTESIAN_POINT('',(89.4825,24.,5.));
#19520=CARTESIAN_POINT('Ctrl Pts',(89.4784999401586,24.000477759641,5.11258330249198));
#19521=CARTESIAN_POINT('Ctrl Pts',(89.4784306610618,24.0268374600631,5.11090963381615));
#19522=CARTESIAN_POINT('Ctrl Pts',(89.478808621275,24.0531951260583,5.10923596514032));
#19523=CARTESIAN_POINT('Ctrl Pts',(89.4796399750106,24.0795384836878,5.1075622964645));
#19524=CARTESIAN_POINT('Ctrl Pts',(89.5057980584424,24.9084175965175,5.05490124138162));
#19525=CARTESIAN_POINT('Ctrl Pts',(89.9808208362983,25.7231312660314,5.00224018629874));
#19526=CARTESIAN_POINT('Ctrl Pts',(90.6892773720313,26.1541929390351,4.94957913121586));
#19527=CARTESIAN_POINT('Ctrl Pts',(91.3977339077644,26.5852546120388,4.89691807613298));
#19528=CARTESIAN_POINT('Ctrl Pts',(92.3396242013746,26.6326642885323,4.84425702105011));
#19529=CARTESIAN_POINT('Ctrl Pts',(93.0877849303764,26.2749208713486,4.79159596596723));
#19530=CARTESIAN_POINT('Ctrl Pts',(93.8359456593782,25.9171774541649,4.73893491088435));
#19531=CARTESIAN_POINT('Ctrl Pts',(94.3903768237715,25.1542809433041,4.68627385580147));
#19532=CARTESIAN_POINT('Ctrl Pts',(94.4996344284721,24.3322179256395,4.63361280071859));
#19533=CARTESIAN_POINT('Ctrl Pts',(94.6088920331728,23.5101549079749,4.58095174563571));
#19534=CARTESIAN_POINT('Ctrl Pts',(94.2729760781807,22.6289253835066,4.52829069055284));
#19535=CARTESIAN_POINT('Ctrl Pts',(93.6442301819934,22.0881819816233,4.47562963546996));
#19536=CARTESIAN_POINT('Ctrl Pts',(93.0154842858062,21.5474385797399,4.42296858038708));
#19537=CARTESIAN_POINT('Ctrl Pts',(92.0939084484237,21.3471813004415,4.3703075253042));
#19538=CARTESIAN_POINT('Ctrl Pts',(91.2974530394867,21.5782302356247,4.31764647022133));
#19539=CARTESIAN_POINT('Ctrl Pts',(90.5009976305497,21.8092791708079,4.26498541513845));
#19540=CARTESIAN_POINT('Ctrl Pts',(89.8296626500582,22.4716343204727,4.21232436005557));
#19541=CARTESIAN_POINT('Ctrl Pts',(89.5879099693118,23.2649063242647,4.15966330497269));
#19542=CARTESIAN_POINT('Ctrl Pts',(89.5158661107693,23.5013064992303,4.14396997081245));
#19543=CARTESIAN_POINT('Ctrl Pts',(89.481972530589,23.749333117907,4.12827663665222));
#19544=CARTESIAN_POINT('Ctrl Pts',(89.4839748093507,23.9978936309447,4.11258330249198));
#19545=CARTESIAN_POINT('Ctrl Pts',(89.4864157451591,24.0003542166096,4.38741669750802));
#19546=CARTESIAN_POINT('Ctrl Pts',(89.4869741148213,23.5601678531502,4.41514087043795));
#19547=CARTESIAN_POINT('Ctrl Pts',(89.5970300437706,23.1197203102035,4.44286504336787));
#19548=CARTESIAN_POINT('Ctrl Pts',(89.8149442483522,22.7413995457469,4.47058921629779));
#19549=CARTESIAN_POINT('Ctrl Pts',(90.22886433029,22.0227930550715,4.52325027138067));
#19550=CARTESIAN_POINT('Ctrl Pts',(91.0319329355429,21.5283375993164,4.57591132646355));
#19551=CARTESIAN_POINT('Ctrl Pts',(91.8599447465539,21.4822771662391,4.62857238154643));
#19552=CARTESIAN_POINT('Ctrl Pts',(92.6879565575648,21.4362167331619,4.68123343662931));
#19553=CARTESIAN_POINT('Ctrl Pts',(93.5409115743339,21.8385513227625,4.73389449171218));
#19554=CARTESIAN_POINT('Ctrl Pts',(94.0319801400905,22.5068153323074,4.78655554679506));
#19555=CARTESIAN_POINT('Ctrl Pts',(94.523048705847,23.1750793418523,4.83921660187794));
#19556=CARTESIAN_POINT('Ctrl Pts',(94.652230820591,24.1092727713413,4.89187765696082));
#19557=CARTESIAN_POINT('Ctrl Pts',(94.3609401906911,24.8857229575283,4.9445387120437));
#19558=CARTESIAN_POINT('Ctrl Pts',(94.0696495607912,25.6621731437152,4.99719976712658));
#19559=CARTESIAN_POINT('Ctrl Pts',(93.3578861862475,26.2808800866,5.04986082220945));
#19560=CARTESIAN_POINT('Ctrl Pts',(92.5484469044027,26.461249628667,5.10252187729233));
#19561=CARTESIAN_POINT('Ctrl Pts',(91.7390076225579,26.641619170734,5.15518293237521));
#19562=CARTESIAN_POINT('Ctrl Pts',(90.8318924334121,26.3836513119832,5.20784398745809));
#19563=CARTESIAN_POINT('Ctrl Pts',(90.2384935561441,25.8043388788684,5.26050504254097));
#19564=CARTESIAN_POINT('Ctrl Pts',(89.7618020463167,25.3389633465204,5.30280892752999));
#19565=CARTESIAN_POINT('Ctrl Pts',(89.4875608688215,24.6662147404431,5.34511281251901));
#19566=CARTESIAN_POINT('Ctrl Pts',(89.4815253774702,23.997843907913,5.38741669750803));
#19567=CARTESIAN_POINT('Origin',(92.,24.,5.));
#19568=CARTESIAN_POINT('',(89.4800390583838,24.0017354239359,6.38741669750802));
#19569=CARTESIAN_POINT('',(89.4852339904214,24.0016589574482,6.11258330249198));
#19570=CARTESIAN_POINT('',(89.4825,24.,5.));
#19571=CARTESIAN_POINT('Ctrl Pts',(89.4852339904214,24.0016589574482,6.11258330249198));
#19572=CARTESIAN_POINT('Ctrl Pts',(89.4833859739972,24.3036180412943,6.09354263098009));
#19573=CARTESIAN_POINT('Ctrl Pts',(89.5337383064255,24.6049815306727,6.0745019594682));
#19574=CARTESIAN_POINT('Ctrl Pts',(89.6390603134631,24.8857227683913,6.05546128795631));
#19575=CARTESIAN_POINT('Ctrl Pts',(89.9303508811609,25.6621727887753,6.00280023287343));
#19576=CARTESIAN_POINT('Ctrl Pts',(90.642114103715,26.2808795995417,5.95013917779054));
#19577=CARTESIAN_POINT('Ctrl Pts',(91.4515532127125,26.4612491030927,5.89747812270766));
#19578=CARTESIAN_POINT('Ctrl Pts',(92.2609923217099,26.6416186066436,5.84481706762479));
#19579=CARTESIAN_POINT('Ctrl Pts',(93.1681073171506,26.3836508029792,5.79215601254192));
#19580=CARTESIAN_POINT('Ctrl Pts',(93.7615060677044,25.8043384935705,5.73949495745904));
#19581=CARTESIAN_POINT('Ctrl Pts',(94.3549048182582,25.2250261841617,5.68683390237616));
#19582=CARTESIAN_POINT('Ctrl Pts',(94.6345873239251,24.3243693690088,5.63417284729328));
#19583=CARTESIAN_POINT('Ctrl Pts',(94.4737127953066,23.5108312844466,5.5815117922104));
#19584=CARTESIAN_POINT('Ctrl Pts',(94.3128382666882,22.6972931998845,5.52885073712752));
#19585=CARTESIAN_POINT('Ctrl Pts',(93.7114067037844,21.9708738459131,5.47618968204464));
#19586=CARTESIAN_POINT('Ctrl Pts',(92.9421775844463,21.6610167966983,5.42352862696176));
#19587=CARTESIAN_POINT('Ctrl Pts',(92.1729484651082,21.3511597474835,5.37086757187889));
#19588=CARTESIAN_POINT('Ctrl Pts',(91.2359217893358,21.4578650030252,5.31820651679601));
#19589=CARTESIAN_POINT('Ctrl Pts',(90.5560551459534,21.9327399088688,5.26554546171313));
#19590=CARTESIAN_POINT('Ctrl Pts',(89.8977959599792,22.3925223853337,5.21455807530608));
#19591=CARTESIAN_POINT('Ctrl Pts',(89.4806104893556,23.1974441303418,5.16357068889903));
#19592=CARTESIAN_POINT('Ctrl Pts',(89.4784999401586,24.000477759641,5.11258330249198));
#19593=CARTESIAN_POINT('Ctrl Pts',(89.4815253774702,23.997843907913,5.38741669750803));
#19594=CARTESIAN_POINT('Ctrl Pts',(89.4800477209726,23.8342080999941,5.39777386760188));
#19595=CARTESIAN_POINT('Ctrl Pts',(89.4946464973945,23.6708346988265,5.40813103769574));
#19596=CARTESIAN_POINT('Ctrl Pts',(89.5262866764575,23.5108311799897,5.4184882077896));
#19597=CARTESIAN_POINT('Ctrl Pts',(89.6871612394291,22.6972929217049,5.47114926287248));
#19598=CARTESIAN_POINT('Ctrl Pts',(90.2885929307624,21.9708734126142,5.52381031795536));
#19599=CARTESIAN_POINT('Ctrl Pts',(91.0578222143614,21.6610162972326,5.57647137303823));
#19600=CARTESIAN_POINT('Ctrl Pts',(91.8270514979604,21.351159181851,5.62913242812111));
#19601=CARTESIAN_POINT('Ctrl Pts',(92.7640783738252,21.4578644601784,5.68179348320399));
#19602=CARTESIAN_POINT('Ctrl Pts',(93.4439451623861,21.9327394674267,5.73445453828687));
#19603=CARTESIAN_POINT('Ctrl Pts',(94.123811950947,22.407614474675,5.78711559336975));
#19604=CARTESIAN_POINT('Ctrl Pts',(94.5465186522039,23.2506592108443,5.83977664845263));
#19605=CARTESIAN_POINT('Ctrl Pts',(94.5203605631863,24.0795385006725,5.8924377035355));
#19606=CARTESIAN_POINT('Ctrl Pts',(94.4942024741687,24.9084177905007,5.94509875861838));
#19607=CARTESIAN_POINT('Ctrl Pts',(94.0191795948766,25.7231316339878,5.99775981370126));
#19608=CARTESIAN_POINT('Ctrl Pts',(93.3107229078599,26.1541933990406,6.05042086878414));
#19609=CARTESIAN_POINT('Ctrl Pts',(92.6022662208433,26.5852551640933,6.10308192386702));
#19610=CARTESIAN_POINT('Ctrl Pts',(91.6603757261022,26.6326648507116,6.1557429789499));
#19611=CARTESIAN_POINT('Ctrl Pts',(90.9122148373384,26.274921357135,6.20840403403277));
#19612=CARTESIAN_POINT('Ctrl Pts',(90.1640539485746,25.9171778635584,6.26106508911565));
#19613=CARTESIAN_POINT('Ctrl Pts',(89.6096226657881,25.154281189787,6.31372614419853));
#19614=CARTESIAN_POINT('Ctrl Pts',(89.5003650377567,24.3322179965802,6.36638719928141));
#19615=CARTESIAN_POINT('Ctrl Pts',(89.4858215065436,24.2227912963587,6.37339703202361));
#19616=CARTESIAN_POINT('Ctrl Pts',(89.4791659526656,24.1123162318431,6.38040686476582));
#19617=CARTESIAN_POINT('Ctrl Pts',(89.4800390583838,24.0017354239359,6.38741669750802));
#19618=CARTESIAN_POINT('Origin',(92.,24.,5.));
#19619=CARTESIAN_POINT('',(89.4863706869161,24.0004946014336,7.38741669750802));
#19620=CARTESIAN_POINT('',(89.4842076940747,23.9979483279393,7.11258330249198));
#19621=CARTESIAN_POINT('',(89.4825,24.,5.));
#19622=CARTESIAN_POINT('Ctrl Pts',(89.4842076940747,23.9979483279393,7.11258330249198));
#19623=CARTESIAN_POINT('Ctrl Pts',(89.4887014564202,24.5747302879618,7.07617562814402));
#19624=CARTESIAN_POINT('Ctrl Pts',(89.6859403589103,25.1542900307673,7.03976795379607));
#19625=CARTESIAN_POINT('Ctrl Pts',(90.0492387679223,25.5978334202261,7.00336027944811));
#19626=CARTESIAN_POINT('Ctrl Pts',(90.5747235145078,26.23938669937,6.95069922436523));
#19627=CARTESIAN_POINT('Ctrl Pts',(91.4476299917373,26.5963730912254,6.89803816928235));
#19628=CARTESIAN_POINT('Ctrl Pts',(92.2720802164025,26.5068931733543,6.84537711419947));
#19629=CARTESIAN_POINT('Ctrl Pts',(93.0965304410677,26.4174132554832,6.79271605911659));
#19630=CARTESIAN_POINT('Ctrl Pts',(93.8725244131686,25.8814670278857,6.74005500403372));
#19631=CARTESIAN_POINT('Ctrl Pts',(94.248135622552,25.142115251948,6.68739394895084));
#19632=CARTESIAN_POINT('Ctrl Pts',(94.6237468319354,24.4027634760103,6.63473289386796));
#19633=CARTESIAN_POINT('Ctrl Pts',(94.5989752786014,23.4600061517323,6.58207183878508));
#19634=CARTESIAN_POINT('Ctrl Pts',(94.1850552850516,22.7413998145083,6.52941078370221));
#19635=CARTESIAN_POINT('Ctrl Pts',(93.7711352915018,22.0227934772843,6.47674972861933));
#19636=CARTESIAN_POINT('Ctrl Pts',(92.9680668577363,21.5283381271142,6.42408867353645));
#19637=CARTESIAN_POINT('Ctrl Pts',(92.1400552235388,21.4822777038725,6.37142761845357));
#19638=CARTESIAN_POINT('Ctrl Pts',(91.3120435893413,21.4362172806308,6.31876656337069));
#19639=CARTESIAN_POINT('Ctrl Pts',(90.4590887547119,21.8385517843175,6.26610550828781));
#19640=CARTESIAN_POINT('Ctrl Pts',(89.9680202938179,22.5068156511616,6.21344445320493));
#19641=CARTESIAN_POINT('Ctrl Pts',(89.6545075852539,22.9334551762256,6.17982406963395));
#19642=CARTESIAN_POINT('Ctrl Pts',(89.4884970592155,23.4684855231337,6.14620368606297));
#19643=CARTESIAN_POINT('Ctrl Pts',(89.4852339904214,24.0016589574482,6.11258330249198));
#19644=CARTESIAN_POINT('Ctrl Pts',(89.4800390583838,24.0017354239359,6.38741669750802));
#19645=CARTESIAN_POINT('Ctrl Pts',(89.4857251203391,23.2815828562451,6.4330679198487));
#19646=CARTESIAN_POINT('Ctrl Pts',(89.81071724972,22.5569454920104,6.47871914218937));
#19647=CARTESIAN_POINT('Ctrl Pts',(90.3557694668982,22.0881815733762,6.52437036453004));
#19648=CARTESIAN_POINT('Ctrl Pts',(90.9845154973476,21.5474380560208,6.57703141961292));
#19649=CARTESIAN_POINT('Ctrl Pts',(91.906091531523,21.3471807339522,6.6296924746958));
#19650=CARTESIAN_POINT('Ctrl Pts',(92.7025471105349,21.578229718477,6.68235352977867));
#19651=CARTESIAN_POINT('Ctrl Pts',(93.4990026895468,21.8092787030019,6.73501458486155));
#19652=CARTESIAN_POINT('Ctrl Pts',(94.1703378133953,22.4716339941201,6.78767563994444));
#19653=CARTESIAN_POINT('Ctrl Pts',(94.4120905457653,23.2649061673003,6.84033669502731));
#19654=CARTESIAN_POINT('Ctrl Pts',(94.6538432781353,24.0581783404805,6.89299775011019));
#19655=CARTESIAN_POINT('Ctrl Pts',(94.4660136190268,24.9823673957227,6.94565880519307));
#19656=CARTESIAN_POINT('Ctrl Pts',(93.9337855255779,25.6183378164487,6.99831986027595));
#19657=CARTESIAN_POINT('Ctrl Pts',(93.401557432129,26.2543082371747,7.05098091535882));
#19658=CARTESIAN_POINT('Ctrl Pts',(92.5249309043398,26.6020600233844,7.1036419704417));
#19659=CARTESIAN_POINT('Ctrl Pts',(91.7014710306461,26.5038818211034,7.15630302552458));
#19660=CARTESIAN_POINT('Ctrl Pts',(90.8780111569526,26.4057036188225,7.20896408060746));
#19661=CARTESIAN_POINT('Ctrl Pts',(90.1077179373546,25.8615954280509,7.26162513569034));
#19662=CARTESIAN_POINT('Ctrl Pts',(89.7399324979007,25.1183195667607,7.31428619077322));
#19663=CARTESIAN_POINT('Ctrl Pts',(89.5696843862451,24.7742567022501,7.33866302635148));
#19664=CARTESIAN_POINT('Ctrl Pts',(89.4856844315082,24.3875167881334,7.36303986192975));
#19665=CARTESIAN_POINT('Ctrl Pts',(89.4863706869161,24.0004946014336,7.38741669750802));
#19666=CARTESIAN_POINT('Origin',(92.,24.,5.));
#19667=CARTESIAN_POINT('',(89.481789046694,23.9978055657336,8.38741669750803));
#19668=CARTESIAN_POINT('',(89.4784369335473,24.0003195913806,8.11258330249199));
#19669=CARTESIAN_POINT('',(89.4825,24.,5.));
#19670=CARTESIAN_POINT('Ctrl Pts',(89.4784369335473,24.0003195913806,8.11258330249199));
#19671=CARTESIAN_POINT('Ctrl Pts',(89.4784053094568,24.0178575771478,8.11146968039084));
#19672=CARTESIAN_POINT('Ctrl Pts',(89.4785726200148,24.0353949438105,8.1103560582897));
#19673=CARTESIAN_POINT('Ctrl Pts',(89.4789407162088,24.0529280950311,8.10924243618855));
#19674=CARTESIAN_POINT('Ctrl Pts',(89.4963472798269,24.8820372167501,8.05658138110567));
#19675=CARTESIAN_POINT('Ctrl Pts',(89.9627432248613,25.7017199235892,8.00392032602279));
#19676=CARTESIAN_POINT('Ctrl Pts',(90.6666098382641,26.1402363229507,7.95125927093991));
#19677=CARTESIAN_POINT('Ctrl Pts',(91.3704764516668,26.5787527223122,7.89859821585703));
#19678=CARTESIAN_POINT('Ctrl Pts',(92.3118137334378,26.6361028141961,7.84593716077416));
#19679=CARTESIAN_POINT('Ctrl Pts',(93.0637092555993,26.2862772534286,7.79327610569129));
#19680=CARTESIAN_POINT('Ctrl Pts',(93.8156047777607,25.9364516926611,7.74061505060841));
#19681=CARTESIAN_POINT('Ctrl Pts',(94.3780585403126,25.1794504792422,7.68795399552552));
#19682=CARTESIAN_POINT('Ctrl Pts',(94.495988116913,24.3585866313503,7.63529294044264));
#19683=CARTESIAN_POINT('Ctrl Pts',(94.6139176935135,23.5377227834583,7.58263188535976));
#19684=CARTESIAN_POINT('Ctrl Pts',(94.2873230841625,22.6529963010933,7.52997083027689));
#19685=CARTESIAN_POINT('Ctrl Pts',(93.6643205404874,22.105645718888,7.47730977519401));
#19686=CARTESIAN_POINT('Ctrl Pts',(93.0413179968122,21.5582951366827,7.42464872011114));
#19687=CARTESIAN_POINT('Ctrl Pts',(92.1219075188129,21.3483204546372,7.37198766502826));
#19688=CARTESIAN_POINT('Ctrl Pts',(91.32305743792,21.5709487862187,7.31932660994538));
#19689=CARTESIAN_POINT('Ctrl Pts',(90.524207357027,21.7935771178002,7.2666655548625));
#19690=CARTESIAN_POINT('Ctrl Pts',(89.8459176732405,22.4488084630088,7.21400449977962));
#19691=CARTESIAN_POINT('Ctrl Pts',(89.595804339318,23.2394842188293,7.16134344469674));
#19692=CARTESIAN_POINT('Ctrl Pts',(89.5186090146758,23.4835194755668,7.14509006396182));
#19693=CARTESIAN_POINT('Ctrl Pts',(89.4822015557634,23.740457099368,7.1288366832269));
#19694=CARTESIAN_POINT('Ctrl Pts',(89.4842076940747,23.9979483279393,7.11258330249198));
#19695=CARTESIAN_POINT('Ctrl Pts',(89.4863706869161,24.0004946014336,7.38741669750802));
#19696=CARTESIAN_POINT('Ctrl Pts',(89.4871669427931,23.5514362957882,7.41570091701263));
#19697=CARTESIAN_POINT('Ctrl Pts',(89.6019741159521,23.1019979736551,7.44398513651724));
#19698=CARTESIAN_POINT('Ctrl Pts',(89.828352335515,22.7184032628621,7.47226935602185));
#19699=CARTESIAN_POINT('Ctrl Pts',(90.249835271893,22.0042063520624,7.52493041110472));
#19700=CARTESIAN_POINT('Ctrl Pts',(91.058078803959,21.5182560622716,7.5775914661876));
#19701=CARTESIAN_POINT('Ctrl Pts',(91.8865307175797,21.4809390082697,7.63025252127048));
#19702=CARTESIAN_POINT('Ctrl Pts',(92.7149826312004,21.4436219542678,7.68291357635336));
#19703=CARTESIAN_POINT('Ctrl Pts',(93.5636429263759,21.8549381360548,7.73557463143624));
#19704=CARTESIAN_POINT('Ctrl Pts',(94.0476296326406,22.5283489211969,7.78823568651912));
#19705=CARTESIAN_POINT('Ctrl Pts',(94.5316163389053,23.2017597063389,7.840896741602));
#19706=CARTESIAN_POINT('Ctrl Pts',(94.6509294562594,24.1372650948361,7.89355779668487));
#19707=CARTESIAN_POINT('Ctrl Pts',(94.3514585382347,24.910596864736,7.94621885176775));
#19708=CARTESIAN_POINT('Ctrl Pts',(94.05198762021,25.6839286346359,7.99887990685063));
#19709=CARTESIAN_POINT('Ctrl Pts',(93.3337326668065,26.2950867859384,8.05154096193351));
#19710=CARTESIAN_POINT('Ctrl Pts',(92.5224343764949,26.4669018166948,8.10420201701639));
#19711=CARTESIAN_POINT('Ctrl Pts',(91.7111360861833,26.6387168474511,8.15686307209927));
#19712=CARTESIAN_POINT('Ctrl Pts',(90.8067944589634,26.3711887576613,8.20952412718214));
#19713=CARTESIAN_POINT('Ctrl Pts',(90.2195442254209,25.7856437531992,8.26218518226502));
#19714=CARTESIAN_POINT('Ctrl Pts',(89.7540374326078,25.3214886766988,8.30392902067936));
#19715=CARTESIAN_POINT('Ctrl Pts',(89.4877768657504,24.6575058177296,8.34567285909369));
#19716=CARTESIAN_POINT('Ctrl Pts',(89.481789046694,23.9978055657336,8.38741669750803));
#19717=CARTESIAN_POINT('Origin',(92.,24.,5.));
#19718=CARTESIAN_POINT('',(89.4798237559162,24.0015869167785,9.38741669750802));
#19719=CARTESIAN_POINT('',(89.4850510509789,24.0017493960693,9.11258330249199));
#19720=CARTESIAN_POINT('',(89.4825,24.,5.));
#19721=CARTESIAN_POINT('',(93.9134659966651,25.6359872033749,10.));
#19722=CARTESIAN_POINT('Ctrl Pts',(89.4798237559162,24.0015869167785,9.38741669750802));
#19723=CARTESIAN_POINT('Ctrl Pts',(89.4853060534862,23.272907237615,9.43362796642338));
#19724=CARTESIAN_POINT('Ctrl Pts',(89.8192670107975,22.5399678433785,9.47983923533874));
#19725=CARTESIAN_POINT('Ctrl Pts',(90.3760117641787,22.0711228370539,9.5260505042541));
#19726=CARTESIAN_POINT('Ctrl Pts',(91.0104623389641,21.5368403279841,9.57871155933698));
#19727=CARTESIAN_POINT('Ctrl Pts',(91.9342252311205,21.3455170498785,9.63137261441985));
#19728=CARTESIAN_POINT('Ctrl Pts',(92.7281294273515,21.5853893188973,9.68403366950273));
#19729=CARTESIAN_POINT('Ctrl Pts',(93.5220336235825,21.8252615879162,9.73669472458561));
#19730=CARTESIAN_POINT('Ctrl Pts',(94.1860791238883,22.4963294040593,9.78935577966849));
#19731=CARTESIAN_POINT('Ctrl Pts',(94.4192657381557,23.2907292988926,9.84201683475137));
#19732=CARTESIAN_POINT('Ctrl Pts',(94.6524523524231,24.0851291937258,9.89467788983425));
#19733=CARTESIAN_POINT('Ctrl Pts',(94.4547800806522,25.0028611672492,9.94733894491712));
#19734=CARTESIAN_POINT('Ctrl Pts',(93.9134659966651,25.6359872033749,10.));
#19735=CARTESIAN_POINT('',(90.0828969142745,25.6385343069379,10.));
#19736=CARTESIAN_POINT('Origin',(92.,24.,10.));
#19737=CARTESIAN_POINT('Ctrl Pts',(90.0828884583321,25.6385402287508,10.));
#19738=CARTESIAN_POINT('Ctrl Pts',(90.6060432359258,26.2476961579692,9.94901908464118));
#19739=CARTESIAN_POINT('Ctrl Pts',(91.4465813967719,26.5878273311312,9.89803816928235));
#19740=CARTESIAN_POINT('Ctrl Pts',(92.2457357659029,26.5094848424925,9.84705725392353));
#19741=CARTESIAN_POINT('Ctrl Pts',(93.0712272651497,26.4285604793168,9.79439619884065));
#19742=CARTESIAN_POINT('Ctrl Pts',(93.8525623160909,25.9011252999797,9.74173514375777));
#19743=CARTESIAN_POINT('Ctrl Pts',(94.2358877550497,25.1658537096528,9.68907408867489));
#19744=CARTESIAN_POINT('Ctrl Pts',(94.6192131940086,24.4305821193258,9.63641303359201));
#19745=CARTESIAN_POINT('Ctrl Pts',(94.6045290209851,23.487474118009,9.58375197850914));
#19746=CARTESIAN_POINT('Ctrl Pts',(94.1982521612179,22.7645021442661,9.53109092342626));
#19747=CARTESIAN_POINT('Ctrl Pts',(93.7919753014507,22.0415301705231,9.47842986834338));
#19748=CARTESIAN_POINT('Ctrl Pts',(92.9941057549398,21.5386942243541,9.4257688132605));
#19749=CARTESIAN_POINT('Ctrl Pts',(92.1666097685102,21.4839132228271,9.37310775817762));
#19750=CARTESIAN_POINT('Ctrl Pts',(91.3391137820805,21.4291322213001,9.32044670309475));
#19751=CARTESIAN_POINT('Ctrl Pts',(90.4819913557323,21.8224061644151,9.26778564801188));
#19752=CARTESIAN_POINT('Ctrl Pts',(89.983903964328,22.4854401936109,9.215124592929));
#19753=CARTESIAN_POINT('Ctrl Pts',(89.6606130378258,22.9157921545326,9.18094416278333));
#19754=CARTESIAN_POINT('Ctrl Pts',(89.4885781648624,23.4597899774222,9.14676373263766));
#19755=CARTESIAN_POINT('Ctrl Pts',(89.4850510509789,24.0017493960693,9.11258330249199));
#19756=CARTESIAN_POINT('Origin',(92.,24.,12.2084234471775));
#19757=CARTESIAN_POINT('',(88.9217235596202,24.0007881344672,1.79157655282254));
#19758=CARTESIAN_POINT('',(88.9313886636577,24.0003347861522,1.70842344717745));
#19759=CARTESIAN_POINT('',(88.9265,24.0000000000001,12.2084234471775));
#19760=CARTESIAN_POINT('',(92.7937992825328,21.0307770462543,0.999999999999999));
#19761=CARTESIAN_POINT('Ctrl Pts',(88.9313886636577,24.0003347861522,1.70842344717745));
#19762=CARTESIAN_POINT('Ctrl Pts',(88.9310462111061,24.4946152436419,1.68292651844981));
#19763=CARTESIAN_POINT('Ctrl Pts',(89.2764428698256,26.0092287095088,1.6047685346393));
#19764=CARTESIAN_POINT('Ctrl Pts',(91.6460838412789,27.6088416124303,1.47394949574591));
#19765=CARTESIAN_POINT('Ctrl Pts',(94.8312245109702,26.2698537574842,1.31596633049727));
#19766=CARTESIAN_POINT('Ctrl Pts',(95.4433138069375,22.8667064664957,1.15798316524863));
#19767=CARTESIAN_POINT('Ctrl Pts',(93.7762533017603,21.2934286920664,1.05266105508288));
#19768=CARTESIAN_POINT('Ctrl Pts',(92.7937992825328,21.0307770462543,0.999999999999999));
#19769=CARTESIAN_POINT('',(91.2062007174671,21.0307770462543,1.));
#19770=CARTESIAN_POINT('Origin',(92.,24.,0.999999999999999));
#19771=CARTESIAN_POINT('Ctrl Pts',(88.9217235596202,24.0007881344672,1.79157655282254));
#19772=CARTESIAN_POINT('Ctrl Pts',(88.921577466321,24.0437415214614,1.78934283757203));
#19773=CARTESIAN_POINT('Ctrl Pts',(88.9417780704225,25.0992023014299,1.73444806723864));
#19774=CARTESIAN_POINT('Ctrl Pts',(90.1476051992024,27.1179528805983,1.62689224182238));
#19775=CARTESIAN_POINT('Ctrl Pts',(93.5990315417431,27.2555126520044,1.46890907657374));
#19776=CARTESIAN_POINT('Ctrl Pts',(95.5999506290772,24.4393708209746,1.3109259113251));
#19777=CARTESIAN_POINT('Ctrl Pts',(94.349302755893,21.2605908411106,1.15462288580053));
#19778=CARTESIAN_POINT('Ctrl Pts',(92.1519058776305,20.7745943222177,1.05098091535883));
#19779=CARTESIAN_POINT('Ctrl Pts',(91.2042984301044,21.0256873776386,1.));
#19780=CARTESIAN_POINT('Origin',(92.,24.,12.2084234471775));
#19781=CARTESIAN_POINT('',(88.9300512599983,24.0019027884479,2.79157655282254));
#19782=CARTESIAN_POINT('',(88.924991222385,23.997424467889,2.70842344717745));
#19783=CARTESIAN_POINT('',(88.9265,24.0000000000001,12.2084234471775));
#19784=CARTESIAN_POINT('Ctrl Pts',(88.924991222385,23.997424467889,2.70842344717745));
#19785=CARTESIAN_POINT('Ctrl Pts',(88.9323852777363,24.823989803404,2.66555951561375));
#19786=CARTESIAN_POINT('Ctrl Pts',(89.7006356086327,26.6781674340519,2.57003452896717));
#19787=CARTESIAN_POINT('Ctrl Pts',(92.8261379115921,27.5314383230663,2.42184848723771));
#19788=CARTESIAN_POINT('Ctrl Pts',(95.4089769044768,25.2380224116542,2.26386532198907));
#19789=CARTESIAN_POINT('Ctrl Pts',(94.8996889870333,21.8216055629487,2.10588215674044));
#19790=CARTESIAN_POINT('Ctrl Pts',(91.760424111462,20.3812146145649,1.94789899149181));
#19791=CARTESIAN_POINT('Ctrl Pts',(89.3097988736992,21.9256563753203,1.81541275497081));
#19792=CARTESIAN_POINT('Ctrl Pts',(88.9317535085566,23.473734231803,1.73558757353269));
#19793=CARTESIAN_POINT('Ctrl Pts',(88.9313886636577,24.0003347861522,1.70842344717745));
#19794=CARTESIAN_POINT('Ctrl Pts',(88.9300512599983,24.0019027884479,2.79157655282254));
#19795=CARTESIAN_POINT('Ctrl Pts',(88.9278791968914,24.3814602359197,2.77197583473597));
#19796=CARTESIAN_POINT('Ctrl Pts',(89.1684423216005,25.77811538933,2.69971406156651));
#19797=CARTESIAN_POINT('Ctrl Pts',(91.2485917195107,27.5481000558719,2.57479123331418));
#19798=CARTESIAN_POINT('Ctrl Pts',(94.5607983477153,26.5682620509694,2.41680806806555));
#19799=CARTESIAN_POINT('Ctrl Pts',(95.5502716608786,23.2589111130017,2.25882490281691));
#19800=CARTESIAN_POINT('Ctrl Pts',(93.3195310914442,20.621776762524,2.10084173756828));
#19801=CARTESIAN_POINT('Ctrl Pts',(89.9403860022537,21.0427207939439,1.94509228757016));
#19802=CARTESIAN_POINT('Ctrl Pts',(88.9250216955149,23.0310920004536,1.84200389265491));
#19803=CARTESIAN_POINT('Ctrl Pts',(88.9217235596202,24.0007881344672,1.79157655282254));
#19804=CARTESIAN_POINT('Origin',(92.,24.,12.2084234471775));
#19805=CARTESIAN_POINT('',(88.9283005269272,23.9974284308675,3.79157655282254));
#19806=CARTESIAN_POINT('',(88.9237789745047,24.0022328818336,3.70842344717745));
#19807=CARTESIAN_POINT('',(88.9265,24.0000000000001,12.2084234471775));
#19808=CARTESIAN_POINT('Ctrl Pts',(88.9237789745047,24.0022328818336,3.70842344717745));
#19809=CARTESIAN_POINT('Ctrl Pts',(88.9225841955761,24.1480569773282,3.70085356786056));
#19810=CARTESIAN_POINT('Ctrl Pts',(88.9980295686384,25.3070877047366,3.6406226334608));
#19811=CARTESIAN_POINT('Ctrl Pts',(90.47008521615,27.2883135148081,3.52773064397815));
#19812=CARTESIAN_POINT('Ctrl Pts',(93.9177921721967,27.0782652002028,3.36974747872952));
#19813=CARTESIAN_POINT('Ctrl Pts',(95.6259966314009,24.0761257688788,3.21176431348088));
#19814=CARTESIAN_POINT('Ctrl Pts',(94.0452974398027,21.0049366707405,3.05378114823225));
#19815=CARTESIAN_POINT('Ctrl Pts',(90.6094455863014,20.6503742748602,2.89579798298361));
#19816=CARTESIAN_POINT('Ctrl Pts',(89.0248750936135,22.6059034459642,2.78067874929868));
#19817=CARTESIAN_POINT('Ctrl Pts',(88.923301212371,23.808501931078,2.71822057069663));
#19818=CARTESIAN_POINT('Ctrl Pts',(88.924991222385,23.997424467889,2.70842344717745));
#19819=CARTESIAN_POINT('Ctrl Pts',(88.9283005269272,23.9974284308675,3.79157655282254));
#19820=CARTESIAN_POINT('Ctrl Pts',(88.9340588461039,24.7122593506074,3.7546088318999));
#19821=CARTESIAN_POINT('Ctrl Pts',(89.5376068210962,26.4541464677684,3.66498005589439));
#19822=CARTESIAN_POINT('Ctrl Pts',(92.4293689246723,27.6012888422859,3.52269022480599));
#19823=CARTESIAN_POINT('Ctrl Pts',(95.2506150476497,25.6084592491483,3.36470705955735));
#19824=CARTESIAN_POINT('Ctrl Pts',(95.1234423470095,22.1567020569745,3.20672389430872));
#19825=CARTESIAN_POINT('Ctrl Pts',(92.1632008787758,20.3768793413443,3.04874072906008));
#19826=CARTESIAN_POINT('Ctrl Pts',(89.4405686580063,21.6964446537072,2.91035828189803));
#19827=CARTESIAN_POINT('Ctrl Pts',(88.9337148573203,23.3617070023829,2.82463688981885));
#19828=CARTESIAN_POINT('Ctrl Pts',(88.9300512599983,24.0019027884479,2.79157655282254));
#19829=CARTESIAN_POINT('Origin',(92.,24.,12.2084234471775));
#19830=CARTESIAN_POINT('',(88.921616510855,24.0005832747793,4.79157655282255));
#19831=CARTESIAN_POINT('',(88.931280553226,24.0004324467725,4.70842344717745));
#19832=CARTESIAN_POINT('',(88.9265,24.0000000000001,12.2084234471775));
#19833=CARTESIAN_POINT('Ctrl Pts',(88.931280553226,24.0004324467725,4.70842344717745));
#19834=CARTESIAN_POINT('Ctrl Pts',(88.9306673998754,24.4838071032452,4.6834865650245));
#19835=CARTESIAN_POINT('Ctrl Pts',(89.2653045337522,25.9871569627812,4.60588862778867));
#19836=CARTESIAN_POINT('Ctrl Pts',(91.608671679144,27.6056215728149,4.47562963546996));
#19837=CARTESIAN_POINT('Ctrl Pts',(94.8057465121273,26.2981364769134,4.31764647022132));
#19838=CARTESIAN_POINT('Ctrl Pts',(95.4579134988245,22.9061631628408,4.15966330497269));
#19839=CARTESIAN_POINT('Ctrl Pts',(92.973634903104,20.506337181354,4.00168013972405));
#19840=CARTESIAN_POINT('Ctrl Pts',(89.7675876228179,21.2385332724819,3.85126685379231));
#19841=CARTESIAN_POINT('Ctrl Pts',(88.9308958629533,23.1336087406012,3.75351462294344));
#19842=CARTESIAN_POINT('Ctrl Pts',(88.9237789745047,24.0022328818336,3.70842344717745));
#19843=CARTESIAN_POINT('Ctrl Pts',(88.921616510855,24.0005832747793,4.79157655282255));
#19844=CARTESIAN_POINT('Ctrl Pts',(88.9215319311911,24.0327646210542,4.78990288414672));
#19845=CARTESIAN_POINT('Ctrl Pts',(88.9365121376522,25.0774335164314,4.73556816038801));
#19846=CARTESIAN_POINT('Ctrl Pts',(90.1148104659794,27.0983381963848,4.62857238154643));
#19847=CARTESIAN_POINT('Ctrl Pts',(93.5645421252575,27.2719790790494,4.4705892162978));
#19848=CARTESIAN_POINT('Ctrl Pts',(95.5951806759186,24.4778232584366,4.31260605104916));
#19849=CARTESIAN_POINT('Ctrl Pts',(94.3648676419543,21.2502654310841,4.15462288580052));
#19850=CARTESIAN_POINT('Ctrl Pts',(90.9895389394379,20.5168107165773,3.99663972055189));
#19851=CARTESIAN_POINT('Ctrl Pts',(89.1060882305935,22.3750682368835,3.8756242762259));
#19852=CARTESIAN_POINT('Ctrl Pts',(88.9258560368481,23.6939723288529,3.80726988698278));
#19853=CARTESIAN_POINT('Ctrl Pts',(88.9283005269272,23.9974284308675,3.79157655282254));
#19854=CARTESIAN_POINT('Origin',(92.,24.,12.2084234471775));
#19855=CARTESIAN_POINT('',(88.9298378032017,24.0020253448727,5.79157655282255));
#19856=CARTESIAN_POINT('',(88.9253101281647,23.9973677263042,5.70842344717746));
#19857=CARTESIAN_POINT('',(88.9265,24.0000000000001,12.2084234471775));
#19858=CARTESIAN_POINT('Ctrl Pts',(88.9253101281647,23.9973677263042,5.70842344717746));
#19859=CARTESIAN_POINT('Ctrl Pts',(88.9326785820548,24.8133509452838,5.66611956218844));
#19860=CARTESIAN_POINT('Ctrl Pts',(89.6842659096931,26.6570905748761,5.57115462211654));
#19861=CARTESIAN_POINT('Ctrl Pts',(92.7888216332755,27.5399724866421,5.42352862696176));
#19862=CARTESIAN_POINT('Ctrl Pts',(95.3956991685213,25.2739199079453,5.26554546171313));
#19863=CARTESIAN_POINT('Ctrl Pts',(94.9225616555133,21.8523784912208,5.1075622964645));
#19864=CARTESIAN_POINT('Ctrl Pts',(91.798560967482,20.3788030856943,4.94957913121586));
#19865=CARTESIAN_POINT('Ctrl Pts',(89.3215406064417,21.9039233849086,4.81653284812018));
#19866=CARTESIAN_POINT('Ctrl Pts',(88.9319622410737,23.4630291545808,4.73614762010738));
#19867=CARTESIAN_POINT('Ctrl Pts',(88.931280553226,24.0004324467725,4.70842344717745));
#19868=CARTESIAN_POINT('Ctrl Pts',(88.9298378032017,24.0020253448727,5.79157655282255));
#19869=CARTESIAN_POINT('Ctrl Pts',(88.9275816449177,24.3706733068195,5.77253588131065));
#19870=CARTESIAN_POINT('Ctrl Pts',(89.15907081827,25.7561579838992,5.70083415471588));
#19871=CARTESIAN_POINT('Ctrl Pts',(91.2111785351691,27.5399717307178,5.57647137303823));
#19872=CARTESIAN_POINT('Ctrl Pts',(94.533543506554,26.5951486388853,5.41848820778961));
#19873=CARTESIAN_POINT('Ctrl Pts',(95.5578980422049,23.2964371536349,5.26050504254096));
#19874=CARTESIAN_POINT('Ctrl Pts',(93.3551176148942,20.6358811841045,5.10252187729233));
#19875=CARTESIAN_POINT('Ctrl Pts',(89.9595568927723,21.0225555274606,4.94621238071953));
#19876=CARTESIAN_POINT('Ctrl Pts',(88.9241931833305,23.0201964387709,4.8425639392296));
#19877=CARTESIAN_POINT('Ctrl Pts',(88.921616510855,24.0005832747793,4.79157655282255));
#19878=CARTESIAN_POINT('Origin',(92.,24.,12.2084234471775));
#19879=CARTESIAN_POINT('',(88.9285848451792,23.9974952079132,6.79157655282255));
#19880=CARTESIAN_POINT('',(88.9234955495304,24.0021186992918,6.70842344717746));
#19881=CARTESIAN_POINT('',(88.9265,24.0000000000001,12.2084234471775));
#19882=CARTESIAN_POINT('Ctrl Pts',(88.9234955495304,24.0021186992919,6.70842344717746));
#19883=CARTESIAN_POINT('Ctrl Pts',(88.9224296149029,24.1371217233644,6.70141361443525));
#19884=CARTESIAN_POINT('Ctrl Pts',(88.9915972274955,25.2852299955925,6.64174272661017));
#19885=CARTESIAN_POINT('Ctrl Pts',(90.4354575406507,27.2719797777491,6.5294107837022));
#19886=CARTESIAN_POINT('Ctrl Pts',(93.8851899365835,27.0983388580017,6.37142761845357));
#19887=CARTESIAN_POINT('Ctrl Pts',(95.624990714543,24.1143988405745,6.21344445320494));
#19888=CARTESIAN_POINT('Ctrl Pts',(94.0768011856692,21.0266951703267,6.0554612879563));
#19889=CARTESIAN_POINT('Ctrl Pts',(90.6448820957342,20.6358804657318,5.89747812270767));
#19890=CARTESIAN_POINT('Ctrl Pts',(89.031950056972,22.5840074378852,5.78179884244805));
#19891=CARTESIAN_POINT('Ctrl Pts',(88.9235061252867,23.7975922920882,5.71878061727132));
#19892=CARTESIAN_POINT('Ctrl Pts',(88.9253101281647,23.9973677263042,5.70842344717746));
#19893=CARTESIAN_POINT('Ctrl Pts',(88.9285848451792,23.9974952079132,6.79157655282255));
#19894=CARTESIAN_POINT('Ctrl Pts',(88.934071073012,24.7016617835355,6.75516887847459));
#19895=CARTESIAN_POINT('Ctrl Pts',(89.523170546697,26.4326506257241,6.66610014904376));
#19896=CARTESIAN_POINT('Ctrl Pts',(92.3913282372869,27.6056208028793,6.52437036453004));
#19897=CARTESIAN_POINT('Ctrl Pts',(95.2334543225921,25.6426844805108,6.36638719928141));
#19898=CARTESIAN_POINT('Ctrl Pts',(95.1427269710462,22.1897772675992,6.20840403403277));
#19899=CARTESIAN_POINT('Ctrl Pts',(92.2014389895034,20.3788038589624,6.05042086878414));
#19900=CARTESIAN_POINT('Ctrl Pts',(89.453954137816,21.6747786389991,5.9114783750474));
#19901=CARTESIAN_POINT('Ctrl Pts',(88.9338215338625,23.3510984132479,5.82519693639353));
#19902=CARTESIAN_POINT('Ctrl Pts',(88.9298378032017,24.0020253448727,5.79157655282255));
#19903=CARTESIAN_POINT('Origin',(92.,24.,12.2084234471775));
#19904=CARTESIAN_POINT('',(88.9215395889802,24.0003901744224,7.79157655282255));
#19905=CARTESIAN_POINT('',(88.9312255436889,24.0006038361494,7.70842344717745));
#19906=CARTESIAN_POINT('',(88.9265,24.0000000000001,12.2084234471775));
#19907=CARTESIAN_POINT('Ctrl Pts',(88.9312255436888,24.0006038361494,7.70842344717745));
#19908=CARTESIAN_POINT('Ctrl Pts',(88.9303877260141,24.473101429326,7.68404661159919));
#19909=CARTESIAN_POINT('Ctrl Pts',(89.2544808710823,25.9652421749014,7.60700872093804));
#19910=CARTESIAN_POINT('Ctrl Pts',(91.5706309836454,27.601289611435,7.47730977519401));
#19911=CARTESIAN_POINT('Ctrl Pts',(94.781330049974,26.327627111039,7.31932660994538));
#19912=CARTESIAN_POINT('Ctrl Pts',(95.4692678342078,22.9427273359205,7.16134344469674));
#19913=CARTESIAN_POINT('Ctrl Pts',(93.0104612763355,20.5168099727604,7.00336027944811));
#19914=CARTESIAN_POINT('Ctrl Pts',(89.7848977769711,21.2177208955611,6.85238694694168));
#19915=CARTESIAN_POINT('Ctrl Pts',(88.9304374011369,23.122917540683,6.75407466951813));
#19916=CARTESIAN_POINT('Ctrl Pts',(88.9234955495304,24.0021186992919,6.70842344717746));
#19917=CARTESIAN_POINT('Ctrl Pts',(88.9215395889802,24.0003901744224,7.79157655282255));
#19918=CARTESIAN_POINT('Ctrl Pts',(88.9215009805821,24.0218014948814,7.79046293072141));
#19919=CARTESIAN_POINT('Ctrl Pts',(88.931364389904,25.0556766305594,7.73668825353739));
#19920=CARTESIAN_POINT('Ctrl Pts',(90.0822082378052,27.0782645420543,7.63025252127047));
#19921=CARTESIAN_POINT('Ctrl Pts',(93.5299144568995,27.2883128130434,7.47226935602186));
#19922=CARTESIAN_POINT('Ctrl Pts',(95.5899362712428,24.5157488852068,7.31428619077321));
#19923=CARTESIAN_POINT('Ctrl Pts',(94.3937632442239,21.2753832325168,7.15630302552458));
#19924=CARTESIAN_POINT('Ctrl Pts',(91.0263653048422,20.5063379273329,6.99831986027594));
#19925=CARTESIAN_POINT('Ctrl Pts',(89.1145962575176,22.3531167219238,6.87674436937527));
#19926=CARTESIAN_POINT('Ctrl Pts',(88.9261356431535,23.6831360059216,6.80782993355747));
#19927=CARTESIAN_POINT('Ctrl Pts',(88.9285848451792,23.9974952079132,6.79157655282255));
#19928=CARTESIAN_POINT('Origin',(92.,24.,12.2084234471775));
#19929=CARTESIAN_POINT('',(88.9296144608475,24.002135757227,8.79157655282255));
#19930=CARTESIAN_POINT('',(88.925632029797,23.9973209161002,8.70842344717745));
#19931=CARTESIAN_POINT('',(88.9265,24.0000000000001,12.2084234471775));
#19932=CARTESIAN_POINT('Ctrl Pts',(88.925632029797,23.9973209161002,8.70842344717745));
#19933=CARTESIAN_POINT('Ctrl Pts',(88.9329422827741,24.802718621963,8.66667960876312));
#19934=CARTESIAN_POINT('Ctrl Pts',(89.6680867896663,26.6359730058285,8.57227471526591));
#19935=CARTESIAN_POINT('Ctrl Pts',(92.7514084417654,27.5481008201034,8.42520876668582));
#19936=CARTESIAN_POINT('Ctrl Pts',(95.382061787488,25.3096961590962,8.26722560143718));
#19937=CARTESIAN_POINT('Ctrl Pts',(94.9450700899456,21.8833496110771,8.10924243618856));
#19938=CARTESIAN_POINT('Ctrl Pts',(91.8367990863051,20.3768785667209,7.95125927093992));
#19939=CARTESIAN_POINT('Ctrl Pts',(89.3333229638364,21.8820745861535,7.81765294126955));
#19940=CARTESIAN_POINT('Ctrl Pts',(88.9321976558787,23.4523691976585,7.73670766668206));
#19941=CARTESIAN_POINT('Ctrl Pts',(88.9312255436888,24.0006038361494,7.70842344717745));
#19942=CARTESIAN_POINT('Ctrl Pts',(88.9296144608475,24.002135757227,8.79157655282255));
#19943=CARTESIAN_POINT('Ctrl Pts',(88.927286249777,24.3598775143588,8.77309592788534));
#19944=CARTESIAN_POINT('Ctrl Pts',(89.1498335279143,25.734213837484,8.70195424786525));
#19945=CARTESIAN_POINT('Ctrl Pts',(91.1738622820844,27.531437528054,8.57815151276229));
#19946=CARTESIAN_POINT('Ctrl Pts',(94.5060022838614,26.6217540231211,8.42016834751365));
#19947=CARTESIAN_POINT('Ctrl Pts',(95.5651291305171,23.3340327163824,8.26218518226502));
#19948=CARTESIAN_POINT('Ctrl Pts',(93.3905541137143,20.6503749960184,8.10420201701639));
#19949=CARTESIAN_POINT('Ctrl Pts',(89.9789222863521,21.0024380002803,7.94733247386889));
#19950=CARTESIAN_POINT('Ctrl Pts',(88.9233266977404,23.0093011817766,7.84312398580429));
#19951=CARTESIAN_POINT('Ctrl Pts',(88.9215395889802,24.0003901744224,7.79157655282255));
#19952=CARTESIAN_POINT('Origin',(92.,24.,12.2084234471775));
#19953=CARTESIAN_POINT('',(88.929711085108,23.9968960951897,9.79157655282255));
#19954=CARTESIAN_POINT('',(88.9232326966468,24.0019373937314,9.70842344717745));
#19955=CARTESIAN_POINT('',(88.9265,24.0000000000001,12.2084234471775));
#19956=CARTESIAN_POINT('',(91.2062007174671,21.0307770462543,10.));
#19957=CARTESIAN_POINT('Ctrl Pts',(91.2062007174671,21.0307770462543,10.));
#19958=CARTESIAN_POINT('Ctrl Pts',(90.2237466982397,21.2934286920664,9.94733894491712));
#19959=CARTESIAN_POINT('Ctrl Pts',(89.1240892170206,22.3312175686104,9.87786446252464));
#19960=CARTESIAN_POINT('Ctrl Pts',(88.9273642764696,23.6716348903192,9.80838998013216));
#19961=CARTESIAN_POINT('Ctrl Pts',(88.929711085108,23.9968960951897,9.79157655282255));
#19962=CARTESIAN_POINT('',(92.7956975117795,21.0256988737941,10.));
#19963=CARTESIAN_POINT('Origin',(92.,24.,10.));
#19964=CARTESIAN_POINT('Ctrl Pts',(92.7957019287907,21.0256870573369,10.));
#19965=CARTESIAN_POINT('Ctrl Pts',(91.8480950072444,20.7745945181247,9.94901908464118));
#19966=CARTESIAN_POINT('Ctrl Pts',(89.7874430689301,21.2303448029462,9.851826900367));
#19967=CARTESIAN_POINT('Ctrl Pts',(88.9299257816843,23.1123258767864,9.75463471609281));
#19968=CARTESIAN_POINT('Ctrl Pts',(88.9232326966468,24.0019373937314,9.70842344717745));
#19969=CARTESIAN_POINT('Origin',(-24.,92.,5.));
#19970=CARTESIAN_POINT('',(-26.5134952662833,92.0002743405047,1.38741669750802));
#19971=CARTESIAN_POINT('',(-26.515626303127,91.9964684456989,1.11258330249198));
#19972=CARTESIAN_POINT('',(-26.5175,92.,5.));
#19973=CARTESIAN_POINT('',(-25.913465996665,93.635987203375,0.999999999999999));
#19974=CARTESIAN_POINT('Ctrl Pts',(-26.515626303127,91.9964684456989,1.11258330249198));
#19975=CARTESIAN_POINT('Ctrl Pts',(-26.5104636015443,92.5890866576526,1.07505553499465));
#19976=CARTESIAN_POINT('Ctrl Pts',(-26.299221828084,93.1848035603044,1.03752776749732));
#19977=CARTESIAN_POINT('Ctrl Pts',(-25.913465996665,93.635987203375,0.999999999999993));
#19978=CARTESIAN_POINT('',(-26.5175,92.,1.));
#19979=CARTESIAN_POINT('Origin',(-24.,92.,1.));
#19980=CARTESIAN_POINT('',(-26.5175,92.,0.));
#19981=CARTESIAN_POINT('',(-26.5175,92.,5.));
#19982=CARTESIAN_POINT('Origin',(-24.,92.,0.));
#19983=CARTESIAN_POINT('',(-22.0828968401885,93.6385343149869,1.));
#19984=CARTESIAN_POINT('Origin',(-24.,92.,1.));
#19985=CARTESIAN_POINT('Ctrl Pts',(-22.0828883826538,93.638540237813,1.));
#19986=CARTESIAN_POINT('Ctrl Pts',(-22.6060431378804,94.2476960524167,1.05098091535882));
#19987=CARTESIAN_POINT('Ctrl Pts',(-23.4465813540296,94.5878274641506,1.10196183071764));
#19988=CARTESIAN_POINT('Ctrl Pts',(-24.2457357689255,94.5094850217743,1.15294274607647));
#19989=CARTESIAN_POINT('Ctrl Pts',(-25.0712273154455,94.4285607063855,1.20560380115935));
#19990=CARTESIAN_POINT('Ctrl Pts',(-25.8525624034826,93.9011253696412,1.25826485624223));
#19991=CARTESIAN_POINT('Ctrl Pts',(-26.2358878554464,93.1658537184213,1.3109259113251));
#19992=CARTESIAN_POINT('Ctrl Pts',(-26.4214827265107,92.8098568843833,1.33642284005274));
#19993=CARTESIAN_POINT('Ctrl Pts',(-26.5137757562956,92.4051388409379,1.36191976878038));
#19994=CARTESIAN_POINT('Ctrl Pts',(-26.5134952662833,92.0002743405047,1.38741669750802));
#19995=CARTESIAN_POINT('Origin',(-24.,92.,5.));
#19996=CARTESIAN_POINT('',(-26.5187354043533,91.9978903847198,2.38741669750802));
#19997=CARTESIAN_POINT('',(-26.521412539848,92.0006455489043,2.11258330249198));
#19998=CARTESIAN_POINT('',(-26.5175,92.,5.));
#19999=CARTESIAN_POINT('Ctrl Pts',(-26.521412539848,92.0006455489043,2.11258330249198));
#20000=CARTESIAN_POINT('Ctrl Pts',(-26.5215322047965,92.0358286169429,2.11034958724147));
#20001=CARTESIAN_POINT('Ctrl Pts',(-26.5208589221676,92.0710069479233,2.10811587199095));
#20002=CARTESIAN_POINT('Ctrl Pts',(-26.5193783713,92.1061512068912,2.10588215674044));
#20003=CARTESIAN_POINT('Ctrl Pts',(-26.4844735772459,92.9346962763346,2.05322110165756));
#20004=CARTESIAN_POINT('Ctrl Pts',(-26.0008839809308,93.7443039053208,2.00056004657468));
#20005=CARTESIAN_POINT('Ctrl Pts',(-25.2879126402955,94.1678868628806,1.9478989914918));
#20006=CARTESIAN_POINT('Ctrl Pts',(-24.5749412996602,94.5914698204405,1.89523793640892));
#20007=CARTESIAN_POINT('Ctrl Pts',(-23.6325882147045,94.629028106574,1.84257688132604));
#20008=CARTESIAN_POINT('Ctrl Pts',(-22.8882532947045,94.2633575703981,1.78991582624317));
#20009=CARTESIAN_POINT('Ctrl Pts',(-22.1439183747044,93.8976870342222,1.73725477116029));
#20010=CARTESIAN_POINT('Ctrl Pts',(-21.59760161966,93.1287876757369,1.68459371607741));
#20011=CARTESIAN_POINT('Ctrl Pts',(-21.4970124750773,92.3057173952046,1.63193266099453));
#20012=CARTESIAN_POINT('Ctrl Pts',(-21.3964233304946,91.4826471146722,1.57927160591165));
#20013=CARTESIAN_POINT('Ctrl Pts',(-21.7415617963736,90.6054059120928,1.52661055082878));
#20014=CARTESIAN_POINT('Ctrl Pts',(-22.3760121357463,90.0711233584702,1.4739494957459));
#20015=CARTESIAN_POINT('Ctrl Pts',(-23.010462475119,89.5368408048476,1.42128844066302));
#20016=CARTESIAN_POINT('Ctrl Pts',(-23.9342246879853,89.3455169001818,1.36862738558014));
#20017=CARTESIAN_POINT('Ctrl Pts',(-24.7281292572936,89.5853895325345,1.31596633049726));
#20018=CARTESIAN_POINT('Ctrl Pts',(-25.5220338266019,89.8252621648871,1.26330527541438));
#20019=CARTESIAN_POINT('Ctrl Pts',(-26.1860807523522,90.4963313342582,1.21064422033151));
#20020=CARTESIAN_POINT('Ctrl Pts',(-26.4192673158648,91.2907310848487,1.15798316524863));
#20021=CARTESIAN_POINT('Ctrl Pts',(-26.4862784936919,91.5190189507993,1.14284987766308));
#20022=CARTESIAN_POINT('Ctrl Pts',(-26.5177081921649,91.7574917511602,1.12771659007753));
#20023=CARTESIAN_POINT('Ctrl Pts',(-26.515626303127,91.9964684456989,1.11258330249198));
#20024=CARTESIAN_POINT('Ctrl Pts',(-26.5134952662833,92.0002743405047,1.38741669750802));
#20025=CARTESIAN_POINT('Ctrl Pts',(-26.5131964355411,91.5689364894248,1.41458082386326));
#20026=CARTESIAN_POINT('Ctrl Pts',(-26.4078218494689,91.1374324020536,1.4417449502185));
#20027=CARTESIAN_POINT('Ctrl Pts',(-26.1982522460689,90.7645021148374,1.46890907657374));
#20028=CARTESIAN_POINT('Ctrl Pts',(-25.7919753688369,90.0415301281689,1.52157013165661));
#20029=CARTESIAN_POINT('Ctrl Pts',(-24.9941057984822,89.5386941205273,1.57423118673949));
#20030=CARTESIAN_POINT('Ctrl Pts',(-24.1666097792392,89.4839131073783,1.62689224182237));
#20031=CARTESIAN_POINT('Ctrl Pts',(-23.3391137599961,89.4291320942294,1.67955329690525));
#20032=CARTESIAN_POINT('Ctrl Pts',(-22.4819912918646,89.8224060755732,1.73221435198813));
#20033=CARTESIAN_POINT('Ctrl Pts',(-21.9839038787409,90.4854401372494,1.78487540707101));
#20034=CARTESIAN_POINT('Ctrl Pts',(-21.4858164656172,91.1484741989255,1.83753646215388));
#20035=CARTESIAN_POINT('Ctrl Pts',(-21.3467641075012,92.081268340934,1.89019751723676));
#20036=CARTESIAN_POINT('Ctrl Pts',(-21.6298379034514,92.8607543617003,1.94285857231964));
#20037=CARTESIAN_POINT('Ctrl Pts',(-21.9129116994015,93.6402403824667,1.99551962740252));
#20038=CARTESIAN_POINT('Ctrl Pts',(-22.6181116494178,94.2664182819908,2.04818068248539));
#20039=CARTESIAN_POINT('Ctrl Pts',(-23.425603594169,94.4553204550754,2.10084173756827));
#20040=CARTESIAN_POINT('Ctrl Pts',(-24.2330955389203,94.6442226281599,2.15350279265115));
#20041=CARTESIAN_POINT('Ctrl Pts',(-25.1428794784065,94.3958490748049,2.20616384773403));
#20042=CARTESIAN_POINT('Ctrl Pts',(-25.7423596992758,93.8228342131325,2.25882490281691));
#20043=CARTESIAN_POINT('Ctrl Pts',(-26.2303119273634,93.3564236982452,2.30168883438061));
#20044=CARTESIAN_POINT('Ctrl Pts',(-26.5126789427165,92.674928901641,2.34455276594432));
#20045=CARTESIAN_POINT('Ctrl Pts',(-26.5187354043533,91.9978903847198,2.38741669750802));
#20046=CARTESIAN_POINT('Origin',(-24.,92.,5.));
#20047=CARTESIAN_POINT('',(-26.5197283545653,92.0018289503525,3.38741669750802));
#20048=CARTESIAN_POINT('',(-26.5145913332516,92.0015585714996,3.11258330249198));
#20049=CARTESIAN_POINT('',(-26.5175,92.,5.));
#20050=CARTESIAN_POINT('Ctrl Pts',(-26.5145913332516,92.0015585714996,3.11258330249198));
#20051=CARTESIAN_POINT('Ctrl Pts',(-26.5163704675347,92.3124536217307,3.0929825844054));
#20052=CARTESIAN_POINT('Ctrl Pts',(-26.4629228052196,92.6227586740843,3.07338186631882));
#20053=CARTESIAN_POINT('Ctrl Pts',(-26.3514581912821,92.9105967308751,3.05378114823224));
#20054=CARTESIAN_POINT('Ctrl Pts',(-26.0519873173872,93.6839283862082,3.00112009314936));
#20055=CARTESIAN_POINT('Ctrl Pts',(-25.3337324697513,94.2950864454347,2.94845903806649));
#20056=CARTESIAN_POINT('Ctrl Pts',(-24.5224342992986,94.4669014516816,2.89579798298361));
#20057=CARTESIAN_POINT('Ctrl Pts',(-23.711136128846,94.6387164579284,2.84313692790073));
#20058=CARTESIAN_POINT('Ctrl Pts',(-22.8067946355765,94.3711884111957,2.79047587281785));
#20059=CARTESIAN_POINT('Ctrl Pts',(-22.2195444883875,93.7856434915613,2.73781481773497));
#20060=CARTESIAN_POINT('Ctrl Pts',(-21.6322943411984,93.2000985719269,2.68515376265209));
#20061=CARTESIAN_POINT('Ctrl Pts',(-21.3621355400899,92.2965367793909,2.63249270756922));
#20062=CARTESIAN_POINT('Ctrl Pts',(-21.5315889600923,91.4847436160309,2.57983165248634));
#20063=CARTESIAN_POINT('Ctrl Pts',(-21.7010423800948,90.6729504526708,2.52717059740346));
#20064=CARTESIAN_POINT('Ctrl Pts',(-22.3101080212084,89.9529259184868,2.47450954232058));
#20065=CARTESIAN_POINT('Ctrl Pts',(-23.0825657562016,89.6512036069521,2.4218484872377));
#20066=CARTESIAN_POINT('Ctrl Pts',(-23.8550234911947,89.3494812954174,2.36918743215482));
#20067=CARTESIAN_POINT('Ctrl Pts',(-24.7908733200675,89.466061206532,2.31652637707195));
#20068=CARTESIAN_POINT('Ctrl Pts',(-25.4656882386074,89.9480924170396,2.26386532198907));
#20069=CARTESIAN_POINT('Ctrl Pts',(-26.1118796445259,90.4096773895362,2.21343798215671));
#20070=CARTESIAN_POINT('Ctrl Pts',(-26.5187110383817,91.2063686024949,2.16301064232434));
#20071=CARTESIAN_POINT('Ctrl Pts',(-26.521412539848,92.0006455489043,2.11258330249198));
#20072=CARTESIAN_POINT('Ctrl Pts',(-26.5187354043533,91.9978903847198,2.38741669750802));
#20073=CARTESIAN_POINT('Ctrl Pts',(-26.5201196894756,91.8431441975284,2.39721382102719));
#20074=CARTESIAN_POINT('Ctrl Pts',(-26.5070691791327,91.6886308117444,2.40701094454637));
#20075=CARTESIAN_POINT('Ctrl Pts',(-26.4787393827788,91.5369716347155,2.41680806806554));
#20076=CARTESIAN_POINT('Ctrl Pts',(-26.3264623431602,90.7217800879606,2.46946912314842));
#20077=CARTESIAN_POINT('Ctrl Pts',(-25.7327317616706,89.9890531644404,2.5221301782313));
#20078=CARTESIAN_POINT('Ctrl Pts',(-24.9668162273558,89.6710932957471,2.57479123331418));
#20079=CARTESIAN_POINT('Ctrl Pts',(-24.2009006930409,89.3531334270537,2.62745228839706));
#20080=CARTESIAN_POINT('Ctrl Pts',(-23.2628002059009,89.4499406131871,2.68011334347994));
#20081=CARTESIAN_POINT('Ctrl Pts',(-22.5779585445906,89.9176119917392,2.73277439856281));
#20082=CARTESIAN_POINT('Ctrl Pts',(-21.8931168832803,90.3852833702914,2.78543545364569));
#20083=CARTESIAN_POINT('Ctrl Pts',(-21.4615340477996,91.2238189412625,2.83809650872857));
#20084=CARTESIAN_POINT('Ctrl Pts',(-21.4789406121676,92.052928097151,2.89075756381144));
#20085=CARTESIAN_POINT('Ctrl Pts',(-21.4963471765355,92.8820372530396,2.94341861889432));
#20086=CARTESIAN_POINT('Ctrl Pts',(-21.9627431407521,93.7017199938457,2.9960796739772));
#20087=CARTESIAN_POINT('Ctrl Pts',(-22.6666097831963,94.1402364113417,3.04874072906008));
#20088=CARTESIAN_POINT('Ctrl Pts',(-23.3704764256404,94.5787528288377,3.10140178414296));
#20089=CARTESIAN_POINT('Ctrl Pts',(-24.3118137463123,94.6361029230236,3.15406283922584));
#20090=CARTESIAN_POINT('Ctrl Pts',(-25.063709299524,94.286277347798,3.20672389430872));
#20091=CARTESIAN_POINT('Ctrl Pts',(-25.8156048527358,93.9364517725723,3.25938494939159));
#20092=CARTESIAN_POINT('Ctrl Pts',(-26.3780586384875,93.1794505279352,3.31204600447447));
#20093=CARTESIAN_POINT('Ctrl Pts',(-26.4959882199517,92.358586646163,3.36470705955735));
#20094=CARTESIAN_POINT('Ctrl Pts',(-26.5129402673076,92.2405897600233,3.37227693887424));
#20095=CARTESIAN_POINT('Ctrl Pts',(-26.5207069963199,92.1212732637326,3.37984681819113));
#20096=CARTESIAN_POINT('Ctrl Pts',(-26.5197283545653,92.0018289503525,3.38741669750802));
#20097=CARTESIAN_POINT('Origin',(-24.,92.,5.));
#20098=CARTESIAN_POINT('',(-26.5135838218621,92.000354216548,4.38741669750802));
#20099=CARTESIAN_POINT('',(-26.5160253566384,91.9978936308049,4.11258330249198));
#20100=CARTESIAN_POINT('',(-26.5175,92.,5.));
#20101=CARTESIAN_POINT('Ctrl Pts',(-26.5160253566384,91.9978936308049,4.11258330249198));
#20102=CARTESIAN_POINT('Ctrl Pts',(-26.5113087243027,92.5834107803607,4.07561558156934));
#20103=CARTESIAN_POINT('Ctrl Pts',(-26.3074058729855,93.1718905111793,4.03864786064669));
#20104=CARTESIAN_POINT('Ctrl Pts',(-25.9337852402154,93.6183375776454,4.00168013972405));
#20105=CARTESIAN_POINT('Ctrl Pts',(-25.4015572253053,94.2543079045141,3.94901908464117));
#20106=CARTESIAN_POINT('Ctrl Pts',(-24.5249308268757,94.6020596393698,3.8963580295583));
#20107=CARTESIAN_POINT('Ctrl Pts',(-23.7014710746985,94.5038814515943,3.84369697447542));
#20108=CARTESIAN_POINT('Ctrl Pts',(-22.8780113225213,94.4057032638187,3.79103591939254));
#20109=CARTESIAN_POINT('Ctrl Pts',(-22.1077182165964,93.8615951534119,3.73837486430966));
#20110=CARTESIAN_POINT('Ctrl Pts',(-21.7399328314132,93.1183194017708,3.68571380922678));
#20111=CARTESIAN_POINT('Ctrl Pts',(-21.3721474462299,92.3750436501297,3.6330527541439));
#20112=CARTESIAN_POINT('Ctrl Pts',(-21.4068697817883,91.4326002572543,3.58039169906102));
#20113=CARTESIAN_POINT('Ctrl Pts',(-21.8283526559748,90.7184034519114,3.52773064397815));
#20114=CARTESIAN_POINT('Ctrl Pts',(-22.2498355301614,90.0042066465684,3.47506958889527));
#20115=CARTESIAN_POINT('Ctrl Pts',(-23.058078942976,89.5182564287579,3.42240853381239));
#20116=CARTESIAN_POINT('Ctrl Pts',(-23.8865307343324,89.4809393801385,3.36974747872951));
#20117=CARTESIAN_POINT('Ctrl Pts',(-24.7149825256888,89.4436223315191,3.31708642364663));
#20118=CARTESIAN_POINT('Ctrl Pts',(-25.5636426955868,89.8549384520908,3.26442536856376));
#20119=CARTESIAN_POINT('Ctrl Pts',(-26.0476293304589,90.5283491380965,3.21176431348088));
#20120=CARTESIAN_POINT('Ctrl Pts',(-26.3514736272622,90.951112870825,3.17870397648458));
#20121=CARTESIAN_POINT('Ctrl Pts',(-26.5115904850836,91.4771749705661,3.14564363948828));
#20122=CARTESIAN_POINT('Ctrl Pts',(-26.5145913332516,92.0015585714996,3.11258330249198));
#20123=CARTESIAN_POINT('Ctrl Pts',(-26.5197283545653,92.0018289503525,3.38741669750802));
#20124=CARTESIAN_POINT('Ctrl Pts',(-26.5138989211591,91.2903401268976,3.43250787327401));
#20125=CARTESIAN_POINT('Ctrl Pts',(-26.1977683024704,90.5743161275881,3.47759904904));
#20126=CARTESIAN_POINT('Ctrl Pts',(-25.6643206092001,90.105645640677,3.52269022480598));
#20127=CARTESIAN_POINT('Ctrl Pts',(-25.0413180398075,89.5582950358707,3.57535127988886));
#20128=CARTESIAN_POINT('Ctrl Pts',(-24.1219075238456,89.3483203451655,3.62801233497174));
#20129=CARTESIAN_POINT('Ctrl Pts',(-23.3230574099716,89.5709486859401,3.68067339005462));
#20130=CARTESIAN_POINT('Ctrl Pts',(-22.5242072960976,89.7935770267148,3.7333344451375));
#20131=CARTESIAN_POINT('Ctrl Pts',(-21.8459175843117,90.4488083989693,3.78599550022037));
#20132=CARTESIAN_POINT('Ctrl Pts',(-21.5958042400641,91.239484187431,3.83865655530325));
#20133=CARTESIAN_POINT('Ctrl Pts',(-21.3456908958166,92.0301599758926,3.89131761038613));
#20134=CARTESIAN_POINT('Ctrl Pts',(-21.5237539191076,92.9562801805612,3.94397866546901));
#20135=CARTESIAN_POINT('Ctrl Pts',(-22.0492386873867,93.5978334861916,3.99663972055189));
#20136=CARTESIAN_POINT('Ctrl Pts',(-22.5747234556659,94.2393867918219,4.04930077563476));
#20137=CARTESIAN_POINT('Ctrl Pts',(-23.4476299689333,94.5963731984139,4.10196183071764));
#20138=CARTESIAN_POINT('Ctrl Pts',(-24.2720802276353,94.5068932768484,4.15462288580052));
#20139=CARTESIAN_POINT('Ctrl Pts',(-25.0965304863373,94.417413355283,4.2072839408834));
#20140=CARTESIAN_POINT('Ctrl Pts',(-25.8725244904738,93.8814671055602,4.25994499596628));
#20141=CARTESIAN_POINT('Ctrl Pts',(-26.2481357153638,93.1421152990992,4.31260605104916));
#20142=CARTESIAN_POINT('Ctrl Pts',(-26.4260009866856,92.7920059281747,4.33754293320211));
#20143=CARTESIAN_POINT('Ctrl Pts',(-26.5140860549172,92.396285723967,4.36247981535506));
#20144=CARTESIAN_POINT('Ctrl Pts',(-26.5135838218621,92.000354216548,4.38741669750802));
#20145=CARTESIAN_POINT('Origin',(-24.,92.,5.));
#20146=CARTESIAN_POINT('',(-26.5184741887082,91.9978439082844,5.38741669750802));
#20147=CARTESIAN_POINT('',(-26.5215002261917,92.0004777596725,5.11258330249198));
#20148=CARTESIAN_POINT('',(-26.5175,92.,5.));
#20149=CARTESIAN_POINT('Ctrl Pts',(-26.5215002261917,92.0004777596725,5.11258330249198));
#20150=CARTESIAN_POINT('Ctrl Pts',(-26.5215695052931,92.0268374618337,5.11090963381615));
#20151=CARTESIAN_POINT('Ctrl Pts',(-26.5211915450549,92.0531951295678,5.10923596514032));
#20152=CARTESIAN_POINT('Ctrl Pts',(-26.5203601912646,92.0795384889352,5.10756229646449));
#20153=CARTESIAN_POINT('Ctrl Pts',(-26.494202106107,92.9084176564484,5.05490124138161));
#20154=CARTESIAN_POINT('Ctrl Pts',(-26.0191792969125,93.723131379711,5.00224018629873));
#20155=CARTESIAN_POINT('Ctrl Pts',(-25.3107227144406,94.1541930811531,4.94957913121586));
#20156=CARTESIAN_POINT('Ctrl Pts',(-24.6022661319687,94.5852547825952,4.89691807613298));
#20157=CARTESIAN_POINT('Ctrl Pts',(-23.6603757762194,94.6326644622167,4.8442570210501));
#20158=CARTESIAN_POINT('Ctrl Pts',(-22.9122149978594,94.2749210214316,4.79159596596722));
#20159=CARTESIAN_POINT('Ctrl Pts',(-22.1640542194994,93.9171775806464,4.73893491088435));
#20160=CARTESIAN_POINT('Ctrl Pts',(-21.6096230185287,93.1542810194546,4.68627385580146));
#20161=CARTESIAN_POINT('Ctrl Pts',(-21.50036540662,92.3322179475565,4.63361280071859));
#20162=CARTESIAN_POINT('Ctrl Pts',(-21.3911077947114,91.5101548756584,4.58095174563571));
#20163=CARTESIAN_POINT('Ctrl Pts',(-21.7270237718648,90.6289252930541,4.52829069055283));
#20164=CARTESIAN_POINT('Ctrl Pts',(-22.3557697095322,90.0881818554959,4.47562963546995));
#20165=CARTESIAN_POINT('Ctrl Pts',(-22.9845156471996,89.5474384179376,4.42296858038708));
#20166=CARTESIAN_POINT('Ctrl Pts',(-23.906091545381,89.3471811254255,4.3703075253042));
#20167=CARTESIAN_POINT('Ctrl Pts',(-24.7025470068623,89.5782300758527,4.31764647022132));
#20168=CARTESIAN_POINT('Ctrl Pts',(-25.4990024683437,89.80927902628,4.26498541513844));
#20169=CARTESIAN_POINT('Ctrl Pts',(-26.1703374931251,90.4716342196466,4.21232436005556));
#20170=CARTESIAN_POINT('Ctrl Pts',(-26.4120901898205,91.2649062757708,4.15966330497269));
#20171=CARTESIAN_POINT('Ctrl Pts',(-26.4841340531159,91.5013064663318,4.14396997081245));
#20172=CARTESIAN_POINT('Ctrl Pts',(-26.5180276355322,91.7493331013702,4.12827663665222));
#20173=CARTESIAN_POINT('Ctrl Pts',(-26.5160253566384,91.9978936308049,4.11258330249198));
#20174=CARTESIAN_POINT('Ctrl Pts',(-26.5135838218621,92.000354216548,4.38741669750802));
#20175=CARTESIAN_POINT('Ctrl Pts',(-26.5130254522959,91.5601679289134,4.41514087043794));
#20176=CARTESIAN_POINT('Ctrl Pts',(-26.4029695423041,91.1197204618368,4.44286504336787));
#20177=CARTESIAN_POINT('Ctrl Pts',(-26.1850553752594,90.7413997625482,4.47058921629779));
#20178=CARTESIAN_POINT('Ctrl Pts',(-25.7711353646214,90.0227933956572,4.52325027138067));
#20179=CARTESIAN_POINT('Ctrl Pts',(-24.9680668977021,89.5283380250743,4.57591132646355));
#20180=CARTESIAN_POINT('Ctrl Pts',(-24.1400552293209,89.4822775999311,4.62857238154643));
#20181=CARTESIAN_POINT('Ctrl Pts',(-23.3120435609398,89.4362171747879,4.68123343662931));
#20182=CARTESIAN_POINT('Ctrl Pts',(-22.4590886910969,89.8385516950844,4.73389449171218));
#20183=CARTESIAN_POINT('Ctrl Pts',(-21.9680202099297,90.506815589517,4.78655554679506));
#20184=CARTESIAN_POINT('Ctrl Pts',(-21.4769517287624,91.1750794839497,4.83921660187794));
#20185=CARTESIAN_POINT('Ctrl Pts',(-21.3477696362708,92.1092727525185,4.89187765696082));
#20186=CARTESIAN_POINT('Ctrl Pts',(-21.6390602159943,92.8857228049574,4.94453871204369));
#20187=CARTESIAN_POINT('Ctrl Pts',(-21.9303507957177,93.6621728573964,4.99719976712657));
#20188=CARTESIAN_POINT('Ctrl Pts',(-22.6421140476561,94.2808796937054,5.04986082220945));
#20189=CARTESIAN_POINT('Ctrl Pts',(-23.4515531900704,94.4612492047027,5.10252187729233));
#20190=CARTESIAN_POINT('Ctrl Pts',(-24.2609923324847,94.6416187157001,5.15518293237521));
#20191=CARTESIAN_POINT('Ctrl Pts',(-25.1681073653747,94.3836509013857,5.20784398745809));
#20192=CARTESIAN_POINT('Ctrl Pts',(-25.7615061404264,93.8043385680607,5.26050504254096));
#20193=CARTESIAN_POINT('Ctrl Pts',(-26.2381975681409,93.3389631158763,5.30280892752999));
#20194=CARTESIAN_POINT('Ctrl Pts',(-26.5124386983965,92.6662146256838,5.345112812519));
#20195=CARTESIAN_POINT('Ctrl Pts',(-26.5184741887082,91.9978439082844,5.38741669750802));
#20196=CARTESIAN_POINT('Origin',(-24.,92.,5.));
#20197=CARTESIAN_POINT('',(-26.5199605075385,92.0017354236374,6.38741669750802));
#20198=CARTESIAN_POINT('',(-26.5147661754846,92.0016589575576,6.11258330249198));
#20199=CARTESIAN_POINT('',(-26.5175,92.,5.));
#20200=CARTESIAN_POINT('Ctrl Pts',(-26.5147661754846,92.0016589575576,6.11258330249198));
#20201=CARTESIAN_POINT('Ctrl Pts',(-26.5166141920308,92.3036180613248,6.09354263098009));
#20202=CARTESIAN_POINT('Ctrl Pts',(-26.4662618562805,92.604981570585,6.07450195946819));
#20203=CARTESIAN_POINT('Ctrl Pts',(-26.3609398422945,92.8857228268249,6.0554612879563));
#20204=CARTESIAN_POINT('Ctrl Pts',(-26.0696492553794,93.6621728984334,6.00280023287342));
#20205=CARTESIAN_POINT('Ctrl Pts',(-25.3578859858684,94.2808797500175,5.95013917779054));
#20206=CARTESIAN_POINT('Ctrl Pts',(-24.54844682347,94.4612492654679,5.89747812270766));
#20207=CARTESIAN_POINT('Ctrl Pts',(-23.7390076610717,94.6416187809184,5.84481706762479));
#20208=CARTESIAN_POINT('Ctrl Pts',(-22.831892605786,94.3836509602352,5.79215601254191));
#20209=CARTESIAN_POINT('Ctrl Pts',(-22.2384938160841,93.8043386126077,5.73949495745903));
#20210=CARTESIAN_POINT('Ctrl Pts',(-21.6450950263821,93.2250262649801,5.68683390237615));
#20211=CARTESIAN_POINT('Ctrl Pts',(-21.3654125022639,92.3243693904083,5.63417284729328));
#20212=CARTESIAN_POINT('Ctrl Pts',(-21.5262870414957,91.5108312521748,5.58151179221039));
#20213=CARTESIAN_POINT('Ctrl Pts',(-21.6871615807276,90.6972931139413,5.52885073712751));
#20214=CARTESIAN_POINT('Ctrl Pts',(-22.2885931833095,89.9708737120461,5.47618968204464));
#20215=CARTESIAN_POINT('Ctrl Pts',(-23.0578223533957,89.6610166423891,5.42352862696176));
#20216=CARTESIAN_POINT('Ctrl Pts',(-23.827051523482,89.3511595727321,5.37086757187888));
#20217=CARTESIAN_POINT('Ctrl Pts',(-24.7640782610726,89.4578648353135,5.318206516796));
#20218=CARTESIAN_POINT('Ctrl Pts',(-25.4439449493076,89.9327397724859,5.26554546171313));
#20219=CARTESIAN_POINT('Ctrl Pts',(-26.102204178709,90.392522279284,5.21455807530608));
#20220=CARTESIAN_POINT('Ctrl Pts',(-26.5193896768554,91.1974440773951,5.16357068889903));
#20221=CARTESIAN_POINT('Ctrl Pts',(-26.5215002261917,92.0004777596725,5.11258330249198));
#20222=CARTESIAN_POINT('Ctrl Pts',(-26.5184741887082,91.9978439082844,5.38741669750802));
#20223=CARTESIAN_POINT('Ctrl Pts',(-26.5199518449512,91.8342081285527,5.39777386760188));
#20224=CARTESIAN_POINT('Ctrl Pts',(-26.5053530710441,91.670834755527,5.40813103769574));
#20225=CARTESIAN_POINT('Ctrl Pts',(-26.4737128974313,91.5108312642518,5.4184882077896));
#20226=CARTESIAN_POINT('Ctrl Pts',(-26.3128383621713,90.6972931461036,5.47114926287248));
#20227=CARTESIAN_POINT('Ctrl Pts',(-25.711406774438,89.9708737621428,5.52381031795536));
#20228=CARTESIAN_POINT('Ctrl Pts',(-24.9421776233431,89.6610167001358,5.57647137303823));
#20229=CARTESIAN_POINT('Ctrl Pts',(-24.1729484722482,89.3511596381288,5.62913242812111));
#20230=CARTESIAN_POINT('Ctrl Pts',(-23.2359217577917,89.4578648980757,5.68179348320399));
#20231=CARTESIAN_POINT('Ctrl Pts',(-22.5560550863417,89.9327398235241,5.73445453828687));
#20232=CARTESIAN_POINT('Ctrl Pts',(-21.8761884148918,90.4076147489724,5.78711559336975));
#20233=CARTESIAN_POINT('Ctrl Pts',(-21.4534817864484,91.2506593399223,5.83977664845262));
#20234=CARTESIAN_POINT('Ctrl Pts',(-21.4796398709601,92.0795384869714,5.8924377035355));
#20235=CARTESIAN_POINT('Ctrl Pts',(-21.5057979554718,92.9084176340206,5.94509875861838));
#20236=CARTESIAN_POINT('Ctrl Pts',(-21.9808207529386,93.723131337169,5.99775981370126));
#20237=CARTESIAN_POINT('Ctrl Pts',(-22.6892773179196,94.1541930279687,6.05042086878414));
#20238=CARTESIAN_POINT('Ctrl Pts',(-23.3977338829005,94.5852547187683,6.10308192386702));
#20239=CARTESIAN_POINT('Ctrl Pts',(-24.3396242153956,94.6326643972192,6.15574297894989));
#20240=CARTESIAN_POINT('Ctrl Pts',(-25.0877849752844,94.2749209652664,6.20840403403277));
#20241=CARTESIAN_POINT('Ctrl Pts',(-25.8359457351732,93.9171775333136,6.26106508911565));
#20242=CARTESIAN_POINT('Ctrl Pts',(-26.3903769224557,93.154280990957,6.31372614419853));
#20243=CARTESIAN_POINT('Ctrl Pts',(-26.499634531667,92.3322179393546,6.36638719928141));
#20244=CARTESIAN_POINT('Ctrl Pts',(-26.5141780603748,92.2227912579824,6.37339703202361));
#20245=CARTESIAN_POINT('Ctrl Pts',(-26.5208336131063,92.1123162124966,6.38040686476582));
#20246=CARTESIAN_POINT('Ctrl Pts',(-26.5199605075385,92.0017354236374,6.38741669750802));
#20247=CARTESIAN_POINT('Origin',(-24.,92.,5.));
#20248=CARTESIAN_POINT('',(-26.5136288801011,92.0004946012931,7.38741669750802));
#20249=CARTESIAN_POINT('',(-26.5157924718976,91.9979483278017,7.11258330249198));
#20250=CARTESIAN_POINT('',(-26.5175,92.,5.));
#20251=CARTESIAN_POINT('Ctrl Pts',(-26.5157924718976,91.9979483278017,7.11258330249198));
#20252=CARTESIAN_POINT('Ctrl Pts',(-26.511298709256,92.5747303258767,7.07617562814402));
#20253=CARTESIAN_POINT('Ctrl Pts',(-26.3140597937548,93.1542901069194,7.03976795379606));
#20254=CARTESIAN_POINT('Ctrl Pts',(-25.9507613607754,93.5978335256406,7.0033602794481));
#20255=CARTESIAN_POINT('Ctrl Pts',(-25.4252765795229,94.2393868471104,6.95069922436522));
#20256=CARTESIAN_POINT('Ctrl Pts',(-24.552370044704,94.5963732625152,6.89803816928235));
#20257=CARTESIAN_POINT('Ctrl Pts',(-23.7279197656472,94.5068933387405,6.84537711419947));
#20258=CARTESIAN_POINT('Ctrl Pts',(-22.9034694865904,94.4174134149657,6.79271605911659));
#20259=CARTESIAN_POINT('Ctrl Pts',(-22.1274754632958,93.8814671520113,6.74005500403371));
#20260=CARTESIAN_POINT('Ctrl Pts',(-21.7518642291324,93.1421153272968,6.68739394895083));
#20261=CARTESIAN_POINT('Ctrl Pts',(-21.3762529949691,92.4027635025822,6.63473289386796));
#20262=CARTESIAN_POINT('Ctrl Pts',(-21.4010245499371,91.4600061161074,6.58207183878508));
#20263=CARTESIAN_POINT('Ctrl Pts',(-21.8149445707942,90.7413997314748,6.5294107837022));
#20264=CARTESIAN_POINT('Ctrl Pts',(-22.2288645916513,90.0227933468422,6.47674972861932));
#20265=CARTESIAN_POINT('Ctrl Pts',(-23.0319330783976,89.5283379640518,6.42408867353645));
#20266=CARTESIAN_POINT('Ctrl Pts',(-23.8599447672214,89.4822775377715,6.37142761845357));
#20267=CARTESIAN_POINT('Ctrl Pts',(-24.6879564560451,89.4362171114911,6.31876656337069));
#20268=CARTESIAN_POINT('Ctrl Pts',(-25.5409113469464,89.8385516417208,6.26610550828781));
#20269=CARTESIAN_POINT('Ctrl Pts',(-26.0319798402375,90.5068155526521,6.21344445320493));
#20270=CARTESIAN_POINT('Ctrl Pts',(-26.3454925694847,90.9334551058627,6.17982406963395));
#20271=CARTESIAN_POINT('Ctrl Pts',(-26.5115031064752,91.4684854880682,6.14620368606297));
#20272=CARTESIAN_POINT('Ctrl Pts',(-26.5147661754846,92.0016589575576,6.11258330249198));
#20273=CARTESIAN_POINT('Ctrl Pts',(-26.5199605075385,92.0017354236374,6.38741669750802));
#20274=CARTESIAN_POINT('Ctrl Pts',(-26.5142744465628,91.2815829799959,6.43306791984869));
#20275=CARTESIAN_POINT('Ctrl Pts',(-26.1892823731636,90.556945740582,6.47871914218937));
#20276=CARTESIAN_POINT('Ctrl Pts',(-25.6442302498738,90.0881819026962,6.52437036453004));
#20277=CARTESIAN_POINT('Ctrl Pts',(-25.0154843277294,89.5474384784885,6.57703141961292));
#20278=CARTESIAN_POINT('Ctrl Pts',(-24.0939084523006,89.3471811909213,6.6296924746958));
#20279=CARTESIAN_POINT('Ctrl Pts',(-23.2974530104828,89.5782301356438,6.68235352977867));
#20280=CARTESIAN_POINT('Ctrl Pts',(-22.5009975686649,89.8092790803663,6.73501458486155));
#20281=CARTESIAN_POINT('Ctrl Pts',(-21.829662560458,90.4716342573785,6.78767563994443));
#20282=CARTESIAN_POINT('Ctrl Pts',(-21.5879098697311,91.2649062939185,6.84033669502731));
#20283=CARTESIAN_POINT('Ctrl Pts',(-21.3461571790042,92.0581783304585,6.89299775011019));
#20284=CARTESIAN_POINT('Ctrl Pts',(-21.5339868057573,92.9823672265264,6.94565880519306));
#20285=CARTESIAN_POINT('Ctrl Pts',(-22.0662148075274,93.6183375376923,6.99831986027594));
#20286=CARTESIAN_POINT('Ctrl Pts',(-22.5984428092974,94.2543078488581,7.05098091535882));
#20287=CARTESIAN_POINT('Ctrl Pts',(-23.4750691860844,94.602059575122,7.1036419704417));
#20288=CARTESIAN_POINT('Ctrl Pts',(-24.2985289179312,94.5038813897733,7.15630302552458));
#20289=CARTESIAN_POINT('Ctrl Pts',(-25.121988649778,94.4057032044246,7.20896408060746));
#20290=CARTESIAN_POINT('Ctrl Pts',(-25.8922817366847,93.8615951074632,7.26162513569033));
#20291=CARTESIAN_POINT('Ctrl Pts',(-26.2600671127882,93.1183193741671,7.31428619077321));
#20292=CARTESIAN_POINT('Ctrl Pts',(-26.4303151951188,92.7742565689049,7.33866302635148));
#20293=CARTESIAN_POINT('Ctrl Pts',(-26.5143151353889,92.3875167213616,7.36303986192975));
#20294=CARTESIAN_POINT('Ctrl Pts',(-26.5136288801011,92.0004946012931,7.38741669750802));
#20295=CARTESIAN_POINT('Origin',(-24.,92.,5.));
#20296=CARTESIAN_POINT('',(-26.5182105203766,91.9978055611691,8.38741669750802));
#20297=CARTESIAN_POINT('',(-26.5215632327497,92.0003195913041,8.11258330249199));
#20298=CARTESIAN_POINT('',(-26.5175,92.,5.));
#20299=CARTESIAN_POINT('Ctrl Pts',(-26.5215632327497,92.0003195913041,8.11258330249199));
#20300=CARTESIAN_POINT('Ctrl Pts',(-26.5215948568411,92.0178575782261,8.11146968039084));
#20301=CARTESIAN_POINT('Ctrl Pts',(-26.521427546271,92.0353949460436,8.1103560582897));
#20302=CARTESIAN_POINT('Ctrl Pts',(-26.5210594500516,92.052928098419,8.10924243618855));
#20303=CARTESIAN_POINT('Ctrl Pts',(-26.5036528852352,92.8820372747418,8.05658138110567));
#20304=CARTESIAN_POINT('Ctrl Pts',(-26.0372569095473,93.7017200358608,8.00392032602279));
#20305=CARTESIAN_POINT('Ctrl Pts',(-25.3333902497356,94.1402364642016,7.95125927093991));
#20306=CARTESIAN_POINT('Ctrl Pts',(-24.6295235899239,94.5787528925424,7.89859821585703));
#20307=CARTESIAN_POINT('Ctrl Pts',(-23.6881862459885,94.636102988105,7.84593716077416));
#20308=CARTESIAN_POINT('Ctrl Pts',(-22.9362906742079,94.2862774042331,7.79327610569128));
#20309=CARTESIAN_POINT('Ctrl Pts',(-22.1843951024273,93.9364518203612,7.7406150506084));
#20310=CARTESIAN_POINT('Ctrl Pts',(-21.6219413028015,93.1794505570548,7.68795399552552));
#20311=CARTESIAN_POINT('Ctrl Pts',(-21.5040117184286,92.3585866550213,7.63529294044264));
#20312=CARTESIAN_POINT('Ctrl Pts',(-21.3860821340558,91.5377227529878,7.58263188535977));
#20313=CARTESIAN_POINT('Ctrl Pts',(-21.7126767649359,90.6529962122272,7.52997083027689));
#20314=CARTESIAN_POINT('Ctrl Pts',(-22.3356793497081,90.105645593905,7.47730977519401));
#20315=CARTESIAN_POINT('Ctrl Pts',(-22.9586819344804,89.5582949755827,7.42464872011113));
#20316=CARTESIAN_POINT('Ctrl Pts',(-23.8780924731448,89.3483202796988,7.37198766502825));
#20317=CARTESIAN_POINT('Ctrl Pts',(-24.6769426067422,89.5709486259712,7.31932660994537));
#20318=CARTESIAN_POINT('Ctrl Pts',(-25.4757927403397,89.7935769722436,7.2666655548625));
#20319=CARTESIAN_POINT('Ctrl Pts',(-26.1540824688701,90.4488083606723,7.21400449977962));
#20320=CARTESIAN_POINT('Ctrl Pts',(-26.4041958192921,91.2394841686541,7.16134344469674));
#20321=CARTESIAN_POINT('Ctrl Pts',(-26.4813911490268,91.4835194414908,7.14509006396182));
#20322=CARTESIAN_POINT('Ctrl Pts',(-26.517798610341,91.7404570822428,7.1288366832269));
#20323=CARTESIAN_POINT('Ctrl Pts',(-26.5157924718976,91.9979483278017,7.11258330249198));
#20324=CARTESIAN_POINT('Ctrl Pts',(-26.5136288801011,92.0004946012931,7.38741669750802));
#20325=CARTESIAN_POINT('Ctrl Pts',(-26.5128326243634,91.5514363729595,7.41570091701263));
#20326=CARTESIAN_POINT('Ctrl Pts',(-26.3980254709817,91.1019981282164,7.44398513651724));
#20327=CARTESIAN_POINT('Ctrl Pts',(-26.1716472904104,90.7184034835404,7.47226935602185));
#20328=CARTESIAN_POINT('Ctrl Pts',(-25.7501644266289,90.0042066958411,7.52493041110473));
#20329=CARTESIAN_POINT('Ctrl Pts',(-24.9419210337657,89.5182564900734,7.5775914661876));
#20330=CARTESIAN_POINT('Ctrl Pts',(-24.1134692628649,89.4809394423544,7.63025252127048));
#20331=CARTESIAN_POINT('Ctrl Pts',(-23.285017491964,89.4436223946354,7.68291357635336));
#20332=CARTESIAN_POINT('Ctrl Pts',(-22.4363573430257,89.8549385049651,7.73557463143624));
#20333=CARTESIAN_POINT('Ctrl Pts',(-21.9523707200979,90.5283491743849,7.78823568651912));
#20334=CARTESIAN_POINT('Ctrl Pts',(-21.4683840971702,91.2017598438046,7.840896741602));
#20335=CARTESIAN_POINT('Ctrl Pts',(-21.3490710002532,92.1372650723145,7.89355779668487));
#20336=CARTESIAN_POINT('Ctrl Pts',(-21.648541866765,92.9105967084797,7.94621885176775));
#20337=CARTESIAN_POINT('Ctrl Pts',(-21.9480127332768,93.6839283446448,7.99887990685063));
#20338=CARTESIAN_POINT('Ctrl Pts',(-22.6662675632174,94.2950863884653,8.05154096193351));
#20339=CARTESIAN_POINT('Ctrl Pts',(-23.4775657136168,94.4669013906121,8.10420201701639));
#20340=CARTESIAN_POINT('Ctrl Pts',(-24.2888638640162,94.6387163927589,8.15686307209926));
#20341=CARTESIAN_POINT('Ctrl Pts',(-25.1932053348746,94.3711883532321,8.20952412718214));
#20342=CARTESIAN_POINT('Ctrl Pts',(-25.7804554676164,93.785643447789,8.26218518226502));
#20343=CARTESIAN_POINT('Ctrl Pts',(-26.2459621805258,93.3214884497798,8.30392902067936));
#20344=CARTESIAN_POINT('Ctrl Pts',(-26.5122227023915,92.6575056999379,8.34567285909369));
#20345=CARTESIAN_POINT('Ctrl Pts',(-26.5182105203766,91.9978055611691,8.38741669750802));
#20346=CARTESIAN_POINT('Origin',(-24.,92.,5.));
#20347=CARTESIAN_POINT('',(-26.5201758362126,92.0015868137837,9.38741669750802));
#20348=CARTESIAN_POINT('',(-26.5149491154365,92.0017493991467,9.11258330249198));
#20349=CARTESIAN_POINT('',(-26.5175,92.,5.));
#20350=CARTESIAN_POINT('',(-22.0865340033349,93.6359872033749,10.));
#20351=CARTESIAN_POINT('Ctrl Pts',(-26.5201758362126,92.0015868137837,9.38741669750802));
#20352=CARTESIAN_POINT('Ctrl Pts',(-26.5146934294681,91.2729074143925,9.43362796642338));
#20353=CARTESIAN_POINT('Ctrl Pts',(-26.1807323142246,90.5399684977903,9.47983923533873));
#20354=CARTESIAN_POINT('Ctrl Pts',(-25.6239878020485,90.0711234457756,9.52605050425409));
#20355=CARTESIAN_POINT('Ctrl Pts',(-24.9895375021336,89.5368408846388,9.57871155933697));
#20356=CARTESIAN_POINT('Ctrl Pts',(-24.0657754031769,89.3455168748646,9.63137261441985));
#20357=CARTESIAN_POINT('Ctrl Pts',(-23.2718707713924,89.5853895680493,9.68403366950273));
#20358=CARTESIAN_POINT('Ctrl Pts',(-22.4779661396078,89.825262261234,9.73669472458561));
#20359=CARTESIAN_POINT('Ctrl Pts',(-21.8139189749953,90.4963316573775,9.78935577966849));
#20360=CARTESIAN_POINT('Ctrl Pts',(-21.5807324199303,91.2907313838813,9.84201683475137));
#20361=CARTESIAN_POINT('Ctrl Pts',(-21.3475458648653,92.0851311103851,9.89467788983424));
#20362=CARTESIAN_POINT('Ctrl Pts',(-21.5452199193478,93.0028611672492,9.94733894491712));
#20363=CARTESIAN_POINT('Ctrl Pts',(-22.0865340033349,93.6359872033749,10.));
#20364=CARTESIAN_POINT('',(-25.9171032040961,93.6385343199285,10.));
#20365=CARTESIAN_POINT('Origin',(-24.,92.,10.));
#20366=CARTESIAN_POINT('Ctrl Pts',(-25.9171116625783,93.6385402433575,10.));
#20367=CARTESIAN_POINT('Ctrl Pts',(-25.393956920721,94.2476959894344,9.94901908464118));
#20368=CARTESIAN_POINT('Ctrl Pts',(-24.5534186715195,94.5878275437024,9.89803816928236));
#20369=CARTESIAN_POINT('Ctrl Pts',(-23.7542642292644,94.5094851289583,9.84705725392353));
#20370=CARTESIAN_POINT('Ctrl Pts',(-22.9287726544835,94.4285608421125,9.79439619884065));
#20371=CARTESIAN_POINT('Ctrl Pts',(-22.1474375442602,93.9011254113112,9.74173514375777));
#20372=CARTESIAN_POINT('Ctrl Pts',(-21.7641120845165,93.1658537236911,9.68907408867489));
#20373=CARTESIAN_POINT('Ctrl Pts',(-21.3807866247728,92.4305820360709,9.63641303359201));
#20374=CARTESIAN_POINT('Ctrl Pts',(-21.3954708155088,91.487474091632,9.58375197850913));
#20375=CARTESIAN_POINT('Ctrl Pts',(-21.8017477031856,90.764502097224,9.53109092342626));
#20376=CARTESIAN_POINT('Ctrl Pts',(-22.2080245908624,90.041530102816,9.47842986834338));
#20377=CARTESIAN_POINT('Ctrl Pts',(-23.0058941754799,89.5386940584389,9.4257688132605));
#20378=CARTESIAN_POINT('Ctrl Pts',(-23.8333902143466,89.4839130383455,9.37310775817762));
#20379=CARTESIAN_POINT('Ctrl Pts',(-24.6608862532133,89.4291320182521,9.32044670309475));
#20380=CARTESIAN_POINT('Ctrl Pts',(-25.518008746329,89.8224060224424,9.26778564801186));
#20381=CARTESIAN_POINT('Ctrl Pts',(-26.016096172441,90.4854401035392,9.21512459292899));
#20382=CARTESIAN_POINT('Ctrl Pts',(-26.3393871214709,90.9157920981482,9.18094416278332));
#20383=CARTESIAN_POINT('Ctrl Pts',(-26.5114220034557,91.4597899508601,9.14676373263765));
#20384=CARTESIAN_POINT('Ctrl Pts',(-26.5149491154365,92.0017493991467,9.11258330249198));
#20385=CARTESIAN_POINT('Origin',(-24.,92.,12.2084234471775));
#20386=CARTESIAN_POINT('',(-27.078276640009,92.0007881209763,1.79157655282254));
#20387=CARTESIAN_POINT('',(-27.0686108047355,92.0003349297086,1.70842344717745));
#20388=CARTESIAN_POINT('',(-27.0735,92.0000000000001,12.2084234471775));
#20389=CARTESIAN_POINT('',(-23.2062007174672,89.0307770462543,0.999999999999999));
#20390=CARTESIAN_POINT('Ctrl Pts',(-27.0686108047355,92.0003349297086,1.70842344717745));
#20391=CARTESIAN_POINT('Ctrl Pts',(-27.0689532420951,92.4946153833655,1.68292651844981));
#20392=CARTESIAN_POINT('Ctrl Pts',(-26.723556593627,94.0092287415617,1.6047685346393));
#20393=CARTESIAN_POINT('Ctrl Pts',(-24.3539160917338,95.6088396578189,1.4739494957459));
#20394=CARTESIAN_POINT('Ctrl Pts',(-21.1687762982368,94.2698556568795,1.31596633049727));
#20395=CARTESIAN_POINT('Ctrl Pts',(-20.5566852567634,90.8667001441213,1.15798316524863));
#20396=CARTESIAN_POINT('Ctrl Pts',(-22.2237466982397,89.2934286920664,1.05266105508288));
#20397=CARTESIAN_POINT('Ctrl Pts',(-23.2062007174672,89.0307770462543,0.999999999999999));
#20398=CARTESIAN_POINT('',(-24.7937992825329,89.0307770462543,0.999999999999999));
#20399=CARTESIAN_POINT('Origin',(-24.,92.,0.999999999999999));
#20400=CARTESIAN_POINT('Ctrl Pts',(-27.078276640009,92.0007881209763,1.79157655282254));
#20401=CARTESIAN_POINT('Ctrl Pts',(-27.0784227334426,92.0437415110921,1.78934283757203));
#20402=CARTESIAN_POINT('Ctrl Pts',(-27.0582221315001,93.0992023691253,1.73444806723864));
#20403=CARTESIAN_POINT('Ctrl Pts',(-25.8523949517842,95.1179531681003,1.62689224182237));
#20404=CARTESIAN_POINT('Ctrl Pts',(-22.40096829048,95.2555127221397,1.46890907657374));
#20405=CARTESIAN_POINT('Ctrl Pts',(-20.4000492676845,92.4393710995324,1.3109259113251));
#20406=CARTESIAN_POINT('Ctrl Pts',(-21.6506968017521,89.2605902470592,1.15462288580052));
#20407=CARTESIAN_POINT('Ctrl Pts',(-23.8480943965222,88.774594383454,1.05098091535882));
#20408=CARTESIAN_POINT('Ctrl Pts',(-24.7957016814436,89.0256872793281,1.));
#20409=CARTESIAN_POINT('Origin',(-24.,92.,12.2084234471775));
#20410=CARTESIAN_POINT('',(-27.069948942502,92.0019027882837,2.79157655282254));
#20411=CARTESIAN_POINT('',(-27.0750082483734,91.9974244677008,2.70842344717745));
#20412=CARTESIAN_POINT('',(-27.0735,92.0000000000001,12.2084234471775));
#20413=CARTESIAN_POINT('Ctrl Pts',(-27.0750082483734,91.9974244677008,2.70842344717745));
#20414=CARTESIAN_POINT('Ctrl Pts',(-27.0676141928259,92.8239896640293,2.66555951561375));
#20415=CARTESIAN_POINT('Ctrl Pts',(-26.2993639886887,94.678166986954,2.57003452896717));
#20416=CARTESIAN_POINT('Ctrl Pts',(-23.1738622446318,95.5314376817822,2.42184848723771));
#20417=CARTESIAN_POINT('Ctrl Pts',(-20.5910236590807,93.2380222607045,2.26386532198907));
#20418=CARTESIAN_POINT('Ctrl Pts',(-21.1003115510402,89.8216058212251,2.10588215674044));
#20419=CARTESIAN_POINT('Ctrl Pts',(-24.2395757883417,88.3812154557912,1.94789899149181));
#20420=CARTESIAN_POINT('Ctrl Pts',(-26.6902007202702,89.9256564305863,1.81541275497081));
#20421=CARTESIAN_POINT('Ctrl Pts',(-27.0682459760221,91.4737343794429,1.73558757353269));
#20422=CARTESIAN_POINT('Ctrl Pts',(-27.0686108047355,92.0003349297086,1.70842344717745));
#20423=CARTESIAN_POINT('Ctrl Pts',(-27.069948942502,92.0019027882837,2.79157655282254));
#20424=CARTESIAN_POINT('Ctrl Pts',(-27.072121005747,92.3814602607307,2.77197583473597));
#20425=CARTESIAN_POINT('Ctrl Pts',(-26.8315578651691,93.7781155062161,2.69971406156651));
#20426=CARTESIAN_POINT('Ctrl Pts',(-24.7514083303165,95.5481002919865,2.57479123331418));
#20427=CARTESIAN_POINT('Ctrl Pts',(-21.4392014827728,94.5682622165549,2.41680806806554));
#20428=CARTESIAN_POINT('Ctrl Pts',(-20.4497281061605,91.2589110713399,2.25882490281691));
#20429=CARTESIAN_POINT('Ctrl Pts',(-22.6804688187274,88.6217765261786,2.10084173756827));
#20430=CARTESIAN_POINT('Ctrl Pts',(-26.0596141395782,89.0427206231847,1.94509228757015));
#20431=CARTESIAN_POINT('Ctrl Pts',(-27.0749785010789,91.0310919164918,1.84200389265491));
#20432=CARTESIAN_POINT('Ctrl Pts',(-27.078276640009,92.0007881209763,1.79157655282254));
#20433=CARTESIAN_POINT('Origin',(-24.,92.,12.2084234471775));
#20434=CARTESIAN_POINT('',(-27.0716996757212,91.9974284306968,3.79157655282255));
#20435=CARTESIAN_POINT('',(-27.0762204956331,92.0022328813937,3.70842344717745));
#20436=CARTESIAN_POINT('',(-27.0735,92.0000000000001,12.2084234471775));
#20437=CARTESIAN_POINT('Ctrl Pts',(-27.0762204956331,92.0022328813937,3.70842344717745));
#20438=CARTESIAN_POINT('Ctrl Pts',(-27.0774152743552,92.1480569517705,3.70085356786056));
#20439=CARTESIAN_POINT('Ctrl Pts',(-27.0019699142738,93.3070874795555,3.6406226334608));
#20440=CARTESIAN_POINT('Ctrl Pts',(-25.5299145201095,95.2883129487163,3.52773064397815));
#20441=CARTESIAN_POINT('Ctrl Pts',(-22.0822081585386,95.0782646692958,3.36974747872952));
#20442=CARTESIAN_POINT('Ctrl Pts',(-20.3740039924776,92.0761257570406,3.21176431348088));
#20443=CARTESIAN_POINT('Ctrl Pts',(-21.9547029138477,89.0049371841951,3.05378114823225));
#20444=CARTESIAN_POINT('Ctrl Pts',(-25.3905541717125,88.6503748565914,2.89579798298361));
#20445=CARTESIAN_POINT('Ctrl Pts',(-26.9751243964845,90.605903680769,2.78067874929868));
#20446=CARTESIAN_POINT('Ctrl Pts',(-27.0766982584323,91.8085019627027,2.71822057069663));
#20447=CARTESIAN_POINT('Ctrl Pts',(-27.0750082483734,91.9974244677008,2.70842344717745));
#20448=CARTESIAN_POINT('Ctrl Pts',(-27.0716996757212,91.9974284306968,3.79157655282255));
#20449=CARTESIAN_POINT('Ctrl Pts',(-27.0659413561646,92.7122593975924,3.7546088318999));
#20450=CARTESIAN_POINT('Ctrl Pts',(-26.4623933413542,94.4541466296605,3.66498005589438));
#20451=CARTESIAN_POINT('Ctrl Pts',(-23.5706310470027,95.6012890799134,3.52269022480599));
#20452=CARTESIAN_POINT('Ctrl Pts',(-20.7493847378944,93.6084593551842,3.36470705955735));
#20453=CARTESIAN_POINT('Ctrl Pts',(-20.8765574469375,90.1567019355188,3.20672389430872));
#20454=CARTESIAN_POINT('Ctrl Pts',(-23.8367991104361,88.3768791020246,3.04874072906008));
#20455=CARTESIAN_POINT('Ctrl Pts',(-26.5594315108873,89.6964445021905,2.91035828189802));
#20456=CARTESIAN_POINT('Ctrl Pts',(-27.0662853449471,91.3617069600934,2.82463688981884));
#20457=CARTESIAN_POINT('Ctrl Pts',(-27.069948942502,92.0019027882837,2.79157655282254));
#20458=CARTESIAN_POINT('Origin',(-24.,92.,12.2084234471775));
#20459=CARTESIAN_POINT('',(-27.0783836922344,92.0005832748178,4.79157655282255));
#20460=CARTESIAN_POINT('',(-27.0687189181701,92.0004324466973,4.70842344717745));
#20461=CARTESIAN_POINT('',(-27.0735,92.0000000000001,12.2084234471775));
#20462=CARTESIAN_POINT('Ctrl Pts',(-27.0687189181701,92.0004324466973,4.70842344717746));
#20463=CARTESIAN_POINT('Ctrl Pts',(-27.0693320714153,92.4838070199057,4.6834865650245));
#20464=CARTESIAN_POINT('Ctrl Pts',(-26.734694995182,93.9871566204806,4.60588862778867));
#20465=CARTESIAN_POINT('Ctrl Pts',(-24.3913282534434,95.6056209517321,4.47562963546996));
#20466=CARTESIAN_POINT('Ctrl Pts',(-21.1942539711864,94.2981360810344,4.31764647022132));
#20467=CARTESIAN_POINT('Ctrl Pts',(-20.5420870968054,90.9061633512837,4.15966330497269));
#20468=CARTESIAN_POINT('Ctrl Pts',(-23.0263652646397,88.5063377831116,4.00168013972405));
#20469=CARTESIAN_POINT('Ctrl Pts',(-26.232411992584,89.2385337482431,3.85126685379231));
#20470=CARTESIAN_POINT('Ctrl Pts',(-27.0691036084141,91.1336088897795,3.75351462294344));
#20471=CARTESIAN_POINT('Ctrl Pts',(-27.0762204956331,92.0022328813937,3.70842344717745));
#20472=CARTESIAN_POINT('Ctrl Pts',(-27.0783836922344,92.0005832748178,4.79157655282255));
#20473=CARTESIAN_POINT('Ctrl Pts',(-27.078468271904,92.0327646232159,4.78990288414672));
#20474=CARTESIAN_POINT('Ctrl Pts',(-27.0634880644545,93.0774335875127,4.73556816038801));
#20475=CARTESIAN_POINT('Ctrl Pts',(-25.8851896583917,95.0983384007904,4.62857238154643));
#20476=CARTESIAN_POINT('Ctrl Pts',(-22.4354577715254,95.2719792949115,4.47058921629779));
#20477=CARTESIAN_POINT('Ctrl Pts',(-20.4048190868974,92.4778232899584,4.31260605104916));
#20478=CARTESIAN_POINT('Ctrl Pts',(-21.6351322020288,89.2502652496793,4.15462288580052));
#20479=CARTESIAN_POINT('Ctrl Pts',(-25.010461127225,88.5168104867762,3.99663972055189));
#20480=CARTESIAN_POINT('Ctrl Pts',(-26.893911960326,90.3750681296893,3.8756242762259));
#20481=CARTESIAN_POINT('Ctrl Pts',(-27.0741441659616,91.693972308664,3.80726988698278));
#20482=CARTESIAN_POINT('Ctrl Pts',(-27.0716996757212,91.9974284306968,3.79157655282255));
#20483=CARTESIAN_POINT('Origin',(-24.,92.,12.2084234471775));
#20484=CARTESIAN_POINT('',(-27.0701623993453,92.0020253450063,5.79157655282255));
#20485=CARTESIAN_POINT('',(-27.0746893422025,91.9973677267577,5.70842344717746));
#20486=CARTESIAN_POINT('',(-27.0735,92.0000000000001,12.2084234471775));
#20487=CARTESIAN_POINT('Ctrl Pts',(-27.0746893422025,91.9973677267577,5.70842344717746));
#20488=CARTESIAN_POINT('Ctrl Pts',(-27.0673208895816,92.8133508051795,5.66611956218844));
#20489=CARTESIAN_POINT('Ctrl Pts',(-26.3157336914085,94.657090117177,5.57115462211654));
#20490=CARTESIAN_POINT('Ctrl Pts',(-23.2111785026033,95.5399718768618,5.42352862696177));
#20491=CARTESIAN_POINT('Ctrl Pts',(-20.6043014164074,93.2739196885051,5.26554546171313));
#20492=CARTESIAN_POINT('Ctrl Pts',(-21.0774388479142,89.8523788611612,5.1075622964645));
#20493=CARTESIAN_POINT('Ctrl Pts',(-24.2014389978196,88.3788037094653,4.94957913121586));
#20494=CARTESIAN_POINT('Ctrl Pts',(-26.6784589321776,89.9039237459709,4.81653284812018));
#20495=CARTESIAN_POINT('Ctrl Pts',(-27.0680372304395,91.4630292470767,4.73614762010738));
#20496=CARTESIAN_POINT('Ctrl Pts',(-27.0687189181701,92.0004324466973,4.70842344717746));
#20497=CARTESIAN_POINT('Ctrl Pts',(-27.0701623993453,92.0020253450063,5.79157655282255));
#20498=CARTESIAN_POINT('Ctrl Pts',(-27.0724185577782,92.3706733312739,5.77253588131066));
#20499=CARTESIAN_POINT('Ctrl Pts',(-26.840929369154,93.7561580997579,5.70083415471589));
#20500=CARTESIAN_POINT('Ctrl Pts',(-24.7888215168716,95.5399719642594,5.57647137303822));
#20501=CARTESIAN_POINT('Ctrl Pts',(-21.4664563263011,94.5951488100945,5.41848820778961));
#20502=CARTESIAN_POINT('Ctrl Pts',(-20.4421017230708,91.2964371072188,5.26050504254096));
#20503=CARTESIAN_POINT('Ctrl Pts',(-22.6448822957049,88.6358809621643,5.10252187729233));
#20504=CARTESIAN_POINT('Ctrl Pts',(-26.0404432418415,89.0225553310303,4.94621238071952));
#20505=CARTESIAN_POINT('Ctrl Pts',(-27.075807019589,91.0201963741306,4.84256393922959));
#20506=CARTESIAN_POINT('Ctrl Pts',(-27.0783836922344,92.0005832748178,4.79157655282255));
#20507=CARTESIAN_POINT('Origin',(-24.,92.,12.2084234471775));
#20508=CARTESIAN_POINT('',(-27.0714153574487,91.9974952077453,6.79157655282255));
#20509=CARTESIAN_POINT('',(-27.0765039205242,92.0021186989274,6.70842344717745));
#20510=CARTESIAN_POINT('',(-27.0735,92.0000000000001,12.2084234471775));
#20511=CARTESIAN_POINT('Ctrl Pts',(-27.0765039205242,92.0021186989274,6.70842344717745));
#20512=CARTESIAN_POINT('Ctrl Pts',(-27.0775698549682,92.1371216997451,6.70141361443525));
#20513=CARTESIAN_POINT('Ctrl Pts',(-27.0084022542901,93.2852297742065,6.64174272661016));
#20514=CARTESIAN_POINT('Ctrl Pts',(-25.5645421898479,95.27197921413,6.5294107837022));
#20515=CARTESIAN_POINT('Ctrl Pts',(-22.1148103881513,95.0983383242963,6.37142761845358));
#20516=CARTESIAN_POINT('Ctrl Pts',(-20.3750099098822,92.114398820868,6.21344445320493));
#20517=CARTESIAN_POINT('Ctrl Pts',(-21.9231991720717,89.0266956824957,6.05546128795631));
#20518=CARTESIAN_POINT('Ctrl Pts',(-25.355117670839,88.6358810452203,5.89747812270766));
#20519=CARTESIAN_POINT('Ctrl Pts',(-26.9680494317645,90.584007681798,5.78179884244805));
#20520=CARTESIAN_POINT('Ctrl Pts',(-27.0764933447696,91.7975923269541,5.71878061727132));
#20521=CARTESIAN_POINT('Ctrl Pts',(-27.0746893422025,91.9973677267577,5.70842344717746));
#20522=CARTESIAN_POINT('Ctrl Pts',(-27.0714153574487,91.9974952077453,6.79157655282255));
#20523=CARTESIAN_POINT('Ctrl Pts',(-27.0659291292545,92.7016618298241,6.75516887847459));
#20524=CARTESIAN_POINT('Ctrl Pts',(-26.4768296167088,94.4326507862167,6.66610014904376));
#20525=CARTESIAN_POINT('Ctrl Pts',(-23.6086717368945,95.6056210407497,6.52437036453004));
#20526=CARTESIAN_POINT('Ctrl Pts',(-20.7665454640887,93.6426845888844,6.36638719928141));
#20527=CARTESIAN_POINT('Ctrl Pts',(-20.857272821619,90.1897771481731,6.20840403403277));
#20528=CARTESIAN_POINT('Ctrl Pts',(-23.7985609972073,88.3788036200625,6.05042086878414));
#20529=CARTESIAN_POINT('Ctrl Pts',(-26.5460460301536,89.6747784855977,5.91147837504739));
#20530=CARTESIAN_POINT('Ctrl Pts',(-27.0661786684217,91.351098370438,5.82519693639353));
#20531=CARTESIAN_POINT('Ctrl Pts',(-27.0701623993453,92.0020253450063,5.79157655282255));
#20532=CARTESIAN_POINT('Origin',(-24.,92.,12.2084234471775));
#20533=CARTESIAN_POINT('',(-27.0784606140442,92.000390174329,7.79157655282255));
#20534=CARTESIAN_POINT('',(-27.0687739277024,92.0006038359779,7.70842344717745));
#20535=CARTESIAN_POINT('',(-27.0735,92.0000000000001,12.2084234471775));
#20536=CARTESIAN_POINT('Ctrl Pts',(-27.0687739277024,92.0006038359779,7.70842344717745));
#20537=CARTESIAN_POINT('Ctrl Pts',(-27.0696117452305,92.4731013478073,7.68404661159918));
#20538=CARTESIAN_POINT('Ctrl Pts',(-26.745518655979,93.9652418365262,7.60700872093803));
#20539=CARTESIAN_POINT('Ctrl Pts',(-24.4293689423972,95.6012889909869,7.47730977519402));
#20540=CARTESIAN_POINT('Ctrl Pts',(-21.2186704291245,94.3276267101463,7.31932660994538));
#20541=CARTESIAN_POINT('Ctrl Pts',(-20.5307327633938,90.9427275180138,7.16134344469674));
#20542=CARTESIAN_POINT('Ctrl Pts',(-22.9895388977221,88.5168105727741,7.00336027944811));
#20543=CARTESIAN_POINT('Ctrl Pts',(-26.2151018414649,89.2177213748181,6.85238694694168));
#20544=CARTESIAN_POINT('Ctrl Pts',(-27.0695620701135,91.1229176917646,6.75407466951813));
#20545=CARTESIAN_POINT('Ctrl Pts',(-27.0765039205242,92.0021186989274,6.70842344717745));
#20546=CARTESIAN_POINT('Ctrl Pts',(-27.0784606140442,92.000390174329,7.79157655282255));
#20547=CARTESIAN_POINT('Ctrl Pts',(-27.0784992224434,92.0218014961978,7.79046293072141));
#20548=CARTESIAN_POINT('Ctrl Pts',(-27.0686358124042,93.0556766999574,7.73668825353738));
#20549=CARTESIAN_POINT('Ctrl Pts',(-25.9177918888646,95.0782647453892,7.63025252127048));
#20550=CARTESIAN_POINT('Ctrl Pts',(-22.4700854420894,95.288313029852,7.47226935602185));
#20551=CARTESIAN_POINT('Ctrl Pts',(-20.4100634919605,92.5157489192991,7.31428619077322));
#20552=CARTESIAN_POINT('Ctrl Pts',(-21.6062365978313,89.275383052732,7.15630302552458));
#20553=CARTESIAN_POINT('Ctrl Pts',(-24.9736347594025,88.5063376968639,6.99831986027595));
#20554=CARTESIAN_POINT('Ctrl Pts',(-26.8854039328385,90.3531166132715,6.87674436937527));
#20555=CARTESIAN_POINT('Ctrl Pts',(-27.0738645596358,91.6831359850143,6.80782993355747));
#20556=CARTESIAN_POINT('Ctrl Pts',(-27.0714153574487,91.9974952077453,6.79157655282255));
#20557=CARTESIAN_POINT('Origin',(-24.,92.,12.2084234471775));
#20558=CARTESIAN_POINT('',(-27.0703857423214,92.0021357609841,8.79157655282255));
#20559=CARTESIAN_POINT('',(-27.0743674416594,91.9973209105276,8.70842344717745));
#20560=CARTESIAN_POINT('',(-27.0735,92.0000000000001,12.2084234471775));
#20561=CARTESIAN_POINT('Ctrl Pts',(-27.0743674416594,91.9973209105276,8.70842344717745));
#20562=CARTESIAN_POINT('Ctrl Pts',(-27.0670571899902,92.8027184781566,8.66667960876312));
#20563=CARTESIAN_POINT('Ctrl Pts',(-26.3319128073199,94.6359725607219,8.57227471526591));
#20564=CARTESIAN_POINT('Ctrl Pts',(-23.24859168833,95.5481002036266,8.42520876668582));
#20565=CARTESIAN_POINT('Ctrl Pts',(-20.6179387947979,93.3096959362796,8.26722560143718));
#20566=CARTESIAN_POINT('Ctrl Pts',(-21.0549304174885,89.8833499742237,8.10924243618856));
#20567=CARTESIAN_POINT('Ctrl Pts',(-24.1632008855267,88.3768791915844,7.95125927093991));
#20568=CARTESIAN_POINT('Ctrl Pts',(-26.6666765768248,89.8820749507615,7.81765294126956));
#20569=CARTESIAN_POINT('Ctrl Pts',(-27.0678018156826,91.4523692918733,7.73670766668206));
#20570=CARTESIAN_POINT('Ctrl Pts',(-27.0687739277024,92.0006038359779,7.70842344717745));
#20571=CARTESIAN_POINT('Ctrl Pts',(-27.0703857423214,92.0021357609841,8.79157655282255));
#20572=CARTESIAN_POINT('Ctrl Pts',(-27.0727139521361,92.3598775376807,8.77309592788534));
#20573=CARTESIAN_POINT('Ctrl Pts',(-26.8501666541559,93.7342139358697,8.70195424786525));
#20574=CARTESIAN_POINT('Ctrl Pts',(-24.8261377777637,95.5314377737091,8.57815151276229));
#20575=CARTESIAN_POINT('Ctrl Pts',(-21.493997547754,94.6217541894132,8.42016834751366));
#20576=CARTESIAN_POINT('Ctrl Pts',(-20.4348706359933,91.3340326759415,8.26218518226502));
#20577=CARTESIAN_POINT('Ctrl Pts',(-22.6094457936036,88.6503747732116,8.10420201701639));
#20578=CARTESIAN_POINT('Ctrl Pts',(-26.0210778474872,89.0024378034505,7.94733247386889));
#20579=CARTESIAN_POINT('Ctrl Pts',(-27.0766735052339,91.0093011164261,7.84312398580429));
#20580=CARTESIAN_POINT('Ctrl Pts',(-27.0784606140442,92.000390174329,7.79157655282255));
#20581=CARTESIAN_POINT('Origin',(-24.,92.,12.2084234471775));
#20582=CARTESIAN_POINT('',(-27.0702888275776,91.9968971804147,9.79157655282255));
#20583=CARTESIAN_POINT('',(-27.076766805402,92.0019372679897,9.70842344717746));
#20584=CARTESIAN_POINT('',(-27.0735,92.0000000000001,12.2084234471775));
#20585=CARTESIAN_POINT('',(-24.7937992825329,89.0307770462543,10.));
#20586=CARTESIAN_POINT('Ctrl Pts',(-24.7937992825329,89.0307770462543,10.));
#20587=CARTESIAN_POINT('Ctrl Pts',(-25.7762533017603,89.2934286920664,9.94733894491712));
#20588=CARTESIAN_POINT('Ctrl Pts',(-26.8759105460538,90.3312191677288,9.87786446252464));
#20589=CARTESIAN_POINT('Ctrl Pts',(-27.0726356002046,91.6716361186704,9.80838998013215));
#20590=CARTESIAN_POINT('Ctrl Pts',(-27.0702888275776,91.9968971804148,9.79157655282255));
#20591=CARTESIAN_POINT('',(-23.2043027735401,89.0256991239338,10.));
#20592=CARTESIAN_POINT('Origin',(-24.,92.,10.));
#20593=CARTESIAN_POINT('Ctrl Pts',(-23.2042983602306,89.0256873161863,10.));
#20594=CARTESIAN_POINT('Ctrl Pts',(-24.1519057059922,88.7745943606123,9.94901908464117));
#20595=CARTESIAN_POINT('Ctrl Pts',(-26.2125558943074,89.2303462451956,9.851826900367));
#20596=CARTESIAN_POINT('Ctrl Pts',(-27.0700735870785,91.1123260926059,9.75463471609281));
#20597=CARTESIAN_POINT('Ctrl Pts',(-27.076766805402,92.0019372679896,9.70842344717745));
#20598=CARTESIAN_POINT('Origin',(-24.,-92.,5.));
#20599=CARTESIAN_POINT('',(-26.5134954281454,-91.9997257032743,1.38741669750802));
#20600=CARTESIAN_POINT('',(-26.5156258041287,-92.0035321038279,1.11258330249198));
#20601=CARTESIAN_POINT('',(-26.5175,-92.,5.));
#20602=CARTESIAN_POINT('',(-25.913465996665,-90.364012796625,0.999999999999999));
#20603=CARTESIAN_POINT('Ctrl Pts',(-26.5156258041287,-92.0035321038279,
1.11258330249198));
#20604=CARTESIAN_POINT('Ctrl Pts',(-26.5104632893492,-91.410913677985,1.07505553499465));
#20605=CARTESIAN_POINT('Ctrl Pts',(-26.299221828084,-90.8151964396956,1.03752776749732));
#20606=CARTESIAN_POINT('Ctrl Pts',(-25.913465996665,-90.364012796625,0.999999999999993));
#20607=CARTESIAN_POINT('',(-26.5175,-92.,1.));
#20608=CARTESIAN_POINT('Origin',(-24.,-92.,1.));
#20609=CARTESIAN_POINT('',(-26.5175,-92.,0.));
#20610=CARTESIAN_POINT('',(-26.5175,-92.,5.));
#20611=CARTESIAN_POINT('Origin',(-24.,-92.,0.));
#20612=CARTESIAN_POINT('',(-22.0828967253639,-90.3614656719992,1.));
#20613=CARTESIAN_POINT('Origin',(-24.,-92.,1.));
#20614=CARTESIAN_POINT('Ctrl Pts',(-22.0828882653787,-90.3614597476137,
1.));
#20615=CARTESIAN_POINT('Ctrl Pts',(-22.6060429859409,-89.7523041107177,
1.05098091535882));
#20616=CARTESIAN_POINT('Ctrl Pts',(-23.4465812877835,-89.4121723295192,
1.10196183071765));
#20617=CARTESIAN_POINT('Ctrl Pts',(-24.2457357736239,-89.4905147002801,
1.15294274607647));
#20618=CARTESIAN_POINT('Ctrl Pts',(-25.0712273934265,-89.5714389416932,
1.20560380115935));
#20619=CARTESIAN_POINT('Ctrl Pts',(-25.8525625390091,-90.0988745222663,
1.25826485624222));
#20620=CARTESIAN_POINT('Ctrl Pts',(-26.2358880111547,-90.8341462678707,
1.3109259113251));
#20621=CARTESIAN_POINT('Ctrl Pts',(-26.4214828919903,-91.1901431476069,
1.33642284005274));
#20622=CARTESIAN_POINT('Ctrl Pts',(-26.5137759227878,-91.5948612017176,
1.36191976878038));
#20623=CARTESIAN_POINT('Ctrl Pts',(-26.5134954281454,-91.9997257032743,
1.38741669750802));
#20624=CARTESIAN_POINT('Origin',(-24.,-92.,5.));
#20625=CARTESIAN_POINT('',(-26.5187355654992,-92.0021096152222,2.38741669750802));
#20626=CARTESIAN_POINT('',(-26.5214126870217,-91.999354461019,2.11258330249198));
#20627=CARTESIAN_POINT('',(-26.5175,-92.,5.));
#20628=CARTESIAN_POINT('Ctrl Pts',(-26.5214126870217,-91.999354461019,2.11258330249198));
#20629=CARTESIAN_POINT('Ctrl Pts',(-26.5215323520691,-91.9641713906796,
2.11034958724147));
#20630=CARTESIAN_POINT('Ctrl Pts',(-26.5208590695048,-91.928993057358,2.10811587199095));
#20631=CARTESIAN_POINT('Ctrl Pts',(-26.5193785186672,-91.8938487960073,
2.10588215674044));
#20632=CARTESIAN_POINT('Ctrl Pts',(-26.4844737253229,-91.0653036703885,
2.05322110165756));
#20633=CARTESIAN_POINT('Ctrl Pts',(-26.0008841105951,-90.25569596213,2.00056004657468));
#20634=CARTESIAN_POINT('Ctrl Pts',(-25.2879127216155,-89.8321129915859,
1.9478989914918));
#20635=CARTESIAN_POINT('Ctrl Pts',(-24.5749413326358,-89.4085300210418,
1.89523793640892));
#20636=CARTESIAN_POINT('Ctrl Pts',(-23.6325881694044,-89.370971788212,1.84257688132604));
#20637=CARTESIAN_POINT('Ctrl Pts',(-22.8882532181424,-89.7366423255222,
1.78991582624316));
#20638=CARTESIAN_POINT('Ctrl Pts',(-22.1439182668803,-90.1023128628323,
1.73725477116029));
#20639=CARTESIAN_POINT('Ctrl Pts',(-21.5976015275877,-90.8712121702823,
1.68459371607741));
#20640=CARTESIAN_POINT('Ctrl Pts',(-21.4970123488694,-91.6942825335227,
1.63193266099453));
#20641=CARTESIAN_POINT('Ctrl Pts',(-21.3964231701512,-92.5173528967631,
1.57927160591165));
#20642=CARTESIAN_POINT('Ctrl Pts',(-21.7415615520075,-93.3945943157939,
1.52661055082878));
#20643=CARTESIAN_POINT('Ctrl Pts',(-22.3760119861909,-93.9288768514158,
1.4739494957459));
#20644=CARTESIAN_POINT('Ctrl Pts',(-23.0104624203743,-94.4631593870375,
1.42128844066302));
#20645=CARTESIAN_POINT('Ctrl Pts',(-23.934224906885,-94.6544830392504,1.36862738558014));
#20646=CARTESIAN_POINT('Ctrl Pts',(-24.7281293260075,-94.4146105531457,
1.31596633049726));
#20647=CARTESIAN_POINT('Ctrl Pts',(-25.5220337451301,-94.1747380670411,
1.26330527541438));
#20648=CARTESIAN_POINT('Ctrl Pts',(-26.1860800968646,-93.503669442619,1.21064422033151));
#20649=CARTESIAN_POINT('Ctrl Pts',(-26.4192666807451,-92.7092696340464,
1.15798316524863));
#20650=CARTESIAN_POINT('Ctrl Pts',(-26.4862778644254,-92.4809817514334,
1.14284987766308));
#20651=CARTESIAN_POINT('Ctrl Pts',(-26.5177076178372,-92.2425088846187,
1.12771659007753));
#20652=CARTESIAN_POINT('Ctrl Pts',(-26.5156258041287,-92.0035321038279,
1.11258330249198));
#20653=CARTESIAN_POINT('Ctrl Pts',(-26.5134954281454,-91.9997257032743,
1.38741669750802));
#20654=CARTESIAN_POINT('Ctrl Pts',(-26.5131965924704,-92.4310635555512,
1.41458082386326));
#20655=CARTESIAN_POINT('Ctrl Pts',(-26.4078219950606,-92.8625676332891,
1.4417449502185));
#20656=CARTESIAN_POINT('Ctrl Pts',(-26.1982523776868,-93.2354979308673,
1.46890907657374));
#20657=CARTESIAN_POINT('Ctrl Pts',(-25.7919754733646,-93.9584699376238,
1.52157013165662));
#20658=CARTESIAN_POINT('Ctrl Pts',(-24.9941058660117,-94.4613060405015,
1.57423118673949));
#20659=CARTESIAN_POINT('Ctrl Pts',(-24.1666097958723,-94.5160870716528,
1.62689224182237));
#20660=CARTESIAN_POINT('Ctrl Pts',(-23.3391137257328,-94.5708681028041,
1.67955329690525));
#20661=CARTESIAN_POINT('Ctrl Pts',(-22.4819911928069,-94.1775940622292,
1.73221435198813));
#20662=CARTESIAN_POINT('Ctrl Pts',(-21.9839037459974,-93.5145599501885,
1.78487540707101));
#20663=CARTESIAN_POINT('Ctrl Pts',(-21.4858162991878,-92.8515258381478,
1.83753646215388));
#20664=CARTESIAN_POINT('Ctrl Pts',(-21.3467639384947,-91.9187316546413,
1.89019751723676));
#20665=CARTESIAN_POINT('Ctrl Pts',(-21.6298377538243,-91.1392455882325,
1.94285857231964));
#20666=CARTESIAN_POINT('Ctrl Pts',(-21.912911569154,-90.3597595218238,1.99551962740252));
#20667=CARTESIAN_POINT('Ctrl Pts',(-22.6181115605066,-89.7335815725127,
2.0481806824854));
#20668=CARTESIAN_POINT('Ctrl Pts',(-23.425603556166,-89.5446793850464,2.10084173756827));
#20669=CARTESIAN_POINT('Ctrl Pts',(-24.2330955518254,-89.35577719758,2.15350279265115));
#20670=CARTESIAN_POINT('Ctrl Pts',(-25.1428795517915,-89.6041507719583,
2.20616384773403));
#20671=CARTESIAN_POINT('Ctrl Pts',(-25.7423598115282,-90.1771656715372,
2.25882490281691));
#20672=CARTESIAN_POINT('Ctrl Pts',(-26.2303120712523,-90.6435762172788,
2.30168883438061));
#20673=CARTESIAN_POINT('Ctrl Pts',(-26.512679103923,-91.325071055923,2.34455276594432));
#20674=CARTESIAN_POINT('Ctrl Pts',(-26.5187355654992,-92.0021096152222,
2.38741669750802));
#20675=CARTESIAN_POINT('Origin',(-24.,-92.,5.));
#20676=CARTESIAN_POINT('',(-26.5197285159005,-91.9981710495135,3.38741669750802));
#20677=CARTESIAN_POINT('',(-26.5145914825342,-91.9984414286209,3.11258330249198));
#20678=CARTESIAN_POINT('',(-26.5175,-92.,5.));
#20679=CARTESIAN_POINT('Ctrl Pts',(-26.5145914825342,-91.9984414286209,
3.11258330249198));
#20680=CARTESIAN_POINT('Ctrl Pts',(-26.5163706169191,-91.687546359978,3.0929825844054));
#20681=CARTESIAN_POINT('Ctrl Pts',(-26.4629229514308,-91.3772412892129,
3.07338186631882));
#20682=CARTESIAN_POINT('Ctrl Pts',(-26.3514583308843,-91.0894032152641,
3.05378114823224));
#20683=CARTESIAN_POINT('Ctrl Pts',(-26.0519874392331,-90.3160715138328,
3.00112009314936));
#20684=CARTESIAN_POINT('Ctrl Pts',(-25.3337325490401,-89.7049134175565,
2.94845903806649));
#20685=CARTESIAN_POINT('Ctrl Pts',(-24.52243433036,-89.5330984014484,2.89579798298361));
#20686=CARTESIAN_POINT('Ctrl Pts',(-23.7111361116798,-89.3612833853403,
2.84313692790073));
#20687=CARTESIAN_POINT('Ctrl Pts',(-22.8067945645126,-89.6288114494004,
2.79047587281785));
#20688=CARTESIAN_POINT('Ctrl Pts',(-22.219544382578,-90.2143564031656,2.73781481773497));
#20689=CARTESIAN_POINT('Ctrl Pts',(-21.6322942006435,-90.7999013569307,
2.68515376265209));
#20690=CARTESIAN_POINT('Ctrl Pts',(-21.3621353839418,-91.703463200401,2.63249270756922));
#20691=CARTESIAN_POINT('Ctrl Pts',(-21.5315888137355,-92.515256413142,2.57983165248634));
#20692=CARTESIAN_POINT('Ctrl Pts',(-21.7010422435292,-93.327049625883,2.52717059740346));
#20693=CARTESIAN_POINT('Ctrl Pts',(-22.3101079198185,-94.0470742078948,
2.47450954232058));
#20694=CARTESIAN_POINT('Ctrl Pts',(-23.0825657012675,-94.3487965351803,
2.4218484872377));
#20695=CARTESIAN_POINT('Ctrl Pts',(-23.8550234827164,-94.6505188624658,
2.36918743215482));
#20696=CARTESIAN_POINT('Ctrl Pts',(-24.7908733693249,-94.5339389350251,
2.31652637707195));
#20697=CARTESIAN_POINT('Ctrl Pts',(-25.4656883266487,-94.0519076998152,
2.26386532198907));
#20698=CARTESIAN_POINT('Ctrl Pts',(-26.1118797697061,-93.5903227036641,
2.21343798215671));
#20699=CARTESIAN_POINT('Ctrl Pts',(-26.5187111833227,-92.7936314593702,
2.16301064232434));
#20700=CARTESIAN_POINT('Ctrl Pts',(-26.5214126870217,-91.999354461019,2.11258330249198));
#20701=CARTESIAN_POINT('Ctrl Pts',(-26.5187355654992,-92.0021096152222,
2.38741669750802));
#20702=CARTESIAN_POINT('Ctrl Pts',(-26.5201198506077,-92.1568558120996,
2.39721382102719));
#20703=CARTESIAN_POINT('Ctrl Pts',(-26.5070693393431,-92.3113692075874,
2.40701094454637));
#20704=CARTESIAN_POINT('Ctrl Pts',(-26.4787395411232,-92.4630283942082,
2.41680806806554));
#20705=CARTESIAN_POINT('Ctrl Pts',(-26.3264624914741,-93.2782199925207,
2.46946912314842));
#20706=CARTESIAN_POINT('Ctrl Pts',(-25.7327318726689,-94.0109469643662,
2.5221301782313));
#20707=CARTESIAN_POINT('Ctrl Pts',(-24.9668162894688,-94.3289068537565,
2.57479123331418));
#20708=CARTESIAN_POINT('Ctrl Pts',(-24.2009007062687,-94.6468667431468,
2.62745228839706));
#20709=CARTESIAN_POINT('Ctrl Pts',(-23.2628001586737,-94.5500595500819,
2.68011334347993));
#20710=CARTESIAN_POINT('Ctrl Pts',(-22.5779584534227,-94.0823881414071,
2.73277439856281));
#20711=CARTESIAN_POINT('Ctrl Pts',(-21.8931167481717,-93.6147167327323,
2.78543545364569));
#20712=CARTESIAN_POINT('Ctrl Pts',(-21.4615338852647,-92.7761811084476,
2.83809650872857));
#20713=CARTESIAN_POINT('Ctrl Pts',(-21.4789404507956,-91.9470718995605,
2.89075756381145));
#20714=CARTESIAN_POINT('Ctrl Pts',(-21.4963470163266,-91.1179626906734,
2.94341861889432));
#20715=CARTESIAN_POINT('Ctrl Pts',(-21.9627430102955,-90.2982798971839,
2.9960796739772));
#20716=CARTESIAN_POINT('Ctrl Pts',(-22.6666096977841,-89.8597634515608,
3.04874072906008));
#20717=CARTESIAN_POINT('Ctrl Pts',(-23.3704763852727,-89.4212470059377,
3.10140178414296));
#20718=CARTESIAN_POINT('Ctrl Pts',(-24.311813766281,-89.363896908181,3.15406283922584));
#20719=CARTESIAN_POINT('Ctrl Pts',(-25.063709367653,-89.7137225058316,3.20672389430872));
#20720=CARTESIAN_POINT('Ctrl Pts',(-25.8156049690249,-90.0635481034822,
3.25938494939159));
#20721=CARTESIAN_POINT('Ctrl Pts',(-26.3780587907605,-90.8205493965401,
3.31204600447447));
#20722=CARTESIAN_POINT('Ctrl Pts',(-26.4959883797686,-91.641413330862,3.36470705955735));
#20723=CARTESIAN_POINT('Ctrl Pts',(-26.5129404282089,-91.7594102245555,
3.37227693887424));
#20724=CARTESIAN_POINT('Ctrl Pts',(-26.520707157718,-91.8787267284854,3.37984681819113));
#20725=CARTESIAN_POINT('Ctrl Pts',(-26.5197285159005,-91.9981710495135,
3.38741669750802));
#20726=CARTESIAN_POINT('Origin',(-24.,-92.,5.));
#20727=CARTESIAN_POINT('',(-26.5135839828142,-91.9996457834291,4.38741669750802));
#20728=CARTESIAN_POINT('',(-26.5160255060301,-92.0021063693209,4.11258330249198));
#20729=CARTESIAN_POINT('',(-26.5175,-92.,5.));
#20730=CARTESIAN_POINT('Ctrl Pts',(-26.5160255060301,-92.0021063693209,
4.11258330249198));
#20731=CARTESIAN_POINT('Ctrl Pts',(-26.5113088734142,-91.4165891850021,
4.07561558156934));
#20732=CARTESIAN_POINT('Ctrl Pts',(-26.30740600999,-90.828109419245,4.03864786064669));
#20733=CARTESIAN_POINT('Ctrl Pts',(-25.9337853550359,-90.381662326268,4.00168013972405));
#20734=CARTESIAN_POINT('Ctrl Pts',(-25.4015573085244,-89.7456919616342,
3.94901908464117));
#20735=CARTESIAN_POINT('Ctrl Pts',(-24.5249308580447,-89.3979402061153,
3.89635802955829));
#20736=CARTESIAN_POINT('Ctrl Pts',(-23.7014710569733,-89.4961183997274,
3.84369697447542));
#20737=CARTESIAN_POINT('Ctrl Pts',(-22.8780112559018,-89.5942965933394,
3.79103591939254));
#20738=CARTESIAN_POINT('Ctrl Pts',(-22.1077181042387,-90.1384047360825,
3.73837486430966));
#20739=CARTESIAN_POINT('Ctrl Pts',(-21.7399326972187,-90.8816805318427,
3.68571380922678));
#20740=CARTESIAN_POINT('Ctrl Pts',(-21.3721472901988,-91.624956327603,3.6330527541439));
#20741=CARTESIAN_POINT('Ctrl Pts',(-21.406869627822,-92.5673997763804,3.58039169906102));
#20742=CARTESIAN_POINT('Ctrl Pts',(-21.8283525270324,-93.2815966241557,
3.52773064397815));
#20743=CARTESIAN_POINT('Ctrl Pts',(-22.2498354262427,-93.9957934719311,
3.47506958889527));
#20744=CARTESIAN_POINT('Ctrl Pts',(-23.0580788870402,-94.4817437187044,
3.42240853381239));
#20745=CARTESIAN_POINT('Ctrl Pts',(-23.8865307275917,-94.5190607694894,
3.36974747872951));
#20746=CARTESIAN_POINT('Ctrl Pts',(-24.7149825681432,-94.5563778202745,
3.31708642364663));
#20747=CARTESIAN_POINT('Ctrl Pts',(-25.5636427884488,-94.1450616750713,
3.26442536856375));
#20748=CARTESIAN_POINT('Ctrl Pts',(-26.0476294520469,-93.4716509491765,
3.21176431348088));
#20749=CARTESIAN_POINT('Ctrl Pts',(-26.3514737668842,-93.0488871914059,
3.17870397648458));
#20750=CARTESIAN_POINT('Ctrl Pts',(-26.5115906341944,-92.5228250606093,
3.14564363948828));
#20751=CARTESIAN_POINT('Ctrl Pts',(-26.5145914825342,-91.9984414286209,
3.11258330249198));
#20752=CARTESIAN_POINT('Ctrl Pts',(-26.5197285159005,-91.9981710495135,
3.38741669750802));
#20753=CARTESIAN_POINT('Ctrl Pts',(-26.5138990821199,-92.7096599185249,
3.43250787327401));
#20754=CARTESIAN_POINT('Ctrl Pts',(-26.1977684432012,-93.4256839637041,
3.47759904904));
#20755=CARTESIAN_POINT('Ctrl Pts',(-25.664320715776,-93.8943544806311,3.52269022480598));
#20756=CARTESIAN_POINT('Ctrl Pts',(-25.0413181064947,-94.4417051204924,
3.57535127988886));
#20757=CARTESIAN_POINT('Ctrl Pts',(-24.1219075316514,-94.6516798246292,
3.62801233497174));
#20758=CARTESIAN_POINT('Ctrl Pts',(-23.3230573666226,-94.4290514695956,
3.68067339005462));
#20759=CARTESIAN_POINT('Ctrl Pts',(-22.5242072015938,-94.206423114562,3.7333344451375));
#20760=CARTESIAN_POINT('Ctrl Pts',(-21.8459174463795,-93.5511917003581,
3.78599550022038));
#20761=CARTESIAN_POINT('Ctrl Pts',(-21.5958040861176,-92.7605158612689,
3.83865655530325));
#20762=CARTESIAN_POINT('Ctrl Pts',(-21.3456907258557,-91.9698400221797,
3.89131761038613));
#20763=CARTESIAN_POINT('Ctrl Pts',(-21.5237537605461,-91.0437197582053,
3.94397866546901));
#20764=CARTESIAN_POINT('Ctrl Pts',(-22.0492385624731,-90.4021664114935,
3.99663972055189));
#20765=CARTESIAN_POINT('Ctrl Pts',(-22.5747233644,-89.7606130647817,4.04930077563477));
#20766=CARTESIAN_POINT('Ctrl Pts',(-23.4476299335634,-89.4036266353326,
4.10196183071764));
#20767=CARTESIAN_POINT('Ctrl Pts',(-24.2720802450577,-89.4931065626282,
4.15462288580052));
#20768=CARTESIAN_POINT('Ctrl Pts',(-25.096530556552,-89.5825864899237,4.2072839408834));
#20769=CARTESIAN_POINT('Ctrl Pts',(-25.8725246103771,-90.1185327739639,
4.25994499596628));
#20770=CARTESIAN_POINT('Ctrl Pts',(-26.2481358593184,-90.8578846277675,
4.31260605104916));
#20771=CARTESIAN_POINT('Ctrl Pts',(-26.4260011420294,-91.2079940211105,
4.33754293320211));
#20772=CARTESIAN_POINT('Ctrl Pts',(-26.5140862159014,-91.6037142506574,
4.36247981535507));
#20773=CARTESIAN_POINT('Ctrl Pts',(-26.5135839828142,-91.9996457834291,
4.38741669750802));
#20774=CARTESIAN_POINT('Origin',(-24.,-92.,5.));
#20775=CARTESIAN_POINT('',(-26.5184743499735,-92.0021560918536,5.38741669750802));
#20776=CARTESIAN_POINT('',(-26.5215003759084,-91.9995222402991,5.11258330249198));
#20777=CARTESIAN_POINT('',(-26.5175,-92.,5.));
#20778=CARTESIAN_POINT('Ctrl Pts',(-26.5215003759084,-91.9995222402991,
5.11258330249198));
#20779=CARTESIAN_POINT('Ctrl Pts',(-26.521569655014,-91.9731625365728,5.11090963381615));
#20780=CARTESIAN_POINT('Ctrl Pts',(-26.5211916947534,-91.9468048672737,
5.10923596514032));
#20781=CARTESIAN_POINT('Ctrl Pts',(-26.5203603409136,-91.9204615063421,
5.10756229646449));
#20782=CARTESIAN_POINT('Ctrl Pts',(-26.4942022542029,-91.0915822896134,
5.05490124138162));
#20783=CARTESIAN_POINT('Ctrl Pts',(-26.0191794168034,-90.2768685179763,
5.00224018629873));
#20784=CARTESIAN_POINT('Ctrl Pts',(-25.3107227922661,-89.8458067909394,
4.94957913121586));
#20785=CARTESIAN_POINT('Ctrl Pts',(-24.6022661677289,-89.4147450639025,
4.89691807613298));
#20786=CARTESIAN_POINT('Ctrl Pts',(-23.6603757560539,-89.3673353814657,
4.8442570210501));
#20787=CARTESIAN_POINT('Ctrl Pts',(-22.9122149332711,-89.7250788434924,
4.79159596596722));
#20788=CARTESIAN_POINT('Ctrl Pts',(-22.1640541104882,-90.0828223055191,
4.73893491088435));
#20789=CARTESIAN_POINT('Ctrl Pts',(-21.6096228765975,-90.8457189120093,
4.68627385580147));
#20790=CARTESIAN_POINT('Ctrl Pts',(-21.5003652582016,-91.667782032718,4.63361280071859));
#20791=CARTESIAN_POINT('Ctrl Pts',(-21.3911076398056,-92.4898451534267,
4.58095174563571));
#20792=CARTESIAN_POINT('Ctrl Pts',(-21.7270236369044,-93.3710747883539,
4.52829069055283));
#20793=CARTESIAN_POINT('Ctrl Pts',(-22.3557696119043,-93.9118182580198,
4.47562963546995));
#20794=CARTESIAN_POINT('Ctrl Pts',(-22.9845155869041,-94.4525617276857,
4.42296858038707));
#20795=CARTESIAN_POINT('Ctrl Pts',(-23.906091539805,-94.6528190320904,4.3703075253042));
#20796=CARTESIAN_POINT('Ctrl Pts',(-24.7025470485768,-94.4217700679434,
4.31764647022132));
#20797=CARTESIAN_POINT('Ctrl Pts',(-25.4990025573486,-94.1907211037964,
4.26498541513844));
#20798=CARTESIAN_POINT('Ctrl Pts',(-26.1703376219913,-93.5283658710978,
4.21232436005556));
#20799=CARTESIAN_POINT('Ctrl Pts',(-26.412090333041,-92.7350937678741,4.15966330497269));
#20800=CARTESIAN_POINT('Ctrl Pts',(-26.484134200614,-92.4986935632772,4.14396997081245));
#20801=CARTESIAN_POINT('Ctrl Pts',(-26.5180277850428,-92.250666913513,4.12827663665222));
#20802=CARTESIAN_POINT('Ctrl Pts',(-26.5160255060301,-92.0021063693209,
4.11258330249198));
#20803=CARTESIAN_POINT('Ctrl Pts',(-26.5135839828142,-91.9996457834291,
4.38741669750802));
#20804=CARTESIAN_POINT('Ctrl Pts',(-26.5130256132123,-92.4398320992502,
4.41514087043794));
#20805=CARTESIAN_POINT('Ctrl Pts',(-26.4029696961734,-92.8802795945302,
4.44286504336787));
#20806=CARTESIAN_POINT('Ctrl Pts',(-26.185055515175,-93.2586003180438,4.47058921629779));
#20807=CARTESIAN_POINT('Ctrl Pts',(-25.7711354780326,-93.9772067309494,
4.52325027138067));
#20808=CARTESIAN_POINT('Ctrl Pts',(-24.9680669596902,-94.4716621331935,
4.57591132646355));
#20809=CARTESIAN_POINT('Ctrl Pts',(-24.140055238289,-94.5177225612861,4.62857238154642));
#20810=CARTESIAN_POINT('Ctrl Pts',(-23.3120435168878,-94.5637829893786,
4.6812334366293));
#20811=CARTESIAN_POINT('Ctrl Pts',(-22.4590885924278,-94.1614484433196,
4.73389449171218));
#20812=CARTESIAN_POINT('Ctrl Pts',(-21.968020079816,-93.493184506096,4.78655554679506));
#20813=CARTESIAN_POINT('Ctrl Pts',(-21.4769515672042,-92.8249205688725,
4.83921660187794));
#20814=CARTESIAN_POINT('Ctrl Pts',(-21.3477694664407,-91.8907272404844,
4.89187765696082));
#20815=CARTESIAN_POINT('Ctrl Pts',(-21.6390600648163,-91.1142771383271,
4.94453871204369));
#20816=CARTESIAN_POINT('Ctrl Pts',(-21.9303506631919,-90.3378270361698,
4.99719976712657));
#20817=CARTESIAN_POINT('Ctrl Pts',(-22.6421139607067,-89.7191201602431,
5.04986082220945));
#20818=CARTESIAN_POINT('Ctrl Pts',(-23.4515531549517,-89.5387506376962,
5.10252187729233));
#20819=CARTESIAN_POINT('Ctrl Pts',(-24.2609923491968,-89.3583811151493,
5.15518293237521));
#20820=CARTESIAN_POINT('Ctrl Pts',(-25.1681074401721,-89.6163489459821,
5.20784398745809));
#20821=CARTESIAN_POINT('Ctrl Pts',(-25.7615062532208,-90.1956613164022,
5.26050504254096));
#20822=CARTESIAN_POINT('Ctrl Pts',(-26.2381977114593,-90.6610367983859,
5.30280892752998));
#20823=CARTESIAN_POINT('Ctrl Pts',(-26.5124388592754,-91.3337853316565,
5.345112812519));
#20824=CARTESIAN_POINT('Ctrl Pts',(-26.5184743499735,-92.0021560918536,
5.38741669750802));
#20825=CARTESIAN_POINT('Origin',(-24.,-92.,5.));
#20826=CARTESIAN_POINT('',(-26.5199606688991,-91.9982645762516,6.38741669750802));
#20827=CARTESIAN_POINT('',(-26.5147663248015,-91.9983410423439,6.11258330249198));
#20828=CARTESIAN_POINT('',(-26.5175,-92.,5.));
#20829=CARTESIAN_POINT('Ctrl Pts',(-26.5147663248015,-91.9983410423439,
6.11258330249198));
#20830=CARTESIAN_POINT('Ctrl Pts',(-26.5166143414574,-91.6963819206475,
6.09354263098009));
#20831=CARTESIAN_POINT('Ctrl Pts',(-26.4662620027174,-91.3950183934935,
6.07450195946819));
#20832=CARTESIAN_POINT('Ctrl Pts',(-26.3609399824778,-91.1142771205843,
6.0554612879563));
#20833=CARTESIAN_POINT('Ctrl Pts',(-26.0696493782671,-90.3378270028732,
6.00280023287342));
#20834=CARTESIAN_POINT('Ctrl Pts',(-25.3578860664943,-89.7191201145527,
5.95013917779054));
#20835=CARTESIAN_POINT('Ctrl Pts',(-24.5484468560347,-89.5387505883926,
5.89747812270766));
#20836=CARTESIAN_POINT('Ctrl Pts',(-23.739007645575,-89.3583810622326,5.84481706762479));
#20837=CARTESIAN_POINT('Ctrl Pts',(-22.8318925364284,-89.616348898233,5.79215601254191));
#20838=CARTESIAN_POINT('Ctrl Pts',(-22.2384937114928,-90.1956612802579,
5.73949495745903));
#20839=CARTESIAN_POINT('Ctrl Pts',(-21.6450948865572,-90.7749736622827,
5.68683390237615));
#20840=CARTESIAN_POINT('Ctrl Pts',(-21.3654123458325,-91.6756305903319,
5.63417284729328));
#20841=CARTESIAN_POINT('Ctrl Pts',(-21.5262868946164,-92.4891687768701,
5.5815117922104));
#20842=CARTESIAN_POINT('Ctrl Pts',(-21.6871614434003,-93.3027069634083,
5.52885073712752));
#20843=CARTESIAN_POINT('Ctrl Pts',(-22.2885930816928,-94.0291264084354,
5.47618968204464));
#20844=CARTESIAN_POINT('Ctrl Pts',(-23.0578222974529,-94.3389834964905,
5.42352862696176));
#20845=CARTESIAN_POINT('Ctrl Pts',(-23.8270515132129,-94.6488405845455,
5.37086757187888));
#20846=CARTESIAN_POINT('Ctrl Pts',(-24.7640783064405,-94.5421353156285,
5.318206516796));
#20847=CARTESIAN_POINT('Ctrl Pts',(-25.4439450350434,-94.0672603502598,
5.26554546171313));
#20848=CARTESIAN_POINT('Ctrl Pts',(-26.1022043035296,-93.6074778161617,
5.21455807530608));
#20849=CARTESIAN_POINT('Ctrl Pts',(-26.5193898264469,-92.8025559702575,
5.16357068889903));
#20850=CARTESIAN_POINT('Ctrl Pts',(-26.5215003759084,-91.9995222402991,
5.11258330249198));
#20851=CARTESIAN_POINT('Ctrl Pts',(-26.5184743499735,-92.0021560918536,
5.38741669750802));
#20852=CARTESIAN_POINT('Ctrl Pts',(-26.5199520063112,-92.1657918820634,
5.39777386760188));
#20853=CARTESIAN_POINT('Ctrl Pts',(-26.5053532314693,-92.3291652655503,
5.40813103769574));
#20854=CARTESIAN_POINT('Ctrl Pts',(-26.4737130558304,-92.4891687670711,
5.4184882077896));
#20855=CARTESIAN_POINT('Ctrl Pts',(-26.3128385102691,-93.3027069373125,
5.47114926287248));
#20856=CARTESIAN_POINT('Ctrl Pts',(-25.7114068840244,-94.0291263677881,
5.52381031795536));
#20857=CARTESIAN_POINT('Ctrl Pts',(-24.9421776836735,-94.3389834496361,
5.57647137303823));
#20858=CARTESIAN_POINT('Ctrl Pts',(-24.1729484833226,-94.6488405314842,
5.62913242812111));
#20859=CARTESIAN_POINT('Ctrl Pts',(-23.2359217088655,-94.5421352647047,
5.68179348320399));
#20860=CARTESIAN_POINT('Ctrl Pts',(-22.5560549938817,-94.0672603088487,
5.73445453828687));
#20861=CARTESIAN_POINT('Ctrl Pts',(-21.8761882788978,-93.5923853529927,
5.78711559336975));
#20862=CARTESIAN_POINT('Ctrl Pts',(-21.4534816233873,-92.7493407080601,
5.83977664845262));
#20863=CARTESIAN_POINT('Ctrl Pts',(-21.479639709574,-91.9204615079354,5.8924377035355));
#20864=CARTESIAN_POINT('Ctrl Pts',(-21.5057977957607,-91.0915823078107,
5.94509875861838));
#20865=CARTESIAN_POINT('Ctrl Pts',(-21.9808206236446,-90.276868552494,5.99775981370126));
#20866=CARTESIAN_POINT('Ctrl Pts',(-22.6892772339901,-89.8458068340921,
6.05042086878414));
#20867=CARTESIAN_POINT('Ctrl Pts',(-23.3977338443356,-89.4147451156901,
6.10308192386701));
#20868=CARTESIAN_POINT('Ctrl Pts',(-24.3396242371427,-89.3673354342031,
6.15574297894989));
#20869=CARTESIAN_POINT('Ctrl Pts',(-25.0877850449385,-89.7250788890635,
6.20840403403277));
#20870=CARTESIAN_POINT('Ctrl Pts',(-25.8359458527343,-90.0828223439238,
6.26106508911565));
#20871=CARTESIAN_POINT('Ctrl Pts',(-26.3903770755186,-90.8457189351315,
6.31372614419853));
#20872=CARTESIAN_POINT('Ctrl Pts',(-26.499634691726,-91.6677820393728,6.36638719928141));
#20873=CARTESIAN_POINT('Ctrl Pts',(-26.5141782213651,-91.7772087277519,
6.37339703202361));
#20874=CARTESIAN_POINT('Ctrl Pts',(-26.5208337745228,-91.8876837803117,
6.38040686476582));
#20875=CARTESIAN_POINT('Ctrl Pts',(-26.5199606688991,-91.9982645762516,
6.38741669750802));
#20876=CARTESIAN_POINT('Origin',(-24.,-92.,5.));
#20877=CARTESIAN_POINT('',(-26.5136290410546,-91.9995053986546,7.38741669750802));
#20878=CARTESIAN_POINT('',(-26.5157926212741,-92.0020516723221,7.11258330249198));
#20879=CARTESIAN_POINT('',(-26.5175,-92.,5.));
#20880=CARTESIAN_POINT('Ctrl Pts',(-26.5157926212741,-92.0020516723221,
7.11258330249198));
#20881=CARTESIAN_POINT('Ctrl Pts',(-26.5112988583661,-91.4252696399995,
7.07617562814402));
#20882=CARTESIAN_POINT('Ctrl Pts',(-26.3140599311548,-90.8457098245431,
7.03976795379607));
#20883=CARTESIAN_POINT('Ctrl Pts',(-25.9507614766046,-90.4021663794855,
7.00336027944811));
#20884=CARTESIAN_POINT('Ctrl Pts',(-25.4252766641513,-89.760613019922,6.95069922436523));
#20885=CARTESIAN_POINT('Ctrl Pts',(-24.5523700775015,-89.4036265833224,
6.89803816928235));
#20886=CARTESIAN_POINT('Ctrl Pts',(-23.7279197494918,-89.4931065124105,
6.84537711419947));
#20887=CARTESIAN_POINT('Ctrl Pts',(-22.9034694214822,-89.5825864414987,
6.79271605911659));
#20888=CARTESIAN_POINT('Ctrl Pts',(-22.1274753521126,-90.1185327362745,
6.74005500403372));
#20889=CARTESIAN_POINT('Ctrl Pts',(-21.7518640956471,-90.8578846048887,
6.68739394895084));
#20890=CARTESIAN_POINT('Ctrl Pts',(-21.3762528391816,-91.5972364735028,
6.63473289386796));
#20891=CARTESIAN_POINT('Ctrl Pts',(-21.4010243956202,-92.5399939159553,
6.58207183878508));
#20892=CARTESIAN_POINT('Ctrl Pts',(-21.8149444410541,-93.258600343256,6.5294107837022));
#20893=CARTESIAN_POINT('Ctrl Pts',(-22.2288644864881,-93.9772067705567,
6.47674972861932));
#20894=CARTESIAN_POINT('Ctrl Pts',(-23.0319330209176,-94.4716621827056,
6.42408867353644));
#20895=CARTESIAN_POINT('Ctrl Pts',(-23.8599447589054,-94.5177226117208,
6.37142761845357));
#20896=CARTESIAN_POINT('Ctrl Pts',(-24.6879564968933,-94.563783040736,6.31876656337069));
#20897=CARTESIAN_POINT('Ctrl Pts',(-25.5409114384397,-94.1614484866175,
6.26610550828781));
#20898=CARTESIAN_POINT('Ctrl Pts',(-26.0319799608885,-93.4931845360073,
6.21344445320493));
#20899=CARTESIAN_POINT('Ctrl Pts',(-26.3454927087509,-93.0665449574646,
6.17982406963395));
#20900=CARTESIAN_POINT('Ctrl Pts',(-26.5115032555984,-92.531514543491,6.14620368606296));
#20901=CARTESIAN_POINT('Ctrl Pts',(-26.5147663248015,-91.9983410423439,
6.11258330249198));
#20902=CARTESIAN_POINT('Ctrl Pts',(-26.5199606688991,-91.9982645762516,
6.38741669750802));
#20903=CARTESIAN_POINT('Ctrl Pts',(-26.5142746075592,-92.7184170660063,
6.43306791984869));
#20904=CARTESIAN_POINT('Ctrl Pts',(-26.1892825133498,-93.4430543518201,
6.47871914218937));
#20905=CARTESIAN_POINT('Ctrl Pts',(-25.6442303551587,-93.9118182197226,
6.52437036453004));
#20906=CARTESIAN_POINT('Ctrl Pts',(-25.0154843927538,-94.4525616785562,
6.57703141961292));
#20907=CARTESIAN_POINT('Ctrl Pts',(-24.0939084583138,-94.6528189789487,
6.6296924746958));
#20908=CARTESIAN_POINT('Ctrl Pts',(-23.2974529654966,-94.4217700194304,
6.68235352977868));
#20909=CARTESIAN_POINT('Ctrl Pts',(-22.5009974726793,-94.1907210599122,
6.73501458486155));
#20910=CARTESIAN_POINT('Ctrl Pts',(-21.8296624214848,-93.5283658404832,
6.78767563994443));
#20911=CARTESIAN_POINT('Ctrl Pts',(-21.5879097152778,-92.7350937531496,
6.84033669502731));
#20912=CARTESIAN_POINT('Ctrl Pts',(-21.3461570090709,-91.941821665816,6.89299775011018));
#20913=CARTESIAN_POINT('Ctrl Pts',(-21.5339866478515,-91.0176327105778,
6.94565880519306));
#20914=CARTESIAN_POINT('Ctrl Pts',(-22.0662146837015,-90.381662358685,6.99831986027594));
#20915=CARTESIAN_POINT('Ctrl Pts',(-22.5984427195515,-89.7456920067921,
7.05098091535882));
#20916=CARTESIAN_POINT('Ctrl Pts',(-23.4750691524708,-89.3979402582445,
7.1036419704417));
#20917=CARTESIAN_POINT('Ctrl Pts',(-24.2985289370467,-89.4961184498875,
7.15630302552458));
#20918=CARTESIAN_POINT('Ctrl Pts',(-25.1219887216225,-89.5942966415305,
7.20896408060745));
#20919=CARTESIAN_POINT('Ctrl Pts',(-25.8922818578547,-90.1384047733641,
7.26162513569033));
#20920=CARTESIAN_POINT('Ctrl Pts',(-26.2600672575076,-90.8816805542397,
7.31428619077321));
#20921=CARTESIAN_POINT('Ctrl Pts',(-26.4303153507392,-91.2257433815264,
7.33866302635148));
#20922=CARTESIAN_POINT('Ctrl Pts',(-26.5143152963871,-91.6124832538171,
7.36303986192975));
#20923=CARTESIAN_POINT('Ctrl Pts',(-26.5136290410546,-91.9995053986546,
7.38741669750802));
#20924=CARTESIAN_POINT('Origin',(-24.,-92.,5.));
#20925=CARTESIAN_POINT('',(-26.5182106813093,-92.0021944371302,8.38741669750803));
#20926=CARTESIAN_POINT('',(-26.5215633824187,-91.9996804087644,8.11258330249198));
#20927=CARTESIAN_POINT('',(-26.5175,-92.,5.));
#20928=CARTESIAN_POINT('Ctrl Pts',(-26.5215633824187,-91.9996804087644,
8.11258330249198));
#20929=CARTESIAN_POINT('Ctrl Pts',(-26.5215950065109,-91.9821424208031,
8.11146968039083));
#20930=CARTESIAN_POINT('Ctrl Pts',(-26.5214276959298,-91.9646050519462,
8.11035605828969));
#20931=CARTESIAN_POINT('Ctrl Pts',(-26.5210595996876,-91.9470718985316,
8.10924243618854));
#20932=CARTESIAN_POINT('Ctrl Pts',(-26.5036530337928,-91.1179626730645,
8.05658138110567));
#20933=CARTESIAN_POINT('Ctrl Pts',(-26.0372570305162,-90.2982798630938,
8.00392032602279));
#20934=CARTESIAN_POINT('Ctrl Pts',(-25.333390328936,-89.8597634086715,7.95125927093992));
#20935=CARTESIAN_POINT('Ctrl Pts',(-24.6295236273558,-89.4212469542493,
7.89859821585704));
#20936=CARTESIAN_POINT('Ctrl Pts',(-23.688186227472,-89.3638968553754,7.84593716077416));
#20937=CARTESIAN_POINT('Ctrl Pts',(-22.9362906110337,-89.7137224600414,
7.79327610569128));
#20938=CARTESIAN_POINT('Ctrl Pts',(-22.1843949945955,-90.0635480647073,
7.7406150506084));
#20939=CARTESIAN_POINT('Ctrl Pts',(-21.6219411616028,-90.8205493729132,
7.68795399552552));
#20940=CARTESIAN_POINT('Ctrl Pts',(-21.5040115702347,-91.6414133236746,
7.63529294044264));
#20941=CARTESIAN_POINT('Ctrl Pts',(-21.3860819788666,-92.462277274436,7.58263188535977));
#20942=CARTESIAN_POINT('Ctrl Pts',(-21.7126766291231,-93.347003867753,7.52997083027689));
#20943=CARTESIAN_POINT('Ctrl Pts',(-22.3356792508831,-93.8943545185808,
7.47730977519401));
#20944=CARTESIAN_POINT('Ctrl Pts',(-22.9586818726432,-94.4417051694086,
7.42464872011113));
#20945=CARTESIAN_POINT('Ctrl Pts',(-23.8780924659067,-94.6516798777473,
7.37198766502825));
#20946=CARTESIAN_POINT('Ctrl Pts',(-24.6769426469386,-94.429051518253,7.31932660994537));
#20947=CARTESIAN_POINT('Ctrl Pts',(-25.4757928279705,-94.2064231587587,
7.2666655548625));
#20948=CARTESIAN_POINT('Ctrl Pts',(-26.1540825967709,-93.5511917314314,
7.21400449977962));
#20949=CARTESIAN_POINT('Ctrl Pts',(-26.4041959620427,-92.760515876504,7.16134344469674));
#20950=CARTESIAN_POINT('Ctrl Pts',(-26.4813912963606,-92.516480589178,7.14509006396182));
#20951=CARTESIAN_POINT('Ctrl Pts',(-26.5177987598365,-92.25954293317,7.1288366832269));
#20952=CARTESIAN_POINT('Ctrl Pts',(-26.5157926212741,-92.0020516723221,
7.11258330249198));
#20953=CARTESIAN_POINT('Ctrl Pts',(-26.5136290410546,-91.9995053986546,
7.38741669750802));
#20954=CARTESIAN_POINT('Ctrl Pts',(-26.5128327852651,-92.4485636557274,
7.41570091701263));
#20955=CARTESIAN_POINT('Ctrl Pts',(-26.3980256245316,-92.8980019292389,
7.44398513651724));
#20956=CARTESIAN_POINT('Ctrl Pts',(-26.1716474294659,-93.2815965984927,
7.47226935602185));
#20957=CARTESIAN_POINT('Ctrl Pts',(-25.7501645386979,-93.9957934319524,
7.52493041110472));
#20958=CARTESIAN_POINT('Ctrl Pts',(-24.9419210940886,-94.4817436689544,
7.5775914661876));
#20959=CARTESIAN_POINT('Ctrl Pts',(-24.1134692701342,-94.5190607190089,
7.63025252127048));
#20960=CARTESIAN_POINT('Ctrl Pts',(-23.2850174461799,-94.5563777690633,
7.68291357635336));
#20961=CARTESIAN_POINT('Ctrl Pts',(-22.4363572428804,-94.1450616321701,
7.73557463143624));
#20962=CARTESIAN_POINT('Ctrl Pts',(-21.9523705889737,-93.4716509197329,
7.78823568651911));
#20963=CARTESIAN_POINT('Ctrl Pts',(-21.468383935067,-92.7982402072957,7.840896741602));
#20964=CARTESIAN_POINT('Ctrl Pts',(-21.3490708305531,-91.8627349193144,
7.89355779668488));
#20965=CARTESIAN_POINT('Ctrl Pts',(-21.6485417162138,-91.0894032334354,
7.94621885176776));
#20966=CARTESIAN_POINT('Ctrl Pts',(-21.9480126018744,-90.3160715475563,
7.99887990685063));
#20967=CARTESIAN_POINT('Ctrl Pts',(-22.6662674777097,-89.7049134637794,
8.05154096193351));
#20968=CARTESIAN_POINT('Ctrl Pts',(-23.4775656801192,-89.5330984509984,
8.10420201701639));
#20969=CARTESIAN_POINT('Ctrl Pts',(-24.2888638825287,-89.3612834382173,
8.15686307209926));
#20970=CARTESIAN_POINT('Ctrl Pts',(-25.1932054115124,-89.628811496432,8.20952412718214));
#20971=CARTESIAN_POINT('Ctrl Pts',(-25.7804555817247,-90.2143564386821,
8.26218518226502));
#20972=CARTESIAN_POINT('Ctrl Pts',(-26.2459623243365,-90.6785114658679,
8.30392902067935));
#20973=CARTESIAN_POINT('Ctrl Pts',(-26.5122228629259,-91.3424942562717,
8.34567285909369));
#20974=CARTESIAN_POINT('Ctrl Pts',(-26.5182106813093,-92.0021944371302,
8.38741669750803));
#20975=CARTESIAN_POINT('Origin',(-24.,-92.,5.));
#20976=CARTESIAN_POINT('',(-26.5201759878003,-91.9984131478585,9.38741669750802));
#20977=CARTESIAN_POINT('',(-26.5149492652116,-91.9982505980886,9.11258330249198));
#20978=CARTESIAN_POINT('',(-26.5175,-92.,5.));
#20979=CARTESIAN_POINT('',(-22.0865340033349,-90.364012796625,10.));
#20980=CARTESIAN_POINT('Ctrl Pts',(-26.5201759878003,-91.9984131478585,
9.38741669750802));
#20981=CARTESIAN_POINT('Ctrl Pts',(-26.5146936217042,-92.7270926513296,
9.43362796642338));
#20982=CARTESIAN_POINT('Ctrl Pts',(-26.180732565303,-93.4600317456745,9.47983923533874));
#20983=CARTESIAN_POINT('Ctrl Pts',(-25.6239879633605,-93.9288767806186,
9.5260505042541));
#20984=CARTESIAN_POINT('Ctrl Pts',(-24.9895375611504,-94.4631593223022,
9.57871155933697));
#20985=CARTESIAN_POINT('Ctrl Pts',(-24.0657751669118,-94.6544830596338,
9.63137261441985));
#20986=CARTESIAN_POINT('Ctrl Pts',(-23.2718706971314,-94.4146105241972,
9.68403366950273));
#20987=CARTESIAN_POINT('Ctrl Pts',(-22.4779662273509,-94.1747379887606,
9.73669472458561));
#20988=CARTESIAN_POINT('Ctrl Pts',(-21.8139196820286,-93.5036691805557,
9.78935577966849));
#20989=CARTESIAN_POINT('Ctrl Pts',(-21.5807331050278,-92.7092693915533,
9.84201683475137));
#20990=CARTESIAN_POINT('Ctrl Pts',(-21.347546528027,-91.9148696025508,9.89467788983425));
#20991=CARTESIAN_POINT('Ctrl Pts',(-21.5452199193478,-90.9971388327508,
9.94733894491712));
#20992=CARTESIAN_POINT('Ctrl Pts',(-22.0865340033349,-90.364012796625,10.));
#20993=CARTESIAN_POINT('',(-25.9171033105362,-90.3614656677959,10.));
#20994=CARTESIAN_POINT('Origin',(-24.,-92.,10.));
#20995=CARTESIAN_POINT('Ctrl Pts',(-25.9171117712833,-90.3614597429255,
10.));
#20996=CARTESIAN_POINT('Ctrl Pts',(-25.3939570615584,-89.7523041616072,
9.94901908464118));
#20997=CARTESIAN_POINT('Ctrl Pts',(-24.5534187329285,-89.4121722649682,
9.89803816928235));
#20998=CARTESIAN_POINT('Ctrl Pts',(-23.7542642249036,-89.4905146133597,
9.84705725392353));
#20999=CARTESIAN_POINT('Ctrl Pts',(-22.9287725821855,-89.5714388316664,
9.79439619884065));
#21000=CARTESIAN_POINT('Ctrl Pts',(-22.1474374185984,-90.0988744884397,
9.74173514375777));
#21001=CARTESIAN_POINT('Ctrl Pts',(-21.7641119401365,-90.8341462635555,
9.68907408867489));
#21002=CARTESIAN_POINT('Ctrl Pts',(-21.3807864616747,-91.5694180386713,
9.63641303359202));
#21003=CARTESIAN_POINT('Ctrl Pts',(-21.3954706683382,-92.5125259321295,
9.58375197850914));
#21004=CARTESIAN_POINT('Ctrl Pts',(-21.8017475811356,-93.2354979451803,
9.53109092342626));
#21005=CARTESIAN_POINT('Ctrl Pts',(-22.2080244939329,-93.9584699582311,
9.47842986834338));
#21006=CARTESIAN_POINT('Ctrl Pts',(-23.0058941128643,-94.4613060908746,
9.4257688132605));
#21007=CARTESIAN_POINT('Ctrl Pts',(-23.8333901989263,-94.5160871276519,
9.37310775817762));
#21008=CARTESIAN_POINT('Ctrl Pts',(-24.6608862849884,-94.5708681644292,
9.32044670309475));
#21009=CARTESIAN_POINT('Ctrl Pts',(-25.5180088381812,-94.1775941053403,
9.26778564801187));
#21010=CARTESIAN_POINT('Ctrl Pts',(-26.0160962955285,-93.5145599775471,
9.21512459292899));
#21011=CARTESIAN_POINT('Ctrl Pts',(-26.339387264832,-93.0842079526292,9.18094416278332));
#21012=CARTESIAN_POINT('Ctrl Pts',(-26.5114221549398,-92.5402100730638,
9.14676373263765));
#21013=CARTESIAN_POINT('Ctrl Pts',(-26.5149492652116,-91.9982505980886,
9.11258330249198));
#21014=CARTESIAN_POINT('Origin',(-24.,-92.,12.2084234471775));
#21015=CARTESIAN_POINT('',(-27.0782768196867,-91.9992118911386,1.79157655282254));
#21016=CARTESIAN_POINT('',(-27.0686110023456,-91.9996651237392,1.70842344717745));
#21017=CARTESIAN_POINT('',(-27.0735,-91.9999999999999,12.2084234471775));
#21018=CARTESIAN_POINT('',(-23.2062007174672,-94.9692229537457,0.999999999999999));
#21019=CARTESIAN_POINT('Ctrl Pts',(-27.0686110023456,-91.9996651237392,
1.70842344717745));
#21020=CARTESIAN_POINT('Ctrl Pts',(-27.0689534453578,-91.5053846687106,
1.68292651844981));
#21021=CARTESIAN_POINT('Ctrl Pts',(-26.7235567931003,-89.9907712706007,
1.6047685346393));
#21022=CARTESIAN_POINT('Ctrl Pts',(-24.3539161166825,-88.3911596148569,
1.4739494957459));
#21023=CARTESIAN_POINT('Ctrl Pts',(-21.1687759971456,-89.7301450507159,
1.31596633049727));
#21024=CARTESIAN_POINT('Ctrl Pts',(-20.5566856051374,-93.1332975040884,
1.15798316524863));
#21025=CARTESIAN_POINT('Ctrl Pts',(-22.2237466982397,-94.7065713079336,
1.05266105508288));
#21026=CARTESIAN_POINT('Ctrl Pts',(-23.2062007174672,-94.9692229537457,
0.999999999999999));
#21027=CARTESIAN_POINT('',(-24.7937992825329,-94.9692229537457,0.999999999999999));
#21028=CARTESIAN_POINT('Origin',(-24.,-92.,0.999999999999999));
#21029=CARTESIAN_POINT('Ctrl Pts',(-27.0782768196867,-91.9992118911386,
1.79157655282254));
#21030=CARTESIAN_POINT('Ctrl Pts',(-27.0784229132411,-91.9562584982139,
1.78934283757203));
#21031=CARTESIAN_POINT('Ctrl Pts',(-27.058222313234,-90.9007975699364,1.73444806723864));
#21032=CARTESIAN_POINT('Ctrl Pts',(-25.852395087606,-88.8820465732967,1.62689224182237));
#21033=CARTESIAN_POINT('Ctrl Pts',(-22.4009681396119,-88.7444872144855,
1.46890907657374));
#21034=CARTESIAN_POINT('Ctrl Pts',(-20.4000491745082,-91.5606286501729,
1.3109259113251));
#21035=CARTESIAN_POINT('Ctrl Pts',(-21.6506964041098,-94.7394102869818,
1.15462288580052));
#21036=CARTESIAN_POINT('Ctrl Pts',(-23.8480946426715,-95.2254055619768,
1.05098091535882));
#21037=CARTESIAN_POINT('Ctrl Pts',(-24.7957017813267,-94.9743128096467,
1.));
#21038=CARTESIAN_POINT('Origin',(-24.,-92.,12.2084234471775));
#21039=CARTESIAN_POINT('',(-27.0699491247542,-91.9980972118633,2.79157655282254));
#21040=CARTESIAN_POINT('',(-27.075008445109,-92.0025755322285,2.70842344717745));
#21041=CARTESIAN_POINT('',(-27.0735,-91.9999999999999,12.2084234471775));
#21042=CARTESIAN_POINT('Ctrl Pts',(-27.075008445109,-92.0025755322285,2.70842344717745));
#21043=CARTESIAN_POINT('Ctrl Pts',(-27.0676143896354,-91.1760102841626,
2.66555951561375));
#21044=CARTESIAN_POINT('Ctrl Pts',(-26.2993641383815,-89.3218328468575,
2.57003452896717));
#21045=CARTESIAN_POINT('Ctrl Pts',(-23.1738621865499,-88.4685620798055,
2.42184848723771));
#21046=CARTESIAN_POINT('Ctrl Pts',(-20.5910234496019,-90.7619776832305,
2.26386532198907));
#21047=CARTESIAN_POINT('Ctrl Pts',(-21.1003113510007,-94.1783942746989,
2.10588215674044));
#21048=CARTESIAN_POINT('Ctrl Pts',(-24.2395758256157,-95.6187848570707,
1.94789899149181));
#21049=CARTESIAN_POINT('Ctrl Pts',(-26.690200871183,-94.074343589762,1.81541275497081));
#21050=CARTESIAN_POINT('Ctrl Pts',(-27.0682461676098,-92.5262656754663,
1.73558757353269));
#21051=CARTESIAN_POINT('Ctrl Pts',(-27.0686110023456,-91.9996651237392,
1.70842344717745));
#21052=CARTESIAN_POINT('Ctrl Pts',(-27.0699491247542,-91.9980972118633,
2.79157655282254));
#21053=CARTESIAN_POINT('Ctrl Pts',(-27.0721211881235,-91.6185397169383,
2.77197583473597));
#21054=CARTESIAN_POINT('Ctrl Pts',(-26.8315580332634,-90.2218843885842,
2.69971406156651));
#21055=CARTESIAN_POINT('Ctrl Pts',(-24.7514083751606,-88.4518994955133,
2.57479123331418));
#21056=CARTESIAN_POINT('Ctrl Pts',(-21.4392013302128,-89.4317376344075,
2.41680806806554));
#21057=CARTESIAN_POINT('Ctrl Pts',(-20.4497278964894,-92.7410889661721,
2.25882490281691));
#21058=CARTESIAN_POINT('Ctrl Pts',(-22.6804687378898,-95.3782236865055,
2.10084173756827));
#21059=CARTESIAN_POINT('Ctrl Pts',(-26.0596142672113,-94.9572795305498,
1.94509228757015));
#21060=CARTESIAN_POINT('Ctrl Pts',(-27.0749786780307,-92.9689081590363,
1.84200389265491));
#21061=CARTESIAN_POINT('Ctrl Pts',(-27.0782768196867,-91.9992118911386,
1.79157655282254));
#21062=CARTESIAN_POINT('Origin',(-24.,-92.,12.2084234471775));
#21063=CARTESIAN_POINT('',(-27.0716998581066,-92.0025715694568,3.79157655282255));
#21064=CARTESIAN_POINT('',(-27.0762206925998,-91.9977671184427,3.70842344717745));
#21065=CARTESIAN_POINT('',(-27.0735,-91.9999999999999,12.2084234471775));
#21066=CARTESIAN_POINT('Ctrl Pts',(-27.0762206925998,-91.9977671184427,
3.70842344717745));
#21067=CARTESIAN_POINT('Ctrl Pts',(-27.0774154713987,-91.8519430387287,
3.70085356786056));
#21068=CARTESIAN_POINT('Ctrl Pts',(-27.0019701064919,-90.6929124367373,
3.6406226334608));
#21069=CARTESIAN_POINT('Ctrl Pts',(-25.5299146181504,-88.7116868408497,
3.52773064397815));
#21070=CARTESIAN_POINT('Ctrl Pts',(-22.0822080355935,-88.9217351333484,
3.36974747872952));
#21071=CARTESIAN_POINT('Ctrl Pts',(-20.3740037605626,-91.92387423856,3.21176431348088));
#21072=CARTESIAN_POINT('Ctrl Pts',(-21.9547027823836,-94.99506300667,3.05378114823225));
#21073=CARTESIAN_POINT('Ctrl Pts',(-25.3905542616683,-95.349625359661,2.89579798298362));
#21074=CARTESIAN_POINT('Ctrl Pts',(-26.9751245860296,-93.3940964065108,
2.78067874929868));
#21075=CARTESIAN_POINT('Ctrl Pts',(-27.076698455151,-92.1914980490519,2.71822057069663));
#21076=CARTESIAN_POINT('Ctrl Pts',(-27.075008445109,-92.0025755322285,2.70842344717745));
#21077=CARTESIAN_POINT('Ctrl Pts',(-27.0716998581066,-92.0025715694568,
3.79157655282254));
#21078=CARTESIAN_POINT('Ctrl Pts',(-27.0659415382079,-91.2877405601207,
3.7546088318999));
#21079=CARTESIAN_POINT('Ctrl Pts',(-26.4623934875611,-89.5458532246352,
3.66498005589438));
#21080=CARTESIAN_POINT('Ctrl Pts',(-23.5706310215098,-88.3987107062197,
3.52269022480598));
#21081=CARTESIAN_POINT('Ctrl Pts',(-20.7493845448822,-90.3915405493825,
3.36470705955735));
#21082=CARTESIAN_POINT('Ctrl Pts',(-20.876557261488,-93.8432981737925,3.20672389430871));
#21083=CARTESIAN_POINT('Ctrl Pts',(-23.8367991007265,-95.6231211133646,
3.04874072906008));
#21084=CARTESIAN_POINT('Ctrl Pts',(-26.5594316628929,-94.3035556341771,
2.91035828189802));
#21085=CARTESIAN_POINT('Ctrl Pts',(-27.0662855269897,-92.6382930779672,
2.82463688981884));
#21086=CARTESIAN_POINT('Ctrl Pts',(-27.0699491247542,-91.9980972118633,
2.79157655282254));
#21087=CARTESIAN_POINT('Origin',(-24.,-92.,12.2084234471775));
#21088=CARTESIAN_POINT('',(-27.0783838750167,-91.9994167251476,4.79157655282255));
#21089=CARTESIAN_POINT('',(-27.0687191146691,-91.9995675532748,4.70842344717746));
#21090=CARTESIAN_POINT('',(-27.0735,-91.9999999999999,12.2084234471775));
#21091=CARTESIAN_POINT('Ctrl Pts',(-27.0687191146691,-91.9995675532748,
4.70842344717746));
#21092=CARTESIAN_POINT('Ctrl Pts',(-27.0693322679535,-91.5161929491144,
4.6834865650245));
#21093=CARTESIAN_POINT('Ctrl Pts',(-26.7346951702922,-90.0128432522753,
4.60588862778867));
#21094=CARTESIAN_POINT('Ctrl Pts',(-24.3913282785028,-88.3943788173915,
4.47562963546995));
#21095=CARTESIAN_POINT('Ctrl Pts',(-21.1942537915233,-89.7018637718047,
4.31764647022133));
#21096=CARTESIAN_POINT('Ctrl Pts',(-20.5420868753907,-93.0938367187666,
4.15966330497269));
#21097=CARTESIAN_POINT('Ctrl Pts',(-23.026365202284,-95.4936624405808,4.00168013972406));
#21098=CARTESIAN_POINT('Ctrl Pts',(-26.2324121355514,-94.7614664286128,
3.85126685379231));
#21099=CARTESIAN_POINT('Ctrl Pts',(-27.0691038049237,-92.8663911656747,
3.75351462294344));
#21100=CARTESIAN_POINT('Ctrl Pts',(-27.0762206925998,-91.9977671184427,
3.70842344717745));
#21101=CARTESIAN_POINT('Ctrl Pts',(-27.0783838750167,-91.9994167251476,
4.79157655282255));
#21102=CARTESIAN_POINT('Ctrl Pts',(-27.0784684546913,-91.9672353748387,
4.78990288414672));
#21103=CARTESIAN_POINT('Ctrl Pts',(-27.0634882463523,-90.9225663485135,
4.73556816038801));
#21104=CARTESIAN_POINT('Ctrl Pts',(-25.8851897703268,-88.9016614152428,
4.62857238154642));
#21105=CARTESIAN_POINT('Ctrl Pts',(-22.435457678629,-88.7280205108105,4.4705892162978));
#21106=CARTESIAN_POINT('Ctrl Pts',(-20.4048188734298,-91.5221766816716,
4.31260605104916));
#21107=CARTESIAN_POINT('Ctrl Pts',(-21.6351320616123,-94.7497349135865,
4.15462288580052));
#21108=CARTESIAN_POINT('Ctrl Pts',(-25.0104611872221,-95.4831897200468,
3.99663972055189));
#21109=CARTESIAN_POINT('Ctrl Pts',(-26.8939121321552,-93.6249319667866,
3.8756242762259));
#21110=CARTESIAN_POINT('Ctrl Pts',(-27.0741443484921,-92.3060277095063,
3.80726988698278));
#21111=CARTESIAN_POINT('Ctrl Pts',(-27.0716998581066,-92.0025715694568,
3.79157655282254));
#21112=CARTESIAN_POINT('Origin',(-24.,-92.,12.2084234471775));
#21113=CARTESIAN_POINT('',(-27.0701625816395,-91.9979746548734,5.79157655282255));
#21114=CARTESIAN_POINT('',(-27.0746895390839,-92.0026322734109,5.70842344717746));
#21115=CARTESIAN_POINT('',(-27.0735,-91.9999999999999,12.2084234471775));
#21116=CARTESIAN_POINT('Ctrl Pts',(-27.0746895390839,-92.0026322734109,
5.70842344717746));
#21117=CARTESIAN_POINT('Ctrl Pts',(-27.0673210859912,-91.1866491427393,
5.66611956218844));
#21118=CARTESIAN_POINT('Ctrl Pts',(-26.3157338396918,-89.3429097126816,
5.57115462211654));
#21119=CARTESIAN_POINT('Ctrl Pts',(-23.2111784520928,-88.4600278964635,
5.42352862696177));
#21120=CARTESIAN_POINT('Ctrl Pts',(-20.6043011989706,-90.7260802299217,
5.26554546171313));
#21121=CARTESIAN_POINT('Ctrl Pts',(-21.0774386607742,-94.1476212763577,
5.1075622964645));
#21122=CARTESIAN_POINT('Ctrl Pts',(-24.2014390107181,-95.6211965224102,
4.94957913121586));
#21123=CARTESIAN_POINT('Ctrl Pts',(-26.6784591036876,-94.0960763882476,
4.81653284812018));
#21124=CARTESIAN_POINT('Ctrl Pts',(-27.068037426895,-92.536970787307,4.73614762010738));
#21125=CARTESIAN_POINT('Ctrl Pts',(-27.0687191146691,-91.9995675532748,
4.70842344717746));
#21126=CARTESIAN_POINT('Ctrl Pts',(-27.0701625816395,-91.9979746548734,
5.79157655282255));
#21127=CARTESIAN_POINT('Ctrl Pts',(-27.0724187402063,-91.629326646717,5.77253588131066));
#21128=CARTESIAN_POINT('Ctrl Pts',(-26.8409295378372,-90.2438417959684,
5.70083415471588));
#21129=CARTESIAN_POINT('Ctrl Pts',(-24.7888215637087,-88.4600278255509,
5.57647137303823));
#21130=CARTESIAN_POINT('Ctrl Pts',(-21.4664561758692,-89.404851035816,5.41848820778961));
#21131=CARTESIAN_POINT('Ctrl Pts',(-20.4421015118168,-92.7035629345559,
5.26050504254096));
#21132=CARTESIAN_POINT('Ctrl Pts',(-22.6448822152433,-95.3641192375839,
5.10252187729233));
#21133=CARTESIAN_POINT('Ctrl Pts',(-26.040443362995,-94.9774448457586,4.94621238071952));
#21134=CARTESIAN_POINT('Ctrl Pts',(-27.0758072022183,-92.9798036840462,
4.8425639392296));
#21135=CARTESIAN_POINT('Ctrl Pts',(-27.0783838750167,-91.9994167251476,
4.79157655282255));
#21136=CARTESIAN_POINT('Origin',(-24.,-92.,12.2084234471775));
#21137=CARTESIAN_POINT('',(-27.0714155398157,-92.0025047924058,6.79157655282255));
#21138=CARTESIAN_POINT('',(-27.0765041175219,-91.9978813009372,6.70842344717745));
#21139=CARTESIAN_POINT('',(-27.0735,-91.9999999999999,12.2084234471775));
#21140=CARTESIAN_POINT('Ctrl Pts',(-27.0765041175218,-91.9978813009372,
6.70842344717745));
#21141=CARTESIAN_POINT('Ctrl Pts',(-27.077570052034,-91.8628782914749,6.70141361443525));
#21142=CARTESIAN_POINT('Ctrl Pts',(-27.0084024469269,-90.7147701434973,
6.64174272661016));
#21143=CARTESIAN_POINT('Ctrl Pts',(-25.5645422900302,-88.7280205763547,
6.52941078370221));
#21144=CARTESIAN_POINT('Ctrl Pts',(-22.114810267437,-88.9016614773084,6.37142761845357));
#21145=CARTESIAN_POINT('Ctrl Pts',(-20.3750096777634,-91.8856011718064,
6.21344445320494));
#21146=CARTESIAN_POINT('Ctrl Pts',(-21.923199039088,-94.9733045078939,6.0554612879563));
#21147=CARTESIAN_POINT('Ctrl Pts',(-25.3551177576112,-95.3641191701941,
5.89747812270767));
#21148=CARTESIAN_POINT('Ctrl Pts',(-26.9680496218174,-93.4159924088721,
5.78179884244805));
#21149=CARTESIAN_POINT('Ctrl Pts',(-27.0764935417666,-92.2024076860066,
5.71878061727132));
#21150=CARTESIAN_POINT('Ctrl Pts',(-27.0746895390839,-92.0026322734109,
5.70842344717746));
#21151=CARTESIAN_POINT('Ctrl Pts',(-27.0714155398157,-92.0025047924058,
6.79157655282255));
#21152=CARTESIAN_POINT('Ctrl Pts',(-27.0659293112961,-91.2983381285157,
6.75516887847459));
#21153=CARTESIAN_POINT('Ctrl Pts',(-26.4768297637755,-89.5673490693385,
6.66610014904375));
#21154=CARTESIAN_POINT('Ctrl Pts',(-23.6086717136575,-88.3943787451648,
6.52437036453005));
#21155=CARTESIAN_POINT('Ctrl Pts',(-20.7665452720997,-90.3573153135784,
6.36638719928141));
#21156=CARTESIAN_POINT('Ctrl Pts',(-20.8572726350159,-93.8102229593112,
6.20840403403277));
#21157=CARTESIAN_POINT('Ctrl Pts',(-23.7985609852469,-95.6211965949497,
6.05042086878414));
#21158=CARTESIAN_POINT('Ctrl Pts',(-26.5460461813277,-94.3252216524648,
5.9114783750474));
#21159=CARTESIAN_POINT('Ctrl Pts',(-27.0661788504793,-92.6489016680912,
5.82519693639353));
#21160=CARTESIAN_POINT('Ctrl Pts',(-27.0701625816395,-91.9979746548734,
5.79157655282255));
#21161=CARTESIAN_POINT('Origin',(-24.,-92.,12.2084234471775));
#21162=CARTESIAN_POINT('',(-27.0784607967681,-91.9996098257547,7.79157655282255));
#21163=CARTESIAN_POINT('',(-27.0687741242031,-91.9993961639582,7.70842344717745));
#21164=CARTESIAN_POINT('',(-27.0735,-91.9999999999999,12.2084234471775));
#21165=CARTESIAN_POINT('Ctrl Pts',(-27.0687741242031,-91.9993961639582,
7.70842344717745));
#21166=CARTESIAN_POINT('Ctrl Pts',(-27.0696119417858,-91.5268986218895,
7.68404661159918));
#21167=CARTESIAN_POINT('Ctrl Pts',(-26.7455188317855,-90.0347580376889,
7.60700872093803));
#21168=CARTESIAN_POINT('Ctrl Pts',(-24.4293689698895,-88.3987107783728,
7.47730977519402));
#21169=CARTESIAN_POINT('Ctrl Pts',(-21.2186702510283,-89.672373140829,7.31932660994537));
#21170=CARTESIAN_POINT('Ctrl Pts',(-20.5307325412461,-93.057272549676,7.16134344469675));
#21171=CARTESIAN_POINT('Ctrl Pts',(-22.9895388330194,-95.4831896502703,
7.0033602794481));
#21172=CARTESIAN_POINT('Ctrl Pts',(-26.2151019833044,-94.7822788033369,
6.85238694694168));
#21173=CARTESIAN_POINT('Ctrl Pts',(-27.0695622666666,-92.8770823643973,
6.75407466951813));
#21174=CARTESIAN_POINT('Ctrl Pts',(-27.0765041175218,-91.9978813009372,
6.70842344717745));
#21175=CARTESIAN_POINT('Ctrl Pts',(-27.0784607967681,-91.9996098257547,
7.79157655282255));
#21176=CARTESIAN_POINT('Ctrl Pts',(-27.0784994051683,-91.9781985026171,
7.7904629307214));
#21177=CARTESIAN_POINT('Ctrl Pts',(-27.0686359944836,-90.944323237583,7.73668825353738));
#21178=CARTESIAN_POINT('Ctrl Pts',(-25.9177920028682,-88.9217350716083,
7.63025252127049));
#21179=CARTESIAN_POINT('Ctrl Pts',(-22.4700853511787,-88.7116867750179,
7.47226935602185));
#21180=CARTESIAN_POINT('Ctrl Pts',(-20.4100632788413,-91.4842510500175,
7.31428619077321));
#21181=CARTESIAN_POINT('Ctrl Pts',(-21.6062364556795,-94.7246171090759,
7.15630302552459));
#21182=CARTESIAN_POINT('Ctrl Pts',(-24.9736348172233,-95.4936625105602,
6.99831986027594));
#21183=CARTESIAN_POINT('Ctrl Pts',(-26.8854041041607,-93.6468834845165,
6.87674436937527));
#21184=CARTESIAN_POINT('Ctrl Pts',(-27.073864742148,-92.3168640338026,6.80782993355747));
#21185=CARTESIAN_POINT('Ctrl Pts',(-27.0714155398157,-92.0025047924058,
6.79157655282255));
#21186=CARTESIAN_POINT('Origin',(-24.,-92.,12.2084234471775));
#21187=CARTESIAN_POINT('',(-27.0703859251749,-91.9978642356407,8.79157655282255));
#21188=CARTESIAN_POINT('',(-27.0743676381347,-92.0026790873961,8.70842344717746));
#21189=CARTESIAN_POINT('',(-27.0735,-91.9999999999999,12.2084234471775));
#21190=CARTESIAN_POINT('Ctrl Pts',(-27.0743676381347,-92.0026790873961,
8.70842344717746));
#21191=CARTESIAN_POINT('Ctrl Pts',(-27.0670573859793,-91.1972814683818,
8.66667960876313));
#21192=CARTESIAN_POINT('Ctrl Pts',(-26.3319129571347,-89.3640272738251,
8.57227471526591));
#21193=CARTESIAN_POINT('Ctrl Pts',(-23.2485916399684,-88.4518995672047,
8.42520876668582));
#21194=CARTESIAN_POINT('Ctrl Pts',(-20.6179385783441,-90.6903039808948,
8.26722560143718));
#21195=CARTESIAN_POINT('Ctrl Pts',(-21.0549302288588,-94.116650160768,8.10924243618856));
#21196=CARTESIAN_POINT('Ctrl Pts',(-24.1632008959979,-95.6231210406981,
7.95125927093991));
#21197=CARTESIAN_POINT('Ctrl Pts',(-26.6666767475757,-94.1179251847747,
7.81765294126956));
#21198=CARTESIAN_POINT('Ctrl Pts',(-27.0678020121201,-92.5476307431492,
7.73670766668206));
#21199=CARTESIAN_POINT('Ctrl Pts',(-27.0687741242031,-91.9993961639582,
7.70842344717745));
#21200=CARTESIAN_POINT('Ctrl Pts',(-27.0703859251749,-91.9978642356407,
8.79157655282255));
#21201=CARTESIAN_POINT('Ctrl Pts',(-27.0727141338614,-91.6401224413272,
8.77309592788534));
#21202=CARTESIAN_POINT('Ctrl Pts',(-26.8501668180301,-90.265785975548,8.70195424786525));
#21203=CARTESIAN_POINT('Ctrl Pts',(-24.8261378316183,-88.4685620052275,
8.57815151276229));
#21204=CARTESIAN_POINT('Ctrl Pts',(-21.493997396212,-89.3782456609066,8.42016834751366));
#21205=CARTESIAN_POINT('Ctrl Pts',(-20.4348704258473,-92.6659673604641,
8.26218518226503));
#21206=CARTESIAN_POINT('Ctrl Pts',(-22.6094457101907,-95.3496254273119,
8.10420201701638));
#21207=CARTESIAN_POINT('Ctrl Pts',(-26.0210779679428,-94.9975623737004,
7.94733247386889));
#21208=CARTESIAN_POINT('Ctrl Pts',(-27.0766736879126,-92.9906989423899,
7.84312398580428));
#21209=CARTESIAN_POINT('Ctrl Pts',(-27.0784607967681,-91.9996098257547,
7.79157655282255));
#21210=CARTESIAN_POINT('Origin',(-24.,-92.,12.2084234471775));
#21211=CARTESIAN_POINT('',(-27.0702887490762,-92.0031018432153,9.79157655282255));
#21212=CARTESIAN_POINT('',(-27.0767669904684,-91.998062685181,9.70842344717746));
#21213=CARTESIAN_POINT('',(-27.0735,-91.9999999999999,12.2084234471775));
#21214=CARTESIAN_POINT('',(-24.7937992825329,-94.9692229537457,10.));
#21215=CARTESIAN_POINT('Ctrl Pts',(-24.7937992825329,-94.9692229537457,
10.));
#21216=CARTESIAN_POINT('Ctrl Pts',(-25.7762533017603,-94.7065713079336,
9.94733894491712));
#21217=CARTESIAN_POINT('Ctrl Pts',(-26.875910333047,-93.6687793941585,9.87786446252463));
#21218=CARTESIAN_POINT('Ctrl Pts',(-27.0726354893275,-92.3283627763233,
9.80838998013215));
#21219=CARTESIAN_POINT('Ctrl Pts',(-27.0702887490762,-92.0031018432153,
9.79157655282255));
#21220=CARTESIAN_POINT('',(-23.2043026670138,-94.9743009685655,10.));
#21221=CARTESIAN_POINT('Origin',(-24.,-92.,10.));
#21222=CARTESIAN_POINT('Ctrl Pts',(-23.2042982523172,-94.9743127795766,
10.));
#21223=CARTESIAN_POINT('Ctrl Pts',(-24.1519054403103,-95.2254055803294,
9.94901908464118));
#21224=CARTESIAN_POINT('Ctrl Pts',(-26.2125562800898,-94.7696542914347,
9.851826900367));
#21225=CARTESIAN_POINT('Ctrl Pts',(-27.0700738217707,-92.8876739876312,
9.75463471609282));
#21226=CARTESIAN_POINT('Ctrl Pts',(-27.0767669904684,-91.998062685181,9.70842344717746));
#21227=CARTESIAN_POINT('Origin',(92.,-24.,5.));
#21228=CARTESIAN_POINT('',(89.486504426694,-23.9997257424662,1.38741669750802));
#21229=CARTESIAN_POINT('',(89.4843725317804,-24.0035302714347,1.11258330249198));
#21230=CARTESIAN_POINT('',(89.4825,-24.,5.));
#21231=CARTESIAN_POINT('',(90.086534003335,-22.364012796625,0.999999999999999));
#21232=CARTESIAN_POINT('Ctrl Pts',(89.4843725317804,-24.0035302714347,1.11258330249198));
#21233=CARTESIAN_POINT('Ctrl Pts',(89.4895356694446,-23.4109125587034,1.07505553499465));
#21234=CARTESIAN_POINT('Ctrl Pts',(89.7007781719159,-22.8151964396956,1.03752776749733));
#21235=CARTESIAN_POINT('Ctrl Pts',(90.0865340033349,-22.364012796625,0.999999999999998));
#21236=CARTESIAN_POINT('',(89.4825,-24.,1.));
#21237=CARTESIAN_POINT('Origin',(92.,-24.,1.));
#21238=CARTESIAN_POINT('',(89.4825,-24.,0.));
#21239=CARTESIAN_POINT('',(89.4825,-24.,5.));
#21240=CARTESIAN_POINT('Origin',(92.,-24.,0.));
#21241=CARTESIAN_POINT('',(93.9171033775211,-22.3614656597818,0.999999999999999));
#21242=CARTESIAN_POINT('Origin',(92.,-24.,1.));
#21243=CARTESIAN_POINT('Ctrl Pts',(93.9171118396844,-22.3614597340103,0.999999999999999));
#21244=CARTESIAN_POINT('Ctrl Pts',(93.39395715018,-21.7523042564146,1.05098091535882));
#21245=CARTESIAN_POINT('Ctrl Pts',(92.5534187715749,-21.4121721444715,1.10196183071765));
#21246=CARTESIAN_POINT('Ctrl Pts',(91.7542642221519,-21.4905144511518,1.15294274607647));
#21247=CARTESIAN_POINT('Ctrl Pts',(90.9287725366714,-21.5714386263726,1.20560380115935));
#21248=CARTESIAN_POINT('Ctrl Pts',(90.147437339474,-22.0988744252836,1.25826485624223));
#21249=CARTESIAN_POINT('Ctrl Pts',(89.7641118492187,-22.8341462554664,1.31092591132511));
#21250=CARTESIAN_POINT('Ctrl Pts',(89.578516959615,-23.190143176153,1.33642284005274));
#21251=CARTESIAN_POINT('Ctrl Pts',(89.4862239279038,-23.5948612398581,1.36191976878038));
#21252=CARTESIAN_POINT('Ctrl Pts',(89.486504426694,-23.9997257424662,1.38741669750802));
#21253=CARTESIAN_POINT('Origin',(92.,-24.,5.));
#21254=CARTESIAN_POINT('',(89.4812642899865,-24.0021096151709,2.38741669750802));
#21255=CARTESIAN_POINT('',(89.478587803344,-23.999354427872,2.11258330249198));
#21256=CARTESIAN_POINT('',(89.4825,-24.,5.));
#21257=CARTESIAN_POINT('Ctrl Pts',(89.478587803344,-23.999354427872,2.11258330249198));
#21258=CARTESIAN_POINT('Ctrl Pts',(89.478468138627,-23.9641713652006,2.11034958724147));
#21259=CARTESIAN_POINT('Ctrl Pts',(89.4791414214072,-23.928993039682,2.10811587199095));
#21260=CARTESIAN_POINT('Ctrl Pts',(89.4806219723461,-23.8938487862731,2.10588215674044));
#21261=CARTESIAN_POINT('Ctrl Pts',(89.5155267680806,-23.0653038478858,2.05322110165756));
#21262=CARTESIAN_POINT('Ctrl Pts',(89.9991163215577,-22.2556964040098,2.00056004657469));
#21263=CARTESIAN_POINT('Ctrl Pts',(90.7120875494009,-21.8321134766477,1.94789899149181));
#21264=CARTESIAN_POINT('Ctrl Pts',(91.4250587772441,-21.4085305492857,1.89523793640893));
#21265=CARTESIAN_POINT('Ctrl Pts',(92.3674116794532,-21.3709721384377,1.84257688132605));
#21266=CARTESIAN_POINT('Ctrl Pts',(93.1117465266451,-21.7366426720986,1.78991582624317));
#21267=CARTESIAN_POINT('Ctrl Pts',(93.8560813738369,-22.1023132057595,1.7372547711603));
#21268=CARTESIAN_POINT('Ctrl Pts',(94.4023981660114,-22.8712126839293,1.68459371607742));
#21269=CARTESIAN_POINT('Ctrl Pts',(94.502987230808,-23.6942827713943,1.63193266099454));
#21270=CARTESIAN_POINT('Ctrl Pts',(94.6035762956047,-24.5173528588592,1.57927160591166));
#21271=CARTESIAN_POINT('Ctrl Pts',(94.2584376330234,-25.3945935556193,1.52661055082878));
#21272=CARTESIAN_POINT('Ctrl Pts',(93.6239875152206,-25.9288761516102,1.4739494957459));
#21273=CARTESIAN_POINT('Ctrl Pts',(92.9895373974178,-26.4631587476011,1.42128844066303));
#21274=CARTESIAN_POINT('Ctrl Pts',(92.0657758243935,-26.6544832428228,1.36862738558015));
#21275=CARTESIAN_POINT('Ctrl Pts',(91.2718709044644,-26.4146102691233,1.31596633049727));
#21276=CARTESIAN_POINT('Ctrl Pts',(90.4779659845352,-26.1747372954238,1.26330527541439));
#21277=CARTESIAN_POINT('Ctrl Pts',(89.8139177177011,-25.503666852803,1.21064422033151));
#21278=CARTESIAN_POINT('Ctrl Pts',(89.5807312014043,-24.7092672371348,1.15798316524864));
#21279=CARTESIAN_POINT('Ctrl Pts',(89.5137200371456,-24.480979409957,1.14284987766308));
#21280=CARTESIAN_POINT('Ctrl Pts',(89.4822904668902,-24.2425067646591,1.12771659007753));
#21281=CARTESIAN_POINT('Ctrl Pts',(89.4843725317804,-24.0035302714347,1.11258330249198));
#21282=CARTESIAN_POINT('Ctrl Pts',(89.486504426694,-23.9997257424662,1.38741669750802));
#21283=CARTESIAN_POINT('Ctrl Pts',(89.4868032667881,-24.4310635958632,1.41458082386326));
#21284=CARTESIAN_POINT('Ctrl Pts',(89.5921778743622,-24.8625676650245,1.4417449502185));
#21285=CARTESIAN_POINT('Ctrl Pts',(89.8017475042685,-25.2354979719165,1.46890907657374));
#21286=CARTESIAN_POINT('Ctrl Pts',(90.2080244328865,-25.958469996729,1.52157013165662));
#21287=CARTESIAN_POINT('Ctrl Pts',(91.0058940734353,-26.4613061848995,1.57423118673949));
#21288=CARTESIAN_POINT('Ctrl Pts',(91.8333901892196,-26.5160872321709,1.62689224182237));
#21289=CARTESIAN_POINT('Ctrl Pts',(92.6608863050038,-26.5708682794422,1.67955329690525));
#21290=CARTESIAN_POINT('Ctrl Pts',(93.5180088960235,-26.1775941858145,1.73221435198813));
#21291=CARTESIAN_POINT('Ctrl Pts',(94.0160963730402,-25.5145600286215,1.78487540707101));
#21292=CARTESIAN_POINT('Ctrl Pts',(94.5141838500569,-24.8515258714286,1.83753646215389));
#21293=CARTESIAN_POINT('Ctrl Pts',(94.6532362130706,-23.9187316506705,1.89019751723677));
#21294=CARTESIAN_POINT('Ctrl Pts',(94.3701623803631,-23.1392455433219,1.94285857231964));
#21295=CARTESIAN_POINT('Ctrl Pts',(94.0870885476557,-22.3597594359734,1.99551962740252));
#21296=CARTESIAN_POINT('Ctrl Pts',(93.3818885192271,-21.7335814420345,2.0481806824854));
#21297=CARTESIAN_POINT('Ctrl Pts',(92.5743964779127,-21.5446792416752,2.10084173756828));
#21298=CARTESIAN_POINT('Ctrl Pts',(91.7669044365982,-21.3557770413159,2.15350279265115));
#21299=CARTESIAN_POINT('Ctrl Pts',(90.8571203823979,-21.6041506345363,2.20616384773403));
#21300=CARTESIAN_POINT('Ctrl Pts',(90.2576400878061,-22.1771655681069,2.25882490281691));
#21301=CARTESIAN_POINT('Ctrl Pts',(89.7696877997114,-22.6435761415163,2.30168883438061));
#21302=CARTESIAN_POINT('Ctrl Pts',(89.4873207515092,-23.3250710178654,2.34455276594432));
#21303=CARTESIAN_POINT('Ctrl Pts',(89.4812642899865,-24.0021096151709,2.38741669750802));
#21304=CARTESIAN_POINT('Origin',(92.,-24.,5.));
#21305=CARTESIAN_POINT('',(89.4802713394158,-23.9981710493934,3.38741669750802));
#21306=CARTESIAN_POINT('',(89.4854090148867,-23.9984414282173,3.11258330249198));
#21307=CARTESIAN_POINT('',(89.4825,-24.,5.));
#21308=CARTESIAN_POINT('Ctrl Pts',(89.4854090148867,-23.9984414282173,3.11258330249198));
#21309=CARTESIAN_POINT('Ctrl Pts',(89.4836298808409,-23.6875464209234,3.0929825844054));
#21310=CARTESIAN_POINT('Ctrl Pts',(89.5370775357559,-23.3772414115068,3.07338186631883));
#21311=CARTESIAN_POINT('Ctrl Pts',(89.6485421342809,-23.0894033947305,3.05378114823225));
#21312=CARTESIAN_POINT('Ctrl Pts',(89.9480129667671,-22.3160718469038,3.00112009314937));
#21313=CARTESIAN_POINT('Ctrl Pts',(90.6662677151581,-21.704913874088,2.94845903806649));
#21314=CARTESIAN_POINT('Ctrl Pts',(91.4775657731397,-21.5330988908351,2.89579798298361));
#21315=CARTESIAN_POINT('Ctrl Pts',(92.2888638311213,-21.3612839075822,2.84313692790074));
#21316=CARTESIAN_POINT('Ctrl Pts',(93.1932051986935,-21.628811913892,2.79047587281786));
#21317=CARTESIAN_POINT('Ctrl Pts',(93.7804552648549,-22.2143567539363,2.73781481773498));
#21318=CARTESIAN_POINT('Ctrl Pts',(94.3677053310163,-22.7999015939806,2.6851537626521));
#21319=CARTESIAN_POINT('Ctrl Pts',(94.6378640957668,-23.7034632677594,2.63249270756922));
#21320=CARTESIAN_POINT('Ctrl Pts',(94.4684106985952,-24.5152563159491,2.57983165248635));
#21321=CARTESIAN_POINT('Ctrl Pts',(94.2989573014235,-25.3270493641389,2.52717059740347));
#21322=CARTESIAN_POINT('Ctrl Pts',(93.6898917423296,-26.0470737867397,2.47450954232059));
#21323=CARTESIAN_POINT('Ctrl Pts',(92.9174341156813,-26.3487960615596,2.42184848723771));
#21324=CARTESIAN_POINT('Ctrl Pts',(92.1449764890331,-26.6505183363795,2.36918743215483));
#21325=CARTESIAN_POINT('Ctrl Pts',(91.2091267948306,-26.5339384634185,2.31652637707196));
#21326=CARTESIAN_POINT('Ctrl Pts',(90.5343119667252,-26.0519073104888,2.26386532198908));
#21327=CARTESIAN_POINT('Ctrl Pts',(89.8881206474051,-25.5903223931277,2.21343798215671));
#21328=CARTESIAN_POINT('Ctrl Pts',(89.4812892995851,-24.7936312531159,2.16301064232435));
#21329=CARTESIAN_POINT('Ctrl Pts',(89.478587803344,-23.999354427872,2.11258330249198));
#21330=CARTESIAN_POINT('Ctrl Pts',(89.4812642899865,-24.0021096151709,2.38741669750802));
#21331=CARTESIAN_POINT('Ctrl Pts',(89.4798800048903,-24.1568558207352,2.3972138210272));
#21332=CARTESIAN_POINT('Ctrl Pts',(89.4929305169813,-24.3113692249256,2.40701094454637));
#21333=CARTESIAN_POINT('Ctrl Pts',(89.5212603168746,-24.4630284201485,2.41680806806555));
#21334=CARTESIAN_POINT('Ctrl Pts',(89.6735373755183,-25.2782200646988,2.46946912314842));
#21335=CARTESIAN_POINT('Ctrl Pts',(90.2672680277891,-26.0109470798785,2.5221301782313));
#21336=CARTESIAN_POINT('Ctrl Pts',(91.0331836548293,-26.3289069878288,2.57479123331418));
#21337=CARTESIAN_POINT('Ctrl Pts',(91.7990992818695,-26.6468668957791,2.62745228839706));
#21338=CARTESIAN_POINT('Ctrl Pts',(92.7371998836791,-26.5500596964999,2.68011334347994));
#21339=CARTESIAN_POINT('Ctrl Pts',(93.4220416283355,-26.0823882608119,2.73277439856281));
#21340=CARTESIAN_POINT('Ctrl Pts',(94.1068833729918,-25.6147168251239,2.78543545364569));
#21341=CARTESIAN_POINT('Ctrl Pts',(94.538466260495,-24.7761811530271,2.83809650872857));
#21342=CARTESIAN_POINT('Ctrl Pts',(94.5210596939212,-23.9470718966112,2.89075756381145));
#21343=CARTESIAN_POINT('Ctrl Pts',(94.5036531273474,-23.1179626401953,2.94341861889433));
#21344=CARTESIAN_POINT('Ctrl Pts',(94.0372571066967,-22.2982797994604,2.9960796739772));
#21345=CARTESIAN_POINT('Ctrl Pts',(93.3333903788127,-21.8597633286133,3.04874072906008));
#21346=CARTESIAN_POINT('Ctrl Pts',(92.6295236509286,-21.4212468577662,3.10140178414296));
#21347=CARTESIAN_POINT('Ctrl Pts',(91.6881862158112,-21.3638967568069,3.15406283922584));
#21348=CARTESIAN_POINT('Ctrl Pts',(90.9362905712497,-21.713722374568,3.20672389430872));
#21349=CARTESIAN_POINT('Ctrl Pts',(90.1843949266882,-22.063547992329,3.2593849493916));
#21350=CARTESIAN_POINT('Ctrl Pts',(89.6219410726826,-22.8205493288104,3.31204600447448));
#21351=CARTESIAN_POINT('Ctrl Pts',(89.5040114769093,-23.6414133102582,3.36470705955735));
#21352=CARTESIAN_POINT('Ctrl Pts',(89.4870594274965,-23.759410210726,3.37227693887424));
#21353=CARTESIAN_POINT('Ctrl Pts',(89.4792926975419,-23.8787267215066,3.37984681819113));
#21354=CARTESIAN_POINT('Ctrl Pts',(89.4802713394158,-23.9981710493934,3.38741669750802));
#21355=CARTESIAN_POINT('Origin',(92.,-24.,5.));
#21356=CARTESIAN_POINT('',(89.4864158728457,-23.9996457834086,4.38741669750802));
#21357=CARTESIAN_POINT('',(89.4839749917547,-24.0021063689016,4.11258330249198));
#21358=CARTESIAN_POINT('',(89.4825,-24.,5.));
#21359=CARTESIAN_POINT('Ctrl Pts',(89.4839749917547,-24.0021063689016,4.11258330249198));
#21360=CARTESIAN_POINT('Ctrl Pts',(89.4886916234371,-23.4165893004159,4.07561558156934));
#21361=CARTESIAN_POINT('Ctrl Pts',(89.6925944465198,-22.8281096510768,4.0386478606467));
#21362=CARTESIAN_POINT('Ctrl Pts',(90.066215027555,-22.381662646436,4.00168013972406));
#21363=CARTESIAN_POINT('Ctrl Pts',(90.598442968768,-21.7456924076384,3.94901908464118));
#21364=CARTESIAN_POINT('Ctrl Pts',(91.4750692458126,-21.3979407209711,3.8963580295583));
#21365=CARTESIAN_POINT('Ctrl Pts',(92.2985288839647,-21.4961188951354,3.84369697447542));
#21366=CARTESIAN_POINT('Ctrl Pts',(93.1219885221168,-21.5942970692997,3.79103591939254));
#21367=CARTESIAN_POINT('Ctrl Pts',(93.8922815213763,-22.1384051042956,3.73837486430966));
#21368=CARTESIAN_POINT('Ctrl Pts',(94.2600668556347,-22.8816807530475,3.68571380922679));
#21369=CARTESIAN_POINT('Ctrl Pts',(94.627852189893,-23.6249564017993,3.63305275414391));
#21370=CARTESIAN_POINT('Ctrl Pts',(94.5931298591502,-24.5673996643072,3.58039169906103));
#21371=CARTESIAN_POINT('Ctrl Pts',(94.1716470433212,-25.2815963706942,3.52773064397815));
#21372=CARTESIAN_POINT('Ctrl Pts',(93.7501642274922,-25.9957930770812,3.47506958889527));
#21373=CARTESIAN_POINT('Ctrl Pts',(92.941920926577,-26.4817432273472,3.4224085338124));
#21374=CARTESIAN_POINT('Ctrl Pts',(92.1134692499477,-26.5190602709168,3.36974747872952));
#21375=CARTESIAN_POINT('Ctrl Pts',(91.2850175733184,-26.5563773144864,3.31708642364664));
#21376=CARTESIAN_POINT('Ctrl Pts',(90.4363575209752,-26.1450612513594,3.26442536856376));
#21377=CARTESIAN_POINT('Ctrl Pts',(89.9523709530942,-25.4716506583771,3.21176431348088));
#21378=CARTESIAN_POINT('Ctrl Pts',(89.6485266983476,-25.0488869840482,3.17870397648458));
#21379=CARTESIAN_POINT('Ctrl Pts',(89.4884098626544,-24.5228249567292,3.14564363948828));
#21380=CARTESIAN_POINT('Ctrl Pts',(89.4854090148867,-23.9984414282173,3.11258330249198));
#21381=CARTESIAN_POINT('Ctrl Pts',(89.4802713394158,-23.9981710493934,3.38741669750802));
#21382=CARTESIAN_POINT('Ctrl Pts',(89.4861007735321,-24.7096599592594,3.43250787327401));
#21383=CARTESIAN_POINT('Ctrl Pts',(89.8022314305929,-25.4256840455739,3.47759904904));
#21384=CARTESIAN_POINT('Ctrl Pts',(90.3356791886478,-25.8943545894189,3.52269022480599));
#21385=CARTESIAN_POINT('Ctrl Pts',(90.958681833701,-26.4417052607172,3.57535127988886));
#21386=CARTESIAN_POINT('Ctrl Pts',(91.8780924613484,-26.6516799768993,3.62801233497174));
#21387=CARTESIAN_POINT('Ctrl Pts',(92.6769426722523,-26.4290516090785,3.68067339005462));
#21388=CARTESIAN_POINT('Ctrl Pts',(93.4757928831562,-26.2064232412577,3.7333344451375));
#21389=CARTESIAN_POINT('Ctrl Pts',(94.1540826773166,-25.551191789434,3.78599550022038));
#21390=CARTESIAN_POINT('Ctrl Pts',(94.4041960519401,-24.7605159049425,3.83865655530326));
#21391=CARTESIAN_POINT('Ctrl Pts',(94.6543094265635,-23.969840020451,3.89131761038614));
#21392=CARTESIAN_POINT('Ctrl Pts',(94.4762463816501,-23.0437197032917,3.94397866546901));
#21393=CARTESIAN_POINT('Ctrl Pts',(93.9507615495482,-22.4021663197385,3.99663972055189));
#21394=CARTESIAN_POINT('Ctrl Pts',(93.4252767174463,-21.7606129361853,4.04930077563477));
#21395=CARTESIAN_POINT('Ctrl Pts',(92.5523700981559,-21.4036264862383,4.10196183071765));
#21396=CARTESIAN_POINT('Ctrl Pts',(91.727919739318,-21.4931064186725,4.15462288580053));
#21397=CARTESIAN_POINT('Ctrl Pts',(90.9034693804802,-21.5825863511068,4.2072839408834));
#21398=CARTESIAN_POINT('Ctrl Pts',(90.1274752820949,-22.1185326659223,4.25994499596628));
#21399=CARTESIAN_POINT('Ctrl Pts',(89.7518640115846,-22.8578845621823,4.31260605104916));
#21400=CARTESIAN_POINT('Ctrl Pts',(89.5739987186599,-23.20799397563,4.33754293320212));
#21401=CARTESIAN_POINT('Ctrl Pts',(89.4859136397297,-23.6037142279007,4.36247981535507));
#21402=CARTESIAN_POINT('Ctrl Pts',(89.4864158728457,-23.9996457834086,4.38741669750802));
#21403=CARTESIAN_POINT('Origin',(92.,-24.,5.));
#21404=CARTESIAN_POINT('',(89.4815255054053,-24.0021560919774,5.38741669750802));
#21405=CARTESIAN_POINT('',(89.4785001229596,-23.9995222403937,5.11258330249198));
#21406=CARTESIAN_POINT('',(89.4825,-24.,5.));
#21407=CARTESIAN_POINT('Ctrl Pts',(89.4785001229596,-23.9995222403937,5.11258330249198));
#21408=CARTESIAN_POINT('Ctrl Pts',(89.4784308438678,-23.9731625418826,5.11090963381615));
#21409=CARTESIAN_POINT('Ctrl Pts',(89.4788088040536,-23.9468048777982,5.10923596514032));
#21410=CARTESIAN_POINT('Ctrl Pts',(89.4796401577289,-23.9204615220786,5.1075622964645));
#21411=CARTESIAN_POINT('Ctrl Pts',(89.5057982392643,-23.09158246934,5.05490124138162));
#21412=CARTESIAN_POINT('Ctrl Pts',(89.9808209826826,-22.2768688588901,5.00224018629874));
#21413=CARTESIAN_POINT('Ctrl Pts',(90.6892774670547,-21.8458072171371,4.94957913121586));
#21414=CARTESIAN_POINT('Ctrl Pts',(91.3977339514269,-21.4147455753842,4.89691807613299));
#21415=CARTESIAN_POINT('Ctrl Pts',(92.3396241767529,-21.3673359023281,4.84425702105011));
#21416=CARTESIAN_POINT('Ctrl Pts',(93.0877848515153,-21.7250792935763,4.79159596596723));
#21417=CARTESIAN_POINT('Ctrl Pts',(93.8359455262777,-22.0828226848245,4.73893491088435));
#21418=CARTESIAN_POINT('Ctrl Pts',(94.3903766504766,-22.8457191403771,4.68627385580147));
#21419=CARTESIAN_POINT('Ctrl Pts',(94.4996342472564,-23.667782098445,4.63361280071859));
#21420=CARTESIAN_POINT('Ctrl Pts',(94.6088918440362,-24.4898450565128,4.58095174563572));
#21421=CARTESIAN_POINT('Ctrl Pts',(94.272975913397,-25.371074517096,4.52829069055284));
#21422=CARTESIAN_POINT('Ctrl Pts',(93.6442300627918,-25.9118178797765,4.47562963546996));
#21423=CARTESIAN_POINT('Ctrl Pts',(93.0154842121866,-26.452561242457,4.42296858038708));
#21424=CARTESIAN_POINT('Ctrl Pts',(92.0939084416155,-26.6528185072348,4.3703075253042));
#21425=CARTESIAN_POINT('Ctrl Pts',(91.2974530904191,-26.4217695888032,4.31764647022132));
#21426=CARTESIAN_POINT('Ctrl Pts',(90.5009977392227,-26.1907206703715,4.26498541513845));
#21427=CARTESIAN_POINT('Ctrl Pts',(89.8296628074011,-25.5283655687303,4.21232436005557));
#21428=CARTESIAN_POINT('Ctrl Pts',(89.5879101441809,-24.7350936224458,4.15966330497269));
#21429=CARTESIAN_POINT('Ctrl Pts',(89.5158662908614,-24.4986934646177,4.14396997081245));
#21430=CARTESIAN_POINT('Ctrl Pts',(89.4819727131382,-24.2506668639209,4.12827663665222));
#21431=CARTESIAN_POINT('Ctrl Pts',(89.4839749917547,-24.0021063689016,4.11258330249198));
#21432=CARTESIAN_POINT('Ctrl Pts',(89.4864158728457,-23.9996457834086,4.38741669750802));
#21433=CARTESIAN_POINT('Ctrl Pts',(89.4869742424795,-24.439832124507,4.41514087043795));
#21434=CARTESIAN_POINT('Ctrl Pts',(89.5970301658382,-24.8802796450794,4.44286504336787));
#21435=CARTESIAN_POINT('Ctrl Pts',(89.8149443593501,-25.2586003903178,4.47058921629779));
#21436=CARTESIAN_POINT('Ctrl Pts',(90.2288644202614,-25.9772068444889,4.52325027138067));
#21437=CARTESIAN_POINT('Ctrl Pts',(91.0319329847194,-26.4716622751265,4.57591132646355));
#21438=CARTESIAN_POINT('Ctrl Pts',(91.8599447536684,-26.517722705864,4.62857238154643));
#21439=CARTESIAN_POINT('Ctrl Pts',(92.6879565226175,-26.5637831366015,4.68123343662931));
#21440=CARTESIAN_POINT('Ctrl Pts',(93.5409114960576,-26.1614485674388,4.73389449171218));
#21441=CARTESIAN_POINT('Ctrl Pts',(94.0319800368686,-25.4931845918408,4.78655554679506));
#21442=CARTESIAN_POINT('Ctrl Pts',(94.5230485776795,-24.8249206162428,4.83921660187794));
#21443=CARTESIAN_POINT('Ctrl Pts',(94.6522306858613,-23.8907272342096,4.89187765696082));
#21444=CARTESIAN_POINT('Ctrl Pts',(94.3609400707585,-23.1142770874653,4.9445387120437));
#21445=CARTESIAN_POINT('Ctrl Pts',(94.0696494556558,-22.337826940721,4.99719976712657));
#21446=CARTESIAN_POINT('Ctrl Pts',(93.3578861172687,-21.7191200292656,5.04986082220945));
#21447=CARTESIAN_POINT('Ctrl Pts',(92.5484468765423,-21.5387504963612,5.10252187729233));
#21448=CARTESIAN_POINT('Ctrl Pts',(91.739007635816,-21.3583809634567,5.15518293237521));
#21449=CARTESIAN_POINT('Ctrl Pts',(90.8318924927504,-21.6163488091031,5.20784398745809));
#21450=CARTESIAN_POINT('Ctrl Pts',(90.2384936456262,-22.1956612127896,5.26050504254097));
#21451=CARTESIAN_POINT('Ctrl Pts',(89.7618021600142,-22.6610367214972,5.30280892752999));
#21452=CARTESIAN_POINT('Ctrl Pts',(89.48756099645,-23.3337852933997,5.345112812519));
#21453=CARTESIAN_POINT('Ctrl Pts',(89.4815255054053,-24.0021560919774,5.38741669750802));
#21454=CARTESIAN_POINT('Origin',(92.,-24.,5.));
#21455=CARTESIAN_POINT('',(89.4800391863944,-23.9982645761521,6.38741669750803));
#21456=CARTESIAN_POINT('',(89.4852341727342,-23.9983410426721,6.11258330249198));
#21457=CARTESIAN_POINT('',(89.4825,-24.,5.));
#21458=CARTESIAN_POINT('Ctrl Pts',(89.4852341727342,-23.9983410426721,6.11258330249198));
#21459=CARTESIAN_POINT('Ctrl Pts',(89.483386156444,-23.6963819807171,6.09354263098009));
#21460=CARTESIAN_POINT('Ctrl Pts',(89.533738485222,-23.3950185131867,6.07450195946819));
#21461=CARTESIAN_POINT('Ctrl Pts',(89.6390604846241,-23.114277295821,6.0554612879563));
#21462=CARTESIAN_POINT('Ctrl Pts',(89.9303510312042,-22.3378273317272,6.00280023287342));
#21463=CARTESIAN_POINT('Ctrl Pts',(90.6421142021576,-21.719120565815,5.95013917779055));
#21464=CARTESIAN_POINT('Ctrl Pts',(91.4515532524732,-21.5387510753403,5.89747812270767));
#21465=CARTESIAN_POINT('Ctrl Pts',(92.2609923027888,-21.3583815848656,5.84481706762479));
#21466=CARTESIAN_POINT('Ctrl Pts',(93.1681072324665,-21.6163493698282,5.79215601254191));
#21467=CARTESIAN_POINT('Ctrl Pts',(93.7615059400007,-22.1956616372385,5.73949495745904));
#21468=CARTESIAN_POINT('Ctrl Pts',(94.354904647535,-22.7749739046489,5.68683390237616));
#21469=CARTESIAN_POINT('Ctrl Pts',(94.6345871329257,-23.675630654507,5.63417284729328));
#21470=CARTESIAN_POINT('Ctrl Pts',(94.4737126159701,-24.4891686800901,5.5815117922104));
#21471=CARTESIAN_POINT('Ctrl Pts',(94.3128380990145,-25.3027067056733,5.52885073712752));
#21472=CARTESIAN_POINT('Ctrl Pts',(93.7114065797127,-26.0291260069815,5.47618968204464));
#21473=CARTESIAN_POINT('Ctrl Pts',(92.9421775161413,-26.3389830337326,5.42352862696177));
#21474=CARTESIAN_POINT('Ctrl Pts',(92.17294845257,-26.6488400604838,5.37086757187889));
#21475=CARTESIAN_POINT('Ctrl Pts',(91.2359218447291,-26.5421348126778,5.31820651679601));
#21476=CARTESIAN_POINT('Ctrl Pts',(90.556055250635,-26.0672599412612,5.26554546171313));
#21477=CARTESIAN_POINT('Ctrl Pts',(89.8977961123825,-25.6074774981291,5.21455807530608));
#21478=CARTESIAN_POINT('Ctrl Pts',(89.4806106720036,-24.8025558114754,5.16357068889903));
#21479=CARTESIAN_POINT('Ctrl Pts',(89.4785001229596,-23.9995222403937,5.11258330249198));
#21480=CARTESIAN_POINT('Ctrl Pts',(89.4815255054053,-24.0021560919774,5.38741669750802));
#21481=CARTESIAN_POINT('Ctrl Pts',(89.4800478489828,-24.1657918915839,5.39777386760188));
#21482=CARTESIAN_POINT('Ctrl Pts',(89.494646624663,-24.3291652844524,5.40813103769574));
#21483=CARTESIAN_POINT('Ctrl Pts',(89.5262868021188,-24.4891687951612,5.4184882077896));
#21484=CARTESIAN_POINT('Ctrl Pts',(89.6871613569182,-25.3027070121193,5.47114926287248));
#21485=CARTESIAN_POINT('Ctrl Pts',(90.2885930176996,-26.0291264843089,5.52381031795536));
#21486=CARTESIAN_POINT('Ctrl Pts',(91.0578222622228,-26.3389835839502,5.57647137303824));
#21487=CARTESIAN_POINT('Ctrl Pts',(91.827051506746,-26.6488406835915,5.62913242812111));
#21488=CARTESIAN_POINT('Ctrl Pts',(92.764078335011,-26.5421354106845,5.68179348320399));
#21489=CARTESIAN_POINT('Ctrl Pts',(93.4439450890356,-26.0672604275592,5.73445453828687));
#21490=CARTESIAN_POINT('Ctrl Pts',(94.1238118430601,-25.5923854444339,5.78711559336975));
#21491=CARTESIAN_POINT('Ctrl Pts',(94.5465185228442,-24.7493407510902,5.83977664845263));
#21492=CARTESIAN_POINT('Ctrl Pts',(94.5203604351554,-23.920461503368,5.89243770353551));
#21493=CARTESIAN_POINT('Ctrl Pts',(94.4942023474666,-23.0915822556457,5.94509875861838));
#21494=CARTESIAN_POINT('Ctrl Pts',(94.019179492305,-22.2768684535448,5.99775981370126));
#21495=CARTESIAN_POINT('Ctrl Pts',(93.310722841277,-21.8458067103895,6.05042086878414));
#21496=CARTESIAN_POINT('Ctrl Pts',(92.602266190249,-21.4147449672342,6.10308192386702));
#21497=CARTESIAN_POINT('Ctrl Pts',(91.6603757433546,-21.3673352830245,6.15574297894989));
#21498=CARTESIAN_POINT('Ctrl Pts',(90.9122148925964,-21.725078758428,6.20840403403277));
#21499=CARTESIAN_POINT('Ctrl Pts',(90.1640540418382,-22.0828222338316,6.26106508911565));
#21500=CARTESIAN_POINT('Ctrl Pts',(89.6096227872161,-22.8457188688485,6.31372614419853));
#21501=CARTESIAN_POINT('Ctrl Pts',(89.5003651647348,-23.6677820202958,6.36638719928141));
#21502=CARTESIAN_POINT('Ctrl Pts',(89.4858216342605,-23.7772087149586,6.37339703202361));
#21503=CARTESIAN_POINT('Ctrl Pts',(89.4791660807206,-23.8876837738622,6.38040686476582));
#21504=CARTESIAN_POINT('Ctrl Pts',(89.4800391863944,-23.9982645761521,6.38741669750803));
#21505=CARTESIAN_POINT('Origin',(92.,-24.,5.));
#21506=CARTESIAN_POINT('',(89.4863708146039,-23.9995053986078,7.38741669750802));
#21507=CARTESIAN_POINT('',(89.4842078764603,-24.0020516719095,7.11258330249199));
#21508=CARTESIAN_POINT('',(89.4825,-24.,5.));
#21509=CARTESIAN_POINT('Ctrl Pts',(89.4842078764603,-24.0020516719095,7.11258330249199));
#21510=CARTESIAN_POINT('Ctrl Pts',(89.4887016384805,-23.4252697537026,7.07617562814403));
#21511=CARTESIAN_POINT('Ctrl Pts',(89.6859405266727,-22.8457100529155,7.03976795379607));
#21512=CARTESIAN_POINT('Ctrl Pts',(90.0492389093472,-22.4021666956129,7.00336027944811));
#21513=CARTESIAN_POINT('Ctrl Pts',(90.5747236178373,-21.7606134629807,6.95069922436523));
#21514=CARTESIAN_POINT('Ctrl Pts',(91.4476300317824,-21.4036270970037,6.89803816928236));
#21515=CARTESIAN_POINT('Ctrl Pts',(92.2720801966773,-21.4931070083872,6.84537711419948));
#21516=CARTESIAN_POINT('Ctrl Pts',(93.096530361572,-21.5825869197707,6.7927160591166));
#21517=CARTESIAN_POINT('Ctrl Pts',(93.8725242774164,-22.1185331085148,6.74005500403372));
#21518=CARTESIAN_POINT('Ctrl Pts',(94.2481354595693,-22.8578848308521,6.68739394895084));
#21519=CARTESIAN_POINT('Ctrl Pts',(94.6237466417222,-23.5972365531893,6.63473289386796));
#21520=CARTESIAN_POINT('Ctrl Pts',(94.5989750901836,-24.5399938091198,6.58207183878509));
#21521=CARTESIAN_POINT('Ctrl Pts',(94.1850551266417,-25.2586000942469,6.52941078370221));
#21522=CARTESIAN_POINT('Ctrl Pts',(93.7711351630998,-25.977206379374,6.47674972861933));
#21523=CARTESIAN_POINT('Ctrl Pts',(92.9680667875545,-26.4716616936979,6.42408867353645));
#21524=CARTESIAN_POINT('Ctrl Pts',(92.1400552133854,-26.5177221136004,6.37142761845357));
#21525=CARTESIAN_POINT('Ctrl Pts',(91.3120436392162,-26.5637825335029,6.31876656337069));
#21526=CARTESIAN_POINT('Ctrl Pts',(90.4590888664232,-26.1614480589841,6.26610550828782));
#21527=CARTESIAN_POINT('Ctrl Pts',(89.9680204411301,-25.4931842405871,6.21344445320494));
#21528=CARTESIAN_POINT('Ctrl Pts',(89.6545077552948,-25.0665447464531,6.17982406963395));
#21529=CARTESIAN_POINT('Ctrl Pts',(89.4884972412917,-24.5315144383331,6.14620368606297));
#21530=CARTESIAN_POINT('Ctrl Pts',(89.4852341727342,-23.9983410426721,6.11258330249198));
#21531=CARTESIAN_POINT('Ctrl Pts',(89.4800391863944,-23.9982645761521,6.38741669750803));
#21532=CARTESIAN_POINT('Ctrl Pts',(89.4857252480609,-24.7184171072605,6.4330679198487));
#21533=CARTESIAN_POINT('Ctrl Pts',(89.8107173609326,-25.4430544346852,6.47871914218937));
#21534=CARTESIAN_POINT('Ctrl Pts',(90.3557695504229,-25.9118183295065,6.52437036453004));
#21535=CARTESIAN_POINT('Ctrl Pts',(90.9845155489329,-26.4525618193923,6.57703141961292));
#21536=CARTESIAN_POINT('Ctrl Pts',(91.9060915362935,-26.6528191312864,6.6296924746958));
#21537=CARTESIAN_POINT('Ctrl Pts',(92.7025470748465,-26.4217701584994,6.68235352977868));
#21538=CARTESIAN_POINT('Ctrl Pts',(93.4990026133995,-26.1907211857124,6.73501458486155));
#21539=CARTESIAN_POINT('Ctrl Pts',(94.170337703145,-25.5283659282443,6.78767563994443));
#21540=CARTESIAN_POINT('Ctrl Pts',(94.4120904232343,-24.7350937953597,6.84033669502731));
#21541=CARTESIAN_POINT('Ctrl Pts',(94.6538431433237,-23.941821662475,6.89299775011019));
#21542=CARTESIAN_POINT('Ctrl Pts',(94.4660134937569,-23.0176326541737,6.94565880519307));
#21543=CARTESIAN_POINT('Ctrl Pts',(93.9337854273444,-22.3816622657573,6.99831986027595));
#21544=CARTESIAN_POINT('Ctrl Pts',(93.4015573609318,-21.7456918773409,7.05098091535883));
#21545=CARTESIAN_POINT('Ctrl Pts',(92.5249308776734,-21.3979401088093,7.1036419704417));
#21546=CARTESIAN_POINT('Ctrl Pts',(91.7014710458108,-21.4961183060969,7.15630302552458));
#21547=CARTESIAN_POINT('Ctrl Pts',(90.8780112139482,-21.5942965033845,7.20896408060746));
#21548=CARTESIAN_POINT('Ctrl Pts',(90.1077180334812,-22.1384046664913,7.26162513569034));
#21549=CARTESIAN_POINT('Ctrl Pts',(89.7399326127096,-22.8816804900357,7.31428619077321));
#21550=CARTESIAN_POINT('Ctrl Pts',(89.569684509702,-23.2257433370738,7.33866302635148));
#21551=CARTESIAN_POINT('Ctrl Pts',(89.4856845592314,-23.6124832315577,7.36303986192975));
#21552=CARTESIAN_POINT('Ctrl Pts',(89.4863708146039,-23.9995053986078,7.38741669750802));
#21553=CARTESIAN_POINT('Origin',(92.,-24.,5.));
#21554=CARTESIAN_POINT('',(89.4817891743669,-24.002194435609,8.38741669750802));
#21555=CARTESIAN_POINT('',(89.4784371162896,-23.999680408535,8.11258330249198));
#21556=CARTESIAN_POINT('',(89.4825,-24.,5.));
#21557=CARTESIAN_POINT('Ctrl Pts',(89.4784371162896,-23.999680408535,8.11258330249198));
#21558=CARTESIAN_POINT('Ctrl Pts',(89.4784054922001,-23.9821424240367,8.11146968039084));
#21559=CARTESIAN_POINT('Ctrl Pts',(89.4785728027447,-23.9646050586431,8.11035605828969));
#21560=CARTESIAN_POINT('Ctrl Pts',(89.4789408989109,-23.9470719086913,8.10924243618855));
#21561=CARTESIAN_POINT('Ctrl Pts',(89.4963474612121,-23.1179628469758,8.05658138110567));
#21562=CARTESIAN_POINT('Ctrl Pts',(89.9627433725619,-22.298280199785,8.0039203260228));
#21563=CARTESIAN_POINT('Ctrl Pts',(90.6666099349663,-21.8597638322688,7.95125927093992));
#21564=CARTESIAN_POINT('Ctrl Pts',(91.3704764973707,-21.4212474647526,7.89859821585704));
#21565=CARTESIAN_POINT('Ctrl Pts',(92.3118137108296,-21.3638973769109,7.84593716077416));
#21566=CARTESIAN_POINT('Ctrl Pts',(93.0637091784649,-21.7137229122891,7.79327610569128));
#21567=CARTESIAN_POINT('Ctrl Pts',(93.8156046461002,-22.0635484476673,7.7406150506084));
#21568=CARTESIAN_POINT('Ctrl Pts',(94.378058367912,-22.8205496062654,7.68795399552553));
#21569=CARTESIAN_POINT('Ctrl Pts',(94.4959879359714,-23.6414133946617,7.63529294044265));
#21570=CARTESIAN_POINT('Ctrl Pts',(94.6139175040309,-24.462277183058,7.58263188535977));
#21571=CARTESIAN_POINT('Ctrl Pts',(94.287322918338,-25.3470036012526,7.52997083027689));
#21572=CARTESIAN_POINT('Ctrl Pts',(93.6643204198241,-25.8943541437692,7.47730977519401));
#21573=CARTESIAN_POINT('Ctrl Pts',(93.0413179213102,-26.4417046862858,7.42464872011113));
#21574=CARTESIAN_POINT('Ctrl Pts',(92.1219075099752,-26.6516793531245,7.37198766502826));
#21575=CARTESIAN_POINT('Ctrl Pts',(91.3230574869989,-26.4290510376866,7.31932660994538));
#21576=CARTESIAN_POINT('Ctrl Pts',(90.5242074640225,-26.2064227222488,7.2666655548625));
#21577=CARTESIAN_POINT('Ctrl Pts',(89.8459178294048,-25.5511914245345,7.21400449977963));
#21578=CARTESIAN_POINT('Ctrl Pts',(89.5958045136134,-24.7605157260336,7.16134344469675));
#21579=CARTESIAN_POINT('Ctrl Pts',(89.5186091945673,-24.5164804869872,7.14509006396183));
#21580=CARTESIAN_POINT('Ctrl Pts',(89.4822017382943,-24.2595428818132,7.12883668322691));
#21581=CARTESIAN_POINT('Ctrl Pts',(89.4842078764603,-24.0020516719095,7.11258330249199));
#21582=CARTESIAN_POINT('Ctrl Pts',(89.4863708146039,-23.9995053986078,7.38741669750802));
#21583=CARTESIAN_POINT('Ctrl Pts',(89.4871670704398,-24.4485636814537,7.41570091701263));
#21584=CARTESIAN_POINT('Ctrl Pts',(89.6019742377664,-24.8980019807642,7.44398513651724));
#21585=CARTESIAN_POINT('Ctrl Pts',(89.8283524458306,-25.2815966720592,7.47226935602185));
#21586=CARTESIAN_POINT('Ctrl Pts',(90.2498353607997,-25.9957935465564,7.52493041110473));
#21587=CARTESIAN_POINT('Ctrl Pts',(91.0580788518144,-26.4817438115688,7.57759146618761));
#21588=CARTESIAN_POINT('Ctrl Pts',(91.8865307233466,-26.5190608637177,7.63025252127048));
#21589=CARTESIAN_POINT('Ctrl Pts',(92.7149825948789,-26.5563779158667,7.68291357635336));
#21590=CARTESIAN_POINT('Ctrl Pts',(93.5636428469287,-26.1450617551521,7.73557463143624));
#21591=CARTESIAN_POINT('Ctrl Pts',(94.0476295286171,-25.4716510041371,7.78823568651912));
#21592=CARTESIAN_POINT('Ctrl Pts',(94.5316162103055,-24.798240253122,7.84089674160199));
#21593=CARTESIAN_POINT('Ctrl Pts',(94.6509293216325,-23.8627349118064,7.89355779668488));
#21594=CARTESIAN_POINT('Ctrl Pts',(94.3514584187992,-23.0894031813449,7.94621885176775));
#21595=CARTESIAN_POINT('Ctrl Pts',(94.0519875159659,-22.3160714508834,7.99887990685063));
#21596=CARTESIAN_POINT('Ctrl Pts',(93.3337325989723,-21.7049133312758,8.0515409619335));
#21597=CARTESIAN_POINT('Ctrl Pts',(92.5224343499209,-21.5330983089572,8.10420201701638));
#21598=CARTESIAN_POINT('Ctrl Pts',(91.7111361008695,-21.3612832866386,8.15686307209926));
#21599=CARTESIAN_POINT('Ctrl Pts',(90.8067945197604,-21.6288113616088,8.20952412718214));
#21600=CARTESIAN_POINT('Ctrl Pts',(90.2195443159446,-22.2143563368687,8.26218518226502));
#21601=CARTESIAN_POINT('Ctrl Pts',(89.7540375466956,-22.6785113902208,8.30392902067936));
#21602=CARTESIAN_POINT('Ctrl Pts',(89.4877769931074,-23.3424942170044,8.34567285909369));
#21603=CARTESIAN_POINT('Ctrl Pts',(89.4817891743669,-24.002194435609,8.38741669750802));
#21604=CARTESIAN_POINT('Origin',(92.,-24.,5.));
#21605=CARTESIAN_POINT('',(89.4798238762261,-23.9984131135314,9.38741669750802));
#21606=CARTESIAN_POINT('',(89.4850512338518,-23.9982506073194,9.11258330249198));
#21607=CARTESIAN_POINT('',(89.4825,-24.,5.));
#21608=CARTESIAN_POINT('',(93.9134659966651,-22.3640127966251,10.));
#21609=CARTESIAN_POINT('Ctrl Pts',(89.4798238762261,-23.9984131135314,9.38741669750802));
#21610=CARTESIAN_POINT('Ctrl Pts',(89.4853062059344,-24.7270927102602,9.43362796642338));
#21611=CARTESIAN_POINT('Ctrl Pts',(89.8192672097013,-25.4600319638108,9.47983923533874));
#21612=CARTESIAN_POINT('Ctrl Pts',(90.3760118920419,-25.9288769835329,9.5260505042541));
#21613=CARTESIAN_POINT('Ctrl Pts',(91.0104623858714,-26.46315950787,9.57871155933697));
#21614=CARTESIAN_POINT('Ctrl Pts',(91.9342250444885,-26.6544830013391,9.63137261441985));
#21615=CARTESIAN_POINT('Ctrl Pts',(92.7281293690809,-26.4146106072968,9.68403366950273));
#21616=CARTESIAN_POINT('Ctrl Pts',(93.5220336936733,-26.1747382132545,9.73669472458561));
#21617=CARTESIAN_POINT('Ctrl Pts',(94.186079684241,-25.5036699317008,9.78935577966849));
#21618=CARTESIAN_POINT('Ctrl Pts',(94.4192662809857,-24.7092700865749,9.84201683475137));
#21619=CARTESIAN_POINT('Ctrl Pts',(94.6524528777304,-23.914870241449,9.89467788983425));
#21620=CARTESIAN_POINT('Ctrl Pts',(94.4547800806522,-22.9971388327508,9.94733894491712));
#21621=CARTESIAN_POINT('Ctrl Pts',(93.9134659966651,-22.3640127966251,10.));
#21622=CARTESIAN_POINT('',(90.0828970444786,-22.361465706548,10.));
#21623=CARTESIAN_POINT('Origin',(92.,-24.,10.));
#21624=CARTESIAN_POINT('Ctrl Pts',(90.0828885913555,-22.3614597865289,10.));
#21625=CARTESIAN_POINT('Ctrl Pts',(90.6060434082611,-21.752303655963,9.94901908464118));
#21626=CARTESIAN_POINT('Ctrl Pts',(91.4465814718894,-21.4121729024441,9.89803816928235));
#21627=CARTESIAN_POINT('Ctrl Pts',(92.2457357606075,-21.4905154724921,9.84705725392353));
#21628=CARTESIAN_POINT('Ctrl Pts',(93.0712271767912,-21.5714399197601,9.79439619884065));
#21629=CARTESIAN_POINT('Ctrl Pts',(93.8525621626002,-22.0988748222944,9.74173514375777));
#21630=CARTESIAN_POINT('Ctrl Pts',(94.2358875787344,-22.8341463056132,9.68907408867489));
#21631=CARTESIAN_POINT('Ctrl Pts',(94.6192129948686,-23.5694177889319,9.63641303359201));
#21632=CARTESIAN_POINT('Ctrl Pts',(94.6045288413281,-24.5125258530351,9.58375197850914));
#21633=CARTESIAN_POINT('Ctrl Pts',(94.1982520122281,-25.235497804129,9.53109092342626));
#21634=CARTESIAN_POINT('Ctrl Pts',(93.7919751831282,-25.9584697552228,9.47842986834338));
#21635=CARTESIAN_POINT('Ctrl Pts',(92.9941056784689,-26.4613055933073,9.42576881326051));
#21636=CARTESIAN_POINT('Ctrl Pts',(92.1666097496597,-26.5160865743966,9.37310775817763));
#21637=CARTESIAN_POINT('Ctrl Pts',(91.3391138208505,-26.570867555486,9.32044670309475));
#21638=CARTESIAN_POINT('Ctrl Pts',(90.4819914678916,-26.1775936795802,9.26778564801187));
#21639=CARTESIAN_POINT('Ctrl Pts',(89.9839041146304,-25.5145597074388,9.21512459292899));
#21640=CARTESIAN_POINT('Ctrl Pts',(89.6606132128854,-25.0842077835489,9.18094416278332));
#21641=CARTESIAN_POINT('Ctrl Pts',(89.4885783498304,-24.5402099934131,9.14676373263765));
#21642=CARTESIAN_POINT('Ctrl Pts',(89.4850512338518,-23.9982506073194,9.11258330249198));
#21643=CARTESIAN_POINT('Origin',(92.,-24.,12.2084234471775));
#21644=CARTESIAN_POINT('',(88.9217237789782,-23.9992118506711,1.79157655282254));
#21645=CARTESIAN_POINT('',(88.9313888204345,-23.9996651715868,1.70842344717745));
#21646=CARTESIAN_POINT('',(88.9265,-23.9999999999999,12.2084234471775));
#21647=CARTESIAN_POINT('',(92.7937992825328,-26.9692229537457,0.999999999999999));
#21648=CARTESIAN_POINT('Ctrl Pts',(88.9313888204345,-23.9996651715868,1.70842344717745));
#21649=CARTESIAN_POINT('Ctrl Pts',(88.9310463723584,-23.5053847152746,1.68292651844982));
#21650=CARTESIAN_POINT('Ctrl Pts',(89.2764430280357,-21.9907712812588,1.6047685346393));
#21651=CARTESIAN_POINT('Ctrl Pts',(91.6460838609914,-20.3911589633379,1.4739494957459));
#21652=CARTESIAN_POINT('Ctrl Pts',(94.8312242725849,-21.7301456837402,1.31596633049727));
#21653=CARTESIAN_POINT('Ctrl Pts',(95.4433140827682,-25.1332953965992,1.15798316524863));
#21654=CARTESIAN_POINT('Ctrl Pts',(93.7762533017603,-26.7065713079336,1.05266105508288));
#21655=CARTESIAN_POINT('Ctrl Pts',(92.7937992825328,-26.9692229537457,0.999999999999999));
#21656=CARTESIAN_POINT('',(91.2062007174671,-26.9692229537457,1.));
#21657=CARTESIAN_POINT('Origin',(92.,-24.,0.999999999999999));
#21658=CARTESIAN_POINT('Ctrl Pts',(88.9217237789782,-23.9992118506711,1.79157655282254));
#21659=CARTESIAN_POINT('Ctrl Pts',(88.9215776858271,-23.9562584671078,1.78934283757203));
#21660=CARTESIAN_POINT('Ctrl Pts',(88.9417782923113,-22.9007977729438,1.73444806723864));
#21661=CARTESIAN_POINT('Ctrl Pts',(90.1476053652115,-20.8820474355396,1.62689224182238));
#21662=CARTESIAN_POINT('Ctrl Pts',(93.5990313571954,-20.7444874247256,1.46890907657374));
#21663=CARTESIAN_POINT('Ctrl Pts',(95.5999505159819,-23.5606294856849,1.31092591132511));
#21664=CARTESIAN_POINT('Ctrl Pts',(94.349302269142,-26.7394085052657,1.15462288580053));
#21665=CARTESIAN_POINT('Ctrl Pts',(92.1519061796922,-27.2254057458095,1.05098091535883));
#21666=CARTESIAN_POINT('Ctrl Pts',(91.2042985533737,-26.9743125149969,1.));
#21667=CARTESIAN_POINT('Origin',(92.,-24.,12.2084234471775));
#21668=CARTESIAN_POINT('',(88.930051482524,-23.9980972113707,2.79157655282254));
#21669=CARTESIAN_POINT('',(88.9249913784601,-24.0025755321659,2.70842344717745));
#21670=CARTESIAN_POINT('',(88.9265,-23.9999999999999,12.2084234471775));
#21671=CARTESIAN_POINT('Ctrl Pts',(88.9249913784601,-24.0025755321659,2.70842344717745));
#21672=CARTESIAN_POINT('Ctrl Pts',(88.9323854338683,-23.1760102376997,2.66555951561375));
#21673=CARTESIAN_POINT('Ctrl Pts',(89.7006357273797,-21.3218326978092,2.57003452896717));
#21674=CARTESIAN_POINT('Ctrl Pts',(92.8261378655289,-20.4685618660265,2.42184848723771));
#21675=CARTESIAN_POINT('Ctrl Pts',(95.4089767382702,-22.7619776329039,2.26386532198907));
#21676=CARTESIAN_POINT('Ctrl Pts',(94.899688828372,-26.1783943608088,2.10588215674044));
#21677=CARTESIAN_POINT('Ctrl Pts',(91.7604241409854,-27.6187851374898,1.9478989914918));
#21678=CARTESIAN_POINT('Ctrl Pts',(89.3097989934579,-26.0743436082074,1.81541275497081));
#21679=CARTESIAN_POINT('Ctrl Pts',(88.9317536605653,-24.5262657246815,1.73558757353269));
#21680=CARTESIAN_POINT('Ctrl Pts',(88.9313888204345,-23.9996651715868,1.70842344717745));
#21681=CARTESIAN_POINT('Ctrl Pts',(88.930051482524,-23.9980972113707,2.79157655282254));
#21682=CARTESIAN_POINT('Ctrl Pts',(88.9278794195688,-23.6185397913437,2.77197583473597));
#21683=CARTESIAN_POINT('Ctrl Pts',(89.1684425268395,-22.2218847391138,2.69971406156651));
#21684=CARTESIAN_POINT('Ctrl Pts',(91.2485917742672,-20.451900203599,2.57479123331418));
#21685=CARTESIAN_POINT('Ctrl Pts',(94.5607981614372,-21.4317381309793,2.41680806806555));
#21686=CARTESIAN_POINT('Ctrl Pts',(95.5502714048858,-24.7410888412383,2.25882490281692));
#21687=CARTESIAN_POINT('Ctrl Pts',(93.3195309927209,-27.3782229777192,2.10084173756828));
#21688=CARTESIAN_POINT('Ctrl Pts',(89.9403861581344,-26.9572790184773,1.94509228757016));
#21689=CARTESIAN_POINT('Ctrl Pts',(88.9250219115292,-24.96890790723,1.84200389265491));
#21690=CARTESIAN_POINT('Ctrl Pts',(88.9217237789782,-23.9992118506711,1.79157655282254));
#21691=CARTESIAN_POINT('Origin',(92.,-24.,12.2084234471775));
#21692=CARTESIAN_POINT('',(88.9283007496159,-24.0025715689449,3.79157655282255));
#21693=CARTESIAN_POINT('',(88.9237791307625,-23.9977671182961,3.70842344717745));
#21694=CARTESIAN_POINT('',(88.9265,-23.9999999999999,12.2084234471775));
#21695=CARTESIAN_POINT('Ctrl Pts',(88.9237791307624,-23.9977671182961,3.70842344717745));
#21696=CARTESIAN_POINT('Ctrl Pts',(88.9225843518948,-23.8519430302087,3.70085356786056));
#21697=CARTESIAN_POINT('Ctrl Pts',(88.9980297211289,-22.6929123616698,3.6406226334608));
#21698=CARTESIAN_POINT('Ctrl Pts',(90.4700852939275,-20.7116866521342,3.52773064397815));
#21699=CARTESIAN_POINT('Ctrl Pts',(93.9177920746623,-20.9217349563625,3.36974747872952));
#21700=CARTESIAN_POINT('Ctrl Pts',(95.625996447417,-23.9238742346134,3.21176431348088));
#21701=CARTESIAN_POINT('Ctrl Pts',(94.0452973355112,-26.9950631778383,3.05378114823225));
#21702=CARTESIAN_POINT('Ctrl Pts',(90.6094456576621,-27.3496255535896,2.89579798298361));
#21703=CARTESIAN_POINT('Ctrl Pts',(89.0248752439865,-25.3940964847871,2.78067874929868));
#21704=CARTESIAN_POINT('Ctrl Pts',(88.923301368433,-24.1914980595946,2.71822057069663));
#21705=CARTESIAN_POINT('Ctrl Pts',(88.9249913784601,-24.0025755321659,2.70842344717745));
#21706=CARTESIAN_POINT('Ctrl Pts',(88.9283007496159,-24.0025715689449,3.79157655282255));
#21707=CARTESIAN_POINT('Ctrl Pts',(88.934059068375,-23.287740701024,3.75460883189991));
#21708=CARTESIAN_POINT('Ctrl Pts',(89.5376069996118,-21.5458537101333,3.66498005589439));
#21709=CARTESIAN_POINT('Ctrl Pts',(92.429368893546,-20.3987114188412,3.52269022480599));
#21710=CARTESIAN_POINT('Ctrl Pts',(95.2506148119859,-22.3915408673733,3.36470705955735));
#21711=CARTESIAN_POINT('Ctrl Pts',(95.1234421205799,-25.8432978095596,3.20672389430872));
#21712=CARTESIAN_POINT('Ctrl Pts',(92.1632008669202,-27.6231203956681,3.04874072906009));
#21713=CARTESIAN_POINT('Ctrl Pts',(89.4405688436026,-26.3035551797938,2.91035828189803));
#21714=CARTESIAN_POINT('Ctrl Pts',(88.9337150795902,-24.6382929511448,2.82463688981885));
#21715=CARTESIAN_POINT('Ctrl Pts',(88.930051482524,-23.9980972113707,2.79157655282254));
#21716=CARTESIAN_POINT('Origin',(92.,-24.,12.2084234471775));
#21717=CARTESIAN_POINT('',(88.9216167340283,-23.9994167252631,4.79157655282255));
#21718=CARTESIAN_POINT('',(88.9312807091126,-23.9995675532497,4.70842344717745));
#21719=CARTESIAN_POINT('',(88.9265,-23.9999999999999,12.2084234471775));
#21720=CARTESIAN_POINT('Ctrl Pts',(88.9312807091126,-23.9995675532497,4.70842344717745));
#21721=CARTESIAN_POINT('Ctrl Pts',(88.9306675557931,-23.5161929213318,4.6834865650245));
#21722=CARTESIAN_POINT('Ctrl Pts',(89.2653046726707,-22.0128431381641,4.60588862778867));
#21723=CARTESIAN_POINT('Ctrl Pts',(91.6086716990242,-20.394378610344,4.47562963546995));
#21724=CARTESIAN_POINT('Ctrl Pts',(94.8057463695968,-21.7018636398323,4.31764647022133));
#21725=CARTESIAN_POINT('Ctrl Pts',(95.4579133231718,-25.0938367815869,4.15966330497269));
#21726=CARTESIAN_POINT('Ctrl Pts',(92.9736348536358,-27.493662641186,4.00168013972405));
#21727=CARTESIAN_POINT('Ctrl Pts',(89.7675877362369,-26.761466587215,3.85126685379231));
#21728=CARTESIAN_POINT('Ctrl Pts',(88.9308960188484,-24.8663912154056,3.75351462294344));
#21729=CARTESIAN_POINT('Ctrl Pts',(88.9237791307624,-23.9977671182961,3.70842344717745));
#21730=CARTESIAN_POINT('Ctrl Pts',(88.9216167340283,-23.9994167252631,4.79157655282255));
#21731=CARTESIAN_POINT('Ctrl Pts',(88.9215321543705,-23.9672353813211,4.78990288414672));
#21732=CARTESIAN_POINT('Ctrl Pts',(88.9365123597457,-22.9225665616792,4.73556816038801));
#21733=CARTESIAN_POINT('Ctrl Pts',(90.1148106026499,-20.9016620282348,4.62857238154643));
#21734=CARTESIAN_POINT('Ctrl Pts',(93.5645420118329,-20.7280211581598,4.4705892162978));
#21735=CARTESIAN_POINT('Ctrl Pts',(95.595180415279,-23.5221767762025,4.31260605104916));
#21736=CARTESIAN_POINT('Ctrl Pts',(94.3648674705089,-26.7497343695717,4.15462288580053));
#21737=CARTESIAN_POINT('Ctrl Pts',(90.9895390126931,-27.4831890308961,3.99663972055189));
#21738=CARTESIAN_POINT('Ctrl Pts',(89.1060884403934,-25.6249316453216,3.8756242762259));
#21739=CARTESIAN_POINT('Ctrl Pts',(88.9258562597141,-24.3060276489616,3.80726988698278));
#21740=CARTESIAN_POINT('Ctrl Pts',(88.9283007496159,-24.0025715689449,3.79157655282255));
#21741=CARTESIAN_POINT('Origin',(92.,-24.,12.2084234471775));
#21742=CARTESIAN_POINT('',(88.929838025779,-23.9979746552741,5.79157655282255));
#21743=CARTESIAN_POINT('',(88.9253102843548,-24.0026322735621,5.70842344717746));
#21744=CARTESIAN_POINT('',(88.9265,-23.9999999999999,12.2084234471775));
#21745=CARTESIAN_POINT('Ctrl Pts',(88.9253102843548,-24.0026322735621,5.70842344717746));
#21746=CARTESIAN_POINT('Ctrl Pts',(88.9326787378706,-23.1866490960334,5.66611956218844));
#21747=CARTESIAN_POINT('Ctrl Pts',(89.6842660273292,-21.3429095601006,5.57115462211654));
#21748=CARTESIAN_POINT('Ctrl Pts',(92.7888215932045,-20.4600276931837,5.42352862696176));
#21749=CARTESIAN_POINT('Ctrl Pts',(95.3956989960243,-22.7260801567682,5.26554546171313));
#21750=CARTESIAN_POINT('Ctrl Pts',(94.9225615070513,-26.1476213996829,5.10756229646449));
#21751=CARTESIAN_POINT('Ctrl Pts',(91.7985609777146,-27.6211967303539,4.94957913121586));
#21752=CARTESIAN_POINT('Ctrl Pts',(89.3215407425041,-26.0960765086132,4.81653284812018));
#21753=CARTESIAN_POINT('Ctrl Pts',(88.9319623969259,-24.5369708181419,4.73614762010738));
#21754=CARTESIAN_POINT('Ctrl Pts',(88.9312807091126,-23.9995675532497,4.70842344717745));
#21755=CARTESIAN_POINT('Ctrl Pts',(88.929838025779,-23.9979746552741,5.79157655282255));
#21756=CARTESIAN_POINT('Ctrl Pts',(88.9275818676586,-23.6293267200531,5.77253588131065));
#21757=CARTESIAN_POINT('Ctrl Pts',(89.1590710242286,-22.2438421434169,5.70083415471588));
#21758=CARTESIAN_POINT('Ctrl Pts',(91.2111785923562,-20.4600285259192,5.57647137303824));
#21759=CARTESIAN_POINT('Ctrl Pts',(94.53354332288,-21.4048515492551,5.4184882077896));
#21760=CARTESIAN_POINT('Ctrl Pts',(95.5578977842681,-24.7035627953589,5.26050504254097));
#21761=CARTESIAN_POINT('Ctrl Pts',(93.3551175166525,-27.3641185720073,5.10252187729233));
#21762=CARTESIAN_POINT('Ctrl Pts',(89.9595570406981,-26.9774442566838,4.94621238071953));
#21763=CARTESIAN_POINT('Ctrl Pts',(88.924193406317,-24.9798034901964,4.8425639392296));
#21764=CARTESIAN_POINT('Ctrl Pts',(88.9216167340283,-23.9994167252631,4.79157655282255));
#21765=CARTESIAN_POINT('Origin',(92.,-24.,12.2084234471775));
#21766=CARTESIAN_POINT('',(88.9285850678455,-24.0025047919022,6.79157655282255));
#21767=CARTESIAN_POINT('',(88.9234957058127,-23.9978813008156,6.70842344717745));
#21768=CARTESIAN_POINT('',(88.9265,-23.9999999999999,12.2084234471775));
#21769=CARTESIAN_POINT('Ctrl Pts',(88.9234957058127,-23.9978813008156,6.70842344717746));
#21770=CARTESIAN_POINT('Ctrl Pts',(88.9224297712393,-23.862878283601,6.70141361443525));
#21771=CARTESIAN_POINT('Ctrl Pts',(88.9915973803182,-22.7147700696948,6.64174272661017));
#21772=CARTESIAN_POINT('Ctrl Pts',(90.4354576201273,-20.7280203884636,6.52941078370221));
#21773=CARTESIAN_POINT('Ctrl Pts',(93.8851898408184,-20.9016612993894,6.37142761845357));
#21774=CARTESIAN_POINT('Ctrl Pts',(95.6249905303983,-23.885601165237,6.21344445320494));
#21775=CARTESIAN_POINT('Ctrl Pts',(94.0768010801705,-26.9733046786334,6.0554612879563));
#21776=CARTESIAN_POINT('Ctrl Pts',(90.6448821645723,-27.3641193633755,5.89747812270767));
#21777=CARTESIAN_POINT('Ctrl Pts',(89.031950207745,-25.4159924901842,5.78179884244805));
#21778=CARTESIAN_POINT('Ctrl Pts',(88.9235062815685,-24.2024076976298,5.71878061727132));
#21779=CARTESIAN_POINT('Ctrl Pts',(88.9253102843548,-24.0026322735621,5.70842344717746));
#21780=CARTESIAN_POINT('Ctrl Pts',(88.9285850678455,-24.0025047919022,6.79157655282255));
#21781=CARTESIAN_POINT('Ctrl Pts',(88.934071295281,-23.2983382673306,6.75516887847459));
#21782=CARTESIAN_POINT('Ctrl Pts',(89.5231707262624,-21.5673495506398,6.66610014904376));
#21783=CARTESIAN_POINT('Ctrl Pts',(92.3913282089151,-20.3943794585145,6.52437036453004));
#21784=CARTESIAN_POINT('Ctrl Pts',(95.2334540881775,-22.3573156385801,6.36638719928141));
#21785=CARTESIAN_POINT('Ctrl Pts',(95.1427267432077,-25.8102226011645,6.20840403403277));
#21786=CARTESIAN_POINT('Ctrl Pts',(92.2014389749,-27.6211958785123,6.05042086878414));
#21787=CARTESIAN_POINT('Ctrl Pts',(89.4539543223964,-26.3252211924294,5.9114783750474));
#21788=CARTESIAN_POINT('Ctrl Pts',(88.933821756151,-24.6489015397087,5.82519693639353));
#21789=CARTESIAN_POINT('Ctrl Pts',(88.929838025779,-23.9979746552741,5.79157655282255));
#21790=CARTESIAN_POINT('Origin',(92.,-24.,12.2084234471775));
#21791=CARTESIAN_POINT('',(88.9215398120818,-23.9996098254745,7.79157655282255));
#21792=CARTESIAN_POINT('',(88.931225699577,-23.9993961639011,7.70842344717745));
#21793=CARTESIAN_POINT('',(88.9265,-23.9999999999999,12.2084234471775));
#21794=CARTESIAN_POINT('Ctrl Pts',(88.931225699577,-23.9993961639011,7.70842344717745));
#21795=CARTESIAN_POINT('Ctrl Pts',(88.9303878819455,-23.526898594714,7.68404661159918));
#21796=CARTESIAN_POINT('Ctrl Pts',(89.2544810105531,-22.0347579248864,7.60700872093804));
#21797=CARTESIAN_POINT('Ctrl Pts',(91.5706310054557,-20.3987105715367,7.47730977519401));
#21798=CARTESIAN_POINT('Ctrl Pts',(94.7813299086865,-21.6723730071853,7.31932660994538));
#21799=CARTESIAN_POINT('Ctrl Pts',(95.4692676579736,-25.0572726103797,7.16134344469675));
#21800=CARTESIAN_POINT('Ctrl Pts',(93.0104612250053,-27.483189850294,7.00336027944811));
#21801=CARTESIAN_POINT('Ctrl Pts',(89.7848978894953,-26.7822789631047,6.85238694694168));
#21802=CARTESIAN_POINT('Ctrl Pts',(88.9304375570666,-24.8770824147627,6.75407466951813));
#21803=CARTESIAN_POINT('Ctrl Pts',(88.9234957058127,-23.9978813008156,6.70842344717746));
#21804=CARTESIAN_POINT('Ctrl Pts',(88.9215398120818,-23.9996098254745,7.79157655282255));
#21805=CARTESIAN_POINT('Ctrl Pts',(88.921501203685,-23.9781985065647,7.79046293072141));
#21806=CARTESIAN_POINT('Ctrl Pts',(88.9313646122183,-22.9443234457007,7.73668825353739));
#21807=CARTESIAN_POINT('Ctrl Pts',(90.0822083770022,-20.9217356813897,7.63025252127048));
#21808=CARTESIAN_POINT('Ctrl Pts',(93.5299143458989,-20.7116874252053,7.47226935602185));
#21809=CARTESIAN_POINT('Ctrl Pts',(95.5899360110292,-23.4842511522573,7.31428619077322));
#21810=CARTESIAN_POINT('Ctrl Pts',(94.3937630706594,-26.7246165699189,7.15630302552457));
#21811=CARTESIAN_POINT('Ctrl Pts',(91.0263653754403,-27.4936618194068,6.99831986027595));
#21812=CARTESIAN_POINT('Ctrl Pts',(89.1145964666983,-25.6468831586791,6.87674436937527));
#21813=CARTESIAN_POINT('Ctrl Pts',(88.9261358659971,-24.3168639711034,6.80782993355747));
#21814=CARTESIAN_POINT('Ctrl Pts',(88.9285850678455,-24.0025047919022,6.79157655282255));
#21815=CARTESIAN_POINT('Origin',(92.,-24.,12.2084234471775));
#21816=CARTESIAN_POINT('',(88.9296146841086,-23.99786424691,8.79157655282255));
#21817=CARTESIAN_POINT('',(88.925632185667,-24.0026790855389,8.70842344717746));
#21818=CARTESIAN_POINT('',(88.9265,-23.9999999999999,12.2084234471775));
#21819=CARTESIAN_POINT('Ctrl Pts',(88.925632185667,-24.0026790855389,8.70842344717745));
#21820=CARTESIAN_POINT('Ctrl Pts',(88.9329424382585,-23.1972814204421,8.66667960876312));
#21821=CARTESIAN_POINT('Ctrl Pts',(89.6680869085145,-21.3640271254411,8.57227471526591));
#21822=CARTESIAN_POINT('Ctrl Pts',(92.7514084034007,-20.4518993616932,8.42520876668581));
#21823=CARTESIAN_POINT('Ctrl Pts',(95.38206161577,-22.6903039066152,8.26722560143718));
#21824=CARTESIAN_POINT('Ctrl Pts',(94.9450699403021,-26.1166502818288,8.10924243618855));
#21825=CARTESIAN_POINT('Ctrl Pts',(91.8367990946118,-27.6231212490059,7.95125927093992));
#21826=CARTESIAN_POINT('Ctrl Pts',(89.3333230992967,-26.1179253063225,7.81765294126955));
#21827=CARTESIAN_POINT('Ctrl Pts',(88.9321978117167,-24.5476307745572,7.73670766668206));
#21828=CARTESIAN_POINT('Ctrl Pts',(88.931225699577,-23.9993961639011,7.70842344717745));
#21829=CARTESIAN_POINT('Ctrl Pts',(88.9296146841086,-23.99786424691,8.79157655282255));
#21830=CARTESIAN_POINT('Ctrl Pts',(88.9272864716551,-23.6401225112663,8.77309592788534));
#21831=CARTESIAN_POINT('Ctrl Pts',(89.149833727977,-22.265786270585,8.70195424786526));
#21832=CARTESIAN_POINT('Ctrl Pts',(91.1738623478633,-20.4685627419331,8.57815151276229));
#21833=CARTESIAN_POINT('Ctrl Pts',(94.5060020988175,-21.3782461595948,8.42016834751366));
#21834=CARTESIAN_POINT('Ctrl Pts',(95.5651288739418,-24.665967239189,8.26218518226502));
#21835=CARTESIAN_POINT('Ctrl Pts',(93.3905540118639,-27.3496247591347,8.10420201701638));
#21836=CARTESIAN_POINT('Ctrl Pts',(89.9789224334285,-26.9975617834284,7.94733247386889));
#21837=CARTESIAN_POINT('Ctrl Pts',(88.9233269207872,-24.9906987464103,7.84312398580428));
#21838=CARTESIAN_POINT('Ctrl Pts',(88.9215398120818,-23.9996098254745,7.79157655282255));
#21839=CARTESIAN_POINT('Origin',(92.,-24.,12.2084234471775));
#21840=CARTESIAN_POINT('',(88.9297109890477,-24.0031050978172,9.79157655282255));
#21841=CARTESIAN_POINT('',(88.9232328435277,-23.9980626432726,9.70842344717746));
#21842=CARTESIAN_POINT('',(88.9265,-23.9999999999999,12.2084234471775));
#21843=CARTESIAN_POINT('',(91.2062007174671,-26.9692229537457,10.));
#21844=CARTESIAN_POINT('Ctrl Pts',(91.2062007174671,-26.9692229537457,10.));
#21845=CARTESIAN_POINT('Ctrl Pts',(90.2237466982397,-26.7065713079336,9.94733894491712));
#21846=CARTESIAN_POINT('Ctrl Pts',(89.1240889563566,-25.6687841901452,9.87786446252464));
#21847=CARTESIAN_POINT('Ctrl Pts',(88.9273641407895,-24.3283664602092,9.80838998013216));
#21848=CARTESIAN_POINT('Ctrl Pts',(88.9297109890477,-24.0031050978172,9.79157655282255));
#21849=CARTESIAN_POINT('',(92.7956974280508,-26.974301052007,10.));
#21850=CARTESIAN_POINT('Origin',(92.,-24.,10.));
#21851=CARTESIAN_POINT('Ctrl Pts',(92.7957018439802,-26.9743128659187,10.));
#21852=CARTESIAN_POINT('Ctrl Pts',(91.8480947973977,-27.2254055278759,9.94901908464117));
#21853=CARTESIAN_POINT('Ctrl Pts',(89.7874433743318,-26.7696547721755,9.85182690036699));
#21854=CARTESIAN_POINT('Ctrl Pts',(88.9299259678011,-24.8876740595768,9.75463471609281));
#21855=CARTESIAN_POINT('Ctrl Pts',(88.9232328435277,-23.9980626432726,9.70842344717746));
#21856=CARTESIAN_POINT('Origin',(24.,92.,5.));
#21857=CARTESIAN_POINT('',(21.4865042982783,92.0002742229179,1.38741669750802));
#21858=CARTESIAN_POINT('',(21.4843731420169,91.9964690566784,1.11258330249198));
#21859=CARTESIAN_POINT('',(21.4825,92.,5.));
#21860=CARTESIAN_POINT('',(22.086534003335,93.635987203375,0.999999999999999));
#21861=CARTESIAN_POINT('Ctrl Pts',(21.4843731420169,91.9964690566784,1.11258330249198));
#21862=CARTESIAN_POINT('Ctrl Pts',(21.4895360512898,92.5890870308544,1.07505553499465));
#21863=CARTESIAN_POINT('Ctrl Pts',(21.700778171916,93.1848035603045,1.03752776749732));
#21864=CARTESIAN_POINT('Ctrl Pts',(22.086534003335,93.635987203375,0.99999999999999));
#21865=CARTESIAN_POINT('',(21.4825,92.,1.));
#21866=CARTESIAN_POINT('Origin',(24.,92.,1.));
#21867=CARTESIAN_POINT('',(21.4825,92.,0.));
#21868=CARTESIAN_POINT('',(21.4825,92.,5.));
#21869=CARTESIAN_POINT('Origin',(24.,92.,0.));
#21870=CARTESIAN_POINT('',(25.917103468466,93.6385343514563,0.999999999999998));
#21871=CARTESIAN_POINT('Origin',(24.,92.,1.));
#21872=CARTESIAN_POINT('Ctrl Pts',(25.9171119325404,93.6385402784441,0.999999999999998));
#21873=CARTESIAN_POINT('Ctrl Pts',(25.393957270488,94.247695615171,1.05098091535882));
#21874=CARTESIAN_POINT('Ctrl Pts',(24.5534188240449,94.5878280192362,1.10196183071765));
#21875=CARTESIAN_POINT('Ctrl Pts',(23.7542642184068,94.50948576913,1.15294274607647));
#21876=CARTESIAN_POINT('Ctrl Pts',(22.9287724748585,94.4285616523478,1.20560380115935));
#21877=CARTESIAN_POINT('Ctrl Pts',(22.1474372319946,93.9011256605461,1.25826485624223));
#21878=CARTESIAN_POINT('Ctrl Pts',(21.7641117257107,93.1658537555941,1.31092591132511));
#21879=CARTESIAN_POINT('Ctrl Pts',(21.5785168283464,92.8098567987064,1.33642284005274));
#21880=CARTESIAN_POINT('Ctrl Pts',(21.4862237958222,92.4051387264905,1.36191976878038));
#21881=CARTESIAN_POINT('Ctrl Pts',(21.4865042982783,92.0002742229179,1.38741669750802));
#21882=CARTESIAN_POINT('Origin',(24.,92.,5.));
#21883=CARTESIAN_POINT('',(21.4812641621455,91.9978903848741,2.38741669750802));
#21884=CARTESIAN_POINT('',(21.4785876236681,92.0006455599548,2.11258330249197));
#21885=CARTESIAN_POINT('',(21.4825,92.,5.));
#21886=CARTESIAN_POINT('Ctrl Pts',(21.4785876236681,92.0006455599548,2.11258330249197));
#21887=CARTESIAN_POINT('Ctrl Pts',(21.4784679588297,92.0358286254365,2.11034958724146));
#21888=CARTESIAN_POINT('Ctrl Pts',(21.4791412415305,92.071006953815,2.10811587199095));
#21889=CARTESIAN_POINT('Ctrl Pts',(21.480621792432,92.1061512101347,2.10588215674043));
#21890=CARTESIAN_POINT('Ctrl Pts',(21.5155265872823,92.9346962171463,2.05322110165756));
#21891=CARTESIAN_POINT('Ctrl Pts',(21.9991161631697,93.7443037579804,2.00056004657468));
#21892=CARTESIAN_POINT('Ctrl Pts',(22.7120874500748,94.1678867011383,1.9478989914918));
#21893=CARTESIAN_POINT('Ctrl Pts',(23.4250587369799,94.5914696442962,1.89523793640892));
#21894=CARTESIAN_POINT('Ctrl Pts',(24.3674117349026,94.6290279897781,1.84257688132604));
#21895=CARTESIAN_POINT('Ctrl Pts',(25.1117466201968,94.2633574548232,1.78991582624316));
#21896=CARTESIAN_POINT('Ctrl Pts',(25.8560815054909,93.8976869198683,1.73725477116029));
#21897=CARTESIAN_POINT('Ctrl Pts',(26.4023982781565,93.1287875044767,1.68459371607741));
#21898=CARTESIAN_POINT('Ctrl Pts',(26.5029873847571,92.3057173158972,1.63193266099453));
#21899=CARTESIAN_POINT('Ctrl Pts',(26.6035764913577,91.4826471273178,1.57927160591165));
#21900=CARTESIAN_POINT('Ctrl Pts',(26.2584379318934,90.6054061655505,1.52661055082877));
#21901=CARTESIAN_POINT('Ctrl Pts',(25.6239876980049,90.0711235918099,1.4739494957459));
#21902=CARTESIAN_POINT('Ctrl Pts',(24.9895374641163,89.5368410180693,1.42128844066302));
#21903=CARTESIAN_POINT('Ctrl Pts',(24.0657755558035,89.3455168323553,1.36862738558014));
#21904=CARTESIAN_POINT('Ctrl Pts',(23.2718708195104,89.5853896272901,1.31596633049726));
#21905=CARTESIAN_POINT('Ctrl Pts',(22.4779660832173,89.8252624222249,1.26330527541438));
#21906=CARTESIAN_POINT('Ctrl Pts',(21.8139185189438,90.4963321978086,1.2106442203315));
#21907=CARTESIAN_POINT('Ctrl Pts',(21.5807319779765,91.2907318840647,1.15798316524862));
#21908=CARTESIAN_POINT('Ctrl Pts',(21.5137208066282,91.5190197315273,1.14284987766308));
#21909=CARTESIAN_POINT('Ctrl Pts',(21.4822911692267,91.7574924580249,1.12771659007753));
#21910=CARTESIAN_POINT('Ctrl Pts',(21.4843731420169,91.9964690566784,1.11258330249198));
#21911=CARTESIAN_POINT('Ctrl Pts',(21.4865042982783,92.0002742229179,1.38741669750802));
#21912=CARTESIAN_POINT('Ctrl Pts',(21.486803142278,91.5689363684933,1.41458082386326));
#21913=CARTESIAN_POINT('Ctrl Pts',(21.5921777588412,91.1374323068698,1.4417449502185));
#21914=CARTESIAN_POINT('Ctrl Pts',(21.8017473998347,90.764501991722,1.46890907657374));
#21915=CARTESIAN_POINT('Ctrl Pts',(22.2080243499465,90.0415299509042,1.52157013165662));
#21916=CARTESIAN_POINT('Ctrl Pts',(23.0058940198741,89.5386936873713,1.5742311867395));
#21917=CARTESIAN_POINT('Ctrl Pts',(23.833390176038,89.4839126258589,1.62689224182238));
#21918=CARTESIAN_POINT('Ctrl Pts',(24.6608863322019,89.4291315643466,1.67955329690525));
#21919=CARTESIAN_POINT('Ctrl Pts',(25.5180089746021,89.8224057048548,1.73221435198813));
#21920=CARTESIAN_POINT('Ctrl Pts',(26.0160964783391,90.4854399019793,1.78487540707101));
#21921=CARTESIAN_POINT('Ctrl Pts',(26.5141839820761,91.1484740991038,1.83753646215389));
#21922=CARTESIAN_POINT('Ctrl Pts',(26.6532363471501,92.0812683528444,1.89019751723676));
#21923=CARTESIAN_POINT('Ctrl Pts',(26.3701624990712,92.8607544964156,1.94285857231964));
#21924=CARTESIAN_POINT('Ctrl Pts',(26.0870886509923,93.6402406399867,1.99551962740252));
#21925=CARTESIAN_POINT('Ctrl Pts',(25.3818885897605,94.2664186733884,2.0481806824854));
#21926=CARTESIAN_POINT('Ctrl Pts',(24.5743965080577,94.4553208851494,2.10084173756828));
#21927=CARTESIAN_POINT('Ctrl Pts',(23.7669044263549,94.6442230969105,2.15350279265116));
#21928=CARTESIAN_POINT('Ctrl Pts',(22.857120324181,94.3958494870309,2.20616384773403));
#21929=CARTESIAN_POINT('Ctrl Pts',(22.2576399987561,93.8228345233925,2.25882490281691));
#21930=CARTESIAN_POINT('Ctrl Pts',(21.7696876855645,93.3564239255092,2.30168883438062));
#21931=CARTESIAN_POINT('Ctrl Pts',(21.4873206236216,92.6749290158026,2.34455276594432));
#21932=CARTESIAN_POINT('Ctrl Pts',(21.4812641621455,91.9978903848741,2.38741669750802));
#21933=CARTESIAN_POINT('Origin',(24.,92.,5.));
#21934=CARTESIAN_POINT('',(21.4802712114252,92.0018289507128,3.38741669750802));
#21935=CARTESIAN_POINT('',(21.4854088326161,92.0015585716341,3.11258330249198));
#21936=CARTESIAN_POINT('',(21.4825,92.,5.));
#21937=CARTESIAN_POINT('Ctrl Pts',(21.4854088326161,92.0015585716341,3.11258330249198));
#21938=CARTESIAN_POINT('Ctrl Pts',(21.4836296984461,92.3124536014081,3.0929825844054));
#21939=CARTESIAN_POINT('Ctrl Pts',(21.5370773572355,92.6227586333046,3.07338186631882));
#21940=CARTESIAN_POINT('Ctrl Pts',(21.6485419638298,92.910596671031,3.05378114823224));
#21941=CARTESIAN_POINT('Ctrl Pts',(21.9480128179958,93.6839282751438,3.00112009314936));
#21942=CARTESIAN_POINT('Ctrl Pts',(22.666267618347,94.2950862932019,2.94845903806648));
#21943=CARTESIAN_POINT('Ctrl Pts',(23.4775657352139,94.4669012884929,2.8957979829836));
#21944=CARTESIAN_POINT('Ctrl Pts',(24.2888638520808,94.638716283784,2.84313692790073));
#21945=CARTESIAN_POINT('Ctrl Pts',(25.1932052854634,94.371188256308,2.79047587281785));
#21946=CARTESIAN_POINT('Ctrl Pts',(25.7804553940472,93.7856433745946,2.73781481773497));
#21947=CARTESIAN_POINT('Ctrl Pts',(26.367705502631,93.2000984928813,2.68515376265209));
#21948=CARTESIAN_POINT('Ctrl Pts',(26.6378642864159,92.2965367569306,2.63249270756921));
#21949=CARTESIAN_POINT('Ctrl Pts',(26.4684108772915,91.4847436484407,2.57983165248634));
#21950=CARTESIAN_POINT('Ctrl Pts',(26.2989574681671,90.6729505399509,2.52717059740346));
#21951=CARTESIAN_POINT('Ctrl Pts',(25.6898918661334,89.9529260589219,2.47450954232058));
#21952=CARTESIAN_POINT('Ctrl Pts',(24.9174341827592,89.6512037648828,2.4218484872377));
#21953=CARTESIAN_POINT('Ctrl Pts',(24.1449764993849,89.3494814708436,2.36918743215482));
#21954=CARTESIAN_POINT('Ctrl Pts',(23.2091267346701,89.4660613637943,2.31652637707195));
#21955=CARTESIAN_POINT('Ctrl Pts',(22.5343118592193,89.9480925468641,2.26386532198907));
#21956=CARTESIAN_POINT('Ctrl Pts',(21.8881204945621,90.4096774930869,2.2134379821567));
#21957=CARTESIAN_POINT('Ctrl Pts',(21.4812891226481,91.2063686712679,2.16301064232434));
#21958=CARTESIAN_POINT('Ctrl Pts',(21.4785876236681,92.0006455599548,2.11258330249197));
#21959=CARTESIAN_POINT('Ctrl Pts',(21.4812641621455,91.9978903848741,2.38741669750802));
#21960=CARTESIAN_POINT('Ctrl Pts',(21.47987987706,91.8431441716248,2.3972138210272));
#21961=CARTESIAN_POINT('Ctrl Pts',(21.492930389882,91.6886307597355,2.40701094454637));
#21962=CARTESIAN_POINT('Ctrl Pts',(21.5212601912555,91.5369715569028,2.41680806806554));
#21963=CARTESIAN_POINT('Ctrl Pts',(21.6735372578557,90.7217798714484,2.46946912314842));
#21964=CARTESIAN_POINT('Ctrl Pts',(22.2672679397321,89.9890528179368,2.5221301782313));
#21965=CARTESIAN_POINT('Ctrl Pts',(23.0331836055545,89.6710928935685,2.57479123331418));
#21966=CARTESIAN_POINT('Ctrl Pts',(23.7990992713769,89.3531329692002,2.62745228839706));
#21967=CARTESIAN_POINT('Ctrl Pts',(24.7371999211453,89.4499401739752,2.68011334347994));
#21968=CARTESIAN_POINT('Ctrl Pts',(25.4220417006604,89.9176116335594,2.73277439856282));
#21969=CARTESIAN_POINT('Ctrl Pts',(26.1068834801755,90.3852830931436,2.78543545364569));
#21970=CARTESIAN_POINT('Ctrl Pts',(26.5384663894374,91.2238188075369,2.83809650872857));
#21971=CARTESIAN_POINT('Ctrl Pts',(26.5210598219411,92.052928105998,2.89075756381145));
#21972=CARTESIAN_POINT('Ctrl Pts',(26.5036532544449,92.8820374044591,2.94341861889433));
#21973=CARTESIAN_POINT('Ctrl Pts',(26.0372572101906,93.701720286988,2.99607967397721));
#21974=CARTESIAN_POINT('Ctrl Pts',(25.3333904465718,94.1402367801487,3.04874072906008));
#21975=CARTESIAN_POINT('Ctrl Pts',(24.6295236829529,94.5787532733095,3.10140178414296));
#21976=CARTESIAN_POINT('Ctrl Pts',(23.6881861999696,94.636103377102,3.15406283922584));
#21977=CARTESIAN_POINT('Ctrl Pts',(22.9362905172017,94.2862777415509,3.20672389430872));
#21978=CARTESIAN_POINT('Ctrl Pts',(22.1843948344338,93.9364521059997,3.2593849493916));
#21979=CARTESIAN_POINT('Ctrl Pts',(21.6219409518813,93.1794507311049,3.31204600447447));
#21980=CARTESIAN_POINT('Ctrl Pts',(21.5040113501232,92.3585867079682,3.36470705955735));
#21981=CARTESIAN_POINT('Ctrl Pts',(21.4870592998501,92.2405898015078,3.37227693887424));
#21982=CARTESIAN_POINT('Ctrl Pts',(21.4792925695015,92.1212732846669,3.37984681819113));
#21983=CARTESIAN_POINT('Ctrl Pts',(21.4802712114252,92.0018289507128,3.38741669750802));
#21984=CARTESIAN_POINT('Origin',(24.,92.,5.));
#21985=CARTESIAN_POINT('',(21.4864157451591,92.0003542166096,4.38741669750802));
#21986=CARTESIAN_POINT('',(21.4839748093506,91.9978936309448,4.11258330249198));
#21987=CARTESIAN_POINT('',(21.4825,92.,5.));
#21988=CARTESIAN_POINT('Ctrl Pts',(21.4839748093506,91.9978936309448,4.11258330249198));
#21989=CARTESIAN_POINT('Ctrl Pts',(21.4886914413751,92.5834107418754,4.07561558156933));
#21990=CARTESIAN_POINT('Ctrl Pts',(21.6925942792402,93.1718904338738,4.03864786064669));
#21991=CARTESIAN_POINT('Ctrl Pts',(22.0662148873617,93.6183374708837,4.00168013972404));
#21992=CARTESIAN_POINT('Ctrl Pts',(22.5984428671594,94.2543077557916,3.94901908464117));
#21993=CARTESIAN_POINT('Ctrl Pts',(23.4750692077561,94.6020594676884,3.89635802955829));
#21994=CARTESIAN_POINT('Ctrl Pts',(24.298528905607,94.5038812863977,3.84369697447541));
#21995=CARTESIAN_POINT('Ctrl Pts',(25.1219886034578,94.4057031051071,3.79103591939254));
#21996=CARTESIAN_POINT('Ctrl Pts',(25.8922816585629,93.8615950306291,3.73837486430965));
#21997=CARTESIAN_POINT('Ctrl Pts',(26.2600670194834,93.1183193280088,3.68571380922678));
#21998=CARTESIAN_POINT('Ctrl Pts',(26.6278523804038,92.3750436253885,3.6330527541439));
#21999=CARTESIAN_POINT('Ctrl Pts',(26.5931300471397,91.4326002946258,3.58039169906102));
#22000=CARTESIAN_POINT('Ctrl Pts',(26.1716472007571,90.7184035364296,3.52773064397814));
#22001=CARTESIAN_POINT('Ctrl Pts',(25.7501643543746,90.0042067782334,3.47506958889527));
#22002=CARTESIAN_POINT('Ctrl Pts',(24.9419209948735,89.5182565926036,3.42240853381239));
#22003=CARTESIAN_POINT('Ctrl Pts',(24.113469258178,89.4809395463902,3.36974747872951));
#22004=CARTESIAN_POINT('Ctrl Pts',(23.2850175214824,89.4436225001769,3.31708642364663));
#22005=CARTESIAN_POINT('Ctrl Pts',(22.4363574075923,89.85493859338,3.26442536856375));
#22006=CARTESIAN_POINT('Ctrl Pts',(21.9523708046376,90.5283492350653,3.21176431348087));
#22007=CARTESIAN_POINT('Ctrl Pts',(21.6485265278719,90.9511129399696,3.17870397648458));
#22008=CARTESIAN_POINT('Ctrl Pts',(21.4884096805934,91.4771750052055,3.14564363948828));
#22009=CARTESIAN_POINT('Ctrl Pts',(21.4854088326161,92.0015585716341,3.11258330249198));
#22010=CARTESIAN_POINT('Ctrl Pts',(21.4802712114252,92.0018289507128,3.38741669750802));
#22011=CARTESIAN_POINT('Ctrl Pts',(21.4861006458386,91.2903400047059,3.43250787327401));
#22012=CARTESIAN_POINT('Ctrl Pts',(21.8022313189484,90.5743158820022,3.47759904904));
#22013=CARTESIAN_POINT('Ctrl Pts',(22.335679104099,90.105645314345,3.52269022480599));
#22014=CARTESIAN_POINT('Ctrl Pts',(22.9586817807967,89.5582946152369,3.57535127988887));
#22015=CARTESIAN_POINT('Ctrl Pts',(23.8780924551558,89.3483198883991,3.62801233497174));
#22016=CARTESIAN_POINT('Ctrl Pts',(24.6769427066419,89.5709482675317,3.68067339005462));
#22017=CARTESIAN_POINT('Ctrl Pts',(25.475792958128,89.7935766466644,3.7333344451375));
#22018=CARTESIAN_POINT('Ctrl Pts',(26.154082786741,90.4488081317675,3.78599550022038));
#22019=CARTESIAN_POINT('Ctrl Pts',(26.4041961740691,91.2394840564229,3.83865655530326));
#22020=CARTESIAN_POINT('Ctrl Pts',(26.6543095613971,92.0301599810783,3.89131761038613));
#22021=CARTESIAN_POINT('Ctrl Pts',(26.4762465074402,92.9562803452861,3.94397866546901));
#22022=CARTESIAN_POINT('Ctrl Pts',(25.9507616486448,93.59783376143,3.99663972055189));
#22023=CARTESIAN_POINT('Ctrl Pts',(25.4252767898494,94.239387177574,4.04930077563477));
#22024=CARTESIAN_POINT('Ctrl Pts',(24.5523701262155,94.596373645654,4.10196183071765));
#22025=CARTESIAN_POINT('Ctrl Pts',(23.7279197254965,94.5068937086739,4.15462288580053));
#22026=CARTESIAN_POINT('Ctrl Pts',(22.9034693247774,94.4174137716938,4.2072839408834));
#22027=CARTESIAN_POINT('Ctrl Pts',(22.1274751869732,93.8814674296536,4.25994499596628));
#22028=CARTESIAN_POINT('Ctrl Pts',(21.7518638973824,93.1421154958358,4.31260605104916));
#22029=CARTESIAN_POINT('Ctrl Pts',(21.5739985954225,92.7920060646031,4.33754293320211));
#22030=CARTESIAN_POINT('Ctrl Pts',(21.4859135120177,92.3962857922303,4.36247981535507));
#22031=CARTESIAN_POINT('Ctrl Pts',(21.4864157451591,92.0003542166096,4.38741669750802));
#22032=CARTESIAN_POINT('Origin',(24.,92.,5.));
#22033=CARTESIAN_POINT('',(21.4815253774702,91.9978439079131,5.38741669750803));
#22034=CARTESIAN_POINT('',(21.4784999401586,92.000477759641,5.11258330249198));
#22035=CARTESIAN_POINT('',(21.4825,92.,5.));
#22036=CARTESIAN_POINT('Ctrl Pts',(21.4784999401586,92.000477759641,5.11258330249198));
#22037=CARTESIAN_POINT('Ctrl Pts',(21.4784306610618,92.0268374600631,5.11090963381615));
#22038=CARTESIAN_POINT('Ctrl Pts',(21.478808621275,92.0531951260584,5.10923596514032));
#22039=CARTESIAN_POINT('Ctrl Pts',(21.4796399750105,92.0795384836879,5.10756229646448));
#22040=CARTESIAN_POINT('Ctrl Pts',(21.5057980584424,92.9084175965176,5.05490124138161));
#22041=CARTESIAN_POINT('Ctrl Pts',(21.9808208362983,93.7231312660315,5.00224018629873));
#22042=CARTESIAN_POINT('Ctrl Pts',(22.6892773720314,94.1541929390351,4.94957913121586));
#22043=CARTESIAN_POINT('Ctrl Pts',(23.3977339077645,94.5852546120388,4.89691807613298));
#22044=CARTESIAN_POINT('Ctrl Pts',(24.3396242013747,94.6326642885323,4.8442570210501));
#22045=CARTESIAN_POINT('Ctrl Pts',(25.0877849303764,94.2749208713486,4.79159596596722));
#22046=CARTESIAN_POINT('Ctrl Pts',(25.8359456593782,93.9171774541649,4.73893491088434));
#22047=CARTESIAN_POINT('Ctrl Pts',(26.3903768237716,93.154280943304,4.68627385580146));
#22048=CARTESIAN_POINT('Ctrl Pts',(26.4996344284722,92.3322179256394,4.63361280071859));
#22049=CARTESIAN_POINT('Ctrl Pts',(26.6088920331728,91.5101549079748,4.58095174563571));
#22050=CARTESIAN_POINT('Ctrl Pts',(26.2729760781807,90.6289253835065,4.52829069055283));
#22051=CARTESIAN_POINT('Ctrl Pts',(25.6442301819934,90.0881819816232,4.47562963546995));
#22052=CARTESIAN_POINT('Ctrl Pts',(25.0154842858061,89.5474385797398,4.42296858038707));
#22053=CARTESIAN_POINT('Ctrl Pts',(24.0939084484235,89.3471813004415,4.37030752530419));
#22054=CARTESIAN_POINT('Ctrl Pts',(23.2974530394866,89.5782302356247,4.31764647022132));
#22055=CARTESIAN_POINT('Ctrl Pts',(22.5009976305496,89.8092791708079,4.26498541513844));
#22056=CARTESIAN_POINT('Ctrl Pts',(21.8296626500581,90.4716343204728,4.21232436005556));
#22057=CARTESIAN_POINT('Ctrl Pts',(21.5879099693117,91.2649063242647,4.15966330497268));
#22058=CARTESIAN_POINT('Ctrl Pts',(21.5158661107693,91.5013064992303,4.14396997081245));
#22059=CARTESIAN_POINT('Ctrl Pts',(21.481972530589,91.749333117907,4.12827663665221));
#22060=CARTESIAN_POINT('Ctrl Pts',(21.4839748093506,91.9978936309448,4.11258330249198));
#22061=CARTESIAN_POINT('Ctrl Pts',(21.4864157451591,92.0003542166096,4.38741669750802));
#22062=CARTESIAN_POINT('Ctrl Pts',(21.4869741148212,91.5601678531502,4.41514087043795));
#22063=CARTESIAN_POINT('Ctrl Pts',(21.5970300437705,91.1197203102036,4.44286504336787));
#22064=CARTESIAN_POINT('Ctrl Pts',(21.8149442483521,90.7413995457469,4.47058921629779));
#22065=CARTESIAN_POINT('Ctrl Pts',(22.2288643302899,90.0227930550715,4.52325027138067));
#22066=CARTESIAN_POINT('Ctrl Pts',(23.0319329355429,89.5283375993164,4.57591132646355));
#22067=CARTESIAN_POINT('Ctrl Pts',(23.8599447465539,89.4822771662391,4.62857238154643));
#22068=CARTESIAN_POINT('Ctrl Pts',(24.6879565575648,89.4362167331619,4.68123343662931));
#22069=CARTESIAN_POINT('Ctrl Pts',(25.5409115743339,89.8385513227625,4.73389449171218));
#22070=CARTESIAN_POINT('Ctrl Pts',(26.0319801400904,90.5068153323074,4.78655554679506));
#22071=CARTESIAN_POINT('Ctrl Pts',(26.523048705847,91.1750793418522,4.83921660187794));
#22072=CARTESIAN_POINT('Ctrl Pts',(26.652230820591,92.1092727713413,4.89187765696082));
#22073=CARTESIAN_POINT('Ctrl Pts',(26.3609401906912,92.8857229575282,4.9445387120437));
#22074=CARTESIAN_POINT('Ctrl Pts',(26.0696495607913,93.6621731437152,4.99719976712658));
#22075=CARTESIAN_POINT('Ctrl Pts',(25.3578861862475,94.2808800866,5.04986082220945));
#22076=CARTESIAN_POINT('Ctrl Pts',(24.5484469044027,94.461249628667,5.10252187729233));
#22077=CARTESIAN_POINT('Ctrl Pts',(23.7390076225579,94.641619170734,5.15518293237521));
#22078=CARTESIAN_POINT('Ctrl Pts',(22.8318924334121,94.3836513119832,5.20784398745809));
#22079=CARTESIAN_POINT('Ctrl Pts',(22.2384935561441,93.8043388788684,5.26050504254097));
#22080=CARTESIAN_POINT('Ctrl Pts',(21.7618020463168,93.3389633465204,5.30280892752999));
#22081=CARTESIAN_POINT('Ctrl Pts',(21.4875608688215,92.6662147404431,5.34511281251901));
#22082=CARTESIAN_POINT('Ctrl Pts',(21.4815253774702,91.9978439079131,5.38741669750803));
#22083=CARTESIAN_POINT('Origin',(24.,92.,5.));
#22084=CARTESIAN_POINT('',(21.4800390583838,92.0017354239359,6.38741669750802));
#22085=CARTESIAN_POINT('',(21.4852339904214,92.0016589574482,6.11258330249198));
#22086=CARTESIAN_POINT('',(21.4825,92.,5.));
#22087=CARTESIAN_POINT('Ctrl Pts',(21.4852339904214,92.0016589574482,6.11258330249198));
#22088=CARTESIAN_POINT('Ctrl Pts',(21.4833859739972,92.3036180412943,6.09354263098008));
#22089=CARTESIAN_POINT('Ctrl Pts',(21.5337383064256,92.6049815306727,6.07450195946819));
#22090=CARTESIAN_POINT('Ctrl Pts',(21.6390603134632,92.8857227683913,6.0554612879563));
#22091=CARTESIAN_POINT('Ctrl Pts',(21.930350881161,93.6621727887753,6.00280023287342));
#22092=CARTESIAN_POINT('Ctrl Pts',(22.6421141037151,94.2808795995417,5.95013917779054));
#22093=CARTESIAN_POINT('Ctrl Pts',(23.4515532127125,94.4612491030927,5.89747812270766));
#22094=CARTESIAN_POINT('Ctrl Pts',(24.26099232171,94.6416186066436,5.84481706762478));
#22095=CARTESIAN_POINT('Ctrl Pts',(25.1681073171508,94.3836508029792,5.7921560125419));
#22096=CARTESIAN_POINT('Ctrl Pts',(25.7615060677045,93.8043384935704,5.73949495745902));
#22097=CARTESIAN_POINT('Ctrl Pts',(26.3549048182583,93.2250261841617,5.68683390237615));
#22098=CARTESIAN_POINT('Ctrl Pts',(26.6345873239251,92.3243693690087,5.63417284729327));
#22099=CARTESIAN_POINT('Ctrl Pts',(26.4737127953066,91.5108312844465,5.58151179221039));
#22100=CARTESIAN_POINT('Ctrl Pts',(26.3128382666881,90.6972931998844,5.52885073712751));
#22101=CARTESIAN_POINT('Ctrl Pts',(25.7114067037843,89.9708738459131,5.47618968204463));
#22102=CARTESIAN_POINT('Ctrl Pts',(24.9421775844462,89.6610167966983,5.42352862696176));
#22103=CARTESIAN_POINT('Ctrl Pts',(24.1729484651081,89.3511597474835,5.37086757187888));
#22104=CARTESIAN_POINT('Ctrl Pts',(23.2359217893358,89.4578650030252,5.318206516796));
#22105=CARTESIAN_POINT('Ctrl Pts',(22.5560551459534,89.9327399088688,5.26554546171312));
#22106=CARTESIAN_POINT('Ctrl Pts',(21.8977959599792,90.3925223853337,5.21455807530607));
#22107=CARTESIAN_POINT('Ctrl Pts',(21.4806104893556,91.1974441303419,5.16357068889902));
#22108=CARTESIAN_POINT('Ctrl Pts',(21.4784999401586,92.000477759641,5.11258330249198));
#22109=CARTESIAN_POINT('Ctrl Pts',(21.4815253774702,91.9978439079131,5.38741669750803));
#22110=CARTESIAN_POINT('Ctrl Pts',(21.4800477209727,91.8342080999941,5.39777386760188));
#22111=CARTESIAN_POINT('Ctrl Pts',(21.4946464973945,91.6708346988264,5.40813103769574));
#22112=CARTESIAN_POINT('Ctrl Pts',(21.5262866764575,91.5108311799897,5.4184882077896));
#22113=CARTESIAN_POINT('Ctrl Pts',(21.6871612394291,90.6972929217049,5.47114926287248));
#22114=CARTESIAN_POINT('Ctrl Pts',(22.2885929307624,89.9708734126143,5.52381031795536));
#22115=CARTESIAN_POINT('Ctrl Pts',(23.0578222143614,89.6610162972326,5.57647137303823));
#22116=CARTESIAN_POINT('Ctrl Pts',(23.8270514979604,89.351159181851,5.62913242812111));
#22117=CARTESIAN_POINT('Ctrl Pts',(24.7640783738252,89.4578644601783,5.68179348320399));
#22118=CARTESIAN_POINT('Ctrl Pts',(25.443945162386,89.9327394674266,5.73445453828687));
#22119=CARTESIAN_POINT('Ctrl Pts',(26.1238119509469,90.407614474675,5.78711559336975));
#22120=CARTESIAN_POINT('Ctrl Pts',(26.5465186522039,91.2506592108443,5.83977664845262));
#22121=CARTESIAN_POINT('Ctrl Pts',(26.5203605631863,92.0795385006725,5.8924377035355));
#22122=CARTESIAN_POINT('Ctrl Pts',(26.4942024741688,92.9084177905007,5.94509875861838));
#22123=CARTESIAN_POINT('Ctrl Pts',(26.0191795948766,93.7231316339878,5.99775981370126));
#22124=CARTESIAN_POINT('Ctrl Pts',(25.3107229078599,94.1541933990405,6.05042086878414));
#22125=CARTESIAN_POINT('Ctrl Pts',(24.6022662208433,94.5852551640932,6.10308192386702));
#22126=CARTESIAN_POINT('Ctrl Pts',(23.6603757261022,94.6326648507116,6.1557429789499));
#22127=CARTESIAN_POINT('Ctrl Pts',(22.9122148373384,94.274921357135,6.20840403403277));
#22128=CARTESIAN_POINT('Ctrl Pts',(22.1640539485746,93.9171778635585,6.26106508911565));
#22129=CARTESIAN_POINT('Ctrl Pts',(21.6096226657882,93.154281189787,6.31372614419853));
#22130=CARTESIAN_POINT('Ctrl Pts',(21.5003650377567,92.3322179965802,6.36638719928141));
#22131=CARTESIAN_POINT('Ctrl Pts',(21.4858215065436,92.2227912963587,6.37339703202361));
#22132=CARTESIAN_POINT('Ctrl Pts',(21.4791659526657,92.1123162318432,6.38040686476582));
#22133=CARTESIAN_POINT('Ctrl Pts',(21.4800390583838,92.0017354239359,6.38741669750802));
#22134=CARTESIAN_POINT('Origin',(24.,92.,5.));
#22135=CARTESIAN_POINT('',(21.4863706869161,92.0004946014336,7.38741669750803));
#22136=CARTESIAN_POINT('',(21.4842076940747,91.9979483279393,7.11258330249198));
#22137=CARTESIAN_POINT('',(21.4825,92.,5.));
#22138=CARTESIAN_POINT('Ctrl Pts',(21.4842076940747,91.9979483279393,7.11258330249198));
#22139=CARTESIAN_POINT('Ctrl Pts',(21.4887014564203,92.5747302879618,7.07617562814402));
#22140=CARTESIAN_POINT('Ctrl Pts',(21.6859403589103,93.1542900307673,7.03976795379606));
#22141=CARTESIAN_POINT('Ctrl Pts',(22.0492387679223,93.5978334202261,7.0033602794481));
#22142=CARTESIAN_POINT('Ctrl Pts',(22.5747235145078,94.23938669937,6.95069922436522));
#22143=CARTESIAN_POINT('Ctrl Pts',(23.4476299917374,94.5963730912254,6.89803816928234));
#22144=CARTESIAN_POINT('Ctrl Pts',(24.2720802164026,94.5068931733543,6.84537711419947));
#22145=CARTESIAN_POINT('Ctrl Pts',(25.0965304410678,94.4174132554832,6.79271605911659));
#22146=CARTESIAN_POINT('Ctrl Pts',(25.8725244131687,93.8814670278857,6.74005500403371));
#22147=CARTESIAN_POINT('Ctrl Pts',(26.2481356225521,93.142115251948,6.68739394895083));
#22148=CARTESIAN_POINT('Ctrl Pts',(26.6237468319354,92.4027634760102,6.63473289386796));
#22149=CARTESIAN_POINT('Ctrl Pts',(26.5989752786013,91.4600061517323,6.58207183878508));
#22150=CARTESIAN_POINT('Ctrl Pts',(26.1850552850515,90.7413998145083,6.5294107837022));
#22151=CARTESIAN_POINT('Ctrl Pts',(25.7711352915018,90.0227934772843,6.47674972861932));
#22152=CARTESIAN_POINT('Ctrl Pts',(24.9680668577364,89.5283381271142,6.42408867353644));
#22153=CARTESIAN_POINT('Ctrl Pts',(24.1400552235389,89.4822777038725,6.37142761845356));
#22154=CARTESIAN_POINT('Ctrl Pts',(23.3120435893413,89.4362172806309,6.31876656337069));
#22155=CARTESIAN_POINT('Ctrl Pts',(22.4590887547118,89.8385517843175,6.26610550828781));
#22156=CARTESIAN_POINT('Ctrl Pts',(21.9680202938178,90.5068156511617,6.21344445320493));
#22157=CARTESIAN_POINT('Ctrl Pts',(21.6545075852538,90.9334551762256,6.17982406963395));
#22158=CARTESIAN_POINT('Ctrl Pts',(21.4884970592155,91.4684855231337,6.14620368606296));
#22159=CARTESIAN_POINT('Ctrl Pts',(21.4852339904214,92.0016589574482,6.11258330249198));
#22160=CARTESIAN_POINT('Ctrl Pts',(21.4800390583838,92.0017354239359,6.38741669750802));
#22161=CARTESIAN_POINT('Ctrl Pts',(21.4857251203391,91.2815828562451,6.4330679198487));
#22162=CARTESIAN_POINT('Ctrl Pts',(21.81071724972,90.5569454920104,6.47871914218937));
#22163=CARTESIAN_POINT('Ctrl Pts',(22.3557694668982,90.0881815733762,6.52437036453004));
#22164=CARTESIAN_POINT('Ctrl Pts',(22.9845154973476,89.5474380560209,6.57703141961292));
#22165=CARTESIAN_POINT('Ctrl Pts',(23.906091531523,89.3471807339522,6.6296924746958));
#22166=CARTESIAN_POINT('Ctrl Pts',(24.702547110535,89.578229718477,6.68235352977867));
#22167=CARTESIAN_POINT('Ctrl Pts',(25.4990026895469,89.8092787030018,6.73501458486155));
#22168=CARTESIAN_POINT('Ctrl Pts',(26.1703378133953,90.47163399412,6.78767563994444));
#22169=CARTESIAN_POINT('Ctrl Pts',(26.4120905457653,91.2649061673002,6.84033669502731));
#22170=CARTESIAN_POINT('Ctrl Pts',(26.6538432781353,92.0581783404805,6.89299775011019));
#22171=CARTESIAN_POINT('Ctrl Pts',(26.4660136190269,92.9823673957227,6.94565880519307));
#22172=CARTESIAN_POINT('Ctrl Pts',(25.933785525578,93.6183378164486,6.99831986027595));
#22173=CARTESIAN_POINT('Ctrl Pts',(25.4015574321291,94.2543082371746,7.05098091535882));
#22174=CARTESIAN_POINT('Ctrl Pts',(24.5249309043397,94.6020600233844,7.1036419704417));
#22175=CARTESIAN_POINT('Ctrl Pts',(23.7014710306461,94.5038818211034,7.15630302552458));
#22176=CARTESIAN_POINT('Ctrl Pts',(22.8780111569525,94.4057036188225,7.20896408060746));
#22177=CARTESIAN_POINT('Ctrl Pts',(22.1077179373546,93.8615954280509,7.26162513569034));
#22178=CARTESIAN_POINT('Ctrl Pts',(21.7399324979007,93.1183195667607,7.31428619077322));
#22179=CARTESIAN_POINT('Ctrl Pts',(21.5696843862451,92.7742567022501,7.33866302635149));
#22180=CARTESIAN_POINT('Ctrl Pts',(21.4856844315082,92.3875167881335,7.36303986192976));
#22181=CARTESIAN_POINT('Ctrl Pts',(21.4863706869161,92.0004946014336,7.38741669750803));
#22182=CARTESIAN_POINT('Origin',(24.,92.,5.));
#22183=CARTESIAN_POINT('',(21.481789046694,91.9978055657336,8.38741669750803));
#22184=CARTESIAN_POINT('',(21.4784369335473,92.0003195913806,8.11258330249198));
#22185=CARTESIAN_POINT('',(21.4825,92.,5.));
#22186=CARTESIAN_POINT('Ctrl Pts',(21.4784369335473,92.0003195913806,8.11258330249198));
#22187=CARTESIAN_POINT('Ctrl Pts',(21.4784053094568,92.0178575771478,8.11146968039083));
#22188=CARTESIAN_POINT('Ctrl Pts',(21.4785726200147,92.0353949438105,8.11035605828969));
#22189=CARTESIAN_POINT('Ctrl Pts',(21.4789407162088,92.0529280950311,8.10924243618854));
#22190=CARTESIAN_POINT('Ctrl Pts',(21.4963472798269,92.8820372167501,8.05658138110567));
#22191=CARTESIAN_POINT('Ctrl Pts',(21.9627432248614,93.7017199235893,8.00392032602278));
#22192=CARTESIAN_POINT('Ctrl Pts',(22.6666098382642,94.1402363229508,7.95125927093991));
#22193=CARTESIAN_POINT('Ctrl Pts',(23.3704764516669,94.5787527223123,7.89859821585703));
#22194=CARTESIAN_POINT('Ctrl Pts',(24.3118137334379,94.6361028141961,7.84593716077415));
#22195=CARTESIAN_POINT('Ctrl Pts',(25.0637092555993,94.2862772534286,7.79327610569127));
#22196=CARTESIAN_POINT('Ctrl Pts',(25.8156047777607,93.9364516926611,7.7406150506084));
#22197=CARTESIAN_POINT('Ctrl Pts',(26.3780585403126,93.1794504792422,7.68795399552551));
#22198=CARTESIAN_POINT('Ctrl Pts',(26.4959881169131,92.3585866313502,7.63529294044264));
#22199=CARTESIAN_POINT('Ctrl Pts',(26.6139176935135,91.5377227834583,7.58263188535976));
#22200=CARTESIAN_POINT('Ctrl Pts',(26.2873230841625,90.6529963010932,7.52997083027688));
#22201=CARTESIAN_POINT('Ctrl Pts',(25.6643205404874,90.1056457188879,7.477309775194));
#22202=CARTESIAN_POINT('Ctrl Pts',(25.0413179968122,89.5582951366826,7.42464872011113));
#22203=CARTESIAN_POINT('Ctrl Pts',(24.1219075188128,89.3483204546371,7.37198766502825));
#22204=CARTESIAN_POINT('Ctrl Pts',(23.3230574379199,89.5709487862187,7.31932660994537));
#22205=CARTESIAN_POINT('Ctrl Pts',(22.524207357027,89.7935771178002,7.26666555486249));
#22206=CARTESIAN_POINT('Ctrl Pts',(21.8459176732406,90.4488084630088,7.21400449977961));
#22207=CARTESIAN_POINT('Ctrl Pts',(21.595804339318,91.2394842188293,7.16134344469673));
#22208=CARTESIAN_POINT('Ctrl Pts',(21.5186090146758,91.4835194755669,7.14509006396181));
#22209=CARTESIAN_POINT('Ctrl Pts',(21.4822015557635,91.740457099368,7.1288366832269));
#22210=CARTESIAN_POINT('Ctrl Pts',(21.4842076940747,91.9979483279393,7.11258330249198));
#22211=CARTESIAN_POINT('Ctrl Pts',(21.4863706869161,92.0004946014336,7.38741669750803));
#22212=CARTESIAN_POINT('Ctrl Pts',(21.4871669427931,91.5514362957882,7.41570091701263));
#22213=CARTESIAN_POINT('Ctrl Pts',(21.6019741159521,91.1019979736551,7.44398513651724));
#22214=CARTESIAN_POINT('Ctrl Pts',(21.828352335515,90.7184032628621,7.47226935602185));
#22215=CARTESIAN_POINT('Ctrl Pts',(22.249835271893,90.0042063520624,7.52493041110472));
#22216=CARTESIAN_POINT('Ctrl Pts',(23.058078803959,89.5182560622716,7.57759146618761));
#22217=CARTESIAN_POINT('Ctrl Pts',(23.8865307175797,89.4809390082697,7.63025252127048));
#22218=CARTESIAN_POINT('Ctrl Pts',(24.7149826312004,89.4436219542678,7.68291357635336));
#22219=CARTESIAN_POINT('Ctrl Pts',(25.5636429263759,89.8549381360548,7.73557463143624));
#22220=CARTESIAN_POINT('Ctrl Pts',(26.0476296326406,90.5283489211969,7.78823568651912));
#22221=CARTESIAN_POINT('Ctrl Pts',(26.5316163389053,91.2017597063389,7.840896741602));
#22222=CARTESIAN_POINT('Ctrl Pts',(26.6509294562594,92.1372650948361,7.89355779668487));
#22223=CARTESIAN_POINT('Ctrl Pts',(26.3514585382347,92.910596864736,7.94621885176775));
#22224=CARTESIAN_POINT('Ctrl Pts',(26.05198762021,93.6839286346359,7.99887990685063));
#22225=CARTESIAN_POINT('Ctrl Pts',(25.3337326668066,94.2950867859385,8.05154096193351));
#22226=CARTESIAN_POINT('Ctrl Pts',(24.5224343764949,94.4669018166948,8.10420201701639));
#22227=CARTESIAN_POINT('Ctrl Pts',(23.7111360861833,94.6387168474512,8.15686307209927));
#22228=CARTESIAN_POINT('Ctrl Pts',(22.8067944589634,94.3711887576613,8.20952412718214));
#22229=CARTESIAN_POINT('Ctrl Pts',(22.2195442254209,93.7856437531992,8.26218518226502));
#22230=CARTESIAN_POINT('Ctrl Pts',(21.7540374326078,93.3214886766988,8.30392902067936));
#22231=CARTESIAN_POINT('Ctrl Pts',(21.4877768657504,92.6575058177296,8.34567285909369));
#22232=CARTESIAN_POINT('Ctrl Pts',(21.481789046694,91.9978055657336,8.38741669750803));
#22233=CARTESIAN_POINT('Origin',(24.,92.,5.));
#22234=CARTESIAN_POINT('',(21.4798237559162,92.0015869167785,9.38741669750802));
#22235=CARTESIAN_POINT('',(21.4850510509789,92.0017493960693,9.11258330249198));
#22236=CARTESIAN_POINT('',(21.4825,92.,5.));
#22237=CARTESIAN_POINT('',(25.9134659966651,93.6359872033749,10.));
#22238=CARTESIAN_POINT('Ctrl Pts',(21.4798237559162,92.0015869167785,9.38741669750802));
#22239=CARTESIAN_POINT('Ctrl Pts',(21.4853060534863,91.272907237615,9.43362796642338));
#22240=CARTESIAN_POINT('Ctrl Pts',(21.8192670107975,90.5399678433785,9.47983923533874));
#22241=CARTESIAN_POINT('Ctrl Pts',(22.3760117641787,90.0711228370539,9.5260505042541));
#22242=CARTESIAN_POINT('Ctrl Pts',(23.0104623389641,89.5368403279841,9.57871155933698));
#22243=CARTESIAN_POINT('Ctrl Pts',(23.9342252311204,89.3455170498785,9.63137261441985));
#22244=CARTESIAN_POINT('Ctrl Pts',(24.7281294273514,89.5853893188973,9.68403366950273));
#22245=CARTESIAN_POINT('Ctrl Pts',(25.5220336235825,89.8252615879161,9.73669472458561));
#22246=CARTESIAN_POINT('Ctrl Pts',(26.1860791238883,90.4963294040593,9.78935577966849));
#22247=CARTESIAN_POINT('Ctrl Pts',(26.4192657381557,91.2907292988926,9.84201683475137));
#22248=CARTESIAN_POINT('Ctrl Pts',(26.6524523524231,92.0851291937258,9.89467788983425));
#22249=CARTESIAN_POINT('Ctrl Pts',(26.4547800806522,93.0028611672492,9.94733894491712));
#22250=CARTESIAN_POINT('Ctrl Pts',(25.9134659966651,93.6359872033749,10.));
#22251=CARTESIAN_POINT('',(22.0828969142744,93.6385343069377,10.));
#22252=CARTESIAN_POINT('Origin',(24.,92.,10.));
#22253=CARTESIAN_POINT('Ctrl Pts',(22.082888458332,93.6385402287507,10.));
#22254=CARTESIAN_POINT('Ctrl Pts',(22.6060432359257,94.2476961579691,9.94901908464118));
#22255=CARTESIAN_POINT('Ctrl Pts',(23.4465813967719,94.5878273311312,9.89803816928235));
#22256=CARTESIAN_POINT('Ctrl Pts',(24.245735765903,94.5094848424925,9.84705725392352));
#22257=CARTESIAN_POINT('Ctrl Pts',(25.0712272651498,94.4285604793168,9.79439619884064));
#22258=CARTESIAN_POINT('Ctrl Pts',(25.8525623160909,93.9011252999797,9.74173514375777));
#22259=CARTESIAN_POINT('Ctrl Pts',(26.2358877550498,93.1658537096527,9.68907408867489));
#22260=CARTESIAN_POINT('Ctrl Pts',(26.6192131940086,92.4305821193258,9.63641303359201));
#22261=CARTESIAN_POINT('Ctrl Pts',(26.6045290209851,91.487474118009,9.58375197850913));
#22262=CARTESIAN_POINT('Ctrl Pts',(26.1982521612179,90.7645021442661,9.53109092342625));
#22263=CARTESIAN_POINT('Ctrl Pts',(25.7919753014507,90.0415301705232,9.47842986834338));
#22264=CARTESIAN_POINT('Ctrl Pts',(24.9941057549398,89.5386942243541,9.4257688132605));
#22265=CARTESIAN_POINT('Ctrl Pts',(24.1666097685101,89.4839132228271,9.37310775817762));
#22266=CARTESIAN_POINT('Ctrl Pts',(23.3391137820805,89.4291322213001,9.32044670309475));
#22267=CARTESIAN_POINT('Ctrl Pts',(22.4819913557322,89.8224061644151,9.26778564801186));
#22268=CARTESIAN_POINT('Ctrl Pts',(21.983903964328,90.4854401936108,9.21512459292898));
#22269=CARTESIAN_POINT('Ctrl Pts',(21.6606130378257,90.9157921545326,9.18094416278331));
#22270=CARTESIAN_POINT('Ctrl Pts',(21.4885781648623,91.4597899774222,9.14676373263764));
#22271=CARTESIAN_POINT('Ctrl Pts',(21.4850510509789,92.0017493960693,9.11258330249198));
#22272=CARTESIAN_POINT('Origin',(24.,92.,12.2084234471775));
#22273=CARTESIAN_POINT('',(20.9217235596202,92.0007881344673,1.79157655282254));
#22274=CARTESIAN_POINT('',(20.9313886636577,92.0003347861523,1.70842344717745));
#22275=CARTESIAN_POINT('',(20.9265,92.0000000000001,12.2084234471775));
#22276=CARTESIAN_POINT('',(24.7937992825328,89.0307770462543,0.999999999999999));
#22277=CARTESIAN_POINT('Ctrl Pts',(20.9313886636577,92.0003347861523,1.70842344717745));
#22278=CARTESIAN_POINT('Ctrl Pts',(20.9310462111061,92.494615243642,1.68292651844981));
#22279=CARTESIAN_POINT('Ctrl Pts',(21.2764428698256,94.0092287095088,1.6047685346393));
#22280=CARTESIAN_POINT('Ctrl Pts',(23.6460838412789,95.6088416124304,1.47394949574591));
#22281=CARTESIAN_POINT('Ctrl Pts',(26.8312245109703,94.2698537574842,1.31596633049727));
#22282=CARTESIAN_POINT('Ctrl Pts',(27.4433138069374,90.8667064664957,1.15798316524863));
#22283=CARTESIAN_POINT('Ctrl Pts',(25.7762533017603,89.2934286920663,1.05266105508288));
#22284=CARTESIAN_POINT('Ctrl Pts',(24.7937992825328,89.0307770462543,0.999999999999999));
#22285=CARTESIAN_POINT('',(23.2062007174671,89.0307770462543,0.999999999999999));
#22286=CARTESIAN_POINT('Origin',(24.,92.,0.999999999999999));
#22287=CARTESIAN_POINT('Ctrl Pts',(20.9217235596202,92.0007881344672,1.79157655282254));
#22288=CARTESIAN_POINT('Ctrl Pts',(20.921577466321,92.0437415214615,1.78934283757203));
#22289=CARTESIAN_POINT('Ctrl Pts',(20.9417780704225,93.09920230143,1.73444806723864));
#22290=CARTESIAN_POINT('Ctrl Pts',(22.1476051992024,95.1179528805984,1.62689224182237));
#22291=CARTESIAN_POINT('Ctrl Pts',(25.5990315417433,95.2555126520043,1.46890907657374));
#22292=CARTESIAN_POINT('Ctrl Pts',(27.5999506290771,92.4393708209745,1.3109259113251));
#22293=CARTESIAN_POINT('Ctrl Pts',(26.3493027558931,89.2605908411105,1.15462288580052));
#22294=CARTESIAN_POINT('Ctrl Pts',(24.1519058776304,88.7745943222177,1.05098091535882));
#22295=CARTESIAN_POINT('Ctrl Pts',(23.2042984301043,89.0256873776387,1.));
#22296=CARTESIAN_POINT('Origin',(24.,92.,12.2084234471775));
#22297=CARTESIAN_POINT('',(20.9300512599983,92.001902788448,2.79157655282254));
#22298=CARTESIAN_POINT('',(20.924991222385,91.997424467889,2.70842344717745));
#22299=CARTESIAN_POINT('',(20.9265,92.0000000000001,12.2084234471775));
#22300=CARTESIAN_POINT('Ctrl Pts',(20.924991222385,91.997424467889,2.70842344717745));
#22301=CARTESIAN_POINT('Ctrl Pts',(20.9323852777363,92.823989803404,2.66555951561375));
#22302=CARTESIAN_POINT('Ctrl Pts',(21.7006356086326,94.6781674340518,2.57003452896717));
#22303=CARTESIAN_POINT('Ctrl Pts',(24.8261379115922,95.5314383230663,2.42184848723771));
#22304=CARTESIAN_POINT('Ctrl Pts',(27.4089769044768,93.2380224116542,2.26386532198907));
#22305=CARTESIAN_POINT('Ctrl Pts',(26.8996889870333,89.8216055629486,2.10588215674044));
#22306=CARTESIAN_POINT('Ctrl Pts',(23.760424111462,88.3812146145649,1.94789899149181));
#22307=CARTESIAN_POINT('Ctrl Pts',(21.3097988736992,89.9256563753203,1.81541275497081));
#22308=CARTESIAN_POINT('Ctrl Pts',(20.9317535085566,91.473734231803,1.73558757353269));
#22309=CARTESIAN_POINT('Ctrl Pts',(20.9313886636577,92.0003347861523,1.70842344717745));
#22310=CARTESIAN_POINT('Ctrl Pts',(20.9300512599983,92.001902788448,2.79157655282254));
#22311=CARTESIAN_POINT('Ctrl Pts',(20.9278791968914,92.3814602359198,2.77197583473597));
#22312=CARTESIAN_POINT('Ctrl Pts',(21.1684423216004,93.77811538933,2.69971406156651));
#22313=CARTESIAN_POINT('Ctrl Pts',(23.2485917195109,95.548100055872,2.57479123331418));
#22314=CARTESIAN_POINT('Ctrl Pts',(26.5607983477153,94.5682620509693,2.41680806806554));
#22315=CARTESIAN_POINT('Ctrl Pts',(27.5502716608787,91.2589111130016,2.25882490281691));
#22316=CARTESIAN_POINT('Ctrl Pts',(25.3195310914441,88.6217767625239,2.10084173756827));
#22317=CARTESIAN_POINT('Ctrl Pts',(21.9403860022537,89.042720793944,1.94509228757015));
#22318=CARTESIAN_POINT('Ctrl Pts',(20.9250216955149,91.0310920004536,1.84200389265491));
#22319=CARTESIAN_POINT('Ctrl Pts',(20.9217235596202,92.0007881344672,1.79157655282254));
#22320=CARTESIAN_POINT('Origin',(24.,92.,12.2084234471775));
#22321=CARTESIAN_POINT('',(20.9283005269272,91.9974284308675,3.79157655282254));
#22322=CARTESIAN_POINT('',(20.9237789745046,92.0022328818336,3.70842344717745));
#22323=CARTESIAN_POINT('',(20.9265,92.0000000000001,12.2084234471775));
#22324=CARTESIAN_POINT('Ctrl Pts',(20.9237789745046,92.0022328818336,3.70842344717745));
#22325=CARTESIAN_POINT('Ctrl Pts',(20.9225841955761,92.1480569773283,3.70085356786056));
#22326=CARTESIAN_POINT('Ctrl Pts',(20.9980295686384,93.3070877047366,3.6406226334608));
#22327=CARTESIAN_POINT('Ctrl Pts',(22.47008521615,95.288313514808,3.52773064397815));
#22328=CARTESIAN_POINT('Ctrl Pts',(25.9177921721966,95.0782652002028,3.36974747872952));
#22329=CARTESIAN_POINT('Ctrl Pts',(27.625996631401,92.0761257688787,3.21176431348088));
#22330=CARTESIAN_POINT('Ctrl Pts',(26.0452974398026,89.0049366707406,3.05378114823225));
#22331=CARTESIAN_POINT('Ctrl Pts',(22.6094455863014,88.6503742748602,2.89579798298361));
#22332=CARTESIAN_POINT('Ctrl Pts',(21.0248750936135,90.6059034459642,2.78067874929868));
#22333=CARTESIAN_POINT('Ctrl Pts',(20.923301212371,91.808501931078,2.71822057069663));
#22334=CARTESIAN_POINT('Ctrl Pts',(20.924991222385,91.997424467889,2.70842344717745));
#22335=CARTESIAN_POINT('Ctrl Pts',(20.9283005269272,91.9974284308675,3.79157655282254));
#22336=CARTESIAN_POINT('Ctrl Pts',(20.9340588461039,92.7122593506074,3.7546088318999));
#22337=CARTESIAN_POINT('Ctrl Pts',(21.5376068210963,94.4541464677684,3.66498005589438));
#22338=CARTESIAN_POINT('Ctrl Pts',(24.4293689246723,95.601288842286,3.52269022480598));
#22339=CARTESIAN_POINT('Ctrl Pts',(27.2506150476498,93.6084592491481,3.36470705955735));
#22340=CARTESIAN_POINT('Ctrl Pts',(27.1234423470096,90.1567020569745,3.20672389430872));
#22341=CARTESIAN_POINT('Ctrl Pts',(24.1632008787755,88.3768793413442,3.04874072906008));
#22342=CARTESIAN_POINT('Ctrl Pts',(21.4405686580064,89.6964446537074,2.91035828189802));
#22343=CARTESIAN_POINT('Ctrl Pts',(20.9337148573203,91.361707002383,2.82463688981884));
#22344=CARTESIAN_POINT('Ctrl Pts',(20.9300512599983,92.001902788448,2.79157655282254));
#22345=CARTESIAN_POINT('Origin',(24.,92.,12.2084234471775));
#22346=CARTESIAN_POINT('',(20.921616510855,92.0005832747793,4.79157655282255));
#22347=CARTESIAN_POINT('',(20.931280553226,92.0004324467725,4.70842344717745));
#22348=CARTESIAN_POINT('',(20.9265,92.0000000000001,12.2084234471775));
#22349=CARTESIAN_POINT('Ctrl Pts',(20.931280553226,92.0004324467725,4.70842344717745));
#22350=CARTESIAN_POINT('Ctrl Pts',(20.9306673998754,92.4838071032452,4.6834865650245));
#22351=CARTESIAN_POINT('Ctrl Pts',(21.2653045337522,93.9871569627812,4.60588862778867));
#22352=CARTESIAN_POINT('Ctrl Pts',(23.608671679144,95.6056215728149,4.47562963546996));
#22353=CARTESIAN_POINT('Ctrl Pts',(26.8057465121274,94.2981364769134,4.31764647022132));
#22354=CARTESIAN_POINT('Ctrl Pts',(27.4579134988245,90.9061631628407,4.15966330497269));
#22355=CARTESIAN_POINT('Ctrl Pts',(24.973634903104,88.5063371813541,4.00168013972405));
#22356=CARTESIAN_POINT('Ctrl Pts',(21.7675876228179,89.2385332724819,3.85126685379231));
#22357=CARTESIAN_POINT('Ctrl Pts',(20.9308958629532,91.1336087406012,3.75351462294344));
#22358=CARTESIAN_POINT('Ctrl Pts',(20.9237789745046,92.0022328818336,3.70842344717745));
#22359=CARTESIAN_POINT('Ctrl Pts',(20.921616510855,92.0005832747793,4.79157655282255));
#22360=CARTESIAN_POINT('Ctrl Pts',(20.921531931191,92.0327646210543,4.78990288414672));
#22361=CARTESIAN_POINT('Ctrl Pts',(20.9365121376523,93.0774335164315,4.73556816038801));
#22362=CARTESIAN_POINT('Ctrl Pts',(22.1148104659795,95.0983381963849,4.62857238154642));
#22363=CARTESIAN_POINT('Ctrl Pts',(25.5645421252575,95.2719790790493,4.47058921629779));
#22364=CARTESIAN_POINT('Ctrl Pts',(27.5951806759185,92.4778232584365,4.31260605104916));
#22365=CARTESIAN_POINT('Ctrl Pts',(26.3648676419543,89.2502654310841,4.15462288580052));
#22366=CARTESIAN_POINT('Ctrl Pts',(22.9895389394378,88.5168107165773,3.99663972055189));
#22367=CARTESIAN_POINT('Ctrl Pts',(21.1060882305935,90.3750682368836,3.87562427622589));
#22368=CARTESIAN_POINT('Ctrl Pts',(20.9258560368481,91.693972328853,3.80726988698278));
#22369=CARTESIAN_POINT('Ctrl Pts',(20.9283005269272,91.9974284308675,3.79157655282254));
#22370=CARTESIAN_POINT('Origin',(24.,92.,12.2084234471775));
#22371=CARTESIAN_POINT('',(20.9298378032017,92.0020253448728,5.79157655282255));
#22372=CARTESIAN_POINT('',(20.9253101281647,91.9973677263042,5.70842344717746));
#22373=CARTESIAN_POINT('',(20.9265,92.0000000000001,12.2084234471775));
#22374=CARTESIAN_POINT('Ctrl Pts',(20.9253101281647,91.9973677263042,5.70842344717746));
#22375=CARTESIAN_POINT('Ctrl Pts',(20.9326785820548,92.8133509452838,5.66611956218844));
#22376=CARTESIAN_POINT('Ctrl Pts',(21.6842659096931,94.6570905748761,5.57115462211654));
#22377=CARTESIAN_POINT('Ctrl Pts',(24.7888216332756,95.5399724866421,5.42352862696176));
#22378=CARTESIAN_POINT('Ctrl Pts',(27.3956991685213,93.2739199079453,5.26554546171313));
#22379=CARTESIAN_POINT('Ctrl Pts',(26.9225616555133,89.8523784912207,5.1075622964645));
#22380=CARTESIAN_POINT('Ctrl Pts',(23.798560967482,88.3788030856943,4.94957913121586));
#22381=CARTESIAN_POINT('Ctrl Pts',(21.3215406064417,89.9039233849086,4.81653284812018));
#22382=CARTESIAN_POINT('Ctrl Pts',(20.9319622410737,91.4630291545808,4.73614762010738));
#22383=CARTESIAN_POINT('Ctrl Pts',(20.931280553226,92.0004324467725,4.70842344717745));
#22384=CARTESIAN_POINT('Ctrl Pts',(20.9298378032017,92.0020253448728,5.79157655282255));
#22385=CARTESIAN_POINT('Ctrl Pts',(20.9275816449178,92.3706733068195,5.77253588131066));
#22386=CARTESIAN_POINT('Ctrl Pts',(21.15907081827,93.7561579838992,5.70083415471589));
#22387=CARTESIAN_POINT('Ctrl Pts',(23.2111785351691,95.5399717307178,5.57647137303823));
#22388=CARTESIAN_POINT('Ctrl Pts',(26.5335435065542,94.5951486388852,5.4184882077896));
#22389=CARTESIAN_POINT('Ctrl Pts',(27.5578980422048,91.2964371536349,5.26050504254097));
#22390=CARTESIAN_POINT('Ctrl Pts',(25.3551176148943,88.6358811841043,5.10252187729233));
#22391=CARTESIAN_POINT('Ctrl Pts',(21.9595568927721,89.0225555274607,4.94621238071952));
#22392=CARTESIAN_POINT('Ctrl Pts',(20.9241931833304,91.0201964387709,4.8425639392296));
#22393=CARTESIAN_POINT('Ctrl Pts',(20.921616510855,92.0005832747793,4.79157655282255));
#22394=CARTESIAN_POINT('Origin',(24.,92.,12.2084234471775));
#22395=CARTESIAN_POINT('',(20.9285848451792,91.9974952079133,6.79157655282254));
#22396=CARTESIAN_POINT('',(20.9234955495304,92.0021186992919,6.70842344717746));
#22397=CARTESIAN_POINT('',(20.9265,92.0000000000001,12.2084234471775));
#22398=CARTESIAN_POINT('Ctrl Pts',(20.9234955495304,92.0021186992918,6.70842344717746));
#22399=CARTESIAN_POINT('Ctrl Pts',(20.9224296149028,92.1371217233644,6.70141361443525));
#22400=CARTESIAN_POINT('Ctrl Pts',(20.9915972274954,93.2852299955925,6.64174272661017));
#22401=CARTESIAN_POINT('Ctrl Pts',(22.4354575406508,95.2719797777492,6.5294107837022));
#22402=CARTESIAN_POINT('Ctrl Pts',(25.8851899365834,95.0983388580017,6.37142761845357));
#22403=CARTESIAN_POINT('Ctrl Pts',(27.624990714543,92.1143988405745,6.21344445320494));
#22404=CARTESIAN_POINT('Ctrl Pts',(26.0768011856691,89.0266951703267,6.0554612879563));
#22405=CARTESIAN_POINT('Ctrl Pts',(22.6448820957342,88.6358804657318,5.89747812270767));
#22406=CARTESIAN_POINT('Ctrl Pts',(21.031950056972,90.5840074378853,5.78179884244805));
#22407=CARTESIAN_POINT('Ctrl Pts',(20.9235061252868,91.7975922920882,5.71878061727132));
#22408=CARTESIAN_POINT('Ctrl Pts',(20.9253101281647,91.9973677263042,5.70842344717746));
#22409=CARTESIAN_POINT('Ctrl Pts',(20.9285848451792,91.9974952079133,6.79157655282254));
#22410=CARTESIAN_POINT('Ctrl Pts',(20.934071073012,92.7016617835356,6.75516887847459));
#22411=CARTESIAN_POINT('Ctrl Pts',(21.5231705466971,94.4326506257242,6.66610014904376));
#22412=CARTESIAN_POINT('Ctrl Pts',(24.3913282372869,95.6056208028792,6.52437036453004));
#22413=CARTESIAN_POINT('Ctrl Pts',(27.2334543225922,93.6426844805108,6.36638719928141));
#22414=CARTESIAN_POINT('Ctrl Pts',(27.1427269710462,90.1897772675991,6.20840403403277));
#22415=CARTESIAN_POINT('Ctrl Pts',(24.2014389895034,88.3788038589624,6.05042086878413));
#22416=CARTESIAN_POINT('Ctrl Pts',(21.453954137816,89.6747786389992,5.9114783750474));
#22417=CARTESIAN_POINT('Ctrl Pts',(20.9338215338625,91.3510984132479,5.82519693639353));
#22418=CARTESIAN_POINT('Ctrl Pts',(20.9298378032017,92.0020253448728,5.79157655282255));
#22419=CARTESIAN_POINT('Origin',(24.,92.,12.2084234471775));
#22420=CARTESIAN_POINT('',(20.9215395889802,92.0003901744224,7.79157655282255));
#22421=CARTESIAN_POINT('',(20.9312255436888,92.0006038361494,7.70842344717746));
#22422=CARTESIAN_POINT('',(20.9265,92.0000000000001,12.2084234471775));
#22423=CARTESIAN_POINT('Ctrl Pts',(20.9312255436888,92.0006038361494,7.70842344717745));
#22424=CARTESIAN_POINT('Ctrl Pts',(20.9303877260141,92.473101429326,7.68404661159919));
#22425=CARTESIAN_POINT('Ctrl Pts',(21.2544808710823,93.9652421749014,7.60700872093804));
#22426=CARTESIAN_POINT('Ctrl Pts',(23.5706309836456,95.601289611435,7.47730977519401));
#22427=CARTESIAN_POINT('Ctrl Pts',(26.7813300499739,94.327627111039,7.31932660994538));
#22428=CARTESIAN_POINT('Ctrl Pts',(27.4692678342079,90.9427273359204,7.16134344469674));
#22429=CARTESIAN_POINT('Ctrl Pts',(25.0104612763354,88.5168099727604,7.00336027944811));
#22430=CARTESIAN_POINT('Ctrl Pts',(21.7848977769712,89.2177208955611,6.85238694694168));
#22431=CARTESIAN_POINT('Ctrl Pts',(20.9304374011369,91.1229175406829,6.75407466951813));
#22432=CARTESIAN_POINT('Ctrl Pts',(20.9234955495304,92.0021186992918,6.70842344717746));
#22433=CARTESIAN_POINT('Ctrl Pts',(20.9215395889802,92.0003901744224,7.79157655282255));
#22434=CARTESIAN_POINT('Ctrl Pts',(20.9215009805821,92.0218014948814,7.7904629307214));
#22435=CARTESIAN_POINT('Ctrl Pts',(20.931364389904,93.0556766305594,7.73668825353738));
#22436=CARTESIAN_POINT('Ctrl Pts',(22.0822082378054,95.0782645420543,7.63025252127048));
#22437=CARTESIAN_POINT('Ctrl Pts',(25.5299144568995,95.2883128130433,7.47226935602185));
#22438=CARTESIAN_POINT('Ctrl Pts',(27.5899362712429,92.5157488852068,7.31428619077321));
#22439=CARTESIAN_POINT('Ctrl Pts',(26.3937632442238,89.2753832325168,7.15630302552458));
#22440=CARTESIAN_POINT('Ctrl Pts',(23.0263653048422,88.5063379273328,6.99831986027595));
#22441=CARTESIAN_POINT('Ctrl Pts',(21.1145962575175,90.3531167219238,6.87674436937527));
#22442=CARTESIAN_POINT('Ctrl Pts',(20.9261356431535,91.6831360059216,6.80782993355747));
#22443=CARTESIAN_POINT('Ctrl Pts',(20.9285848451792,91.9974952079133,6.79157655282254));
#22444=CARTESIAN_POINT('Origin',(24.,92.,12.2084234471775));
#22445=CARTESIAN_POINT('',(20.9296144608475,92.002135757227,8.79157655282255));
#22446=CARTESIAN_POINT('',(20.925632029797,91.9973209161002,8.70842344717745));
#22447=CARTESIAN_POINT('',(20.9265,92.0000000000001,12.2084234471775));
#22448=CARTESIAN_POINT('Ctrl Pts',(20.925632029797,91.9973209161002,8.70842344717745));
#22449=CARTESIAN_POINT('Ctrl Pts',(20.9329422827742,92.802718621963,8.66667960876312));
#22450=CARTESIAN_POINT('Ctrl Pts',(21.6680867896664,94.6359730058285,8.57227471526591));
#22451=CARTESIAN_POINT('Ctrl Pts',(24.7514084417654,95.5481008201034,8.42520876668582));
#22452=CARTESIAN_POINT('Ctrl Pts',(27.382061787488,93.3096961590962,8.26722560143718));
#22453=CARTESIAN_POINT('Ctrl Pts',(26.9450700899455,89.8833496110771,8.10924243618856));
#22454=CARTESIAN_POINT('Ctrl Pts',(23.8367990863051,88.3768785667208,7.95125927093992));
#22455=CARTESIAN_POINT('Ctrl Pts',(21.3333229638364,89.8820745861535,7.81765294126955));
#22456=CARTESIAN_POINT('Ctrl Pts',(20.9321976558787,91.4523691976585,7.73670766668206));
#22457=CARTESIAN_POINT('Ctrl Pts',(20.9312255436888,92.0006038361494,7.70842344717745));
#22458=CARTESIAN_POINT('Ctrl Pts',(20.9296144608475,92.0021357572271,8.79157655282255));
#22459=CARTESIAN_POINT('Ctrl Pts',(20.927286249777,92.3598775143589,8.77309592788534));
#22460=CARTESIAN_POINT('Ctrl Pts',(21.1498335279144,93.734213837484,8.70195424786525));
#22461=CARTESIAN_POINT('Ctrl Pts',(23.1738622820844,95.5314375280541,8.57815151276229));
#22462=CARTESIAN_POINT('Ctrl Pts',(26.5060022838615,94.621754023121,8.42016834751365));
#22463=CARTESIAN_POINT('Ctrl Pts',(27.5651291305171,91.3340327163824,8.26218518226502));
#22464=CARTESIAN_POINT('Ctrl Pts',(25.3905541137142,88.6503749960184,8.10420201701638));
#22465=CARTESIAN_POINT('Ctrl Pts',(21.9789222863521,89.0024380002803,7.9473324738689));
#22466=CARTESIAN_POINT('Ctrl Pts',(20.9233266977404,91.0093011817766,7.84312398580428));
#22467=CARTESIAN_POINT('Ctrl Pts',(20.9215395889802,92.0003901744224,7.79157655282255));
#22468=CARTESIAN_POINT('Origin',(24.,92.,12.2084234471775));
#22469=CARTESIAN_POINT('',(20.929711085108,91.9968960951898,9.79157655282254));
#22470=CARTESIAN_POINT('',(20.9232326966468,92.0019373937314,9.70842344717745));
#22471=CARTESIAN_POINT('',(20.9265,92.0000000000001,12.2084234471775));
#22472=CARTESIAN_POINT('',(23.2062007174671,89.0307770462543,10.));
#22473=CARTESIAN_POINT('Ctrl Pts',(23.2062007174671,89.0307770462543,10.));
#22474=CARTESIAN_POINT('Ctrl Pts',(22.2237466982397,89.2934286920664,9.94733894491712));
#22475=CARTESIAN_POINT('Ctrl Pts',(21.1240892170206,90.3312175686103,9.87786446252463));
#22476=CARTESIAN_POINT('Ctrl Pts',(20.9273642764696,91.6716348903192,9.80838998013215));
#22477=CARTESIAN_POINT('Ctrl Pts',(20.929711085108,91.9968960951898,9.79157655282254));
#22478=CARTESIAN_POINT('',(24.7956975117795,89.0256988737941,10.));
#22479=CARTESIAN_POINT('Origin',(24.,92.,10.));
#22480=CARTESIAN_POINT('Ctrl Pts',(24.7957019287906,89.0256870573369,10.));
#22481=CARTESIAN_POINT('Ctrl Pts',(23.8480950072444,88.7745945181247,9.94901908464118));
#22482=CARTESIAN_POINT('Ctrl Pts',(21.7874430689301,89.2303448029462,9.851826900367));
#22483=CARTESIAN_POINT('Ctrl Pts',(20.9299257816843,91.1123258767864,9.75463471609281));
#22484=CARTESIAN_POINT('Ctrl Pts',(20.9232326966468,92.0019373937314,9.70842344717745));
#22485=CARTESIAN_POINT('Origin',(24.,-92.,5.));
#22486=CARTESIAN_POINT('',(21.486504426694,-91.9997257424662,1.38741669750802));
#22487=CARTESIAN_POINT('',(21.4843725317804,-92.0035302714346,1.11258330249198));
#22488=CARTESIAN_POINT('',(21.4825,-92.,5.));
#22489=CARTESIAN_POINT('',(22.086534003335,-90.364012796625,0.999999999999999));
#22490=CARTESIAN_POINT('Ctrl Pts',(21.4843725317804,-92.0035302714346,1.11258330249198));
#22491=CARTESIAN_POINT('Ctrl Pts',(21.4895356694446,-91.4109125587033,1.07505553499465));
#22492=CARTESIAN_POINT('Ctrl Pts',(21.700778171916,-90.8151964396955,1.03752776749732));
#22493=CARTESIAN_POINT('Ctrl Pts',(22.086534003335,-90.364012796625,0.999999999999996));
#22494=CARTESIAN_POINT('',(21.4825,-92.,1.));
#22495=CARTESIAN_POINT('Origin',(24.,-92.,1.));
#22496=CARTESIAN_POINT('',(21.4825,-92.,0.));
#22497=CARTESIAN_POINT('',(21.4825,-92.,5.));
#22498=CARTESIAN_POINT('Origin',(24.,-92.,0.));
#22499=CARTESIAN_POINT('',(25.9171033775212,-90.3614656597817,0.999999999999999));
#22500=CARTESIAN_POINT('Origin',(24.,-92.,1.));
#22501=CARTESIAN_POINT('Ctrl Pts',(25.9171118396844,-90.3614597340102,0.999999999999999));
#22502=CARTESIAN_POINT('Ctrl Pts',(25.3939571501801,-89.7523042564146,1.05098091535882));
#22503=CARTESIAN_POINT('Ctrl Pts',(24.5534187715749,-89.4121721444715,1.10196183071765));
#22504=CARTESIAN_POINT('Ctrl Pts',(23.7542642221519,-89.4905144511518,1.15294274607647));
#22505=CARTESIAN_POINT('Ctrl Pts',(22.9287725366714,-89.5714386263726,1.20560380115935));
#22506=CARTESIAN_POINT('Ctrl Pts',(22.147437339474,-90.0988744252836,1.25826485624223));
#22507=CARTESIAN_POINT('Ctrl Pts',(21.7641118492188,-90.8341462554665,1.31092591132511));
#22508=CARTESIAN_POINT('Ctrl Pts',(21.578516959615,-91.1901431761531,1.33642284005274));
#22509=CARTESIAN_POINT('Ctrl Pts',(21.4862239279038,-91.5948612398581,1.36191976878038));
#22510=CARTESIAN_POINT('Ctrl Pts',(21.486504426694,-91.9997257424662,1.38741669750802));
#22511=CARTESIAN_POINT('Origin',(24.,-92.,5.));
#22512=CARTESIAN_POINT('',(21.4812642899864,-92.0021096151708,2.38741669750802));
#22513=CARTESIAN_POINT('',(21.4785878033439,-91.999354427872,2.11258330249198));
#22514=CARTESIAN_POINT('',(21.4825,-92.,5.));
#22515=CARTESIAN_POINT('Ctrl Pts',(21.4785878033439,-91.999354427872,2.11258330249198));
#22516=CARTESIAN_POINT('Ctrl Pts',(21.4784681386269,-91.9641713652006,2.11034958724146));
#22517=CARTESIAN_POINT('Ctrl Pts',(21.4791414214071,-91.928993039682,2.10811587199095));
#22518=CARTESIAN_POINT('Ctrl Pts',(21.480621972346,-91.8938487862731,2.10588215674044));
#22519=CARTESIAN_POINT('Ctrl Pts',(21.5155267680805,-91.0653038478858,2.05322110165756));
#22520=CARTESIAN_POINT('Ctrl Pts',(21.9991163215578,-90.2556964040098,2.00056004657468));
#22521=CARTESIAN_POINT('Ctrl Pts',(22.712087549401,-89.8321134766477,1.9478989914918));
#22522=CARTESIAN_POINT('Ctrl Pts',(23.4250587772441,-89.4085305492857,1.89523793640892));
#22523=CARTESIAN_POINT('Ctrl Pts',(24.3674116794533,-89.3709721384377,1.84257688132605));
#22524=CARTESIAN_POINT('Ctrl Pts',(25.1117465266451,-89.7366426720986,1.78991582624317));
#22525=CARTESIAN_POINT('Ctrl Pts',(25.8560813738369,-90.1023132057595,1.73725477116029));
#22526=CARTESIAN_POINT('Ctrl Pts',(26.4023981660114,-90.8712126839294,1.68459371607741));
#22527=CARTESIAN_POINT('Ctrl Pts',(26.502987230808,-91.6942827713944,1.63193266099453));
#22528=CARTESIAN_POINT('Ctrl Pts',(26.6035762956046,-92.5173528588593,1.57927160591166));
#22529=CARTESIAN_POINT('Ctrl Pts',(26.2584376330233,-93.3945935556194,1.52661055082878));
#22530=CARTESIAN_POINT('Ctrl Pts',(25.6239875152205,-93.9288761516103,1.4739494957459));
#22531=CARTESIAN_POINT('Ctrl Pts',(24.9895373974178,-94.4631587476011,1.42128844066302));
#22532=CARTESIAN_POINT('Ctrl Pts',(24.0657758243935,-94.6544832428229,1.36862738558014));
#22533=CARTESIAN_POINT('Ctrl Pts',(23.2718709044643,-94.4146102691233,1.31596633049727));
#22534=CARTESIAN_POINT('Ctrl Pts',(22.4779659845352,-94.1747372954238,1.26330527541439));
#22535=CARTESIAN_POINT('Ctrl Pts',(21.8139177177011,-93.503666852803,1.21064422033151));
#22536=CARTESIAN_POINT('Ctrl Pts',(21.5807312014042,-92.7092672371347,1.15798316524863));
#22537=CARTESIAN_POINT('Ctrl Pts',(21.5137200371456,-92.480979409957,1.14284987766308));
#22538=CARTESIAN_POINT('Ctrl Pts',(21.4822904668902,-92.2425067646591,1.12771659007753));
#22539=CARTESIAN_POINT('Ctrl Pts',(21.4843725317804,-92.0035302714346,1.11258330249198));
#22540=CARTESIAN_POINT('Ctrl Pts',(21.486504426694,-91.9997257424662,1.38741669750802));
#22541=CARTESIAN_POINT('Ctrl Pts',(21.4868032667881,-92.4310635958632,1.41458082386326));
#22542=CARTESIAN_POINT('Ctrl Pts',(21.5921778743622,-92.8625676650245,1.4417449502185));
#22543=CARTESIAN_POINT('Ctrl Pts',(21.8017475042685,-93.2354979719165,1.46890907657374));
#22544=CARTESIAN_POINT('Ctrl Pts',(22.2080244328865,-93.958469996729,1.52157013165662));
#22545=CARTESIAN_POINT('Ctrl Pts',(23.0058940734354,-94.4613061848995,1.57423118673949));
#22546=CARTESIAN_POINT('Ctrl Pts',(23.8333901892196,-94.5160872321709,1.62689224182237));
#22547=CARTESIAN_POINT('Ctrl Pts',(24.6608863050039,-94.5708682794422,1.67955329690525));
#22548=CARTESIAN_POINT('Ctrl Pts',(25.5180088960235,-94.1775941858145,1.73221435198813));
#22549=CARTESIAN_POINT('Ctrl Pts',(26.0160963730402,-93.5145600286215,1.78487540707101));
#22550=CARTESIAN_POINT('Ctrl Pts',(26.5141838500568,-92.8515258714286,1.83753646215389));
#22551=CARTESIAN_POINT('Ctrl Pts',(26.6532362130706,-91.9187316506704,1.89019751723677));
#22552=CARTESIAN_POINT('Ctrl Pts',(26.3701623803631,-91.1392455433219,1.94285857231964));
#22553=CARTESIAN_POINT('Ctrl Pts',(26.0870885476557,-90.3597594359734,1.99551962740252));
#22554=CARTESIAN_POINT('Ctrl Pts',(25.3818885192271,-89.7335814420344,2.0481806824854));
#22555=CARTESIAN_POINT('Ctrl Pts',(24.5743964779126,-89.5446792416752,2.10084173756828));
#22556=CARTESIAN_POINT('Ctrl Pts',(23.7669044365982,-89.3557770413159,2.15350279265115));
#22557=CARTESIAN_POINT('Ctrl Pts',(22.857120382398,-89.6041506345363,2.20616384773403));
#22558=CARTESIAN_POINT('Ctrl Pts',(22.2576400878061,-90.1771655681069,2.25882490281691));
#22559=CARTESIAN_POINT('Ctrl Pts',(21.7696877997114,-90.6435761415163,2.30168883438061));
#22560=CARTESIAN_POINT('Ctrl Pts',(21.4873207515092,-91.3250710178653,2.34455276594432));
#22561=CARTESIAN_POINT('Ctrl Pts',(21.4812642899864,-92.0021096151708,2.38741669750802));
#22562=CARTESIAN_POINT('Origin',(24.,-92.,5.));
#22563=CARTESIAN_POINT('',(21.4802713394158,-91.9981710493934,3.38741669750802));
#22564=CARTESIAN_POINT('',(21.4854090148867,-91.9984414282173,3.11258330249198));
#22565=CARTESIAN_POINT('',(21.4825,-92.,5.));
#22566=CARTESIAN_POINT('Ctrl Pts',(21.4854090148867,-91.9984414282173,3.11258330249198));
#22567=CARTESIAN_POINT('Ctrl Pts',(21.4836298808409,-91.6875464209233,3.0929825844054));
#22568=CARTESIAN_POINT('Ctrl Pts',(21.5370775357559,-91.3772414115068,3.07338186631883));
#22569=CARTESIAN_POINT('Ctrl Pts',(21.6485421342809,-91.0894033947304,3.05378114823225));
#22570=CARTESIAN_POINT('Ctrl Pts',(21.9480129667671,-90.3160718469037,3.00112009314937));
#22571=CARTESIAN_POINT('Ctrl Pts',(22.666267715158,-89.704913874088,2.94845903806649));
#22572=CARTESIAN_POINT('Ctrl Pts',(23.4775657731397,-89.5330988908351,2.89579798298361));
#22573=CARTESIAN_POINT('Ctrl Pts',(24.2888638311213,-89.3612839075822,2.84313692790073));
#22574=CARTESIAN_POINT('Ctrl Pts',(25.1932051986936,-89.6288119138921,2.79047587281785));
#22575=CARTESIAN_POINT('Ctrl Pts',(25.780455264855,-90.2143567539364,2.73781481773498));
#22576=CARTESIAN_POINT('Ctrl Pts',(26.3677053310164,-90.7999015939806,2.6851537626521));
#22577=CARTESIAN_POINT('Ctrl Pts',(26.6378640957668,-91.7034632677594,2.63249270756922));
#22578=CARTESIAN_POINT('Ctrl Pts',(26.4684106985951,-92.5152563159492,2.57983165248634));
#22579=CARTESIAN_POINT('Ctrl Pts',(26.2989573014234,-93.3270493641389,2.52717059740346));
#22580=CARTESIAN_POINT('Ctrl Pts',(25.6898917423295,-94.0470737867398,2.47450954232059));
#22581=CARTESIAN_POINT('Ctrl Pts',(24.9174341156813,-94.3487960615597,2.42184848723771));
#22582=CARTESIAN_POINT('Ctrl Pts',(24.1449764890331,-94.6505183363795,2.36918743215483));
#22583=CARTESIAN_POINT('Ctrl Pts',(23.2091267948305,-94.5339384634185,2.31652637707195));
#22584=CARTESIAN_POINT('Ctrl Pts',(22.5343119667251,-94.0519073104887,2.26386532198907));
#22585=CARTESIAN_POINT('Ctrl Pts',(21.8881206474051,-93.5903223931276,2.21343798215671));
#22586=CARTESIAN_POINT('Ctrl Pts',(21.4812892995851,-92.7936312531158,2.16301064232434));
#22587=CARTESIAN_POINT('Ctrl Pts',(21.4785878033439,-91.999354427872,2.11258330249198));
#22588=CARTESIAN_POINT('Ctrl Pts',(21.4812642899864,-92.0021096151708,2.38741669750802));
#22589=CARTESIAN_POINT('Ctrl Pts',(21.4798800048902,-92.1568558207351,2.39721382102719));
#22590=CARTESIAN_POINT('Ctrl Pts',(21.4929305169812,-92.3113692249255,2.40701094454637));
#22591=CARTESIAN_POINT('Ctrl Pts',(21.5212603168746,-92.4630284201484,2.41680806806555));
#22592=CARTESIAN_POINT('Ctrl Pts',(21.6735373755183,-93.2782200646987,2.46946912314842));
#22593=CARTESIAN_POINT('Ctrl Pts',(22.2672680277891,-94.0109470798785,2.5221301782313));
#22594=CARTESIAN_POINT('Ctrl Pts',(23.0331836548293,-94.3289069878288,2.57479123331418));
#22595=CARTESIAN_POINT('Ctrl Pts',(23.7990992818695,-94.6468668957792,2.62745228839706));
#22596=CARTESIAN_POINT('Ctrl Pts',(24.7371998836791,-94.5500596964999,2.68011334347994));
#22597=CARTESIAN_POINT('Ctrl Pts',(25.4220416283354,-94.0823882608119,2.73277439856281));
#22598=CARTESIAN_POINT('Ctrl Pts',(26.1068833729918,-93.6147168251238,2.78543545364569));
#22599=CARTESIAN_POINT('Ctrl Pts',(26.538466260495,-92.776181153027,2.83809650872857));
#22600=CARTESIAN_POINT('Ctrl Pts',(26.5210596939212,-91.9470718966112,2.89075756381145));
#22601=CARTESIAN_POINT('Ctrl Pts',(26.5036531273474,-91.1179626401953,2.94341861889433));
#22602=CARTESIAN_POINT('Ctrl Pts',(26.0372571066966,-90.2982797994603,2.9960796739772));
#22603=CARTESIAN_POINT('Ctrl Pts',(25.3333903788126,-89.8597633286133,3.04874072906008));
#22604=CARTESIAN_POINT('Ctrl Pts',(24.6295236509285,-89.4212468577661,3.10140178414296));
#22605=CARTESIAN_POINT('Ctrl Pts',(23.6881862158112,-89.3638967568069,3.15406283922584));
#22606=CARTESIAN_POINT('Ctrl Pts',(22.9362905712497,-89.7137223745679,3.20672389430872));
#22607=CARTESIAN_POINT('Ctrl Pts',(22.1843949266883,-90.063547992329,3.2593849493916));
#22608=CARTESIAN_POINT('Ctrl Pts',(21.6219410726826,-90.8205493288104,3.31204600447447));
#22609=CARTESIAN_POINT('Ctrl Pts',(21.5040114769092,-91.6414133102583,3.36470705955735));
#22610=CARTESIAN_POINT('Ctrl Pts',(21.4870594274965,-91.759410210726,3.37227693887424));
#22611=CARTESIAN_POINT('Ctrl Pts',(21.4792926975419,-91.8787267215066,3.37984681819113));
#22612=CARTESIAN_POINT('Ctrl Pts',(21.4802713394158,-91.9981710493934,3.38741669750802));
#22613=CARTESIAN_POINT('Origin',(24.,-92.,5.));
#22614=CARTESIAN_POINT('',(21.4864158728456,-91.9996457834086,4.38741669750802));
#22615=CARTESIAN_POINT('',(21.4839749917546,-92.0021063689016,4.11258330249198));
#22616=CARTESIAN_POINT('',(21.4825,-92.,5.));
#22617=CARTESIAN_POINT('Ctrl Pts',(21.4839749917546,-92.0021063689016,4.11258330249198));
#22618=CARTESIAN_POINT('Ctrl Pts',(21.4886916234371,-91.4165893004159,4.07561558156934));
#22619=CARTESIAN_POINT('Ctrl Pts',(21.6925944465197,-90.8281096510767,4.0386478606467));
#22620=CARTESIAN_POINT('Ctrl Pts',(22.066215027555,-90.3816626464359,4.00168013972405));
#22621=CARTESIAN_POINT('Ctrl Pts',(22.598442968768,-89.7456924076384,3.94901908464118));
#22622=CARTESIAN_POINT('Ctrl Pts',(23.4750692458127,-89.3979407209711,3.8963580295583));
#22623=CARTESIAN_POINT('Ctrl Pts',(24.2985288839648,-89.4961188951354,3.84369697447542));
#22624=CARTESIAN_POINT('Ctrl Pts',(25.1219885221169,-89.5942970692997,3.79103591939254));
#22625=CARTESIAN_POINT('Ctrl Pts',(25.8922815213764,-90.1384051042956,3.73837486430966));
#22626=CARTESIAN_POINT('Ctrl Pts',(26.2600668556347,-90.8816807530475,3.68571380922678));
#22627=CARTESIAN_POINT('Ctrl Pts',(26.627852189893,-91.6249564017994,3.6330527541439));
#22628=CARTESIAN_POINT('Ctrl Pts',(26.5931298591502,-92.5673996643073,3.58039169906103));
#22629=CARTESIAN_POINT('Ctrl Pts',(26.1716470433212,-93.2815963706942,3.52773064397815));
#22630=CARTESIAN_POINT('Ctrl Pts',(25.7501642274921,-93.9957930770812,3.47506958889527));
#22631=CARTESIAN_POINT('Ctrl Pts',(24.9419209265769,-94.4817432273472,3.42240853381239));
#22632=CARTESIAN_POINT('Ctrl Pts',(24.1134692499477,-94.5190602709168,3.36974747872951));
#22633=CARTESIAN_POINT('Ctrl Pts',(23.2850175733184,-94.5563773144863,3.31708642364664));
#22634=CARTESIAN_POINT('Ctrl Pts',(22.4363575209751,-94.1450612513594,3.26442536856376));
#22635=CARTESIAN_POINT('Ctrl Pts',(21.9523709530942,-93.4716506583771,3.21176431348088));
#22636=CARTESIAN_POINT('Ctrl Pts',(21.6485266983476,-93.0488869840482,3.17870397648458));
#22637=CARTESIAN_POINT('Ctrl Pts',(21.4884098626544,-92.5228249567292,3.14564363948828));
#22638=CARTESIAN_POINT('Ctrl Pts',(21.4854090148867,-91.9984414282173,3.11258330249198));
#22639=CARTESIAN_POINT('Ctrl Pts',(21.4802713394158,-91.9981710493934,3.38741669750802));
#22640=CARTESIAN_POINT('Ctrl Pts',(21.4861007735321,-92.7096599592594,3.43250787327401));
#22641=CARTESIAN_POINT('Ctrl Pts',(21.802231430593,-93.4256840455739,3.47759904904));
#22642=CARTESIAN_POINT('Ctrl Pts',(22.3356791886479,-93.8943545894189,3.52269022480599));
#22643=CARTESIAN_POINT('Ctrl Pts',(22.958681833701,-94.4417052607172,3.57535127988886));
#22644=CARTESIAN_POINT('Ctrl Pts',(23.8780924613484,-94.6516799768993,3.62801233497174));
#22645=CARTESIAN_POINT('Ctrl Pts',(24.6769426722523,-94.4290516090785,3.68067339005462));
#22646=CARTESIAN_POINT('Ctrl Pts',(25.4757928831562,-94.2064232412577,3.7333344451375));
#22647=CARTESIAN_POINT('Ctrl Pts',(26.1540826773166,-93.5511917894339,3.78599550022038));
#22648=CARTESIAN_POINT('Ctrl Pts',(26.4041960519401,-92.7605159049424,3.83865655530326));
#22649=CARTESIAN_POINT('Ctrl Pts',(26.6543094265636,-91.9698400204509,3.89131761038614));
#22650=CARTESIAN_POINT('Ctrl Pts',(26.4762463816501,-91.0437197032917,3.94397866546901));
#22651=CARTESIAN_POINT('Ctrl Pts',(25.9507615495482,-90.4021663197385,3.99663972055189));
#22652=CARTESIAN_POINT('Ctrl Pts',(25.4252767174463,-89.7606129361853,4.04930077563477));
#22653=CARTESIAN_POINT('Ctrl Pts',(24.5523700981559,-89.4036264862382,4.10196183071765));
#22654=CARTESIAN_POINT('Ctrl Pts',(23.727919739318,-89.4931064186725,4.15462288580053));
#22655=CARTESIAN_POINT('Ctrl Pts',(22.9034693804802,-89.5825863511067,4.2072839408834));
#22656=CARTESIAN_POINT('Ctrl Pts',(22.1274752820949,-90.1185326659223,4.25994499596628));
#22657=CARTESIAN_POINT('Ctrl Pts',(21.7518640115845,-90.8578845621824,4.31260605104916));
#22658=CARTESIAN_POINT('Ctrl Pts',(21.5739987186599,-91.20799397563,4.33754293320211));
#22659=CARTESIAN_POINT('Ctrl Pts',(21.4859136397297,-91.6037142279008,4.36247981535507));
#22660=CARTESIAN_POINT('Ctrl Pts',(21.4864158728456,-91.9996457834086,4.38741669750802));
#22661=CARTESIAN_POINT('Origin',(24.,-92.,5.));
#22662=CARTESIAN_POINT('',(21.4815255054053,-92.0021560919774,5.38741669750802));
#22663=CARTESIAN_POINT('',(21.4785001229596,-91.9995222403937,5.11258330249198));
#22664=CARTESIAN_POINT('',(21.4825,-92.,5.));
#22665=CARTESIAN_POINT('Ctrl Pts',(21.4785001229596,-91.9995222403937,5.11258330249198));
#22666=CARTESIAN_POINT('Ctrl Pts',(21.4784308438678,-91.9731625418826,5.11090963381615));
#22667=CARTESIAN_POINT('Ctrl Pts',(21.4788088040536,-91.9468048777982,5.10923596514032));
#22668=CARTESIAN_POINT('Ctrl Pts',(21.4796401577289,-91.9204615220785,5.10756229646449));
#22669=CARTESIAN_POINT('Ctrl Pts',(21.5057982392643,-91.0915824693399,5.05490124138162));
#22670=CARTESIAN_POINT('Ctrl Pts',(21.9808209826826,-90.2768688588901,5.00224018629874));
#22671=CARTESIAN_POINT('Ctrl Pts',(22.6892774670547,-89.8458072171371,4.94957913121586));
#22672=CARTESIAN_POINT('Ctrl Pts',(23.3977339514269,-89.4147455753841,4.89691807613298));
#22673=CARTESIAN_POINT('Ctrl Pts',(24.3396241767529,-89.367335902328,4.8442570210501));
#22674=CARTESIAN_POINT('Ctrl Pts',(25.0877848515153,-89.7250792935763,4.79159596596723));
#22675=CARTESIAN_POINT('Ctrl Pts',(25.8359455262777,-90.0828226848246,4.73893491088435));
#22676=CARTESIAN_POINT('Ctrl Pts',(26.3903766504766,-90.8457191403772,4.68627385580147));
#22677=CARTESIAN_POINT('Ctrl Pts',(26.4996342472564,-91.6677820984451,4.63361280071859));
#22678=CARTESIAN_POINT('Ctrl Pts',(26.6088918440362,-92.4898450565129,4.58095174563571));
#22679=CARTESIAN_POINT('Ctrl Pts',(26.2729759133969,-93.371074517096,4.52829069055283));
#22680=CARTESIAN_POINT('Ctrl Pts',(25.6442300627918,-93.9118178797764,4.47562963546995));
#22681=CARTESIAN_POINT('Ctrl Pts',(25.0154842121866,-94.4525612424569,4.42296858038708));
#22682=CARTESIAN_POINT('Ctrl Pts',(24.0939084416155,-94.6528185072348,4.3703075253042));
#22683=CARTESIAN_POINT('Ctrl Pts',(23.2974530904191,-94.4217695888032,4.31764647022132));
#22684=CARTESIAN_POINT('Ctrl Pts',(22.5009977392227,-94.1907206703715,4.26498541513844));
#22685=CARTESIAN_POINT('Ctrl Pts',(21.8296628074011,-93.5283655687303,4.21232436005556));
#22686=CARTESIAN_POINT('Ctrl Pts',(21.5879101441809,-92.7350936224457,4.15966330497269));
#22687=CARTESIAN_POINT('Ctrl Pts',(21.5158662908614,-92.4986934646177,4.14396997081245));
#22688=CARTESIAN_POINT('Ctrl Pts',(21.4819727131382,-92.2506668639209,4.12827663665222));
#22689=CARTESIAN_POINT('Ctrl Pts',(21.4839749917546,-92.0021063689016,4.11258330249198));
#22690=CARTESIAN_POINT('Ctrl Pts',(21.4864158728456,-91.9996457834086,4.38741669750802));
#22691=CARTESIAN_POINT('Ctrl Pts',(21.4869742424795,-92.4398321245071,4.41514087043795));
#22692=CARTESIAN_POINT('Ctrl Pts',(21.5970301658382,-92.8802796450794,4.44286504336787));
#22693=CARTESIAN_POINT('Ctrl Pts',(21.8149443593501,-93.2586003903179,4.47058921629779));
#22694=CARTESIAN_POINT('Ctrl Pts',(22.2288644202614,-93.9772068444889,4.52325027138067));
#22695=CARTESIAN_POINT('Ctrl Pts',(23.0319329847194,-94.4716622751266,4.57591132646355));
#22696=CARTESIAN_POINT('Ctrl Pts',(23.8599447536685,-94.517722705864,4.62857238154643));
#22697=CARTESIAN_POINT('Ctrl Pts',(24.6879565226175,-94.5637831366015,4.68123343662931));
#22698=CARTESIAN_POINT('Ctrl Pts',(25.5409114960577,-94.1614485674387,4.73389449171218));
#22699=CARTESIAN_POINT('Ctrl Pts',(26.0319800368686,-93.4931845918408,4.78655554679506));
#22700=CARTESIAN_POINT('Ctrl Pts',(26.5230485776795,-92.8249206162428,4.83921660187794));
#22701=CARTESIAN_POINT('Ctrl Pts',(26.6522306858613,-91.8907272342096,4.89187765696082));
#22702=CARTESIAN_POINT('Ctrl Pts',(26.3609400707586,-91.1142770874653,4.9445387120437));
#22703=CARTESIAN_POINT('Ctrl Pts',(26.0696494556558,-90.337826940721,4.99719976712657));
#22704=CARTESIAN_POINT('Ctrl Pts',(25.3578861172687,-89.7191200292656,5.04986082220945));
#22705=CARTESIAN_POINT('Ctrl Pts',(24.5484468765423,-89.5387504963611,5.10252187729233));
#22706=CARTESIAN_POINT('Ctrl Pts',(23.7390076358159,-89.3583809634566,5.15518293237521));
#22707=CARTESIAN_POINT('Ctrl Pts',(22.8318924927503,-89.616348809103,5.20784398745809));
#22708=CARTESIAN_POINT('Ctrl Pts',(22.2384936456262,-90.1956612127896,5.26050504254097));
#22709=CARTESIAN_POINT('Ctrl Pts',(21.7618021600142,-90.6610367214971,5.30280892752998));
#22710=CARTESIAN_POINT('Ctrl Pts',(21.48756099645,-91.3337852933997,5.345112812519));
#22711=CARTESIAN_POINT('Ctrl Pts',(21.4815255054053,-92.0021560919774,5.38741669750802));
#22712=CARTESIAN_POINT('Origin',(24.,-92.,5.));
#22713=CARTESIAN_POINT('',(21.4800391863945,-91.998264576152,6.38741669750802));
#22714=CARTESIAN_POINT('',(21.4852341727342,-91.998341042672,6.11258330249198));
#22715=CARTESIAN_POINT('',(21.4825,-92.,5.));
#22716=CARTESIAN_POINT('Ctrl Pts',(21.4852341727342,-91.998341042672,6.11258330249198));
#22717=CARTESIAN_POINT('Ctrl Pts',(21.483386156444,-91.696381980717,6.09354263098009));
#22718=CARTESIAN_POINT('Ctrl Pts',(21.533738485222,-91.3950185131866,6.07450195946819));
#22719=CARTESIAN_POINT('Ctrl Pts',(21.6390604846241,-91.1142772958209,6.0554612879563));
#22720=CARTESIAN_POINT('Ctrl Pts',(21.9303510312042,-90.3378273317271,6.00280023287342));
#22721=CARTESIAN_POINT('Ctrl Pts',(22.6421142021576,-89.719120565815,5.95013917779055));
#22722=CARTESIAN_POINT('Ctrl Pts',(23.4515532524732,-89.5387510753403,5.89747812270767));
#22723=CARTESIAN_POINT('Ctrl Pts',(24.2609923027888,-89.3583815848656,5.84481706762479));
#22724=CARTESIAN_POINT('Ctrl Pts',(25.1681072324665,-89.6163493698282,5.79215601254191));
#22725=CARTESIAN_POINT('Ctrl Pts',(25.7615059400007,-90.1956616372385,5.73949495745904));
#22726=CARTESIAN_POINT('Ctrl Pts',(26.3549046475349,-90.7749739046489,5.68683390237615));
#22727=CARTESIAN_POINT('Ctrl Pts',(26.6345871329256,-91.675630654507,5.63417284729328));
#22728=CARTESIAN_POINT('Ctrl Pts',(26.47371261597,-92.4891686800902,5.5815117922104));
#22729=CARTESIAN_POINT('Ctrl Pts',(26.3128380990145,-93.3027067056733,5.52885073712752));
#22730=CARTESIAN_POINT('Ctrl Pts',(25.7114065797126,-94.0291260069815,5.47618968204464));
#22731=CARTESIAN_POINT('Ctrl Pts',(24.9421775161413,-94.3389830337326,5.42352862696176));
#22732=CARTESIAN_POINT('Ctrl Pts',(24.17294845257,-94.6488400604838,5.37086757187889));
#22733=CARTESIAN_POINT('Ctrl Pts',(23.2359218447291,-94.5421348126778,5.31820651679601));
#22734=CARTESIAN_POINT('Ctrl Pts',(22.556055250635,-94.0672599412612,5.26554546171313));
#22735=CARTESIAN_POINT('Ctrl Pts',(21.8977961123825,-93.6074774981291,5.21455807530608));
#22736=CARTESIAN_POINT('Ctrl Pts',(21.4806106720036,-92.8025558114754,5.16357068889903));
#22737=CARTESIAN_POINT('Ctrl Pts',(21.4785001229596,-91.9995222403937,5.11258330249198));
#22738=CARTESIAN_POINT('Ctrl Pts',(21.4815255054053,-92.0021560919774,5.38741669750802));
#22739=CARTESIAN_POINT('Ctrl Pts',(21.4800478489828,-92.1657918915838,5.39777386760188));
#22740=CARTESIAN_POINT('Ctrl Pts',(21.494646624663,-92.3291652844524,5.40813103769574));
#22741=CARTESIAN_POINT('Ctrl Pts',(21.5262868021188,-92.4891687951612,5.4184882077896));
#22742=CARTESIAN_POINT('Ctrl Pts',(21.6871613569182,-93.3027070121194,5.47114926287248));
#22743=CARTESIAN_POINT('Ctrl Pts',(22.2885930176996,-94.0291264843089,5.52381031795536));
#22744=CARTESIAN_POINT('Ctrl Pts',(23.0578222622228,-94.3389835839502,5.57647137303824));
#22745=CARTESIAN_POINT('Ctrl Pts',(23.827051506746,-94.6488406835915,5.62913242812111));
#22746=CARTESIAN_POINT('Ctrl Pts',(24.7640783350111,-94.5421354106846,5.68179348320399));
#22747=CARTESIAN_POINT('Ctrl Pts',(25.4439450890356,-94.0672604275592,5.73445453828687));
#22748=CARTESIAN_POINT('Ctrl Pts',(26.1238118430602,-93.5923854444339,5.78711559336975));
#22749=CARTESIAN_POINT('Ctrl Pts',(26.5465185228442,-92.7493407510902,5.83977664845263));
#22750=CARTESIAN_POINT('Ctrl Pts',(26.5203604351554,-91.9204615033679,5.8924377035355));
#22751=CARTESIAN_POINT('Ctrl Pts',(26.4942023474666,-91.0915822556456,5.94509875861838));
#22752=CARTESIAN_POINT('Ctrl Pts',(26.019179492305,-90.2768684535448,5.99775981370126));
#22753=CARTESIAN_POINT('Ctrl Pts',(25.310722841277,-89.8458067103895,6.05042086878414));
#22754=CARTESIAN_POINT('Ctrl Pts',(24.602266190249,-89.4147449672342,6.10308192386702));
#22755=CARTESIAN_POINT('Ctrl Pts',(23.6603757433546,-89.3673352830245,6.15574297894989));
#22756=CARTESIAN_POINT('Ctrl Pts',(22.9122148925964,-89.7250787584281,6.20840403403277));
#22757=CARTESIAN_POINT('Ctrl Pts',(22.1640540418382,-90.0828222338316,6.26106508911565));
#22758=CARTESIAN_POINT('Ctrl Pts',(21.6096227872161,-90.8457188688485,6.31372614419853));
#22759=CARTESIAN_POINT('Ctrl Pts',(21.5003651647348,-91.6677820202957,6.36638719928141));
#22760=CARTESIAN_POINT('Ctrl Pts',(21.4858216342605,-91.7772087149585,6.37339703202361));
#22761=CARTESIAN_POINT('Ctrl Pts',(21.4791660807206,-91.8876837738621,6.38040686476582));
#22762=CARTESIAN_POINT('Ctrl Pts',(21.4800391863945,-91.998264576152,6.38741669750802));
#22763=CARTESIAN_POINT('Origin',(24.,-92.,5.));
#22764=CARTESIAN_POINT('',(21.4863708146038,-91.9995053986078,7.38741669750802));
#22765=CARTESIAN_POINT('',(21.4842078764603,-92.0020516719096,7.11258330249198));
#22766=CARTESIAN_POINT('',(21.4825,-92.,5.));
#22767=CARTESIAN_POINT('Ctrl Pts',(21.4842078764603,-92.0020516719096,7.11258330249198));
#22768=CARTESIAN_POINT('Ctrl Pts',(21.4887016384805,-91.4252697537026,7.07617562814403));
#22769=CARTESIAN_POINT('Ctrl Pts',(21.6859405266728,-90.8457100529155,7.03976795379607));
#22770=CARTESIAN_POINT('Ctrl Pts',(22.0492389093472,-90.402166695613,7.00336027944811));
#22771=CARTESIAN_POINT('Ctrl Pts',(22.5747236178373,-89.7606134629807,6.95069922436523));
#22772=CARTESIAN_POINT('Ctrl Pts',(23.4476300317824,-89.4036270970037,6.89803816928235));
#22773=CARTESIAN_POINT('Ctrl Pts',(24.2720801966772,-89.4931070083872,6.84537711419947));
#22774=CARTESIAN_POINT('Ctrl Pts',(25.096530361572,-89.5825869197707,6.79271605911659));
#22775=CARTESIAN_POINT('Ctrl Pts',(25.8725242774164,-90.1185331085148,6.74005500403372));
#22776=CARTESIAN_POINT('Ctrl Pts',(26.2481354595693,-90.8578848308521,6.68739394895084));
#22777=CARTESIAN_POINT('Ctrl Pts',(26.6237466417222,-91.5972365531893,6.63473289386796));
#22778=CARTESIAN_POINT('Ctrl Pts',(26.5989750901836,-92.5399938091198,6.58207183878508));
#22779=CARTESIAN_POINT('Ctrl Pts',(26.1850551266417,-93.2586000942469,6.52941078370221));
#22780=CARTESIAN_POINT('Ctrl Pts',(25.7711351630998,-93.9772063793741,6.47674972861933));
#22781=CARTESIAN_POINT('Ctrl Pts',(24.9680667875545,-94.4716616936979,6.42408867353644));
#22782=CARTESIAN_POINT('Ctrl Pts',(24.1400552133854,-94.5177221136004,6.37142761845357));
#22783=CARTESIAN_POINT('Ctrl Pts',(23.3120436392162,-94.5637825335029,6.31876656337069));
#22784=CARTESIAN_POINT('Ctrl Pts',(22.4590888664231,-94.1614480589841,6.26610550828782));
#22785=CARTESIAN_POINT('Ctrl Pts',(21.96802044113,-93.4931842405871,6.21344445320494));
#22786=CARTESIAN_POINT('Ctrl Pts',(21.6545077552948,-93.0665447464531,6.17982406963395));
#22787=CARTESIAN_POINT('Ctrl Pts',(21.4884972412917,-92.5315144383331,6.14620368606297));
#22788=CARTESIAN_POINT('Ctrl Pts',(21.4852341727342,-91.998341042672,6.11258330249198));
#22789=CARTESIAN_POINT('Ctrl Pts',(21.4800391863945,-91.998264576152,6.38741669750802));
#22790=CARTESIAN_POINT('Ctrl Pts',(21.4857252480609,-92.7184171072604,6.4330679198487));
#22791=CARTESIAN_POINT('Ctrl Pts',(21.8107173609326,-93.4430544346852,6.47871914218937));
#22792=CARTESIAN_POINT('Ctrl Pts',(22.3557695504229,-93.9118183295065,6.52437036453004));
#22793=CARTESIAN_POINT('Ctrl Pts',(22.9845155489329,-94.4525618193924,6.57703141961292));
#22794=CARTESIAN_POINT('Ctrl Pts',(23.9060915362935,-94.6528191312864,6.6296924746958));
#22795=CARTESIAN_POINT('Ctrl Pts',(24.7025470748465,-94.4217701584994,6.68235352977868));
#22796=CARTESIAN_POINT('Ctrl Pts',(25.4990026133996,-94.1907211857124,6.73501458486155));
#22797=CARTESIAN_POINT('Ctrl Pts',(26.170337703145,-93.5283659282443,6.78767563994443));
#22798=CARTESIAN_POINT('Ctrl Pts',(26.4120904232343,-92.7350937953596,6.84033669502731));
#22799=CARTESIAN_POINT('Ctrl Pts',(26.6538431433236,-91.941821662475,6.89299775011019));
#22800=CARTESIAN_POINT('Ctrl Pts',(26.4660134937569,-91.0176326541737,6.94565880519307));
#22801=CARTESIAN_POINT('Ctrl Pts',(25.9337854273443,-90.3816622657573,6.99831986027595));
#22802=CARTESIAN_POINT('Ctrl Pts',(25.4015573609318,-89.7456918773409,7.05098091535883));
#22803=CARTESIAN_POINT('Ctrl Pts',(24.5249308776734,-89.3979401088093,7.1036419704417));
#22804=CARTESIAN_POINT('Ctrl Pts',(23.7014710458108,-89.4961183060969,7.15630302552458));
#22805=CARTESIAN_POINT('Ctrl Pts',(22.8780112139481,-89.5942965033845,7.20896408060746));
#22806=CARTESIAN_POINT('Ctrl Pts',(22.1077180334812,-90.1384046664913,7.26162513569034));
#22807=CARTESIAN_POINT('Ctrl Pts',(21.7399326127095,-90.8816804900357,7.31428619077321));
#22808=CARTESIAN_POINT('Ctrl Pts',(21.569684509702,-91.2257433370738,7.33866302635148));
#22809=CARTESIAN_POINT('Ctrl Pts',(21.4856845592314,-91.6124832315577,7.36303986192975));
#22810=CARTESIAN_POINT('Ctrl Pts',(21.4863708146038,-91.9995053986078,7.38741669750802));
#22811=CARTESIAN_POINT('Origin',(24.,-92.,5.));
#22812=CARTESIAN_POINT('',(21.4817891743669,-92.002194435609,8.38741669750802));
#22813=CARTESIAN_POINT('',(21.4784371162896,-91.9996804085349,8.11258330249198));
#22814=CARTESIAN_POINT('',(21.4825,-92.,5.));
#22815=CARTESIAN_POINT('Ctrl Pts',(21.4784371162896,-91.9996804085349,8.11258330249198));
#22816=CARTESIAN_POINT('Ctrl Pts',(21.4784054922,-91.9821424240367,8.11146968039084));
#22817=CARTESIAN_POINT('Ctrl Pts',(21.4785728027446,-91.9646050586431,8.11035605828969));
#22818=CARTESIAN_POINT('Ctrl Pts',(21.4789408989108,-91.9470719086913,8.10924243618855));
#22819=CARTESIAN_POINT('Ctrl Pts',(21.496347461212,-91.1179628469758,8.05658138110567));
#22820=CARTESIAN_POINT('Ctrl Pts',(21.9627433725619,-90.298280199785,8.00392032602279));
#22821=CARTESIAN_POINT('Ctrl Pts',(22.6666099349663,-89.8597638322688,7.95125927093991));
#22822=CARTESIAN_POINT('Ctrl Pts',(23.3704764973707,-89.4212474647526,7.89859821585703));
#22823=CARTESIAN_POINT('Ctrl Pts',(24.3118137108296,-89.3638973769109,7.84593716077416));
#22824=CARTESIAN_POINT('Ctrl Pts',(25.0637091784649,-89.7137229122891,7.79327610569128));
#22825=CARTESIAN_POINT('Ctrl Pts',(25.8156046461002,-90.0635484476673,7.7406150506084));
#22826=CARTESIAN_POINT('Ctrl Pts',(26.378058367912,-90.8205496062653,7.68795399552553));
#22827=CARTESIAN_POINT('Ctrl Pts',(26.4959879359715,-91.6414133946616,7.63529294044265));
#22828=CARTESIAN_POINT('Ctrl Pts',(26.6139175040309,-92.462277183058,7.58263188535977));
#22829=CARTESIAN_POINT('Ctrl Pts',(26.2873229183381,-93.3470036012526,7.52997083027689));
#22830=CARTESIAN_POINT('Ctrl Pts',(25.6643204198242,-93.8943541437692,7.47730977519401));
#22831=CARTESIAN_POINT('Ctrl Pts',(25.0413179213102,-94.4417046862858,7.42464872011113));
#22832=CARTESIAN_POINT('Ctrl Pts',(24.1219075099752,-94.6516793531244,7.37198766502826));
#22833=CARTESIAN_POINT('Ctrl Pts',(23.3230574869989,-94.4290510376866,7.31932660994538));
#22834=CARTESIAN_POINT('Ctrl Pts',(22.5242074640225,-94.2064227222488,7.2666655548625));
#22835=CARTESIAN_POINT('Ctrl Pts',(21.8459178294048,-93.5511914245345,7.21400449977962));
#22836=CARTESIAN_POINT('Ctrl Pts',(21.5958045136134,-92.7605157260336,7.16134344469674));
#22837=CARTESIAN_POINT('Ctrl Pts',(21.5186091945673,-92.5164804869872,7.14509006396182));
#22838=CARTESIAN_POINT('Ctrl Pts',(21.4822017382943,-92.2595428818133,7.1288366832269));
#22839=CARTESIAN_POINT('Ctrl Pts',(21.4842078764603,-92.0020516719096,7.11258330249198));
#22840=CARTESIAN_POINT('Ctrl Pts',(21.4863708146038,-91.9995053986078,7.38741669750802));
#22841=CARTESIAN_POINT('Ctrl Pts',(21.4871670704398,-92.4485636814537,7.41570091701263));
#22842=CARTESIAN_POINT('Ctrl Pts',(21.6019742377664,-92.8980019807643,7.44398513651724));
#22843=CARTESIAN_POINT('Ctrl Pts',(21.8283524458306,-93.2815966720593,7.47226935602185));
#22844=CARTESIAN_POINT('Ctrl Pts',(22.2498353607997,-93.9957935465564,7.52493041110473));
#22845=CARTESIAN_POINT('Ctrl Pts',(23.0580788518144,-94.4817438115688,7.57759146618761));
#22846=CARTESIAN_POINT('Ctrl Pts',(23.8865307233467,-94.5190608637177,7.63025252127049));
#22847=CARTESIAN_POINT('Ctrl Pts',(24.714982594879,-94.5563779158666,7.68291357635336));
#22848=CARTESIAN_POINT('Ctrl Pts',(25.5636428469288,-94.1450617551521,7.73557463143624));
#22849=CARTESIAN_POINT('Ctrl Pts',(26.0476295286171,-93.4716510041371,7.78823568651912));
#22850=CARTESIAN_POINT('Ctrl Pts',(26.5316162103055,-92.798240253122,7.840896741602));
#22851=CARTESIAN_POINT('Ctrl Pts',(26.6509293216325,-91.8627349118065,7.89355779668488));
#22852=CARTESIAN_POINT('Ctrl Pts',(26.3514584187992,-91.0894031813449,7.94621885176775));
#22853=CARTESIAN_POINT('Ctrl Pts',(26.0519875159658,-90.3160714508833,7.99887990685063));
#22854=CARTESIAN_POINT('Ctrl Pts',(25.3337325989722,-89.7049133312758,8.0515409619335));
#22855=CARTESIAN_POINT('Ctrl Pts',(24.5224343499209,-89.5330983089572,8.10420201701638));
#22856=CARTESIAN_POINT('Ctrl Pts',(23.7111361008695,-89.3612832866386,8.15686307209926));
#22857=CARTESIAN_POINT('Ctrl Pts',(22.8067945197604,-89.6288113616089,8.20952412718214));
#22858=CARTESIAN_POINT('Ctrl Pts',(22.2195443159446,-90.2143563368687,8.26218518226502));
#22859=CARTESIAN_POINT('Ctrl Pts',(21.7540375466957,-90.6785113902208,8.30392902067935));
#22860=CARTESIAN_POINT('Ctrl Pts',(21.4877769931074,-91.3424942170044,8.34567285909369));
#22861=CARTESIAN_POINT('Ctrl Pts',(21.4817891743669,-92.002194435609,8.38741669750802));
#22862=CARTESIAN_POINT('Origin',(24.,-92.,5.));
#22863=CARTESIAN_POINT('',(21.4798238762261,-91.9984131135315,9.38741669750802));
#22864=CARTESIAN_POINT('',(21.4850512338518,-91.9982506073194,9.11258330249198));
#22865=CARTESIAN_POINT('',(21.4825,-92.,5.));
#22866=CARTESIAN_POINT('',(25.913465996665,-90.364012796625,10.));
#22867=CARTESIAN_POINT('Ctrl Pts',(21.4798238762261,-91.9984131135315,9.38741669750802));
#22868=CARTESIAN_POINT('Ctrl Pts',(21.4853062059344,-92.7270927102602,9.43362796642338));
#22869=CARTESIAN_POINT('Ctrl Pts',(21.8192672097013,-93.4600319638108,9.47983923533874));
#22870=CARTESIAN_POINT('Ctrl Pts',(22.3760118920419,-93.9288769835329,9.5260505042541));
#22871=CARTESIAN_POINT('Ctrl Pts',(23.0104623858715,-94.4631595078699,9.57871155933697));
#22872=CARTESIAN_POINT('Ctrl Pts',(23.9342250444886,-94.6544830013391,9.63137261441985));
#22873=CARTESIAN_POINT('Ctrl Pts',(24.7281293690809,-94.4146106072968,9.68403366950273));
#22874=CARTESIAN_POINT('Ctrl Pts',(25.5220336936733,-94.1747382132545,9.73669472458561));
#22875=CARTESIAN_POINT('Ctrl Pts',(26.186079684241,-93.5036699317008,9.78935577966849));
#22876=CARTESIAN_POINT('Ctrl Pts',(26.4192662809857,-92.7092700865749,9.84201683475137));
#22877=CARTESIAN_POINT('Ctrl Pts',(26.6524528777304,-91.9148702414489,9.89467788983425));
#22878=CARTESIAN_POINT('Ctrl Pts',(26.4547800806522,-90.9971388327508,9.94733894491712));
#22879=CARTESIAN_POINT('Ctrl Pts',(25.913465996665,-90.364012796625,10.));
#22880=CARTESIAN_POINT('',(22.0828970444786,-90.361465706548,10.));
#22881=CARTESIAN_POINT('Origin',(24.,-92.,10.));
#22882=CARTESIAN_POINT('Ctrl Pts',(22.0828885913556,-90.3614597865289,10.));
#22883=CARTESIAN_POINT('Ctrl Pts',(22.6060434082611,-89.752303655963,9.94901908464118));
#22884=CARTESIAN_POINT('Ctrl Pts',(23.4465814718894,-89.4121729024441,9.89803816928235));
#22885=CARTESIAN_POINT('Ctrl Pts',(24.2457357606074,-89.490515472492,9.84705725392353));
#22886=CARTESIAN_POINT('Ctrl Pts',(25.0712271767912,-89.57143991976,9.79439619884065));
#22887=CARTESIAN_POINT('Ctrl Pts',(25.8525621626002,-90.0988748222943,9.74173514375777));
#22888=CARTESIAN_POINT('Ctrl Pts',(26.2358875787344,-90.8341463056131,9.68907408867489));
#22889=CARTESIAN_POINT('Ctrl Pts',(26.6192129948686,-91.5694177889319,9.63641303359202));
#22890=CARTESIAN_POINT('Ctrl Pts',(26.6045288413281,-92.5125258530351,9.58375197850914));
#22891=CARTESIAN_POINT('Ctrl Pts',(26.1982520122281,-93.235497804129,9.53109092342626));
#22892=CARTESIAN_POINT('Ctrl Pts',(25.7919751831282,-93.9584697552228,9.47842986834338));
#22893=CARTESIAN_POINT('Ctrl Pts',(24.9941056784689,-94.4613055933072,9.4257688132605));
#22894=CARTESIAN_POINT('Ctrl Pts',(24.1666097496597,-94.5160865743966,9.37310775817762));
#22895=CARTESIAN_POINT('Ctrl Pts',(23.3391138208506,-94.5708675554859,9.32044670309475));
#22896=CARTESIAN_POINT('Ctrl Pts',(22.4819914678916,-94.1775936795802,9.26778564801187));
#22897=CARTESIAN_POINT('Ctrl Pts',(21.9839041146304,-93.5145597074388,9.21512459292899));
#22898=CARTESIAN_POINT('Ctrl Pts',(21.6606132128853,-93.0842077835489,9.18094416278332));
#22899=CARTESIAN_POINT('Ctrl Pts',(21.4885783498304,-92.5402099934131,9.14676373263765));
#22900=CARTESIAN_POINT('Ctrl Pts',(21.4850512338518,-91.9982506073194,9.11258330249198));
#22901=CARTESIAN_POINT('Origin',(24.,-92.,12.2084234471775));
#22902=CARTESIAN_POINT('',(20.9217237789782,-91.9992118506711,1.79157655282254));
#22903=CARTESIAN_POINT('',(20.9313888204345,-91.9996651715868,1.70842344717745));
#22904=CARTESIAN_POINT('',(20.9265,-91.9999999999999,12.2084234471775));
#22905=CARTESIAN_POINT('',(24.7937992825329,-94.9692229537457,0.999999999999999));
#22906=CARTESIAN_POINT('Ctrl Pts',(20.9313888204345,-91.9996651715868,1.70842344717745));
#22907=CARTESIAN_POINT('Ctrl Pts',(20.9310463723584,-91.5053847152746,1.68292651844981));
#22908=CARTESIAN_POINT('Ctrl Pts',(21.2764430280356,-89.9907712812588,1.6047685346393));
#22909=CARTESIAN_POINT('Ctrl Pts',(23.6460838609915,-88.3911589633379,1.4739494957459));
#22910=CARTESIAN_POINT('Ctrl Pts',(26.8312242725849,-89.7301456837401,1.31596633049727));
#22911=CARTESIAN_POINT('Ctrl Pts',(27.4433140827682,-93.1332953965992,1.15798316524863));
#22912=CARTESIAN_POINT('Ctrl Pts',(25.7762533017603,-94.7065713079336,1.05266105508288));
#22913=CARTESIAN_POINT('Ctrl Pts',(24.7937992825328,-94.9692229537457,0.999999999999999));
#22914=CARTESIAN_POINT('',(23.2062007174671,-94.9692229537457,0.999999999999999));
#22915=CARTESIAN_POINT('Origin',(24.,-92.,0.999999999999999));
#22916=CARTESIAN_POINT('Ctrl Pts',(20.9217237789782,-91.9992118506711,1.79157655282254));
#22917=CARTESIAN_POINT('Ctrl Pts',(20.9215776858271,-91.9562584671078,1.78934283757203));
#22918=CARTESIAN_POINT('Ctrl Pts',(20.9417782923113,-90.9007977729437,1.73444806723864));
#22919=CARTESIAN_POINT('Ctrl Pts',(22.1476053652116,-88.8820474355396,1.62689224182237));
#22920=CARTESIAN_POINT('Ctrl Pts',(25.5990313571955,-88.7444874247256,1.46890907657374));
#22921=CARTESIAN_POINT('Ctrl Pts',(27.5999505159819,-91.5606294856851,1.3109259113251));
#22922=CARTESIAN_POINT('Ctrl Pts',(26.3493022691421,-94.7394085052657,1.15462288580052));
#22923=CARTESIAN_POINT('Ctrl Pts',(24.1519061796922,-95.2254057458095,1.05098091535882));
#22924=CARTESIAN_POINT('Ctrl Pts',(23.2042985533737,-94.9743125149969,1.));
#22925=CARTESIAN_POINT('Origin',(24.,-92.,12.2084234471775));
#22926=CARTESIAN_POINT('',(20.930051482524,-91.9980972113707,2.79157655282254));
#22927=CARTESIAN_POINT('',(20.9249913784601,-92.002575532166,2.70842344717745));
#22928=CARTESIAN_POINT('',(20.9265,-91.9999999999999,12.2084234471775));
#22929=CARTESIAN_POINT('Ctrl Pts',(20.9249913784601,-92.002575532166,2.70842344717745));
#22930=CARTESIAN_POINT('Ctrl Pts',(20.9323854338683,-91.1760102376998,2.66555951561375));
#22931=CARTESIAN_POINT('Ctrl Pts',(21.7006357273797,-89.3218326978092,2.57003452896717));
#22932=CARTESIAN_POINT('Ctrl Pts',(24.8261378655289,-88.4685618660265,2.42184848723771));
#22933=CARTESIAN_POINT('Ctrl Pts',(27.4089767382702,-90.7619776329038,2.26386532198907));
#22934=CARTESIAN_POINT('Ctrl Pts',(26.8996888283721,-94.1783943608088,2.10588215674044));
#22935=CARTESIAN_POINT('Ctrl Pts',(23.7604241409854,-95.6187851374897,1.9478989914918));
#22936=CARTESIAN_POINT('Ctrl Pts',(21.309798993458,-94.0743436082074,1.81541275497081));
#22937=CARTESIAN_POINT('Ctrl Pts',(20.9317536605653,-92.5262657246815,1.73558757353269));
#22938=CARTESIAN_POINT('Ctrl Pts',(20.9313888204345,-91.9996651715868,1.70842344717745));
#22939=CARTESIAN_POINT('Ctrl Pts',(20.930051482524,-91.9980972113706,2.79157655282254));
#22940=CARTESIAN_POINT('Ctrl Pts',(20.9278794195688,-91.6185397913436,2.77197583473597));
#22941=CARTESIAN_POINT('Ctrl Pts',(21.1684425268396,-90.2218847391137,2.69971406156651));
#22942=CARTESIAN_POINT('Ctrl Pts',(23.2485917742673,-88.4519002035991,2.57479123331418));
#22943=CARTESIAN_POINT('Ctrl Pts',(26.5607981614372,-89.4317381309793,2.41680806806554));
#22944=CARTESIAN_POINT('Ctrl Pts',(27.5502714048858,-92.7410888412383,2.25882490281691));
#22945=CARTESIAN_POINT('Ctrl Pts',(25.3195309927208,-95.3782229777193,2.10084173756827));
#22946=CARTESIAN_POINT('Ctrl Pts',(21.9403861581344,-94.9572790184773,1.94509228757015));
#22947=CARTESIAN_POINT('Ctrl Pts',(20.9250219115291,-92.96890790723,1.84200389265491));
#22948=CARTESIAN_POINT('Ctrl Pts',(20.9217237789782,-91.9992118506711,1.79157655282254));
#22949=CARTESIAN_POINT('Origin',(24.,-92.,12.2084234471775));
#22950=CARTESIAN_POINT('',(20.9283007496159,-92.002571568945,3.79157655282255));
#22951=CARTESIAN_POINT('',(20.9237791307624,-91.9977671182961,3.70842344717745));
#22952=CARTESIAN_POINT('',(20.9265,-91.9999999999999,12.2084234471775));
#22953=CARTESIAN_POINT('Ctrl Pts',(20.9237791307624,-91.9977671182962,3.70842344717745));
#22954=CARTESIAN_POINT('Ctrl Pts',(20.9225843518948,-91.8519430302088,3.70085356786056));
#22955=CARTESIAN_POINT('Ctrl Pts',(20.9980297211289,-90.6929123616699,3.6406226334608));
#22956=CARTESIAN_POINT('Ctrl Pts',(22.4700852939276,-88.7116866521341,3.52773064397815));
#22957=CARTESIAN_POINT('Ctrl Pts',(25.9177920746621,-88.9217349563625,3.36974747872952));
#22958=CARTESIAN_POINT('Ctrl Pts',(27.6259964474171,-91.9238742346134,3.21176431348088));
#22959=CARTESIAN_POINT('Ctrl Pts',(26.0452973355111,-94.9950631778383,3.05378114823225));
#22960=CARTESIAN_POINT('Ctrl Pts',(22.6094456576622,-95.3496255535895,2.89579798298361));
#22961=CARTESIAN_POINT('Ctrl Pts',(21.0248752439865,-93.3940964847872,2.78067874929868));
#22962=CARTESIAN_POINT('Ctrl Pts',(20.923301368433,-92.1914980595947,2.71822057069663));
#22963=CARTESIAN_POINT('Ctrl Pts',(20.9249913784601,-92.002575532166,2.70842344717745));
#22964=CARTESIAN_POINT('Ctrl Pts',(20.9283007496159,-92.002571568945,3.79157655282255));
#22965=CARTESIAN_POINT('Ctrl Pts',(20.934059068375,-91.2877407010241,3.7546088318999));
#22966=CARTESIAN_POINT('Ctrl Pts',(21.5376069996117,-89.5458537101333,3.66498005589438));
#22967=CARTESIAN_POINT('Ctrl Pts',(24.429368893546,-88.3987114188411,3.52269022480599));
#22968=CARTESIAN_POINT('Ctrl Pts',(27.2506148119859,-90.3915408673734,3.36470705955735));
#22969=CARTESIAN_POINT('Ctrl Pts',(27.1234421205799,-93.8432978095595,3.20672389430872));
#22970=CARTESIAN_POINT('Ctrl Pts',(24.1632008669201,-95.6231203956682,3.04874072906008));
#22971=CARTESIAN_POINT('Ctrl Pts',(21.4405688436026,-94.3035551797938,2.91035828189803));
#22972=CARTESIAN_POINT('Ctrl Pts',(20.9337150795902,-92.6382929511448,2.82463688981885));
#22973=CARTESIAN_POINT('Ctrl Pts',(20.930051482524,-91.9980972113706,2.79157655282254));
#22974=CARTESIAN_POINT('Origin',(24.,-92.,12.2084234471775));
#22975=CARTESIAN_POINT('',(20.9216167340284,-91.9994167252631,4.79157655282255));
#22976=CARTESIAN_POINT('',(20.9312807091126,-91.9995675532498,4.70842344717745));
#22977=CARTESIAN_POINT('',(20.9265,-91.9999999999999,12.2084234471775));
#22978=CARTESIAN_POINT('Ctrl Pts',(20.9312807091126,-91.9995675532498,4.70842344717746));
#22979=CARTESIAN_POINT('Ctrl Pts',(20.9306675557931,-91.5161929213319,4.6834865650245));
#22980=CARTESIAN_POINT('Ctrl Pts',(21.2653046726707,-90.0128431381642,4.60588862778867));
#22981=CARTESIAN_POINT('Ctrl Pts',(23.6086716990241,-88.3943786103439,4.47562963546995));
#22982=CARTESIAN_POINT('Ctrl Pts',(26.8057463695968,-89.7018636398323,4.31764647022133));
#22983=CARTESIAN_POINT('Ctrl Pts',(27.4579133231717,-93.0938367815869,4.15966330497269));
#22984=CARTESIAN_POINT('Ctrl Pts',(24.9736348536359,-95.4936626411861,4.00168013972405));
#22985=CARTESIAN_POINT('Ctrl Pts',(21.7675877362369,-94.761466587215,3.85126685379231));
#22986=CARTESIAN_POINT('Ctrl Pts',(20.9308960188484,-92.8663912154057,3.75351462294344));
#22987=CARTESIAN_POINT('Ctrl Pts',(20.9237791307624,-91.9977671182962,3.70842344717745));
#22988=CARTESIAN_POINT('Ctrl Pts',(20.9216167340284,-91.9994167252631,4.79157655282255));
#22989=CARTESIAN_POINT('Ctrl Pts',(20.9215321543705,-91.9672353813212,4.78990288414672));
#22990=CARTESIAN_POINT('Ctrl Pts',(20.9365123597457,-90.9225665616792,4.73556816038801));
#22991=CARTESIAN_POINT('Ctrl Pts',(22.1148106026499,-88.9016620282347,4.62857238154642));
#22992=CARTESIAN_POINT('Ctrl Pts',(25.564542011833,-88.7280211581599,4.4705892162978));
#22993=CARTESIAN_POINT('Ctrl Pts',(27.595180415279,-91.5221767762026,4.31260605104916));
#22994=CARTESIAN_POINT('Ctrl Pts',(26.3648674705088,-94.7497343695717,4.15462288580052));
#22995=CARTESIAN_POINT('Ctrl Pts',(22.9895390126931,-95.4831890308962,3.99663972055189));
#22996=CARTESIAN_POINT('Ctrl Pts',(21.1060884403934,-93.6249316453216,3.8756242762259));
#22997=CARTESIAN_POINT('Ctrl Pts',(20.9258562597141,-92.3060276489616,3.80726988698278));
#22998=CARTESIAN_POINT('Ctrl Pts',(20.9283007496159,-92.002571568945,3.79157655282255));
#22999=CARTESIAN_POINT('Origin',(24.,-92.,12.2084234471775));
#23000=CARTESIAN_POINT('',(20.929838025779,-91.9979746552741,5.79157655282255));
#23001=CARTESIAN_POINT('',(20.9253102843548,-92.0026322735622,5.70842344717746));
#23002=CARTESIAN_POINT('',(20.9265,-91.9999999999999,12.2084234471775));
#23003=CARTESIAN_POINT('Ctrl Pts',(20.9253102843548,-92.0026322735622,5.70842344717746));
#23004=CARTESIAN_POINT('Ctrl Pts',(20.9326787378706,-91.1866490960334,5.66611956218844));
#23005=CARTESIAN_POINT('Ctrl Pts',(21.6842660273292,-89.3429095601005,5.57115462211654));
#23006=CARTESIAN_POINT('Ctrl Pts',(24.7888215932045,-88.4600276931838,5.42352862696176));
#23007=CARTESIAN_POINT('Ctrl Pts',(27.3956989960243,-90.726080156768,5.26554546171313));
#23008=CARTESIAN_POINT('Ctrl Pts',(26.9225615070512,-94.1476213996829,5.10756229646449));
#23009=CARTESIAN_POINT('Ctrl Pts',(23.7985609777147,-95.6211967303539,4.94957913121586));
#23010=CARTESIAN_POINT('Ctrl Pts',(21.3215407425041,-94.0960765086133,4.81653284812018));
#23011=CARTESIAN_POINT('Ctrl Pts',(20.9319623969258,-92.536970818142,4.73614762010738));
#23012=CARTESIAN_POINT('Ctrl Pts',(20.9312807091126,-91.9995675532498,4.70842344717746));
#23013=CARTESIAN_POINT('Ctrl Pts',(20.929838025779,-91.9979746552741,5.79157655282255));
#23014=CARTESIAN_POINT('Ctrl Pts',(20.9275818676586,-91.6293267200531,5.77253588131065));
#23015=CARTESIAN_POINT('Ctrl Pts',(21.1590710242286,-90.2438421434169,5.70083415471588));
#23016=CARTESIAN_POINT('Ctrl Pts',(23.2111785923562,-88.4600285259193,5.57647137303824));
#23017=CARTESIAN_POINT('Ctrl Pts',(26.53354332288,-89.404851549255,5.4184882077896));
#23018=CARTESIAN_POINT('Ctrl Pts',(27.5578977842682,-92.7035627953589,5.26050504254097));
#23019=CARTESIAN_POINT('Ctrl Pts',(25.3551175166524,-95.3641185720074,5.10252187729234));
#23020=CARTESIAN_POINT('Ctrl Pts',(21.959557040698,-94.9774442566837,4.94621238071952));
#23021=CARTESIAN_POINT('Ctrl Pts',(20.924193406317,-92.9798034901965,4.8425639392296));
#23022=CARTESIAN_POINT('Ctrl Pts',(20.9216167340284,-91.9994167252631,4.79157655282255));
#23023=CARTESIAN_POINT('Origin',(24.,-92.,12.2084234471775));
#23024=CARTESIAN_POINT('',(20.9285850678454,-92.0025047919022,6.79157655282255));
#23025=CARTESIAN_POINT('',(20.9234957058127,-91.9978813008157,6.70842344717746));
#23026=CARTESIAN_POINT('',(20.9265,-91.9999999999999,12.2084234471775));
#23027=CARTESIAN_POINT('Ctrl Pts',(20.9234957058127,-91.9978813008157,6.70842344717746));
#23028=CARTESIAN_POINT('Ctrl Pts',(20.9224297712393,-91.862878283601,6.70141361443525));
#23029=CARTESIAN_POINT('Ctrl Pts',(20.9915973803182,-90.7147700696949,6.64174272661017));
#23030=CARTESIAN_POINT('Ctrl Pts',(22.4354576201274,-88.7280203884636,6.52941078370221));
#23031=CARTESIAN_POINT('Ctrl Pts',(25.8851898408183,-88.9016612993893,6.37142761845357));
#23032=CARTESIAN_POINT('Ctrl Pts',(27.6249905303984,-91.885601165237,6.21344445320494));
#23033=CARTESIAN_POINT('Ctrl Pts',(26.0768010801705,-94.9733046786333,6.0554612879563));
#23034=CARTESIAN_POINT('Ctrl Pts',(22.6448821645724,-95.3641193633754,5.89747812270767));
#23035=CARTESIAN_POINT('Ctrl Pts',(21.031950207745,-93.4159924901843,5.78179884244805));
#23036=CARTESIAN_POINT('Ctrl Pts',(20.9235062815685,-92.2024076976298,5.71878061727132));
#23037=CARTESIAN_POINT('Ctrl Pts',(20.9253102843548,-92.0026322735622,5.70842344717746));
#23038=CARTESIAN_POINT('Ctrl Pts',(20.9285850678454,-92.0025047919022,6.79157655282255));
#23039=CARTESIAN_POINT('Ctrl Pts',(20.934071295281,-91.2983382673306,6.75516887847459));
#23040=CARTESIAN_POINT('Ctrl Pts',(21.5231707262624,-89.5673495506398,6.66610014904376));
#23041=CARTESIAN_POINT('Ctrl Pts',(24.3913282089151,-88.3943794585145,6.52437036453004));
#23042=CARTESIAN_POINT('Ctrl Pts',(27.2334540881776,-90.35731563858,6.3663871992814));
#23043=CARTESIAN_POINT('Ctrl Pts',(27.1427267432077,-93.8102226011646,6.20840403403277));
#23044=CARTESIAN_POINT('Ctrl Pts',(24.2014389748999,-95.6211958785123,6.05042086878413));
#23045=CARTESIAN_POINT('Ctrl Pts',(21.4539543223964,-94.3252211924294,5.9114783750474));
#23046=CARTESIAN_POINT('Ctrl Pts',(20.933821756151,-92.6489015397087,5.82519693639353));
#23047=CARTESIAN_POINT('Ctrl Pts',(20.929838025779,-91.9979746552741,5.79157655282255));
#23048=CARTESIAN_POINT('Origin',(24.,-92.,12.2084234471775));
#23049=CARTESIAN_POINT('',(20.9215398120818,-91.9996098254746,7.79157655282255));
#23050=CARTESIAN_POINT('',(20.9312256995769,-91.9993961639011,7.70842344717745));
#23051=CARTESIAN_POINT('',(20.9265,-91.9999999999999,12.2084234471775));
#23052=CARTESIAN_POINT('Ctrl Pts',(20.9312256995769,-91.9993961639011,7.70842344717745));
#23053=CARTESIAN_POINT('Ctrl Pts',(20.9303878819454,-91.5268985947141,7.68404661159918));
#23054=CARTESIAN_POINT('Ctrl Pts',(21.2544810105531,-90.0347579248865,7.60700872093804));
#23055=CARTESIAN_POINT('Ctrl Pts',(23.5706310054557,-88.3987105715367,7.47730977519401));
#23056=CARTESIAN_POINT('Ctrl Pts',(26.7813299086865,-89.6723730071853,7.31932660994538));
#23057=CARTESIAN_POINT('Ctrl Pts',(27.4692676579736,-93.0572726103796,7.16134344469675));
#23058=CARTESIAN_POINT('Ctrl Pts',(25.0104612250054,-95.483189850294,7.00336027944811));
#23059=CARTESIAN_POINT('Ctrl Pts',(21.7848978894954,-94.7822789631047,6.85238694694168));
#23060=CARTESIAN_POINT('Ctrl Pts',(20.9304375570666,-92.8770824147627,6.75407466951813));
#23061=CARTESIAN_POINT('Ctrl Pts',(20.9234957058127,-91.9978813008157,6.70842344717746));
#23062=CARTESIAN_POINT('Ctrl Pts',(20.9215398120818,-91.9996098254745,7.79157655282255));
#23063=CARTESIAN_POINT('Ctrl Pts',(20.9215012036849,-91.9781985065648,7.7904629307214));
#23064=CARTESIAN_POINT('Ctrl Pts',(20.9313646122183,-90.9443234457007,7.73668825353738));
#23065=CARTESIAN_POINT('Ctrl Pts',(22.0822083770023,-88.9217356813896,7.63025252127048));
#23066=CARTESIAN_POINT('Ctrl Pts',(25.5299143458989,-88.7116874252054,7.47226935602185));
#23067=CARTESIAN_POINT('Ctrl Pts',(27.5899360110292,-91.4842511522572,7.31428619077322));
#23068=CARTESIAN_POINT('Ctrl Pts',(26.3937630706594,-94.724616569919,7.15630302552458));
#23069=CARTESIAN_POINT('Ctrl Pts',(23.0263653754403,-95.4936618194068,6.99831986027594));
#23070=CARTESIAN_POINT('Ctrl Pts',(21.1145964666983,-93.6468831586791,6.87674436937527));
#23071=CARTESIAN_POINT('Ctrl Pts',(20.9261358659971,-92.3168639711034,6.80782993355747));
#23072=CARTESIAN_POINT('Ctrl Pts',(20.9285850678454,-92.0025047919022,6.79157655282255));
#23073=CARTESIAN_POINT('Origin',(24.,-92.,12.2084234471775));
#23074=CARTESIAN_POINT('',(20.9296146841086,-91.99786424691,8.79157655282255));
#23075=CARTESIAN_POINT('',(20.925632185667,-92.002679085539,8.70842344717746));
#23076=CARTESIAN_POINT('',(20.9265,-91.9999999999999,12.2084234471775));
#23077=CARTESIAN_POINT('Ctrl Pts',(20.925632185667,-92.002679085539,8.70842344717746));
#23078=CARTESIAN_POINT('Ctrl Pts',(20.9329424382584,-91.1972814204422,8.66667960876312));
#23079=CARTESIAN_POINT('Ctrl Pts',(21.6680869085146,-89.3640271254411,8.57227471526591));
#23080=CARTESIAN_POINT('Ctrl Pts',(24.7514084034007,-88.4518993616932,8.42520876668581));
#23081=CARTESIAN_POINT('Ctrl Pts',(27.3820616157699,-90.6903039066151,8.26722560143718));
#23082=CARTESIAN_POINT('Ctrl Pts',(26.9450699403022,-94.1166502818289,8.10924243618855));
#23083=CARTESIAN_POINT('Ctrl Pts',(23.8367990946118,-95.6231212490058,7.95125927093992));
#23084=CARTESIAN_POINT('Ctrl Pts',(21.3333230992967,-94.1179253063224,7.81765294126955));
#23085=CARTESIAN_POINT('Ctrl Pts',(20.9321978117167,-92.5476307745573,7.73670766668206));
#23086=CARTESIAN_POINT('Ctrl Pts',(20.9312256995769,-91.9993961639011,7.70842344717745));
#23087=CARTESIAN_POINT('Ctrl Pts',(20.9296146841086,-91.99786424691,8.79157655282255));
#23088=CARTESIAN_POINT('Ctrl Pts',(20.9272864716551,-91.6401225112664,8.77309592788534));
#23089=CARTESIAN_POINT('Ctrl Pts',(21.149833727977,-90.265786270585,8.70195424786525));
#23090=CARTESIAN_POINT('Ctrl Pts',(23.1738623478633,-88.4685627419331,8.57815151276229));
#23091=CARTESIAN_POINT('Ctrl Pts',(26.5060020988177,-89.3782461595948,8.42016834751365));
#23092=CARTESIAN_POINT('Ctrl Pts',(27.5651288739417,-92.6659672391889,8.26218518226502));
#23093=CARTESIAN_POINT('Ctrl Pts',(25.3905540118639,-95.3496247591348,8.10420201701639));
#23094=CARTESIAN_POINT('Ctrl Pts',(21.9789224334286,-94.9975617834283,7.94733247386889));
#23095=CARTESIAN_POINT('Ctrl Pts',(20.9233269207871,-92.9906987464103,7.84312398580428));
#23096=CARTESIAN_POINT('Ctrl Pts',(20.9215398120818,-91.9996098254745,7.79157655282255));
#23097=CARTESIAN_POINT('Origin',(24.,-92.,12.2084234471775));
#23098=CARTESIAN_POINT('',(20.9297109890477,-92.0031050978172,9.79157655282255));
#23099=CARTESIAN_POINT('',(20.9232328435277,-91.9980626432727,9.70842344717746));
#23100=CARTESIAN_POINT('',(20.9265,-91.9999999999999,12.2084234471775));
#23101=CARTESIAN_POINT('',(23.2062007174671,-94.9692229537457,10.));
#23102=CARTESIAN_POINT('Ctrl Pts',(23.2062007174671,-94.9692229537457,10.));
#23103=CARTESIAN_POINT('Ctrl Pts',(22.2237466982397,-94.7065713079336,9.94733894491712));
#23104=CARTESIAN_POINT('Ctrl Pts',(21.1240889563567,-93.6687841901452,9.87786446252464));
#23105=CARTESIAN_POINT('Ctrl Pts',(20.9273641407895,-92.3283664602092,9.80838998013216));
#23106=CARTESIAN_POINT('Ctrl Pts',(20.9297109890477,-92.0031050978172,9.79157655282255));
#23107=CARTESIAN_POINT('',(24.7956974280508,-94.9743010520069,10.));
#23108=CARTESIAN_POINT('Origin',(24.,-92.,10.));
#23109=CARTESIAN_POINT('Ctrl Pts',(24.7957018439802,-94.9743128659187,10.));
#23110=CARTESIAN_POINT('Ctrl Pts',(23.8480947973978,-95.2254055278759,9.94901908464117));
#23111=CARTESIAN_POINT('Ctrl Pts',(21.7874433743319,-94.7696547721756,9.85182690036699));
#23112=CARTESIAN_POINT('Ctrl Pts',(20.9299259678012,-92.8876740595769,9.75463471609281));
#23113=CARTESIAN_POINT('Ctrl Pts',(20.9232328435277,-91.9980626432727,9.70842344717746));
#23114=CARTESIAN_POINT('Origin',(-92.,24.,5.));
#23115=CARTESIAN_POINT('',(-94.5134952662832,24.0002743405048,1.38741669750802));
#23116=CARTESIAN_POINT('',(-94.515626303127,23.9964684456989,1.11258330249198));
#23117=CARTESIAN_POINT('',(-94.5175,24.,5.));
#23118=CARTESIAN_POINT('',(-93.913465996665,25.635987203375,0.999999999999999));
#23119=CARTESIAN_POINT('Ctrl Pts',(-94.515626303127,23.9964684456989,1.11258330249198));
#23120=CARTESIAN_POINT('Ctrl Pts',(-94.5104636015443,24.5890866576526,1.07505553499465));
#23121=CARTESIAN_POINT('Ctrl Pts',(-94.299221828084,25.1848035603044,1.03752776749732));
#23122=CARTESIAN_POINT('Ctrl Pts',(-93.913465996665,25.635987203375,0.999999999999995));
#23123=CARTESIAN_POINT('',(-94.5175,24.,1.));
#23124=CARTESIAN_POINT('Origin',(-92.,24.,1.));
#23125=CARTESIAN_POINT('',(-94.5175,24.,0.));
#23126=CARTESIAN_POINT('',(-94.5175,24.,5.));
#23127=CARTESIAN_POINT('Origin',(-92.,24.,0.));
#23128=CARTESIAN_POINT('',(-90.0828968401885,25.638534314987,1.));
#23129=CARTESIAN_POINT('Origin',(-92.,24.,1.));
#23130=CARTESIAN_POINT('Ctrl Pts',(-90.0828883826538,25.6385402378131,1.));
#23131=CARTESIAN_POINT('Ctrl Pts',(-90.6060431378804,26.2476960524168,1.05098091535882));
#23132=CARTESIAN_POINT('Ctrl Pts',(-91.4465813540296,26.5878274641506,1.10196183071765));
#23133=CARTESIAN_POINT('Ctrl Pts',(-92.2457357689255,26.5094850217743,1.15294274607647));
#23134=CARTESIAN_POINT('Ctrl Pts',(-93.0712273154455,26.4285607063854,1.20560380115935));
#23135=CARTESIAN_POINT('Ctrl Pts',(-93.8525624034825,25.9011253696412,1.25826485624222));
#23136=CARTESIAN_POINT('Ctrl Pts',(-94.2358878554464,25.1658537184213,1.3109259113251));
#23137=CARTESIAN_POINT('Ctrl Pts',(-94.4214827265106,24.8098568843833,1.33642284005274));
#23138=CARTESIAN_POINT('Ctrl Pts',(-94.5137757562955,24.4051388409379,1.36191976878038));
#23139=CARTESIAN_POINT('Ctrl Pts',(-94.5134952662832,24.0002743405048,1.38741669750802));
#23140=CARTESIAN_POINT('Origin',(-92.,24.,5.));
#23141=CARTESIAN_POINT('',(-94.5187354043534,23.9978903847199,2.38741669750802));
#23142=CARTESIAN_POINT('',(-94.5214125398479,24.0006455489044,2.11258330249198));
#23143=CARTESIAN_POINT('',(-94.5175,24.,5.));
#23144=CARTESIAN_POINT('Ctrl Pts',(-94.5214125398479,24.0006455489044,2.11258330249198));
#23145=CARTESIAN_POINT('Ctrl Pts',(-94.5215322047964,24.0358286169429,2.11034958724147));
#23146=CARTESIAN_POINT('Ctrl Pts',(-94.5208589221676,24.0710069479233,2.10811587199095));
#23147=CARTESIAN_POINT('Ctrl Pts',(-94.5193783712999,24.1061512068912,2.10588215674044));
#23148=CARTESIAN_POINT('Ctrl Pts',(-94.4844735772458,24.9346962763345,2.05322110165756));
#23149=CARTESIAN_POINT('Ctrl Pts',(-94.0008839809308,25.7443039053207,2.00056004657469));
#23150=CARTESIAN_POINT('Ctrl Pts',(-93.2879126402955,26.1678868628806,1.94789899149181));
#23151=CARTESIAN_POINT('Ctrl Pts',(-92.5749412996603,26.5914698204405,1.89523793640893));
#23152=CARTESIAN_POINT('Ctrl Pts',(-91.6325882147046,26.629028106574,1.84257688132605));
#23153=CARTESIAN_POINT('Ctrl Pts',(-90.8882532947046,26.2633575703982,1.78991582624317));
#23154=CARTESIAN_POINT('Ctrl Pts',(-90.1439183747045,25.8976870342223,1.73725477116029));
#23155=CARTESIAN_POINT('Ctrl Pts',(-89.59760161966,25.128787675737,1.68459371607741));
#23156=CARTESIAN_POINT('Ctrl Pts',(-89.4970124750772,24.3057173952046,1.63193266099454));
#23157=CARTESIAN_POINT('Ctrl Pts',(-89.3964233304945,23.4826471146723,1.57927160591166));
#23158=CARTESIAN_POINT('Ctrl Pts',(-89.7415617963736,22.6054059120929,1.52661055082878));
#23159=CARTESIAN_POINT('Ctrl Pts',(-90.3760121357463,22.0711233584703,1.4739494957459));
#23160=CARTESIAN_POINT('Ctrl Pts',(-91.010462475119,21.5368408048477,1.42128844066303));
#23161=CARTESIAN_POINT('Ctrl Pts',(-91.9342246879853,21.3455169001819,1.36862738558015));
#23162=CARTESIAN_POINT('Ctrl Pts',(-92.7281292572936,21.5853895325345,1.31596633049727));
#23163=CARTESIAN_POINT('Ctrl Pts',(-93.5220338266019,21.8252621648871,1.26330527541439));
#23164=CARTESIAN_POINT('Ctrl Pts',(-94.1860807523522,22.4963313342582,1.21064422033151));
#23165=CARTESIAN_POINT('Ctrl Pts',(-94.4192673158648,23.2907310848487,1.15798316524863));
#23166=CARTESIAN_POINT('Ctrl Pts',(-94.4862784936919,23.5190189507993,1.14284987766308));
#23167=CARTESIAN_POINT('Ctrl Pts',(-94.5177081921648,23.7574917511602,1.12771659007753));
#23168=CARTESIAN_POINT('Ctrl Pts',(-94.515626303127,23.9964684456989,1.11258330249198));
#23169=CARTESIAN_POINT('Ctrl Pts',(-94.5134952662832,24.0002743405048,1.38741669750802));
#23170=CARTESIAN_POINT('Ctrl Pts',(-94.5131964355411,23.5689364894249,1.41458082386326));
#23171=CARTESIAN_POINT('Ctrl Pts',(-94.4078218494689,23.1374324020536,1.4417449502185));
#23172=CARTESIAN_POINT('Ctrl Pts',(-94.1982522460689,22.7645021148375,1.46890907657374));
#23173=CARTESIAN_POINT('Ctrl Pts',(-93.7919753688369,22.041530128169,1.52157013165662));
#23174=CARTESIAN_POINT('Ctrl Pts',(-92.9941057984822,21.5386941205273,1.57423118673949));
#23175=CARTESIAN_POINT('Ctrl Pts',(-92.1666097792392,21.4839131073784,1.62689224182237));
#23176=CARTESIAN_POINT('Ctrl Pts',(-91.3391137599961,21.4291320942294,1.67955329690525));
#23177=CARTESIAN_POINT('Ctrl Pts',(-90.4819912918646,21.8224060755732,1.73221435198813));
#23178=CARTESIAN_POINT('Ctrl Pts',(-89.9839038787409,22.4854401372494,1.78487540707101));
#23179=CARTESIAN_POINT('Ctrl Pts',(-89.4858164656172,23.1484741989255,1.83753646215389));
#23180=CARTESIAN_POINT('Ctrl Pts',(-89.3467641075012,24.081268340934,1.89019751723676));
#23181=CARTESIAN_POINT('Ctrl Pts',(-89.6298379034513,24.8607543617003,1.94285857231964));
#23182=CARTESIAN_POINT('Ctrl Pts',(-89.9129116994015,25.6402403824667,1.99551962740252));
#23183=CARTESIAN_POINT('Ctrl Pts',(-90.6181116494178,26.2664182819909,2.0481806824854));
#23184=CARTESIAN_POINT('Ctrl Pts',(-91.4256035941691,26.4553204550754,2.10084173756828));
#23185=CARTESIAN_POINT('Ctrl Pts',(-92.2330955389203,26.64422262816,2.15350279265116));
#23186=CARTESIAN_POINT('Ctrl Pts',(-93.1428794784065,26.3958490748049,2.20616384773403));
#23187=CARTESIAN_POINT('Ctrl Pts',(-93.7423596992758,25.8228342131325,2.25882490281691));
#23188=CARTESIAN_POINT('Ctrl Pts',(-94.2303119273634,25.3564236982452,2.30168883438061));
#23189=CARTESIAN_POINT('Ctrl Pts',(-94.5126789427165,24.674928901641,2.34455276594432));
#23190=CARTESIAN_POINT('Ctrl Pts',(-94.5187354043534,23.9978903847199,2.38741669750802));
#23191=CARTESIAN_POINT('Origin',(-92.,24.,5.));
#23192=CARTESIAN_POINT('',(-94.5197283545653,24.0018289503525,3.38741669750802));
#23193=CARTESIAN_POINT('',(-94.5145913332515,24.0015585714996,3.11258330249198));
#23194=CARTESIAN_POINT('',(-94.5175,24.,5.));
#23195=CARTESIAN_POINT('Ctrl Pts',(-94.5145913332515,24.0015585714996,3.11258330249198));
#23196=CARTESIAN_POINT('Ctrl Pts',(-94.5163704675347,24.3124536217307,3.0929825844054));
#23197=CARTESIAN_POINT('Ctrl Pts',(-94.4629228052196,24.6227586740842,3.07338186631882));
#23198=CARTESIAN_POINT('Ctrl Pts',(-94.3514581912821,24.9105967308751,3.05378114823225));
#23199=CARTESIAN_POINT('Ctrl Pts',(-94.0519873173872,25.6839283862082,3.00112009314937));
#23200=CARTESIAN_POINT('Ctrl Pts',(-93.3337324697514,26.2950864454346,2.94845903806649));
#23201=CARTESIAN_POINT('Ctrl Pts',(-92.5224342992987,26.4669014516815,2.89579798298361));
#23202=CARTESIAN_POINT('Ctrl Pts',(-91.711136128846,26.6387164579284,2.84313692790074));
#23203=CARTESIAN_POINT('Ctrl Pts',(-90.8067946355765,26.3711884111957,2.79047587281786));
#23204=CARTESIAN_POINT('Ctrl Pts',(-90.2195444883874,25.7856434915614,2.73781481773498));
#23205=CARTESIAN_POINT('Ctrl Pts',(-89.6322943411984,25.200098571927,2.6851537626521));
#23206=CARTESIAN_POINT('Ctrl Pts',(-89.3621355400899,24.2965367793909,2.63249270756922));
#23207=CARTESIAN_POINT('Ctrl Pts',(-89.5315889600924,23.4847436160309,2.57983165248634));
#23208=CARTESIAN_POINT('Ctrl Pts',(-89.7010423800949,22.6729504526708,2.52717059740347));
#23209=CARTESIAN_POINT('Ctrl Pts',(-90.3101080212083,21.9529259184869,2.47450954232059));
#23210=CARTESIAN_POINT('Ctrl Pts',(-91.0825657562014,21.6512036069522,2.42184848723771));
#23211=CARTESIAN_POINT('Ctrl Pts',(-91.8550234911946,21.3494812954175,2.36918743215483));
#23212=CARTESIAN_POINT('Ctrl Pts',(-92.7908733200675,21.466061206532,2.31652637707195));
#23213=CARTESIAN_POINT('Ctrl Pts',(-93.4656882386074,21.9480924170396,2.26386532198907));
#23214=CARTESIAN_POINT('Ctrl Pts',(-94.1118796445259,22.4096773895362,2.21343798215671));
#23215=CARTESIAN_POINT('Ctrl Pts',(-94.5187110383817,23.2063686024949,2.16301064232434));
#23216=CARTESIAN_POINT('Ctrl Pts',(-94.5214125398479,24.0006455489044,2.11258330249198));
#23217=CARTESIAN_POINT('Ctrl Pts',(-94.5187354043534,23.9978903847199,2.38741669750802));
#23218=CARTESIAN_POINT('Ctrl Pts',(-94.5201196894756,23.8431441975285,2.3972138210272));
#23219=CARTESIAN_POINT('Ctrl Pts',(-94.5070691791327,23.6886308117444,2.40701094454637));
#23220=CARTESIAN_POINT('Ctrl Pts',(-94.4787393827788,23.5369716347155,2.41680806806555));
#23221=CARTESIAN_POINT('Ctrl Pts',(-94.3264623431602,22.7217800879606,2.46946912314842));
#23222=CARTESIAN_POINT('Ctrl Pts',(-93.7327317616706,21.9890531644405,2.5221301782313));
#23223=CARTESIAN_POINT('Ctrl Pts',(-92.9668162273558,21.6710932957471,2.57479123331418));
#23224=CARTESIAN_POINT('Ctrl Pts',(-92.2009006930409,21.3531334270537,2.62745228839706));
#23225=CARTESIAN_POINT('Ctrl Pts',(-91.2628002059009,21.449940613187,2.68011334347994));
#23226=CARTESIAN_POINT('Ctrl Pts',(-90.5779585445906,21.9176119917392,2.73277439856282));
#23227=CARTESIAN_POINT('Ctrl Pts',(-89.8931168832802,22.3852833702914,2.78543545364569));
#23228=CARTESIAN_POINT('Ctrl Pts',(-89.4615340477996,23.2238189412625,2.83809650872857));
#23229=CARTESIAN_POINT('Ctrl Pts',(-89.4789406121676,24.0529280971511,2.89075756381145));
#23230=CARTESIAN_POINT('Ctrl Pts',(-89.4963471765355,24.8820372530396,2.94341861889433));
#23231=CARTESIAN_POINT('Ctrl Pts',(-89.9627431407521,25.7017199938457,2.99607967397721));
#23232=CARTESIAN_POINT('Ctrl Pts',(-90.6666097831963,26.1402364113417,3.04874072906009));
#23233=CARTESIAN_POINT('Ctrl Pts',(-91.3704764256404,26.5787528288377,3.10140178414296));
#23234=CARTESIAN_POINT('Ctrl Pts',(-92.3118137463122,26.6361029230235,3.15406283922584));
#23235=CARTESIAN_POINT('Ctrl Pts',(-93.063709299524,26.2862773477979,3.20672389430872));
#23236=CARTESIAN_POINT('Ctrl Pts',(-93.8156048527357,25.9364517725724,3.2593849493916));
#23237=CARTESIAN_POINT('Ctrl Pts',(-94.3780586384875,25.1794505279353,3.31204600447447));
#23238=CARTESIAN_POINT('Ctrl Pts',(-94.4959882199517,24.358586646163,3.36470705955735));
#23239=CARTESIAN_POINT('Ctrl Pts',(-94.5129402673076,24.2405897600233,3.37227693887424));
#23240=CARTESIAN_POINT('Ctrl Pts',(-94.5207069963199,24.1212732637326,3.37984681819113));
#23241=CARTESIAN_POINT('Ctrl Pts',(-94.5197283545653,24.0018289503525,3.38741669750802));
#23242=CARTESIAN_POINT('Origin',(-92.,24.,5.));
#23243=CARTESIAN_POINT('',(-94.5135838218621,24.000354216548,4.38741669750802));
#23244=CARTESIAN_POINT('',(-94.5160253566384,23.9978936308049,4.11258330249198));
#23245=CARTESIAN_POINT('',(-94.5175,24.,5.));
#23246=CARTESIAN_POINT('Ctrl Pts',(-94.5160253566384,23.9978936308049,4.11258330249198));
#23247=CARTESIAN_POINT('Ctrl Pts',(-94.5113087243027,24.5834107803607,4.07561558156934));
#23248=CARTESIAN_POINT('Ctrl Pts',(-94.3074058729855,25.1718905111793,4.03864786064669));
#23249=CARTESIAN_POINT('Ctrl Pts',(-93.9337852402154,25.6183375776454,4.00168013972405));
#23250=CARTESIAN_POINT('Ctrl Pts',(-93.4015572253053,26.2543079045141,3.94901908464117));
#23251=CARTESIAN_POINT('Ctrl Pts',(-92.5249308268757,26.6020596393699,3.8963580295583));
#23252=CARTESIAN_POINT('Ctrl Pts',(-91.7014710746985,26.5038814515943,3.84369697447542));
#23253=CARTESIAN_POINT('Ctrl Pts',(-90.8780113225213,26.4057032638187,3.79103591939254));
#23254=CARTESIAN_POINT('Ctrl Pts',(-90.1077182165965,25.8615951534119,3.73837486430966));
#23255=CARTESIAN_POINT('Ctrl Pts',(-89.7399328314132,25.1183194017708,3.68571380922678));
#23256=CARTESIAN_POINT('Ctrl Pts',(-89.3721474462299,24.3750436501297,3.6330527541439));
#23257=CARTESIAN_POINT('Ctrl Pts',(-89.4068697817883,23.4326002572544,3.58039169906103));
#23258=CARTESIAN_POINT('Ctrl Pts',(-89.8283526559748,22.7184034519114,3.52773064397815));
#23259=CARTESIAN_POINT('Ctrl Pts',(-90.2498355301613,22.0042066465685,3.47506958889527));
#23260=CARTESIAN_POINT('Ctrl Pts',(-91.058078942976,21.518256428758,3.42240853381239));
#23261=CARTESIAN_POINT('Ctrl Pts',(-91.8865307343323,21.4809393801385,3.36974747872952));
#23262=CARTESIAN_POINT('Ctrl Pts',(-92.7149825256887,21.4436223315191,3.31708642364664));
#23263=CARTESIAN_POINT('Ctrl Pts',(-93.5636426955868,21.8549384520908,3.26442536856376));
#23264=CARTESIAN_POINT('Ctrl Pts',(-94.0476293304588,22.5283491380965,3.21176431348088));
#23265=CARTESIAN_POINT('Ctrl Pts',(-94.3514736272621,22.951112870825,3.17870397648458));
#23266=CARTESIAN_POINT('Ctrl Pts',(-94.5115904850835,23.4771749705661,3.14564363948828));
#23267=CARTESIAN_POINT('Ctrl Pts',(-94.5145913332515,24.0015585714996,3.11258330249198));
#23268=CARTESIAN_POINT('Ctrl Pts',(-94.5197283545653,24.0018289503525,3.38741669750802));
#23269=CARTESIAN_POINT('Ctrl Pts',(-94.5138989211591,23.2903401268977,3.43250787327401));
#23270=CARTESIAN_POINT('Ctrl Pts',(-94.1977683024704,22.5743161275881,3.47759904904));
#23271=CARTESIAN_POINT('Ctrl Pts',(-93.6643206092001,22.105645640677,3.52269022480599));
#23272=CARTESIAN_POINT('Ctrl Pts',(-93.0413180398075,21.5582950358707,3.57535127988887));
#23273=CARTESIAN_POINT('Ctrl Pts',(-92.1219075238456,21.3483203451655,3.62801233497174));
#23274=CARTESIAN_POINT('Ctrl Pts',(-91.3230574099717,21.5709486859402,3.68067339005462));
#23275=CARTESIAN_POINT('Ctrl Pts',(-90.5242072960977,21.7935770267148,3.7333344451375));
#23276=CARTESIAN_POINT('Ctrl Pts',(-89.8459175843116,22.4488083989694,3.78599550022038));
#23277=CARTESIAN_POINT('Ctrl Pts',(-89.5958042400641,23.239484187431,3.83865655530326));
#23278=CARTESIAN_POINT('Ctrl Pts',(-89.3456908958165,24.0301599758926,3.89131761038613));
#23279=CARTESIAN_POINT('Ctrl Pts',(-89.5237539191075,24.9562801805613,3.94397866546901));
#23280=CARTESIAN_POINT('Ctrl Pts',(-90.0492386873867,25.5978334861916,3.99663972055189));
#23281=CARTESIAN_POINT('Ctrl Pts',(-90.5747234556659,26.2393867918219,4.04930077563477));
#23282=CARTESIAN_POINT('Ctrl Pts',(-91.4476299689333,26.5963731984139,4.10196183071765));
#23283=CARTESIAN_POINT('Ctrl Pts',(-92.2720802276353,26.5068932768485,4.15462288580053));
#23284=CARTESIAN_POINT('Ctrl Pts',(-93.0965304863372,26.417413355283,4.2072839408834));
#23285=CARTESIAN_POINT('Ctrl Pts',(-93.8725244904738,25.8814671055602,4.25994499596628));
#23286=CARTESIAN_POINT('Ctrl Pts',(-94.2481357153638,25.1421152990992,4.31260605104916));
#23287=CARTESIAN_POINT('Ctrl Pts',(-94.4260009866856,24.7920059281746,4.33754293320211));
#23288=CARTESIAN_POINT('Ctrl Pts',(-94.5140860549172,24.396285723967,4.36247981535507));
#23289=CARTESIAN_POINT('Ctrl Pts',(-94.5135838218621,24.000354216548,4.38741669750802));
#23290=CARTESIAN_POINT('Origin',(-92.,24.,5.));
#23291=CARTESIAN_POINT('',(-94.5184741887081,23.9978439082845,5.38741669750803));
#23292=CARTESIAN_POINT('',(-94.5215002261916,24.0004777596726,5.11258330249198));
#23293=CARTESIAN_POINT('',(-94.5175,24.,5.));
#23294=CARTESIAN_POINT('Ctrl Pts',(-94.5215002261916,24.0004777596726,5.11258330249198));
#23295=CARTESIAN_POINT('Ctrl Pts',(-94.521569505293,24.0268374618337,5.11090963381616));
#23296=CARTESIAN_POINT('Ctrl Pts',(-94.5211915450548,24.0531951295678,5.10923596514032));
#23297=CARTESIAN_POINT('Ctrl Pts',(-94.5203601912645,24.0795384889352,5.1075622964645));
#23298=CARTESIAN_POINT('Ctrl Pts',(-94.494202106107,24.9084176564483,5.05490124138162));
#23299=CARTESIAN_POINT('Ctrl Pts',(-94.0191792969125,25.723131379711,5.00224018629874));
#23300=CARTESIAN_POINT('Ctrl Pts',(-93.3107227144406,26.1541930811531,4.94957913121586));
#23301=CARTESIAN_POINT('Ctrl Pts',(-92.6022661319687,26.5852547825952,4.89691807613298));
#23302=CARTESIAN_POINT('Ctrl Pts',(-91.6603757762195,26.6326644622167,4.84425702105011));
#23303=CARTESIAN_POINT('Ctrl Pts',(-90.9122149978595,26.2749210214316,4.79159596596723));
#23304=CARTESIAN_POINT('Ctrl Pts',(-90.1640542194994,25.9171775806464,4.73893491088435));
#23305=CARTESIAN_POINT('Ctrl Pts',(-89.6096230185287,25.1542810194546,4.68627385580147));
#23306=CARTESIAN_POINT('Ctrl Pts',(-89.50036540662,24.3322179475565,4.63361280071859));
#23307=CARTESIAN_POINT('Ctrl Pts',(-89.3911077947114,23.5101548756584,4.58095174563571));
#23308=CARTESIAN_POINT('Ctrl Pts',(-89.7270237718648,22.6289252930542,4.52829069055284));
#23309=CARTESIAN_POINT('Ctrl Pts',(-90.3557697095322,22.0881818554959,4.47562963546996));
#23310=CARTESIAN_POINT('Ctrl Pts',(-90.9845156471996,21.5474384179377,4.42296858038708));
#23311=CARTESIAN_POINT('Ctrl Pts',(-91.9060915453809,21.3471811254255,4.3703075253042));
#23312=CARTESIAN_POINT('Ctrl Pts',(-92.7025470068623,21.5782300758527,4.31764647022132));
#23313=CARTESIAN_POINT('Ctrl Pts',(-93.4990024683437,21.80927902628,4.26498541513844));
#23314=CARTESIAN_POINT('Ctrl Pts',(-94.1703374931251,22.4716342196466,4.21232436005557));
#23315=CARTESIAN_POINT('Ctrl Pts',(-94.4120901898205,23.2649062757708,4.15966330497269));
#23316=CARTESIAN_POINT('Ctrl Pts',(-94.4841340531159,23.5013064663318,4.14396997081245));
#23317=CARTESIAN_POINT('Ctrl Pts',(-94.5180276355322,23.7493331013702,4.12827663665222));
#23318=CARTESIAN_POINT('Ctrl Pts',(-94.5160253566384,23.9978936308049,4.11258330249198));
#23319=CARTESIAN_POINT('Ctrl Pts',(-94.5135838218621,24.000354216548,4.38741669750802));
#23320=CARTESIAN_POINT('Ctrl Pts',(-94.5130254522959,23.5601679289135,4.41514087043795));
#23321=CARTESIAN_POINT('Ctrl Pts',(-94.4029695423041,23.1197204618369,4.44286504336787));
#23322=CARTESIAN_POINT('Ctrl Pts',(-94.1850553752593,22.7413997625482,4.47058921629779));
#23323=CARTESIAN_POINT('Ctrl Pts',(-93.7711353646214,22.0227933956572,4.52325027138067));
#23324=CARTESIAN_POINT('Ctrl Pts',(-92.968066897702,21.5283380250743,4.57591132646355));
#23325=CARTESIAN_POINT('Ctrl Pts',(-92.1400552293209,21.4822775999311,4.62857238154643));
#23326=CARTESIAN_POINT('Ctrl Pts',(-91.3120435609398,21.4362171747878,4.6812334366293));
#23327=CARTESIAN_POINT('Ctrl Pts',(-90.4590886910969,21.8385516950844,4.73389449171218));
#23328=CARTESIAN_POINT('Ctrl Pts',(-89.9680202099297,22.506815589517,4.78655554679506));
#23329=CARTESIAN_POINT('Ctrl Pts',(-89.4769517287624,23.1750794839497,4.83921660187794));
#23330=CARTESIAN_POINT('Ctrl Pts',(-89.3477696362708,24.1092727525185,4.89187765696082));
#23331=CARTESIAN_POINT('Ctrl Pts',(-89.6390602159942,24.8857228049574,4.9445387120437));
#23332=CARTESIAN_POINT('Ctrl Pts',(-89.9303507957177,25.6621728573963,4.99719976712658));
#23333=CARTESIAN_POINT('Ctrl Pts',(-90.6421140476561,26.2808796937054,5.04986082220945));
#23334=CARTESIAN_POINT('Ctrl Pts',(-91.4515531900703,26.4612492047028,5.10252187729233));
#23335=CARTESIAN_POINT('Ctrl Pts',(-92.2609923324846,26.6416187157001,5.15518293237521));
#23336=CARTESIAN_POINT('Ctrl Pts',(-93.1681073653747,26.3836509013857,5.20784398745809));
#23337=CARTESIAN_POINT('Ctrl Pts',(-93.7615061404264,25.8043385680607,5.26050504254097));
#23338=CARTESIAN_POINT('Ctrl Pts',(-94.2381975681409,25.3389631158763,5.30280892752999));
#23339=CARTESIAN_POINT('Ctrl Pts',(-94.5124386983965,24.6662146256838,5.34511281251901));
#23340=CARTESIAN_POINT('Ctrl Pts',(-94.5184741887081,23.9978439082845,5.38741669750803));
#23341=CARTESIAN_POINT('Origin',(-92.,24.,5.));
#23342=CARTESIAN_POINT('',(-94.5199605075385,24.0017354236374,6.38741669750802));
#23343=CARTESIAN_POINT('',(-94.5147661754846,24.0016589575576,6.11258330249198));
#23344=CARTESIAN_POINT('',(-94.5175,24.,5.));
#23345=CARTESIAN_POINT('Ctrl Pts',(-94.5147661754846,24.0016589575576,6.11258330249198));
#23346=CARTESIAN_POINT('Ctrl Pts',(-94.5166141920307,24.3036180613248,6.09354263098009));
#23347=CARTESIAN_POINT('Ctrl Pts',(-94.4662618562805,24.604981570585,6.07450195946819));
#23348=CARTESIAN_POINT('Ctrl Pts',(-94.3609398422945,24.8857228268249,6.0554612879563));
#23349=CARTESIAN_POINT('Ctrl Pts',(-94.0696492553794,25.6621728984334,6.00280023287342));
#23350=CARTESIAN_POINT('Ctrl Pts',(-93.3578859858684,26.2808797500176,5.95013917779055));
#23351=CARTESIAN_POINT('Ctrl Pts',(-92.5484468234701,26.4612492654681,5.89747812270767));
#23352=CARTESIAN_POINT('Ctrl Pts',(-91.7390076610717,26.6416187809185,5.84481706762479));
#23353=CARTESIAN_POINT('Ctrl Pts',(-90.8318926057861,26.3836509602352,5.79215601254191));
#23354=CARTESIAN_POINT('Ctrl Pts',(-90.2384938160841,25.8043386126076,5.73949495745903));
#23355=CARTESIAN_POINT('Ctrl Pts',(-89.6450950263822,25.2250262649801,5.68683390237615));
#23356=CARTESIAN_POINT('Ctrl Pts',(-89.3654125022639,24.3243693904083,5.63417284729328));
#23357=CARTESIAN_POINT('Ctrl Pts',(-89.5262870414957,23.5108312521748,5.5815117922104));
#23358=CARTESIAN_POINT('Ctrl Pts',(-89.6871615807275,22.6972931139413,5.52885073712752));
#23359=CARTESIAN_POINT('Ctrl Pts',(-90.2885931833094,21.9708737120461,5.47618968204464));
#23360=CARTESIAN_POINT('Ctrl Pts',(-91.0578223533957,21.6610166423891,5.42352862696177));
#23361=CARTESIAN_POINT('Ctrl Pts',(-91.8270515234819,21.3511595727322,5.37086757187889));
#23362=CARTESIAN_POINT('Ctrl Pts',(-92.7640782610725,21.4578648353135,5.31820651679601));
#23363=CARTESIAN_POINT('Ctrl Pts',(-93.4439449493075,21.932739772486,5.26554546171313));
#23364=CARTESIAN_POINT('Ctrl Pts',(-94.1022041787089,22.392522279284,5.21455807530608));
#23365=CARTESIAN_POINT('Ctrl Pts',(-94.5193896768554,23.1974440773951,5.16357068889903));
#23366=CARTESIAN_POINT('Ctrl Pts',(-94.5215002261916,24.0004777596726,5.11258330249198));
#23367=CARTESIAN_POINT('Ctrl Pts',(-94.5184741887081,23.9978439082845,5.38741669750803));
#23368=CARTESIAN_POINT('Ctrl Pts',(-94.5199518449512,23.8342081285527,5.39777386760188));
#23369=CARTESIAN_POINT('Ctrl Pts',(-94.5053530710441,23.6708347555271,5.40813103769574));
#23370=CARTESIAN_POINT('Ctrl Pts',(-94.4737128974312,23.5108312642518,5.4184882077896));
#23371=CARTESIAN_POINT('Ctrl Pts',(-94.3128383621712,22.6972931461036,5.47114926287248));
#23372=CARTESIAN_POINT('Ctrl Pts',(-93.7114067744379,21.9708737621428,5.52381031795536));
#23373=CARTESIAN_POINT('Ctrl Pts',(-92.9421776233431,21.6610167001358,5.57647137303824));
#23374=CARTESIAN_POINT('Ctrl Pts',(-92.1729484722482,21.3511596381289,5.62913242812112));
#23375=CARTESIAN_POINT('Ctrl Pts',(-91.2359217577917,21.4578648980758,5.68179348320399));
#23376=CARTESIAN_POINT('Ctrl Pts',(-90.5560550863417,21.9327398235241,5.73445453828687));
#23377=CARTESIAN_POINT('Ctrl Pts',(-89.8761884148917,22.4076147489725,5.78711559336975));
#23378=CARTESIAN_POINT('Ctrl Pts',(-89.4534817864484,23.2506593399223,5.83977664845262));
#23379=CARTESIAN_POINT('Ctrl Pts',(-89.4796398709601,24.0795384869714,5.8924377035355));
#23380=CARTESIAN_POINT('Ctrl Pts',(-89.5057979554718,24.9084176340206,5.94509875861838));
#23381=CARTESIAN_POINT('Ctrl Pts',(-89.9808207529386,25.723131337169,5.99775981370126));
#23382=CARTESIAN_POINT('Ctrl Pts',(-90.6892773179196,26.1541930279687,6.05042086878414));
#23383=CARTESIAN_POINT('Ctrl Pts',(-91.3977338829005,26.5852547187684,6.10308192386702));
#23384=CARTESIAN_POINT('Ctrl Pts',(-92.3396242153956,26.6326643972193,6.15574297894989));
#23385=CARTESIAN_POINT('Ctrl Pts',(-93.0877849752844,26.2749209652664,6.20840403403277));
#23386=CARTESIAN_POINT('Ctrl Pts',(-93.8359457351732,25.9171775333136,6.26106508911565));
#23387=CARTESIAN_POINT('Ctrl Pts',(-94.3903769224557,25.154280990957,6.31372614419853));
#23388=CARTESIAN_POINT('Ctrl Pts',(-94.499634531667,24.3322179393546,6.36638719928141));
#23389=CARTESIAN_POINT('Ctrl Pts',(-94.5141780603748,24.2227912579823,6.37339703202361));
#23390=CARTESIAN_POINT('Ctrl Pts',(-94.5208336131063,24.1123162124966,6.38040686476582));
#23391=CARTESIAN_POINT('Ctrl Pts',(-94.5199605075385,24.0017354236374,6.38741669750802));
#23392=CARTESIAN_POINT('Origin',(-92.,24.,5.));
#23393=CARTESIAN_POINT('',(-94.5136288801011,24.0004946012931,7.38741669750802));
#23394=CARTESIAN_POINT('',(-94.5157924718976,23.9979483278017,7.11258330249199));
#23395=CARTESIAN_POINT('',(-94.5175,24.,5.));
#23396=CARTESIAN_POINT('Ctrl Pts',(-94.5157924718976,23.9979483278017,7.11258330249199));
#23397=CARTESIAN_POINT('Ctrl Pts',(-94.511298709256,24.5747303258767,7.07617562814403));
#23398=CARTESIAN_POINT('Ctrl Pts',(-94.3140597937548,25.1542901069194,7.03976795379607));
#23399=CARTESIAN_POINT('Ctrl Pts',(-93.9507613607754,25.5978335256406,7.00336027944811));
#23400=CARTESIAN_POINT('Ctrl Pts',(-93.4252765795229,26.2393868471104,6.95069922436523));
#23401=CARTESIAN_POINT('Ctrl Pts',(-92.552370044704,26.5963732625152,6.89803816928236));
#23402=CARTESIAN_POINT('Ctrl Pts',(-91.7279197656473,26.5068933387405,6.84537711419948));
#23403=CARTESIAN_POINT('Ctrl Pts',(-90.9034694865905,26.4174134149657,6.7927160591166));
#23404=CARTESIAN_POINT('Ctrl Pts',(-90.1274754632958,25.8814671520113,6.74005500403372));
#23405=CARTESIAN_POINT('Ctrl Pts',(-89.7518642291325,25.1421153272968,6.68739394895084));
#23406=CARTESIAN_POINT('Ctrl Pts',(-89.3762529949691,24.4027635025822,6.63473289386796));
#23407=CARTESIAN_POINT('Ctrl Pts',(-89.4010245499371,23.4600061161074,6.58207183878508));
#23408=CARTESIAN_POINT('Ctrl Pts',(-89.8149445707942,22.7413997314749,6.52941078370221));
#23409=CARTESIAN_POINT('Ctrl Pts',(-90.2288645916513,22.0227933468423,6.47674972861933));
#23410=CARTESIAN_POINT('Ctrl Pts',(-91.0319330783976,21.5283379640519,6.42408867353645));
#23411=CARTESIAN_POINT('Ctrl Pts',(-91.8599447672213,21.4822775377715,6.37142761845357));
#23412=CARTESIAN_POINT('Ctrl Pts',(-92.6879564560451,21.4362171114912,6.31876656337069));
#23413=CARTESIAN_POINT('Ctrl Pts',(-93.5409113469464,21.8385516417208,6.26610550828782));
#23414=CARTESIAN_POINT('Ctrl Pts',(-94.0319798402375,22.5068155526521,6.21344445320494));
#23415=CARTESIAN_POINT('Ctrl Pts',(-94.3454925694847,22.9334551058627,6.17982406963395));
#23416=CARTESIAN_POINT('Ctrl Pts',(-94.5115031064752,23.4684854880682,6.14620368606297));
#23417=CARTESIAN_POINT('Ctrl Pts',(-94.5147661754846,24.0016589575576,6.11258330249198));
#23418=CARTESIAN_POINT('Ctrl Pts',(-94.5199605075385,24.0017354236374,6.38741669750802));
#23419=CARTESIAN_POINT('Ctrl Pts',(-94.5142744465628,23.2815829799959,6.4330679198487));
#23420=CARTESIAN_POINT('Ctrl Pts',(-94.1892823731636,22.556945740582,6.47871914218937));
#23421=CARTESIAN_POINT('Ctrl Pts',(-93.6442302498737,22.0881819026962,6.52437036453004));
#23422=CARTESIAN_POINT('Ctrl Pts',(-93.0154843277293,21.5474384784885,6.57703141961292));
#23423=CARTESIAN_POINT('Ctrl Pts',(-92.0939084523006,21.3471811909213,6.6296924746958));
#23424=CARTESIAN_POINT('Ctrl Pts',(-91.2974530104828,21.5782301356438,6.68235352977868));
#23425=CARTESIAN_POINT('Ctrl Pts',(-90.500997568665,21.8092790803663,6.73501458486156));
#23426=CARTESIAN_POINT('Ctrl Pts',(-89.829662560458,22.4716342573785,6.78767563994443));
#23427=CARTESIAN_POINT('Ctrl Pts',(-89.5879098697311,23.2649062939185,6.84033669502731));
#23428=CARTESIAN_POINT('Ctrl Pts',(-89.3461571790042,24.0581783304585,6.89299775011019));
#23429=CARTESIAN_POINT('Ctrl Pts',(-89.5339868057573,24.9823672265264,6.94565880519307));
#23430=CARTESIAN_POINT('Ctrl Pts',(-90.0662148075274,25.6183375376923,6.99831986027595));
#23431=CARTESIAN_POINT('Ctrl Pts',(-90.5984428092974,26.2543078488581,7.05098091535882));
#23432=CARTESIAN_POINT('Ctrl Pts',(-91.4750691860844,26.602059575122,7.1036419704417));
#23433=CARTESIAN_POINT('Ctrl Pts',(-92.2985289179312,26.5038813897733,7.15630302552458));
#23434=CARTESIAN_POINT('Ctrl Pts',(-93.121988649778,26.4057032044245,7.20896408060746));
#23435=CARTESIAN_POINT('Ctrl Pts',(-93.8922817366847,25.8615951074633,7.26162513569034));
#23436=CARTESIAN_POINT('Ctrl Pts',(-94.2600671127882,25.1183193741671,7.31428619077321));
#23437=CARTESIAN_POINT('Ctrl Pts',(-94.4303151951188,24.774256568905,7.33866302635148));
#23438=CARTESIAN_POINT('Ctrl Pts',(-94.5143151353889,24.3875167213616,7.36303986192975));
#23439=CARTESIAN_POINT('Ctrl Pts',(-94.5136288801011,24.0004946012931,7.38741669750802));
#23440=CARTESIAN_POINT('Origin',(-92.,24.,5.));
#23441=CARTESIAN_POINT('',(-94.5182105203766,23.9978055611691,8.38741669750802));
#23442=CARTESIAN_POINT('',(-94.5215632327497,24.0003195913041,8.11258330249198));
#23443=CARTESIAN_POINT('',(-94.5175,24.,5.));
#23444=CARTESIAN_POINT('Ctrl Pts',(-94.5215632327497,24.0003195913041,8.11258330249198));
#23445=CARTESIAN_POINT('Ctrl Pts',(-94.5215948568411,24.0178575782261,8.11146968039084));
#23446=CARTESIAN_POINT('Ctrl Pts',(-94.521427546271,24.0353949460436,8.11035605828969));
#23447=CARTESIAN_POINT('Ctrl Pts',(-94.5210594500516,24.0529280984189,8.10924243618855));
#23448=CARTESIAN_POINT('Ctrl Pts',(-94.5036528852352,24.8820372747418,8.05658138110567));
#23449=CARTESIAN_POINT('Ctrl Pts',(-94.0372569095472,25.7017200358608,8.0039203260228));
#23450=CARTESIAN_POINT('Ctrl Pts',(-93.3333902497356,26.1402364642016,7.95125927093992));
#23451=CARTESIAN_POINT('Ctrl Pts',(-92.6295235899239,26.5787528925424,7.89859821585704));
#23452=CARTESIAN_POINT('Ctrl Pts',(-91.6881862459885,26.636102988105,7.84593716077416));
#23453=CARTESIAN_POINT('Ctrl Pts',(-90.9362906742079,26.2862774042331,7.79327610569128));
#23454=CARTESIAN_POINT('Ctrl Pts',(-90.1843951024273,25.9364518203612,7.7406150506084));
#23455=CARTESIAN_POINT('Ctrl Pts',(-89.6219413028015,25.1794505570548,7.68795399552552));
#23456=CARTESIAN_POINT('Ctrl Pts',(-89.5040117184286,24.3585866550213,7.63529294044265));
#23457=CARTESIAN_POINT('Ctrl Pts',(-89.3860821340558,23.5377227529879,7.58263188535977));
#23458=CARTESIAN_POINT('Ctrl Pts',(-89.7126767649358,22.6529962122272,7.52997083027689));
#23459=CARTESIAN_POINT('Ctrl Pts',(-90.3356793497081,22.105645593905,7.47730977519401));
#23460=CARTESIAN_POINT('Ctrl Pts',(-90.9586819344803,21.5582949755827,7.42464872011113));
#23461=CARTESIAN_POINT('Ctrl Pts',(-91.8780924731448,21.3483202796988,7.37198766502825));
#23462=CARTESIAN_POINT('Ctrl Pts',(-92.6769426067422,21.5709486259712,7.31932660994538));
#23463=CARTESIAN_POINT('Ctrl Pts',(-93.4757927403396,21.7935769722436,7.2666655548625));
#23464=CARTESIAN_POINT('Ctrl Pts',(-94.15408246887,22.4488083606723,7.21400449977962));
#23465=CARTESIAN_POINT('Ctrl Pts',(-94.4041958192921,23.2394841686541,7.16134344469675));
#23466=CARTESIAN_POINT('Ctrl Pts',(-94.4813911490268,23.4835194414908,7.14509006396183));
#23467=CARTESIAN_POINT('Ctrl Pts',(-94.517798610341,23.7404570822428,7.12883668322691));
#23468=CARTESIAN_POINT('Ctrl Pts',(-94.5157924718976,23.9979483278017,7.11258330249199));
#23469=CARTESIAN_POINT('Ctrl Pts',(-94.5136288801011,24.0004946012931,7.38741669750802));
#23470=CARTESIAN_POINT('Ctrl Pts',(-94.5128326243634,23.5514363729595,7.41570091701263));
#23471=CARTESIAN_POINT('Ctrl Pts',(-94.3980254709817,23.1019981282164,7.44398513651724));
#23472=CARTESIAN_POINT('Ctrl Pts',(-94.1716472904104,22.7184034835405,7.47226935602185));
#23473=CARTESIAN_POINT('Ctrl Pts',(-93.7501644266289,22.0042066958411,7.52493041110473));
#23474=CARTESIAN_POINT('Ctrl Pts',(-92.9419210337657,21.5182564900734,7.57759146618761));
#23475=CARTESIAN_POINT('Ctrl Pts',(-92.1134692628649,21.4809394423544,7.63025252127049));
#23476=CARTESIAN_POINT('Ctrl Pts',(-91.285017491964,21.4436223946354,7.68291357635336));
#23477=CARTESIAN_POINT('Ctrl Pts',(-90.4363573430256,21.8549385049651,7.73557463143624));
#23478=CARTESIAN_POINT('Ctrl Pts',(-89.9523707200979,22.5283491743849,7.78823568651912));
#23479=CARTESIAN_POINT('Ctrl Pts',(-89.4683840971702,23.2017598438046,7.84089674160199));
#23480=CARTESIAN_POINT('Ctrl Pts',(-89.3490710002533,24.1372650723145,7.89355779668487));
#23481=CARTESIAN_POINT('Ctrl Pts',(-89.648541866765,24.9105967084797,7.94621885176775));
#23482=CARTESIAN_POINT('Ctrl Pts',(-89.9480127332768,25.6839283446448,7.99887990685063));
#23483=CARTESIAN_POINT('Ctrl Pts',(-90.6662675632173,26.2950863884653,8.05154096193351));
#23484=CARTESIAN_POINT('Ctrl Pts',(-91.4775657136168,26.4669013906121,8.10420201701639));
#23485=CARTESIAN_POINT('Ctrl Pts',(-92.2888638640162,26.6387163927589,8.15686307209926));
#23486=CARTESIAN_POINT('Ctrl Pts',(-93.1932053348746,26.3711883532321,8.20952412718214));
#23487=CARTESIAN_POINT('Ctrl Pts',(-93.7804554676164,25.785643447789,8.26218518226502));
#23488=CARTESIAN_POINT('Ctrl Pts',(-94.2459621805259,25.3214884497798,8.30392902067936));
#23489=CARTESIAN_POINT('Ctrl Pts',(-94.5122227023915,24.6575056999379,8.34567285909369));
#23490=CARTESIAN_POINT('Ctrl Pts',(-94.5182105203766,23.9978055611691,8.38741669750802));
#23491=CARTESIAN_POINT('Origin',(-92.,24.,5.));
#23492=CARTESIAN_POINT('',(-94.5201758362126,24.0015868137836,9.38741669750803));
#23493=CARTESIAN_POINT('',(-94.5149491154365,24.0017493991467,9.11258330249198));
#23494=CARTESIAN_POINT('',(-94.5175,24.,5.));
#23495=CARTESIAN_POINT('',(-90.0865340033349,25.6359872033749,10.));
#23496=CARTESIAN_POINT('Ctrl Pts',(-94.5201758362126,24.0015868137836,9.38741669750803));
#23497=CARTESIAN_POINT('Ctrl Pts',(-94.5146934294681,23.2729074143925,9.43362796642338));
#23498=CARTESIAN_POINT('Ctrl Pts',(-94.1807323142246,22.5399684977904,9.47983923533874));
#23499=CARTESIAN_POINT('Ctrl Pts',(-93.6239878020485,22.0711234457756,9.5260505042541));
#23500=CARTESIAN_POINT('Ctrl Pts',(-92.9895375021336,21.5368408846388,9.57871155933697));
#23501=CARTESIAN_POINT('Ctrl Pts',(-92.0657754031769,21.3455168748646,9.63137261441986));
#23502=CARTESIAN_POINT('Ctrl Pts',(-91.2718707713923,21.5853895680493,9.68403366950274));
#23503=CARTESIAN_POINT('Ctrl Pts',(-90.4779661396077,21.825262261234,9.73669472458561));
#23504=CARTESIAN_POINT('Ctrl Pts',(-89.8139189749953,22.4963316573775,9.78935577966849));
#23505=CARTESIAN_POINT('Ctrl Pts',(-89.5807324199303,23.2907313838813,9.84201683475137));
#23506=CARTESIAN_POINT('Ctrl Pts',(-89.3475458648653,24.0851311103851,9.89467788983425));
#23507=CARTESIAN_POINT('Ctrl Pts',(-89.5452199193478,25.0028611672492,9.94733894491713));
#23508=CARTESIAN_POINT('Ctrl Pts',(-90.0865340033349,25.635987203375,10.));
#23509=CARTESIAN_POINT('',(-93.9171032040961,25.6385343199284,10.));
#23510=CARTESIAN_POINT('Origin',(-92.,24.,10.));
#23511=CARTESIAN_POINT('Ctrl Pts',(-93.9171116625783,25.6385402433575,10.));
#23512=CARTESIAN_POINT('Ctrl Pts',(-93.3939569207211,26.2476959894343,9.94901908464118));
#23513=CARTESIAN_POINT('Ctrl Pts',(-92.5534186715195,26.5878275437024,9.89803816928235));
#23514=CARTESIAN_POINT('Ctrl Pts',(-91.7542642292644,26.5094851289584,9.84705725392353));
#23515=CARTESIAN_POINT('Ctrl Pts',(-90.9287726544835,26.4285608421126,9.79439619884065));
#23516=CARTESIAN_POINT('Ctrl Pts',(-90.1474375442602,25.9011254113112,9.74173514375777));
#23517=CARTESIAN_POINT('Ctrl Pts',(-89.7641120845165,25.1658537236911,9.68907408867489));
#23518=CARTESIAN_POINT('Ctrl Pts',(-89.3807866247728,24.4305820360709,9.63641303359201));
#23519=CARTESIAN_POINT('Ctrl Pts',(-89.3954708155088,23.487474091632,9.58375197850914));
#23520=CARTESIAN_POINT('Ctrl Pts',(-89.8017477031856,22.764502097224,9.53109092342626));
#23521=CARTESIAN_POINT('Ctrl Pts',(-90.2080245908623,22.041530102816,9.47842986834338));
#23522=CARTESIAN_POINT('Ctrl Pts',(-91.0058941754799,21.5386940584389,9.4257688132605));
#23523=CARTESIAN_POINT('Ctrl Pts',(-91.8333902143466,21.4839130383455,9.37310775817762));
#23524=CARTESIAN_POINT('Ctrl Pts',(-92.6608862532132,21.4291320182521,9.32044670309474));
#23525=CARTESIAN_POINT('Ctrl Pts',(-93.518008746329,21.8224060224424,9.26778564801187));
#23526=CARTESIAN_POINT('Ctrl Pts',(-94.016096172441,22.4854401035393,9.21512459292899));
#23527=CARTESIAN_POINT('Ctrl Pts',(-94.3393871214709,22.9157920981482,9.18094416278332));
#23528=CARTESIAN_POINT('Ctrl Pts',(-94.5114220034557,23.4597899508602,9.14676373263765));
#23529=CARTESIAN_POINT('Ctrl Pts',(-94.5149491154365,24.0017493991467,9.11258330249198));
#23530=CARTESIAN_POINT('Origin',(-92.,24.,12.2084234471775));
#23531=CARTESIAN_POINT('',(-95.0782766400089,24.0007881209763,1.79157655282254));
#23532=CARTESIAN_POINT('',(-95.0686108047355,24.0003349297086,1.70842344717745));
#23533=CARTESIAN_POINT('',(-95.0735,24.0000000000001,12.2084234471775));
#23534=CARTESIAN_POINT('',(-91.2062007174672,21.0307770462543,0.999999999999999));
#23535=CARTESIAN_POINT('Ctrl Pts',(-95.0686108047355,24.0003349297086,1.70842344717745));
#23536=CARTESIAN_POINT('Ctrl Pts',(-95.0689532420951,24.4946153833655,1.68292651844981));
#23537=CARTESIAN_POINT('Ctrl Pts',(-94.723556593627,26.0092287415617,1.6047685346393));
#23538=CARTESIAN_POINT('Ctrl Pts',(-92.3539160917337,27.6088396578189,1.4739494957459));
#23539=CARTESIAN_POINT('Ctrl Pts',(-89.1687762982368,26.2698556568796,1.31596633049727));
#23540=CARTESIAN_POINT('Ctrl Pts',(-88.5566852567634,22.8667001441213,1.15798316524863));
#23541=CARTESIAN_POINT('Ctrl Pts',(-90.2237466982397,21.2934286920664,1.05266105508288));
#23542=CARTESIAN_POINT('Ctrl Pts',(-91.2062007174672,21.0307770462543,0.999999999999999));
#23543=CARTESIAN_POINT('',(-92.7937992825328,21.0307770462543,1.));
#23544=CARTESIAN_POINT('Origin',(-92.,24.,0.999999999999999));
#23545=CARTESIAN_POINT('Ctrl Pts',(-95.078276640009,24.0007881209763,1.79157655282254));
#23546=CARTESIAN_POINT('Ctrl Pts',(-95.0784227334426,24.0437415110921,1.78934283757203));
#23547=CARTESIAN_POINT('Ctrl Pts',(-95.0582221315001,25.0992023691253,1.73444806723864));
#23548=CARTESIAN_POINT('Ctrl Pts',(-93.8523949517843,27.1179531681002,1.62689224182237));
#23549=CARTESIAN_POINT('Ctrl Pts',(-90.40096829048,27.2555127221398,1.46890907657374));
#23550=CARTESIAN_POINT('Ctrl Pts',(-88.4000492676845,24.4393710995325,1.3109259113251));
#23551=CARTESIAN_POINT('Ctrl Pts',(-89.6506968017519,21.2605902470593,1.15462288580053));
#23552=CARTESIAN_POINT('Ctrl Pts',(-91.8480943965222,20.7745943834541,1.05098091535883));
#23553=CARTESIAN_POINT('Ctrl Pts',(-92.7957016814436,21.0256872793281,1.));
#23554=CARTESIAN_POINT('Origin',(-92.,24.,12.2084234471775));
#23555=CARTESIAN_POINT('',(-95.069948942502,24.0019027882837,2.79157655282254));
#23556=CARTESIAN_POINT('',(-95.0750082483734,23.9974244677008,2.70842344717745));
#23557=CARTESIAN_POINT('',(-95.0735,24.0000000000001,12.2084234471775));
#23558=CARTESIAN_POINT('Ctrl Pts',(-95.0750082483734,23.9974244677008,2.70842344717745));
#23559=CARTESIAN_POINT('Ctrl Pts',(-95.0676141928259,24.8239896640293,2.66555951561375));
#23560=CARTESIAN_POINT('Ctrl Pts',(-94.2993639886886,26.6781669869539,2.57003452896717));
#23561=CARTESIAN_POINT('Ctrl Pts',(-91.1738622446318,27.5314376817822,2.42184848723771));
#23562=CARTESIAN_POINT('Ctrl Pts',(-88.5910236590807,25.2380222607046,2.26386532198907));
#23563=CARTESIAN_POINT('Ctrl Pts',(-89.1003115510402,21.8216058212252,2.10588215674044));
#23564=CARTESIAN_POINT('Ctrl Pts',(-92.2395757883417,20.3812154557911,1.94789899149181));
#23565=CARTESIAN_POINT('Ctrl Pts',(-94.6902007202701,21.9256564305863,1.81541275497081));
#23566=CARTESIAN_POINT('Ctrl Pts',(-95.068245976022,23.4737343794429,1.73558757353269));
#23567=CARTESIAN_POINT('Ctrl Pts',(-95.0686108047355,24.0003349297086,1.70842344717745));
#23568=CARTESIAN_POINT('Ctrl Pts',(-95.069948942502,24.0019027882837,2.79157655282254));
#23569=CARTESIAN_POINT('Ctrl Pts',(-95.0721210057469,24.3814602607307,2.77197583473597));
#23570=CARTESIAN_POINT('Ctrl Pts',(-94.831557865169,25.7781155062161,2.69971406156651));
#23571=CARTESIAN_POINT('Ctrl Pts',(-92.7514083303166,27.5481002919865,2.57479123331418));
#23572=CARTESIAN_POINT('Ctrl Pts',(-89.4392014827729,26.568262216555,2.41680806806554));
#23573=CARTESIAN_POINT('Ctrl Pts',(-88.4497281061605,23.25891107134,2.25882490281691));
#23574=CARTESIAN_POINT('Ctrl Pts',(-90.6804688187273,20.6217765261787,2.10084173756828));
#23575=CARTESIAN_POINT('Ctrl Pts',(-94.0596141395782,21.0427206231846,1.94509228757015));
#23576=CARTESIAN_POINT('Ctrl Pts',(-95.0749785010789,23.0310919164918,1.84200389265491));
#23577=CARTESIAN_POINT('Ctrl Pts',(-95.078276640009,24.0007881209763,1.79157655282254));
#23578=CARTESIAN_POINT('Origin',(-92.,24.,12.2084234471775));
#23579=CARTESIAN_POINT('',(-95.0716996757212,23.9974284306968,3.79157655282254));
#23580=CARTESIAN_POINT('',(-95.0762204956332,24.0022328813937,3.70842344717745));
#23581=CARTESIAN_POINT('',(-95.0735,24.0000000000001,12.2084234471775));
#23582=CARTESIAN_POINT('Ctrl Pts',(-95.0762204956332,24.0022328813937,3.70842344717745));
#23583=CARTESIAN_POINT('Ctrl Pts',(-95.0774152743553,24.1480569517706,3.70085356786056));
#23584=CARTESIAN_POINT('Ctrl Pts',(-95.0019699142738,25.3070874795556,3.6406226334608));
#23585=CARTESIAN_POINT('Ctrl Pts',(-93.5299145201094,27.2883129487163,3.52773064397815));
#23586=CARTESIAN_POINT('Ctrl Pts',(-90.0822081585387,27.0782646692958,3.36974747872952));
#23587=CARTESIAN_POINT('Ctrl Pts',(-88.3740039924776,24.0761257570407,3.21176431348088));
#23588=CARTESIAN_POINT('Ctrl Pts',(-89.9547029138477,21.0049371841951,3.05378114823225));
#23589=CARTESIAN_POINT('Ctrl Pts',(-93.3905541717124,20.6503748565914,2.89579798298361));
#23590=CARTESIAN_POINT('Ctrl Pts',(-94.9751243964845,22.605903680769,2.78067874929868));
#23591=CARTESIAN_POINT('Ctrl Pts',(-95.0766982584323,23.8085019627026,2.71822057069663));
#23592=CARTESIAN_POINT('Ctrl Pts',(-95.0750082483734,23.9974244677008,2.70842344717745));
#23593=CARTESIAN_POINT('Ctrl Pts',(-95.0716996757212,23.9974284306968,3.79157655282254));
#23594=CARTESIAN_POINT('Ctrl Pts',(-95.0659413561645,24.7122593975924,3.7546088318999));
#23595=CARTESIAN_POINT('Ctrl Pts',(-94.4623933413542,26.4541466296604,3.66498005589438));
#23596=CARTESIAN_POINT('Ctrl Pts',(-91.5706310470027,27.6012890799135,3.52269022480599));
#23597=CARTESIAN_POINT('Ctrl Pts',(-88.7493847378944,25.6084593551841,3.36470705955735));
#23598=CARTESIAN_POINT('Ctrl Pts',(-88.8765574469373,22.156701935519,3.20672389430872));
#23599=CARTESIAN_POINT('Ctrl Pts',(-91.836799110436,20.3768791020246,3.04874072906008));
#23600=CARTESIAN_POINT('Ctrl Pts',(-94.5594315108872,21.6964445021905,2.91035828189803));
#23601=CARTESIAN_POINT('Ctrl Pts',(-95.0662853449471,23.3617069600934,2.82463688981885));
#23602=CARTESIAN_POINT('Ctrl Pts',(-95.069948942502,24.0019027882837,2.79157655282254));
#23603=CARTESIAN_POINT('Origin',(-92.,24.,12.2084234471775));
#23604=CARTESIAN_POINT('',(-95.0783836922344,24.0005832748178,4.79157655282255));
#23605=CARTESIAN_POINT('',(-95.0687189181701,24.0004324466973,4.70842344717745));
#23606=CARTESIAN_POINT('',(-95.0735,24.0000000000001,12.2084234471775));
#23607=CARTESIAN_POINT('Ctrl Pts',(-95.0687189181701,24.0004324466973,4.70842344717745));
#23608=CARTESIAN_POINT('Ctrl Pts',(-95.0693320714153,24.4838070199057,4.6834865650245));
#23609=CARTESIAN_POINT('Ctrl Pts',(-94.7346949951819,25.9871566204806,4.60588862778867));
#23610=CARTESIAN_POINT('Ctrl Pts',(-92.3913282534434,27.6056209517321,4.47562963546996));
#23611=CARTESIAN_POINT('Ctrl Pts',(-89.1942539711864,26.2981360810345,4.31764647022133));
#23612=CARTESIAN_POINT('Ctrl Pts',(-88.5420870968054,22.9061633512837,4.15966330497268));
#23613=CARTESIAN_POINT('Ctrl Pts',(-91.0263652646397,20.5063377831117,4.00168013972405));
#23614=CARTESIAN_POINT('Ctrl Pts',(-94.2324119925839,21.238533748243,3.85126685379231));
#23615=CARTESIAN_POINT('Ctrl Pts',(-95.0691036084142,23.1336088897796,3.75351462294344));
#23616=CARTESIAN_POINT('Ctrl Pts',(-95.0762204956332,24.0022328813937,3.70842344717745));
#23617=CARTESIAN_POINT('Ctrl Pts',(-95.0783836922344,24.0005832748178,4.79157655282255));
#23618=CARTESIAN_POINT('Ctrl Pts',(-95.0784682719039,24.0327646232159,4.78990288414672));
#23619=CARTESIAN_POINT('Ctrl Pts',(-95.0634880644544,25.0774335875127,4.73556816038801));
#23620=CARTESIAN_POINT('Ctrl Pts',(-93.8851896583918,27.0983384007903,4.62857238154643));
#23621=CARTESIAN_POINT('Ctrl Pts',(-90.4354577715253,27.2719792949116,4.47058921629779));
#23622=CARTESIAN_POINT('Ctrl Pts',(-88.4048190868975,24.4778232899584,4.31260605104916));
#23623=CARTESIAN_POINT('Ctrl Pts',(-89.6351322020287,21.2502652496794,4.15462288580053));
#23624=CARTESIAN_POINT('Ctrl Pts',(-93.0104611272249,20.5168104867762,3.99663972055189));
#23625=CARTESIAN_POINT('Ctrl Pts',(-94.8939119603259,22.3750681296892,3.8756242762259));
#23626=CARTESIAN_POINT('Ctrl Pts',(-95.0741441659616,23.693972308664,3.80726988698278));
#23627=CARTESIAN_POINT('Ctrl Pts',(-95.0716996757212,23.9974284306968,3.79157655282254));
#23628=CARTESIAN_POINT('Origin',(-92.,24.,12.2084234471775));
#23629=CARTESIAN_POINT('',(-95.0701623993453,24.0020253450063,5.79157655282255));
#23630=CARTESIAN_POINT('',(-95.0746893422024,23.9973677267576,5.70842344717746));
#23631=CARTESIAN_POINT('',(-95.0735,24.0000000000001,12.2084234471775));
#23632=CARTESIAN_POINT('Ctrl Pts',(-95.0746893422024,23.9973677267576,5.70842344717746));
#23633=CARTESIAN_POINT('Ctrl Pts',(-95.0673208895816,24.8133508051794,5.66611956218844));
#23634=CARTESIAN_POINT('Ctrl Pts',(-94.3157336914086,26.657090117177,5.57115462211653));
#23635=CARTESIAN_POINT('Ctrl Pts',(-91.2111785026033,27.5399718768618,5.42352862696177));
#23636=CARTESIAN_POINT('Ctrl Pts',(-88.6043014164073,25.2739196885051,5.26554546171313));
#23637=CARTESIAN_POINT('Ctrl Pts',(-89.0774388479143,21.8523788611612,5.1075622964645));
#23638=CARTESIAN_POINT('Ctrl Pts',(-92.2014389978195,20.3788037094653,4.94957913121586));
#23639=CARTESIAN_POINT('Ctrl Pts',(-94.6784589321776,21.9039237459708,4.81653284812018));
#23640=CARTESIAN_POINT('Ctrl Pts',(-95.0680372304395,23.4630292470767,4.73614762010738));
#23641=CARTESIAN_POINT('Ctrl Pts',(-95.0687189181701,24.0004324466973,4.70842344717745));
#23642=CARTESIAN_POINT('Ctrl Pts',(-95.0701623993453,24.0020253450063,5.79157655282255));
#23643=CARTESIAN_POINT('Ctrl Pts',(-95.0724185577781,24.3706733312739,5.77253588131065));
#23644=CARTESIAN_POINT('Ctrl Pts',(-94.8409293691539,25.7561580997578,5.70083415471588));
#23645=CARTESIAN_POINT('Ctrl Pts',(-92.7888215168717,27.5399719642595,5.57647137303824));
#23646=CARTESIAN_POINT('Ctrl Pts',(-89.466456326301,26.5951488100944,5.4184882077896));
#23647=CARTESIAN_POINT('Ctrl Pts',(-88.4421017230707,23.2964371072189,5.26050504254096));
#23648=CARTESIAN_POINT('Ctrl Pts',(-90.6448822957048,20.6358809621643,5.10252187729233));
#23649=CARTESIAN_POINT('Ctrl Pts',(-94.0404432418415,21.0225553310303,4.94621238071953));
#23650=CARTESIAN_POINT('Ctrl Pts',(-95.075807019589,23.0201963741307,4.8425639392296));
#23651=CARTESIAN_POINT('Ctrl Pts',(-95.0783836922344,24.0005832748178,4.79157655282255));
#23652=CARTESIAN_POINT('Origin',(-92.,24.,12.2084234471775));
#23653=CARTESIAN_POINT('',(-95.0714153574487,23.9974952077453,6.79157655282255));
#23654=CARTESIAN_POINT('',(-95.0765039205242,24.0021186989273,6.70842344717745));
#23655=CARTESIAN_POINT('',(-95.0735,24.0000000000001,12.2084234471775));
#23656=CARTESIAN_POINT('Ctrl Pts',(-95.0765039205242,24.0021186989273,6.70842344717745));
#23657=CARTESIAN_POINT('Ctrl Pts',(-95.0775698549681,24.1371216997451,6.70141361443525));
#23658=CARTESIAN_POINT('Ctrl Pts',(-95.00840225429,25.2852297742064,6.64174272661017));
#23659=CARTESIAN_POINT('Ctrl Pts',(-93.5645421898479,27.2719792141301,6.5294107837022));
#23660=CARTESIAN_POINT('Ctrl Pts',(-90.1148103881513,27.0983383242962,6.37142761845358));
#23661=CARTESIAN_POINT('Ctrl Pts',(-88.3750099098822,24.1143988208681,6.21344445320493));
#23662=CARTESIAN_POINT('Ctrl Pts',(-89.9231991720716,21.0266956824956,6.05546128795631));
#23663=CARTESIAN_POINT('Ctrl Pts',(-93.355117670839,20.6358810452204,5.89747812270766));
#23664=CARTESIAN_POINT('Ctrl Pts',(-94.9680494317644,22.584007681798,5.78179884244806));
#23665=CARTESIAN_POINT('Ctrl Pts',(-95.0764933447696,23.7975923269541,5.71878061727132));
#23666=CARTESIAN_POINT('Ctrl Pts',(-95.0746893422024,23.9973677267576,5.70842344717746));
#23667=CARTESIAN_POINT('Ctrl Pts',(-95.0714153574487,23.9974952077453,6.79157655282255));
#23668=CARTESIAN_POINT('Ctrl Pts',(-95.0659291292545,24.7016618298241,6.75516887847459));
#23669=CARTESIAN_POINT('Ctrl Pts',(-94.4768296167088,26.4326507862167,6.66610014904375));
#23670=CARTESIAN_POINT('Ctrl Pts',(-91.6086717368946,27.6056210407497,6.52437036453005));
#23671=CARTESIAN_POINT('Ctrl Pts',(-88.7665454640887,25.6426845888844,6.3663871992814));
#23672=CARTESIAN_POINT('Ctrl Pts',(-88.8572728216189,22.1897771481732,6.20840403403277));
#23673=CARTESIAN_POINT('Ctrl Pts',(-91.7985609972073,20.3788036200624,6.05042086878414));
#23674=CARTESIAN_POINT('Ctrl Pts',(-94.5460460301537,21.6747784855977,5.9114783750474));
#23675=CARTESIAN_POINT('Ctrl Pts',(-95.0661786684217,23.351098370438,5.82519693639353));
#23676=CARTESIAN_POINT('Ctrl Pts',(-95.0701623993453,24.0020253450063,5.79157655282255));
#23677=CARTESIAN_POINT('Origin',(-92.,24.,12.2084234471775));
#23678=CARTESIAN_POINT('',(-95.0784606140442,24.000390174329,7.79157655282255));
#23679=CARTESIAN_POINT('',(-95.0687739277024,24.0006038359779,7.70842344717745));
#23680=CARTESIAN_POINT('',(-95.0735,24.0000000000001,12.2084234471775));
#23681=CARTESIAN_POINT('Ctrl Pts',(-95.0687739277024,24.0006038359779,7.70842344717745));
#23682=CARTESIAN_POINT('Ctrl Pts',(-95.0696117452305,24.4731013478073,7.68404661159918));
#23683=CARTESIAN_POINT('Ctrl Pts',(-94.745518655979,25.9652418365262,7.60700872093803));
#23684=CARTESIAN_POINT('Ctrl Pts',(-92.4293689423973,27.6012889909868,7.47730977519402));
#23685=CARTESIAN_POINT('Ctrl Pts',(-89.2186704291244,26.3276267101463,7.31932660994537));
#23686=CARTESIAN_POINT('Ctrl Pts',(-88.5307327633938,22.9427275180138,7.16134344469675));
#23687=CARTESIAN_POINT('Ctrl Pts',(-90.9895388977222,20.516810572774,7.00336027944811));
#23688=CARTESIAN_POINT('Ctrl Pts',(-94.2151018414648,21.2177213748182,6.85238694694168));
#23689=CARTESIAN_POINT('Ctrl Pts',(-95.0695620701134,23.1229176917646,6.75407466951813));
#23690=CARTESIAN_POINT('Ctrl Pts',(-95.0765039205242,24.0021186989273,6.70842344717745));
#23691=CARTESIAN_POINT('Ctrl Pts',(-95.0784606140442,24.000390174329,7.79157655282255));
#23692=CARTESIAN_POINT('Ctrl Pts',(-95.0784992224434,24.0218014961978,7.79046293072141));
#23693=CARTESIAN_POINT('Ctrl Pts',(-95.0686358124042,25.0556766999574,7.73668825353738));
#23694=CARTESIAN_POINT('Ctrl Pts',(-93.9177918888646,27.0782647453892,7.63025252127048));
#23695=CARTESIAN_POINT('Ctrl Pts',(-90.4700854420894,27.288313029852,7.47226935602185));
#23696=CARTESIAN_POINT('Ctrl Pts',(-88.4100634919605,24.5157489192992,7.31428619077322));
#23697=CARTESIAN_POINT('Ctrl Pts',(-89.6062365978313,21.275383052732,7.15630302552458));
#23698=CARTESIAN_POINT('Ctrl Pts',(-92.9736347594024,20.5063376968639,6.99831986027594));
#23699=CARTESIAN_POINT('Ctrl Pts',(-94.8854039328386,22.3531166132715,6.87674436937527));
#23700=CARTESIAN_POINT('Ctrl Pts',(-95.0738645596358,23.6831359850142,6.80782993355747));
#23701=CARTESIAN_POINT('Ctrl Pts',(-95.0714153574487,23.9974952077453,6.79157655282255));
#23702=CARTESIAN_POINT('Origin',(-92.,24.,12.2084234471775));
#23703=CARTESIAN_POINT('',(-95.0703857423214,24.0021357609841,8.79157655282255));
#23704=CARTESIAN_POINT('',(-95.0743674416594,23.9973209105276,8.70842344717745));
#23705=CARTESIAN_POINT('',(-95.0735,24.0000000000001,12.2084234471775));
#23706=CARTESIAN_POINT('Ctrl Pts',(-95.0743674416594,23.9973209105276,8.70842344717745));
#23707=CARTESIAN_POINT('Ctrl Pts',(-95.0670571899902,24.8027184781565,8.66667960876312));
#23708=CARTESIAN_POINT('Ctrl Pts',(-94.3319128073199,26.6359725607219,8.57227471526591));
#23709=CARTESIAN_POINT('Ctrl Pts',(-91.2485916883301,27.5481002036266,8.42520876668582));
#23710=CARTESIAN_POINT('Ctrl Pts',(-88.617938794798,25.3096959362796,8.26722560143718));
#23711=CARTESIAN_POINT('Ctrl Pts',(-89.0549304174884,21.8833499742238,8.10924243618856));
#23712=CARTESIAN_POINT('Ctrl Pts',(-92.1632008855268,20.3768791915845,7.95125927093991));
#23713=CARTESIAN_POINT('Ctrl Pts',(-94.6666765768248,21.8820749507615,7.81765294126956));
#23714=CARTESIAN_POINT('Ctrl Pts',(-95.0678018156825,23.4523692918733,7.73670766668206));
#23715=CARTESIAN_POINT('Ctrl Pts',(-95.0687739277024,24.0006038359779,7.70842344717745));
#23716=CARTESIAN_POINT('Ctrl Pts',(-95.0703857423214,24.0021357609841,8.79157655282255));
#23717=CARTESIAN_POINT('Ctrl Pts',(-95.0727139521361,24.3598775376807,8.77309592788534));
#23718=CARTESIAN_POINT('Ctrl Pts',(-94.8501666541559,25.7342139358697,8.70195424786526));
#23719=CARTESIAN_POINT('Ctrl Pts',(-92.8261377777637,27.5314377737091,8.57815151276228));
#23720=CARTESIAN_POINT('Ctrl Pts',(-89.493997547754,26.6217541894133,8.42016834751367));
#23721=CARTESIAN_POINT('Ctrl Pts',(-88.4348706359932,23.3340326759415,8.26218518226501));
#23722=CARTESIAN_POINT('Ctrl Pts',(-90.6094457936036,20.6503747732117,8.10420201701639));
#23723=CARTESIAN_POINT('Ctrl Pts',(-94.0210778474872,21.0024378034505,7.94733247386889));
#23724=CARTESIAN_POINT('Ctrl Pts',(-95.0766735052339,23.0093011164261,7.84312398580429));
#23725=CARTESIAN_POINT('Ctrl Pts',(-95.0784606140442,24.000390174329,7.79157655282255));
#23726=CARTESIAN_POINT('Origin',(-92.,24.,12.2084234471775));
#23727=CARTESIAN_POINT('',(-95.0702888275776,23.9968971804147,9.79157655282255));
#23728=CARTESIAN_POINT('',(-95.076766805402,24.0019372679897,9.70842344717746));
#23729=CARTESIAN_POINT('',(-95.0735,24.0000000000001,12.2084234471775));
#23730=CARTESIAN_POINT('',(-92.7937992825329,21.0307770462543,10.));
#23731=CARTESIAN_POINT('Ctrl Pts',(-92.7937992825329,21.0307770462543,10.));
#23732=CARTESIAN_POINT('Ctrl Pts',(-93.7762533017603,21.2934286920664,9.94733894491712));
#23733=CARTESIAN_POINT('Ctrl Pts',(-94.8759105460538,22.3312191677288,9.87786446252464));
#23734=CARTESIAN_POINT('Ctrl Pts',(-95.0726356002046,23.6716361186704,9.80838998013215));
#23735=CARTESIAN_POINT('Ctrl Pts',(-95.0702888275776,23.9968971804147,9.79157655282255));
#23736=CARTESIAN_POINT('',(-91.2043027735401,21.0256991239339,10.));
#23737=CARTESIAN_POINT('Origin',(-92.,24.,10.));
#23738=CARTESIAN_POINT('Ctrl Pts',(-91.2042983602307,21.0256873161864,10.));
#23739=CARTESIAN_POINT('Ctrl Pts',(-92.1519057059922,20.7745943606123,9.94901908464117));
#23740=CARTESIAN_POINT('Ctrl Pts',(-94.2125558943073,21.2303462451956,9.85182690036699));
#23741=CARTESIAN_POINT('Ctrl Pts',(-95.0700735870785,23.1123260926059,9.75463471609281));
#23742=CARTESIAN_POINT('Ctrl Pts',(-95.076766805402,24.0019372679897,9.70842344717746));
#23743=CARTESIAN_POINT('Origin',(46.,-46.,36.));
#23744=CARTESIAN_POINT('',(39.,-46.,40.));
#23745=CARTESIAN_POINT('Origin',(46.,-46.,40.));
#23746=CARTESIAN_POINT('',(39.,-46.,32.));
#23747=CARTESIAN_POINT('',(39.,-46.,36.));
#23748=CARTESIAN_POINT('Origin',(46.,-46.,32.));
#23749=CARTESIAN_POINT('Origin',(46.,-46.,32.));
#23750=CARTESIAN_POINT('',(41.5,-46.,32.));
#23751=CARTESIAN_POINT('Origin',(46.,-46.,32.));
#23752=CARTESIAN_POINT('Origin',(-46.,-46.,36.));
#23753=CARTESIAN_POINT('',(-53.,-46.,40.));
#23754=CARTESIAN_POINT('Origin',(-46.,-46.,40.));
#23755=CARTESIAN_POINT('',(-53.,-46.,32.));
#23756=CARTESIAN_POINT('',(-53.,-46.,36.));
#23757=CARTESIAN_POINT('Origin',(-46.,-46.,32.));
#23758=CARTESIAN_POINT('Origin',(-46.,-46.,32.));
#23759=CARTESIAN_POINT('',(-50.5,-46.,32.));
#23760=CARTESIAN_POINT('Origin',(-46.,-46.,32.));
#23761=CARTESIAN_POINT('Origin',(-46.,46.,36.));
#23762=CARTESIAN_POINT('',(-53.,46.,40.));
#23763=CARTESIAN_POINT('Origin',(-46.,46.,40.));
#23764=CARTESIAN_POINT('',(-53.,46.,32.));
#23765=CARTESIAN_POINT('',(-53.,46.,36.));
#23766=CARTESIAN_POINT('Origin',(-46.,46.,32.));
#23767=CARTESIAN_POINT('Origin',(-46.,46.,32.));
#23768=CARTESIAN_POINT('',(-50.5,46.,32.));
#23769=CARTESIAN_POINT('Origin',(-46.,46.,32.));
#23770=CARTESIAN_POINT('Origin',(46.,46.,36.));
#23771=CARTESIAN_POINT('',(39.,46.,40.));
#23772=CARTESIAN_POINT('Origin',(46.,46.,40.));
#23773=CARTESIAN_POINT('',(39.,46.,32.));
#23774=CARTESIAN_POINT('',(39.,46.,36.));
#23775=CARTESIAN_POINT('Origin',(46.,46.,32.));
#23776=CARTESIAN_POINT('Origin',(46.,46.,32.));
#23777=CARTESIAN_POINT('',(41.5,46.,32.));
#23778=CARTESIAN_POINT('Origin',(46.,46.,32.));
#23779=CARTESIAN_POINT('Origin',(46.,-46.,20.));
#23780=CARTESIAN_POINT('',(41.5,-46.,0.));
#23781=CARTESIAN_POINT('',(41.5,-46.,20.));
#23782=CARTESIAN_POINT('Origin',(46.,-46.,0.));
#23783=CARTESIAN_POINT('Origin',(-46.,-46.,20.));
#23784=CARTESIAN_POINT('',(-50.5,-46.,0.));
#23785=CARTESIAN_POINT('',(-50.5,-46.,20.));
#23786=CARTESIAN_POINT('Origin',(-46.,-46.,0.));
#23787=CARTESIAN_POINT('Origin',(-46.,46.,20.));
#23788=CARTESIAN_POINT('',(-50.5,46.,0.));
#23789=CARTESIAN_POINT('',(-50.5,46.,20.));
#23790=CARTESIAN_POINT('Origin',(-46.,46.,0.));
#23791=CARTESIAN_POINT('Origin',(46.,46.,20.));
#23792=CARTESIAN_POINT('',(41.5,46.,0.));
#23793=CARTESIAN_POINT('',(41.5,46.,20.));
#23794=CARTESIAN_POINT('Origin',(46.,46.,0.));
#23795=CARTESIAN_POINT('Origin',(-92.,24.,1.));
#23796=CARTESIAN_POINT('Ctrl Pts',(-93.913465996665,25.635987203375,0.999999999999999));
#23797=CARTESIAN_POINT('Ctrl Pts',(-93.9756063047087,25.5775905725136,0.999999999999998));
#23798=CARTESIAN_POINT('Ctrl Pts',(-94.0343713138295,25.5159402489924,0.999999999999998));
#23799=CARTESIAN_POINT('Ctrl Pts',(-94.0897489850203,25.4514126613156,0.999999999999998));
#23800=CARTESIAN_POINT('Ctrl Pts',(-94.1464813764675,25.3853065162843,0.999999999999998));
#23801=CARTESIAN_POINT('Ctrl Pts',(-94.1996591403008,25.3161801193169,1.));
#23802=CARTESIAN_POINT('Ctrl Pts',(-94.2492404445121,25.2443919311763,1.));
#23803=CARTESIAN_POINT('Ctrl Pts',(-94.2621841917327,25.2256508315724,1.));
#23804=CARTESIAN_POINT('Ctrl Pts',(-94.2748826589411,25.2067281064344,0.999999999999997));
#23805=CARTESIAN_POINT('Ctrl Pts',(-94.2873347259112,25.1876296997861,0.999999999999997));
#23806=CARTESIAN_POINT('Ctrl Pts',(-94.2974956811874,25.1720452947016,0.999999999999996));
#23807=CARTESIAN_POINT('Ctrl Pts',(-94.3074930002328,25.1563430139423,1.));
#23808=CARTESIAN_POINT('Ctrl Pts',(-94.3173172477238,25.1405406475386,1.));
#23809=CARTESIAN_POINT('Ctrl Pts',(-94.3647645434793,25.0642213617018,1.));
#23810=CARTESIAN_POINT('Ctrl Pts',(-94.4082282646501,24.9854948529656,0.999999999999998));
#23811=CARTESIAN_POINT('Ctrl Pts',(-94.447673659524,24.9047536078528,0.999999999999998));
#23812=CARTESIAN_POINT('Ctrl Pts',(-94.4795145183608,24.8395781774593,0.999999999999999));
#23813=CARTESIAN_POINT('Ctrl Pts',(-94.5087365608418,24.773088868802,1.));
#23814=CARTESIAN_POINT('Ctrl Pts',(-94.5353043306397,24.7054742948633,1.));
#23815=CARTESIAN_POINT('Ctrl Pts',(-94.5460290352188,24.6781800832584,1.));
#23816=CARTESIAN_POINT('Ctrl Pts',(-94.5563210329607,24.6507023520544,0.999999999999999));
#23817=CARTESIAN_POINT('Ctrl Pts',(-94.5661772012358,24.623052941431,0.999999999999999));
#23818=CARTESIAN_POINT('Ctrl Pts',(-94.5713953813417,24.6084144327908,0.999999999999999));
#23819=CARTESIAN_POINT('Ctrl Pts',(-94.5764908417308,24.5937291306026,0.999999999999998));
#23820=CARTESIAN_POINT('Ctrl Pts',(-94.5814593622078,24.5790106095272,0.999999999999998));
#23821=CARTESIAN_POINT('Ctrl Pts',(-94.610973429931,24.4915794658263,0.999999999999998));
#23822=CARTESIAN_POINT('Ctrl Pts',(-94.6360512221953,24.4028684394346,1.));
#23823=CARTESIAN_POINT('Ctrl Pts',(-94.6566599719052,24.3132752235806,1.));
#23824=CARTESIAN_POINT('Ctrl Pts',(-94.6775876507752,24.2222955146362,1.));
#23825=CARTESIAN_POINT('Ctrl Pts',(-94.6939073964014,24.130405294356,0.999999999999997));
#23826=CARTESIAN_POINT('Ctrl Pts',(-94.7055430522835,24.037987869175,0.999999999999997));
#23827=CARTESIAN_POINT('Ctrl Pts',(-94.7170875472974,23.9462944988128,0.999999999999997));
#23828=CARTESIAN_POINT('Ctrl Pts',(-94.724021404917,23.8540812223222,0.999999999999998));
#23829=CARTESIAN_POINT('Ctrl Pts',(-94.7262232902698,23.7617032481877,0.999999999999999));
#23830=CARTESIAN_POINT('Ctrl Pts',(-94.7273184961164,23.7157549442746,0.999999999999999));
#23831=CARTESIAN_POINT('Ctrl Pts',(-94.7272422422959,23.6697656818021,1.));
#23832=CARTESIAN_POINT('Ctrl Pts',(-94.7259748077026,23.6237784781036,1.));
#23833=CARTESIAN_POINT('Ctrl Pts',(-94.7255580392477,23.6086565807406,1.));
#23834=CARTESIAN_POINT('Ctrl Pts',(-94.7250123596335,23.5935330552964,0.999999999999996));
#23835=CARTESIAN_POINT('Ctrl Pts',(-94.7243372521877,23.5784152548529,0.999999999999996));
#23836=CARTESIAN_POINT('Ctrl Pts',(-94.7200633700785,23.4827094568323,0.999999999999996));
#23837=CARTESIAN_POINT('Ctrl Pts',(-94.7106224525511,23.3875708315057,0.999999999999995));
#23838=CARTESIAN_POINT('Ctrl Pts',(-94.6959503273247,23.2933977070033,0.999999999999996));
#23839=CARTESIAN_POINT('Ctrl Pts',(-94.6917956792088,23.2667310729442,0.999999999999996));
#23840=CARTESIAN_POINT('Ctrl Pts',(-94.6872212839362,23.2401417258322,0.999999999999998));
#23841=CARTESIAN_POINT('Ctrl Pts',(-94.6822249702578,23.2136384506288,0.999999999999998));
#23842=CARTESIAN_POINT('Ctrl Pts',(-94.6652600471295,23.1236468977724,0.999999999999998));
#23843=CARTESIAN_POINT('Ctrl Pts',(-94.6434348327879,23.0346478147206,0.999999999999998));
#23844=CARTESIAN_POINT('Ctrl Pts',(-94.6170519644753,22.9468734390333,0.999999999999998));
#23845=CARTESIAN_POINT('Ctrl Pts',(-94.5900726212507,22.8571146235805,0.999999999999999));
#23846=CARTESIAN_POINT('Ctrl Pts',(-94.5583270022639,22.7686358185468,1.));
#23847=CARTESIAN_POINT('Ctrl Pts',(-94.5220844975755,22.6816890800785,0.999999999999999));
#23848=CARTESIAN_POINT('Ctrl Pts',(-94.5094176334808,22.6513009341951,0.999999999999999));
#23849=CARTESIAN_POINT('Ctrl Pts',(-94.4962010035889,22.6211000168438,0.999999999999998));
#23850=CARTESIAN_POINT('Ctrl Pts',(-94.4824446757977,22.591097444797,0.999999999999998));
#23851=CARTESIAN_POINT('Ctrl Pts',(-94.4754977537663,22.5759461971739,0.999999999999997));
#23852=CARTESIAN_POINT('Ctrl Pts',(-94.4684131849647,22.5608455360005,0.999999999999999));
#23853=CARTESIAN_POINT('Ctrl Pts',(-94.4611921986787,22.5457969186967,1.));
#23854=CARTESIAN_POINT('Ctrl Pts',(-94.4551822280867,22.5332720718318,1.));
#23855=CARTESIAN_POINT('Ctrl Pts',(-94.4490796032345,22.5207872106202,1.));
#23856=CARTESIAN_POINT('Ctrl Pts',(-94.4428889228564,22.5083503604479,1.));
#23857=CARTESIAN_POINT('Ctrl Pts',(-94.3999256375741,22.4220386936643,1.));
#23858=CARTESIAN_POINT('Ctrl Pts',(-94.3526753109166,22.3379337018791,1.));
#23859=CARTESIAN_POINT('Ctrl Pts',(-94.3014800103383,22.2562854637047,1.));
#23860=CARTESIAN_POINT('Ctrl Pts',(-94.2492799079211,22.1730347288376,1.));
#23861=CARTESIAN_POINT('Ctrl Pts',(-94.1929781399576,22.0923373565558,1.));
#23862=CARTESIAN_POINT('Ctrl Pts',(-94.1328823961135,22.0144657633818,1.));
#23863=CARTESIAN_POINT('Ctrl Pts',(-94.0723186325409,21.9359877139172,1.));
#23864=CARTESIAN_POINT('Ctrl Pts',(-94.0079011060885,21.8603787916184,0.999999999999999));
#23865=CARTESIAN_POINT('Ctrl Pts',(-93.9398956019456,21.7879374141084,0.999999999999999));
#23866=CARTESIAN_POINT('Ctrl Pts',(-93.9029689977178,21.7486021557239,0.999999999999999));
#23867=CARTESIAN_POINT('Ctrl Pts',(-93.8649836956945,21.7102012375533,1.));
#23868=CARTESIAN_POINT('Ctrl Pts',(-93.8259770071998,21.6727861926027,1.));
#23869=CARTESIAN_POINT('Ctrl Pts',(-93.8138450048983,21.6611492290723,1.));
#23870=CARTESIAN_POINT('Ctrl Pts',(-93.8016141734242,21.6496076574392,0.999999999999998));
#23871=CARTESIAN_POINT('Ctrl Pts',(-93.7892855705602,21.6381630928521,0.999999999999998));
#23872=CARTESIAN_POINT('Ctrl Pts',(-93.7779997461575,21.6276865329596,0.999999999999997));
#23873=CARTESIAN_POINT('Ctrl Pts',(-93.7666377236851,21.6172966268635,1.));
#23874=CARTESIAN_POINT('Ctrl Pts',(-93.7552049282741,21.6069982199581,1.));
#23875=CARTESIAN_POINT('Ctrl Pts',(-93.6793958597524,21.5387111032299,1.));
#23876=CARTESIAN_POINT('Ctrl Pts',(-93.6004205023376,21.4743910085569,0.999999999999999));
#23877=CARTESIAN_POINT('Ctrl Pts',(-93.5186050201243,21.4143205611548,0.999999999999999));
#23878=CARTESIAN_POINT('Ctrl Pts',(-93.436718607489,21.3541980353187,0.999999999999999));
#23879=CARTESIAN_POINT('Ctrl Pts',(-93.3519865665313,21.2983316912964,0.999999999999998));
#23880=CARTESIAN_POINT('Ctrl Pts',(-93.264690947132,21.2470310933275,0.999999999999998));
#23881=CARTESIAN_POINT('Ctrl Pts',(-93.1791590995957,21.1967670027101,0.999999999999999));
#23882=CARTESIAN_POINT('Ctrl Pts',(-93.0911655548093,21.1508853499643,0.999999999999997));
#23883=CARTESIAN_POINT('Ctrl Pts',(-93.0009418597692,21.1097134459682,0.999999999999997));
#23884=CARTESIAN_POINT('Ctrl Pts',(-92.9631524544841,21.0924689541994,0.999999999999997));
#23885=CARTESIAN_POINT('Ctrl Pts',(-92.9249714624208,21.07605118337,0.999999999999999));
#23886=CARTESIAN_POINT('Ctrl Pts',(-92.8864145036881,21.0604865582877,0.999999999999999));
#23887=CARTESIAN_POINT('Ctrl Pts',(-92.8564008056109,21.0483706660271,0.999999999999999));
#23888=CARTESIAN_POINT('Ctrl Pts',(-92.8261592741354,21.0367717663531,0.999999999999999));
#23889=CARTESIAN_POINT('Ctrl Pts',(-92.7957016814436,21.0256872793281,0.999999999999999));
#23890=CARTESIAN_POINT('Ctrl Pts',(-91.2062007174672,21.0307770462543,0.999999999999999));
#23891=CARTESIAN_POINT('Ctrl Pts',(-91.1113643609119,21.0654686091134,0.999999999999998));
#23892=CARTESIAN_POINT('Ctrl Pts',(-91.0185712349542,21.1051505773263,0.999999999999999));
#23893=CARTESIAN_POINT('Ctrl Pts',(-90.928062273623,21.1495027068259,0.999999999999997));
#23894=CARTESIAN_POINT('Ctrl Pts',(-90.8362818390432,21.1944778966871,0.999999999999996));
#23895=CARTESIAN_POINT('Ctrl Pts',(-90.7468495275144,21.244256084386,0.999999999999996));
#23896=CARTESIAN_POINT('Ctrl Pts',(-90.6600505960964,21.2985440193193,0.999999999999996));
#23897=CARTESIAN_POINT('Ctrl Pts',(-90.6355418278817,21.3138728994379,0.999999999999996));
#23898=CARTESIAN_POINT('Ctrl Pts',(-90.6112432552945,21.3295615450785,0.999999999999992));
#23899=CARTESIAN_POINT('Ctrl Pts',(-90.5871618961064,21.3456038099433,0.999999999999992));
#23900=CARTESIAN_POINT('Ctrl Pts',(-90.5678312417006,21.3584813006018,0.999999999999992));
#23901=CARTESIAN_POINT('Ctrl Pts',(-90.5486384466368,21.3715882772414,0.999999999999994));
#23902=CARTESIAN_POINT('Ctrl Pts',(-90.52960642948,21.3849077947694,0.999999999999994));
#23903=CARTESIAN_POINT('Ctrl Pts',(-90.446898789443,21.4427905642147,0.999999999999994));
#23904=CARTESIAN_POINT('Ctrl Pts',(-90.367145983118,21.5047351112166,0.999999999999995));
#23905=CARTESIAN_POINT('Ctrl Pts',(-90.2906143666657,21.570444201942,0.999999999999996));
#23906=CARTESIAN_POINT('Ctrl Pts',(-90.2316015138477,21.6211119008557,0.999999999999996));
#23907=CARTESIAN_POINT('Ctrl Pts',(-90.1745045557113,21.6740188392933,0.999999999999995));
#23908=CARTESIAN_POINT('Ctrl Pts',(-90.1194631968057,21.7290405248296,0.999999999999995));
#23909=CARTESIAN_POINT('Ctrl Pts',(-90.0901430626928,21.758350179081,0.999999999999995));
#23910=CARTESIAN_POINT('Ctrl Pts',(-90.0614065056815,21.7882600664935,0.999999999999998));
#23911=CARTESIAN_POINT('Ctrl Pts',(-90.0332766727044,21.8187522035138,0.999999999999998));
#23912=CARTESIAN_POINT('Ctrl Pts',(-90.0236426846049,21.8291952404639,0.999999999999998));
#23913=CARTESIAN_POINT('Ctrl Pts',(-90.0140806611891,21.8397057918699,0.999999999999991));
#23914=CARTESIAN_POINT('Ctrl Pts',(-90.004598089186,21.850275607196,0.999999999999991));
#23915=CARTESIAN_POINT('Ctrl Pts',(-89.9388055962019,21.9236116704984,0.999999999999992));
#23916=CARTESIAN_POINT('Ctrl Pts',(-89.8767453527984,21.9998940815955,0.999999999999998));
#23917=CARTESIAN_POINT('Ctrl Pts',(-89.8186611506175,22.0788444252834,0.999999999999997));
#23918=CARTESIAN_POINT('Ctrl Pts',(-89.7610833542944,22.1571064421111,0.999999999999997));
#23919=CARTESIAN_POINT('Ctrl Pts',(-89.7074121343123,22.2379908576831,0.999999999999994));
#23920=CARTESIAN_POINT('Ctrl Pts',(-89.6579307656577,22.32124888072,0.999999999999994));
#23921=CARTESIAN_POINT('Ctrl Pts',(-89.6098823876189,22.4020957342815,0.999999999999994));
#23922=CARTESIAN_POINT('Ctrl Pts',(-89.5657844916839,22.4851814054866,0.999999999999992));
#23923=CARTESIAN_POINT('Ctrl Pts',(-89.5259442419403,22.5702884173418,0.999999999999991));
#23924=CARTESIAN_POINT('Ctrl Pts',(-89.5051329729808,22.6147455913167,0.999999999999991));
#23925=CARTESIAN_POINT('Ctrl Pts',(-89.4854842991392,22.6597544344945,0.999999999999997));
#23926=CARTESIAN_POINT('Ctrl Pts',(-89.467047707511,22.7052841839688,0.999999999999998));
#23927=CARTESIAN_POINT('Ctrl Pts',(-89.459907033166,22.7229183064012,0.999999999999998));
#23928=CARTESIAN_POINT('Ctrl Pts',(-89.4529482256316,22.7406305682224,0.999999999999992));
#23929=CARTESIAN_POINT('Ctrl Pts',(-89.4461743286839,22.7584191729874,0.999999999999992));
#23930=CARTESIAN_POINT('Ctrl Pts',(-89.4410204433374,22.7719535432535,0.999999999999992));
#23931=CARTESIAN_POINT('Ctrl Pts',(-89.4359736405729,22.7855322273038,0.999999999999996));
#23932=CARTESIAN_POINT('Ctrl Pts',(-89.4310400913489,22.7991405298987,0.999999999999996));
#23933=CARTESIAN_POINT('Ctrl Pts',(-89.3993682456114,22.886501583972,0.999999999999995));
#23934=CARTESIAN_POINT('Ctrl Pts',(-89.3723051104949,22.9752235793332,0.999999999999994));
#23935=CARTESIAN_POINT('Ctrl Pts',(-89.3501019718364,23.0650831124335,0.999999999999994));
#23936=CARTESIAN_POINT('Ctrl Pts',(-89.3450993726547,23.0853294043503,0.999999999999994));
#23937=CARTESIAN_POINT('Ctrl Pts',(-89.3403436950579,23.1056334830589,0.999999999999995));
#23938=CARTESIAN_POINT('Ctrl Pts',(-89.3358381789014,23.1259928495363,0.999999999999995));
#23939=CARTESIAN_POINT('Ctrl Pts',(-89.3154926547755,23.2179294817595,0.999999999999994));
#23940=CARTESIAN_POINT('Ctrl Pts',(-89.3002441342108,23.3109938333353,0.999999999999996));
#23941=CARTESIAN_POINT('Ctrl Pts',(-89.2899827069896,23.4047941591632,0.999999999999996));
#23942=CARTESIAN_POINT('Ctrl Pts',(-89.2792695744502,23.5027235505786,0.999999999999997));
#23943=CARTESIAN_POINT('Ctrl Pts',(-89.2739922714095,23.6014563765805,0.999999999999995));
#23944=CARTESIAN_POINT('Ctrl Pts',(-89.2740832157028,23.7005321536448,0.999999999999995));
#23945=CARTESIAN_POINT('Ctrl Pts',(-89.2741183389869,23.7387958702845,0.999999999999995));
#23946=CARTESIAN_POINT('Ctrl Pts',(-89.2749547528147,23.7771104872619,0.999999999999996));
#23947=CARTESIAN_POINT('Ctrl Pts',(-89.2765906985078,23.8154482999531,0.999999999999996));
#23948=CARTESIAN_POINT('Ctrl Pts',(-89.2771783035686,23.8292186181587,0.999999999999996));
#23949=CARTESIAN_POINT('Ctrl Pts',(-89.2778690508017,23.8429901308395,0.999999999999995));
#23950=CARTESIAN_POINT('Ctrl Pts',(-89.2786619686985,23.8567498857267,0.999999999999995));
#23951=CARTESIAN_POINT('Ctrl Pts',(-89.2840135874435,23.9496182173429,0.999999999999995));
#23952=CARTESIAN_POINT('Ctrl Pts',(-89.2940209180062,24.0420994637446,0.999999999999996));
#23953=CARTESIAN_POINT('Ctrl Pts',(-89.3085609026807,24.1338217237738,0.999999999999996));
#23954=CARTESIAN_POINT('Ctrl Pts',(-89.3230638385443,24.2253102696181,0.999999999999996));
#23955=CARTESIAN_POINT('Ctrl Pts',(-89.3420767704053,24.3160446363436,0.999999999999993));
#23956=CARTESIAN_POINT('Ctrl Pts',(-89.365526168021,24.4056386468464,0.999999999999993));
#23957=CARTESIAN_POINT('Ctrl Pts',(-89.3885742626434,24.4936993836513,0.999999999999993));
#23958=CARTESIAN_POINT('Ctrl Pts',(-89.4159087427651,24.5806592446879,0.999999999999998));
#23959=CARTESIAN_POINT('Ctrl Pts',(-89.447500123989,24.6661223199297,0.999999999999999));
#23960=CARTESIAN_POINT('Ctrl Pts',(-89.463362608983,24.7090345540909,0.999999999999999));
#23961=CARTESIAN_POINT('Ctrl Pts',(-89.4802989345948,24.7515688848954,0.999999999999997));
#23962=CARTESIAN_POINT('Ctrl Pts',(-89.4983087570542,24.7936714134035,0.999999999999997));
#23963=CARTESIAN_POINT('Ctrl Pts',(-89.5036080710629,24.8060599041634,0.999999999999997));
#23964=CARTESIAN_POINT('Ctrl Pts',(-89.5090003430761,24.8184109903508,0.999999999999998));
#23965=CARTESIAN_POINT('Ctrl Pts',(-89.5144855988184,24.8307232500462,0.999999999999998));
#23966=CARTESIAN_POINT('Ctrl Pts',(-89.520079028009,24.8432783169417,0.999999999999998));
#23967=CARTESIAN_POINT('Ctrl Pts',(-89.5257654644254,24.8557847223552,0.999999999999995));
#23968=CARTESIAN_POINT('Ctrl Pts',(-89.5315436189995,24.868239131147,0.999999999999995));
#23969=CARTESIAN_POINT('Ctrl Pts',(-89.5690290042182,24.9490362620044,0.999999999999995));
#23970=CARTESIAN_POINT('Ctrl Pts',(-89.6103840908339,25.0276765323043,0.999999999999998));
#23971=CARTESIAN_POINT('Ctrl Pts',(-89.655539055121,25.1038122347855,0.999999999999997));
#23972=CARTESIAN_POINT('Ctrl Pts',(-89.6999358276934,25.1786695516068,0.999999999999997));
#23973=CARTESIAN_POINT('Ctrl Pts',(-89.7480063970585,25.2511063717929,0.999999999999996));
#23974=CARTESIAN_POINT('Ctrl Pts',(-89.7997205985195,25.3207580282558,0.999999999999995));
#23975=CARTESIAN_POINT('Ctrl Pts',(-89.8498548445873,25.3882817100587,0.999999999999994));
#23976=CARTESIAN_POINT('Ctrl Pts',(-89.9034139287439,25.4531882520902,0.999999999999991));
#23977=CARTESIAN_POINT('Ctrl Pts',(-89.9603980590403,25.5151051167182,0.999999999999991));
#23978=CARTESIAN_POINT('Ctrl Pts',(-89.9815871896822,25.5381284484197,0.999999999999991));
#23979=CARTESIAN_POINT('Ctrl Pts',(-90.0032501397509,25.560737964521,0.999999999999995));
#23980=CARTESIAN_POINT('Ctrl Pts',(-90.025387758703,25.5829128445691,0.999999999999995));
#23981=CARTESIAN_POINT('Ctrl Pts',(-90.0442145502047,25.6017713245233,0.999999999999995));
#23982=CARTESIAN_POINT('Ctrl Pts',(-90.0633846686702,25.6203154277105,0.999999999999994));
#23983=CARTESIAN_POINT('Ctrl Pts',(-90.0828883826537,25.638540237813,0.999999999999994));
#23984=CARTESIAN_POINT('Origin',(-92.,24.,12.2084234471775));
#23985=CARTESIAN_POINT('Ctrl Pts',(-95.076766805402,24.0019372679897,9.70842344717746));
#23986=CARTESIAN_POINT('Ctrl Pts',(-95.0777009893786,24.1261018275903,9.70197366100994));
#23987=CARTESIAN_POINT('Ctrl Pts',(-95.0146667615987,25.2631137100916,9.64286281975954));
#23988=CARTESIAN_POINT('Ctrl Pts',(-93.5990316467515,27.2555126958586,9.53109092342626));
#23989=CARTESIAN_POINT('Ctrl Pts',(-90.1476051047097,27.1179530605299,9.37310775817762));
#23990=CARTESIAN_POINT('Ctrl Pts',(-88.3764282219687,24.1527149914234,9.215124592929));
#23991=CARTESIAN_POINT('Ctrl Pts',(-89.8919231533181,21.0487577497888,9.05714142768035));
#23992=CARTESIAN_POINT('Ctrl Pts',(-93.3195311476575,20.6217766146216,8.89915826243173));
#23993=CARTESIAN_POINT('Ctrl Pts',(-94.9608439554881,22.5621019356809,8.78291893559742));
#23994=CARTESIAN_POINT('Ctrl Pts',(-95.0762792831289,23.7866862376245,8.719340663846));
#23995=CARTESIAN_POINT('Ctrl Pts',(-95.0743674416594,23.9973209105276,8.70842344717745));
#23996=CARTESIAN_POINT('Ctrl Pts',(-95.0702888275776,23.9968971804147,9.79157655282255));
#23997=CARTESIAN_POINT('Ctrl Pts',(-95.0652853128242,24.6903808619892,9.75572892504928));
#23998=CARTESIAN_POINT('Ctrl Pts',(-94.4922439119073,26.4123573994234,9.66722024219312));
#23999=CARTESIAN_POINT('Ctrl Pts',(-91.6460838986403,27.6088399383518,9.5260505042541));
#24000=CARTESIAN_POINT('Ctrl Pts',(-88.7843955634606,25.6770749374766,9.36806733900546));
#24001=CARTESIAN_POINT('Ctrl Pts',(-88.8381773234134,22.2228835564639,9.21008417375683));
#24002=CARTESIAN_POINT('Ctrl Pts',(-91.7604241972829,20.3812153351416,9.05210100850819));
#24003=CARTESIAN_POINT('Ctrl Pts',(-94.5324622678489,21.6531111499586,8.91259846819676));
#24004=CARTESIAN_POINT('Ctrl Pts',(-95.0660796534741,23.3404823888654,8.82575698296822));
#24005=CARTESIAN_POINT('Ctrl Pts',(-95.0703857423214,24.0021357609841,8.79157655282255));
#24006=CARTESIAN_POINT('Ctrl Pts',(-90.0865340033349,25.635987203375,10.));
#24007=CARTESIAN_POINT('Ctrl Pts',(-89.5452199193478,25.0028611672492,9.94733894491712));
#24008=CARTESIAN_POINT('Ctrl Pts',(-89.1498718103828,23.1674010535211,9.84201683475136));
#24009=CARTESIAN_POINT('Ctrl Pts',(-91.1420133042202,21.1541928650905,9.68403366950274));
#24010=CARTESIAN_POINT('Ctrl Pts',(-93.9132996010903,21.7281648944129,9.52605050425409));
#24011=CARTESIAN_POINT('Ctrl Pts',(-94.9487151037096,24.3598882319117,9.36806733900547));
#24012=CARTESIAN_POINT('Ctrl Pts',(-93.3097648188374,26.6665863711808,9.21008417375682));
#24013=CARTESIAN_POINT('Ctrl Pts',(-90.4827056616583,26.5539114461962,9.0521010085082));
#24014=CARTESIAN_POINT('Ctrl Pts',(-89.0319368956585,24.1250886581775,8.89411784325956));
#24015=CARTESIAN_POINT('Ctrl Pts',(-90.2732768955517,21.5826411697067,8.73613467801092));
#24016=CARTESIAN_POINT('Ctrl Pts',(-93.0808263101442,21.2329014567463,8.57815151276229));
#24017=CARTESIAN_POINT('Ctrl Pts',(-94.9080231896089,23.3929749996272,8.42016834751365));
#24018=CARTESIAN_POINT('Ctrl Pts',(-94.097546805733,26.1036603137053,8.26218518226502));
#24019=CARTESIAN_POINT('Ctrl Pts',(-91.3845223931578,26.9062444322857,8.10420201701639));
#24020=CARTESIAN_POINT('Ctrl Pts',(-89.2297579033363,25.0727703008244,7.94621885176775));
#24021=CARTESIAN_POINT('Ctrl Pts',(-89.5876971940872,22.2662546152947,7.78823568651911));
#24022=CARTESIAN_POINT('Ctrl Pts',(-92.1336776409025,21.0323062843058,7.63025252127049));
#24023=CARTESIAN_POINT('Ctrl Pts',(-94.5584078194921,22.4901569016088,7.47226935602184));
#24024=CARTESIAN_POINT('Ctrl Pts',(-94.6625748235914,25.317487010502,7.31428619077322));
#24025=CARTESIAN_POINT('Ctrl Pts',(-92.3516955628713,26.9498113013858,7.15630302552458));
#24026=CARTESIAN_POINT('Ctrl Pts',(-89.7218164325105,25.9065561225943,6.99831986027595));
#24027=CARTESIAN_POINT('Ctrl Pts',(-89.1583275522511,23.1339894343907,6.84033669502731));
#24028=CARTESIAN_POINT('Ctrl Pts',(-91.1723325768719,21.146923903354,6.68235352977868));
#24029=CARTESIAN_POINT('Ctrl Pts',(-93.9370602031581,21.7476957660557,6.52437036453004));
#24030=CARTESIAN_POINT('Ctrl Pts',(-94.9448081097382,24.3913844486004,6.36638719928141));
#24031=CARTESIAN_POINT('Ctrl Pts',(-93.2815145478907,26.6800740756702,6.20840403403277));
#24032=CARTESIAN_POINT('Ctrl Pts',(-90.4558435504055,26.5378450403175,6.05042086878414));
#24033=CARTESIAN_POINT('Ctrl Pts',(-89.0307751580049,24.0937039308721,5.8924377035355));
#24034=CARTESIAN_POINT('Ctrl Pts',(-90.2988950433351,21.5645701580227,5.73445453828688));
#24035=CARTESIAN_POINT('Ctrl Pts',(-93.1099751867047,21.244454378182,5.57647137303824));
#24036=CARTESIAN_POINT('Ctrl Pts',(-94.9142699499044,23.4237125300644,5.4184882077896));
#24037=CARTESIAN_POINT('Ctrl Pts',(-94.0752223982648,26.1256830870713,5.26050504254097));
#24038=CARTESIAN_POINT('Ctrl Pts',(-91.3538772995945,26.8995865300145,5.10252187729233));
#24039=CARTESIAN_POINT('Ctrl Pts',(-89.2185875437792,25.0434660210873,4.9445387120437));
#24040=CARTESIAN_POINT('Ctrl Pts',(-89.606133821254,22.2408862153809,4.78655554679506));
#24041=CARTESIAN_POINT('Ctrl Pts',(-92.1649984307826,21.0338826544913,4.62857238154643));
#24042=CARTESIAN_POINT('Ctrl Pts',(-94.5742038315407,22.5172487662402,4.47058921629779));
#24043=CARTESIAN_POINT('Ctrl Pts',(-94.6485184946103,25.3455208558373,4.31260605104916));
#24044=CARTESIAN_POINT('Ctrl Pts',(-92.3205364822007,26.9533596050059,4.15462288580053));
#24045=CARTESIAN_POINT('Ctrl Pts',(-89.7018169423985,25.88240038523,3.99663972055189));
#24046=CARTESIAN_POINT('Ctrl Pts',(-89.1676278725255,23.1040397712239,3.83865655530326));
#24047=CARTESIAN_POINT('Ctrl Pts',(-91.2024970078837,21.1383456544603,3.68067339005462));
#24048=CARTESIAN_POINT('Ctrl Pts',(-93.9607285557694,21.768269726576,3.52269022480599));
#24049=CARTESIAN_POINT('Ctrl Pts',(-94.9405124242392,24.4224492832982,3.36470705955735));
#24050=CARTESIAN_POINT('Ctrl Pts',(-93.253151066984,26.6934530172094,3.20672389430872));
#24051=CARTESIAN_POINT('Ctrl Pts',(-90.4291391049686,26.5214027346518,3.04874072906008));
#24052=CARTESIAN_POINT('Ctrl Pts',(-89.029951212319,24.0623545122336,2.89075756381145));
#24053=CARTESIAN_POINT('Ctrl Pts',(-90.3246997187609,21.5467477993204,2.73277439856281));
#24054=CARTESIAN_POINT('Ctrl Pts',(-93.139001180181,21.2563262409204,2.57479123331418));
#24055=CARTESIAN_POINT('Ctrl Pts',(-94.9201929246499,23.4545070114807,2.41680806806555));
#24056=CARTESIAN_POINT('Ctrl Pts',(-94.0526634178927,26.1474755214497,2.25882490281691));
#24057=CARTESIAN_POINT('Ctrl Pts',(-91.3233115994341,26.8925961815151,2.10084173756828));
#24058=CARTESIAN_POINT('Ctrl Pts',(-89.2077117493852,25.0140624829424,1.94285857231964));
#24059=CARTESIAN_POINT('Ctrl Pts',(-89.6248688237332,22.215680056917,1.78487540707101));
#24060=CARTESIAN_POINT('Ctrl Pts',(-92.1962362281275,21.0358581128856,1.62689224182237));
#24061=CARTESIAN_POINT('Ctrl Pts',(-94.5898449391916,22.5443661358106,1.46890907657374));
#24062=CARTESIAN_POINT('Ctrl Pts',(-94.6338974915196,25.3736900328969,1.3109259113251));
#24063=CARTESIAN_POINT('Ctrl Pts',(-92.2898922274085,26.9559960431297,1.15294274607647));
#24064=CARTESIAN_POINT('Ctrl Pts',(-89.6809482123999,25.85923592523,0.994959580827835));
#24065=CARTESIAN_POINT('Ctrl Pts',(-89.1795852070609,23.0717155076705,0.836976415579201));
#24066=CARTESIAN_POINT('Ctrl Pts',(-90.5450731455404,21.7830508320407,0.731654305413444));
#24067=CARTESIAN_POINT('Ctrl Pts',(-91.3498000020249,21.5679131979649,0.678993250330566));
#24068=CARTESIAN_POINT('Ctrl Pts',(-89.9456684496579,25.7564253212269,10.1070022498898));
#24069=CARTESIAN_POINT('Ctrl Pts',(-89.3645039014938,25.0766898079629,10.0543411948069));
#24070=CARTESIAN_POINT('Ctrl Pts',(-88.9400510525638,23.1061067782159,9.94901908464118));
#24071=CARTESIAN_POINT('Ctrl Pts',(-91.0788500334022,20.9446902147086,9.79103591939254));
#24072=CARTESIAN_POINT('Ctrl Pts',(-94.0541529050566,21.5609169210655,9.63305275414391));
#24073=CARTESIAN_POINT('Ctrl Pts',(-95.1657936336881,24.3863824863894,9.47506958889527));
#24074=CARTESIAN_POINT('Ctrl Pts',(-93.4061870948087,26.8628951460734,9.31708642364664));
#24075=CARTESIAN_POINT('Ctrl Pts',(-90.3710054760088,26.7419253176407,9.159103258398));
#24076=CARTESIAN_POINT('Ctrl Pts',(-88.8134340044285,24.1342974359261,9.00112009314937));
#24077=CARTESIAN_POINT('Ctrl Pts',(-90.1461589814738,21.4046800297341,8.84313692790073));
#24078=CARTESIAN_POINT('Ctrl Pts',(-93.1603945893153,21.0291931760381,8.68515376265211));
#24079=CARTESIAN_POINT('Ctrl Pts',(-95.1221060619588,23.3482870287292,8.52717059740345));
#24080=CARTESIAN_POINT('Ctrl Pts',(-94.2519640217524,26.2585275939992,8.36918743215484));
#24081=CARTESIAN_POINT('Ctrl Pts',(-91.3392121582154,27.120196356066,8.21120426690619));
#24082=CARTESIAN_POINT('Ctrl Pts',(-89.0258182004901,25.1517455126428,8.05322110165757));
#24083=CARTESIAN_POINT('Ctrl Pts',(-89.4101082685543,22.1386197349377,7.89523793640893));
#24084=CARTESIAN_POINT('Ctrl Pts',(-92.1435187224439,20.813830586732,7.73725477116029));
#24085=CARTESIAN_POINT('Ctrl Pts',(-94.7467527049787,22.3790052613962,7.57927160591167));
#24086=CARTESIAN_POINT('Ctrl Pts',(-94.8585882763444,25.4144777788355,7.42128844066302));
#24087=CARTESIAN_POINT('Ctrl Pts',(-92.37758668938,27.1669705312528,7.2633052754144));
#24088=CARTESIAN_POINT('Ctrl Pts',(-89.5541010980484,26.0469129851116,7.10532211016575));
#24089=CARTESIAN_POINT('Ctrl Pts',(-88.9491292892987,23.0702354622651,6.94733894491712));
#24090=CARTESIAN_POINT('Ctrl Pts',(-91.1114013504886,20.936886126494,6.78935577966849));
#24091=CARTESIAN_POINT('Ctrl Pts',(-94.0796627153006,21.5818856165592,6.63137261441985));
#24092=CARTESIAN_POINT('Ctrl Pts',(-95.1615990146061,24.4201973917876,6.47338944917122));
#24093=CARTESIAN_POINT('Ctrl Pts',(-93.3758570952098,26.8773757884902,6.31540628392258));
#24094=CARTESIAN_POINT('Ctrl Pts',(-90.342165829654,26.724676134977,6.15742311867395));
#24095=CARTESIAN_POINT('Ctrl Pts',(-88.8121867419641,24.1006022275375,5.99943995342532));
#24096=CARTESIAN_POINT('Ctrl Pts',(-90.1736630862473,21.3852786661803,5.84145678817668));
#24097=CARTESIAN_POINT('Ctrl Pts',(-93.1916893480828,21.0415966005281,5.68347362292805));
#24098=CARTESIAN_POINT('Ctrl Pts',(-95.1288126962993,23.3812873949059,5.52549045767941));
#24099=CARTESIAN_POINT('Ctrl Pts',(-94.2279961358928,26.2821716400553,5.36750729243078));
#24100=CARTESIAN_POINT('Ctrl Pts',(-91.3063110339307,27.1130483122969,5.20952412718214));
#24101=CARTESIAN_POINT('Ctrl Pts',(-89.013825501322,25.1202839102265,5.05154096193351));
#24102=CARTESIAN_POINT('Ctrl Pts',(-89.429902163474,22.1113837639744,4.89355779668487));
#24103=CARTESIAN_POINT('Ctrl Pts',(-92.1771452864616,20.8155230061493,4.73557463143624));
#24104=CARTESIAN_POINT('Ctrl Pts',(-94.7637115879574,22.4080915751154,4.5775914661876));
#24105=CARTESIAN_POINT('Ctrl Pts',(-94.8434971484341,25.4445754200009,4.41960830093897));
#24106=CARTESIAN_POINT('Ctrl Pts',(-92.3441337392816,27.1707800539146,4.26162513569034));
#24107=CARTESIAN_POINT('Ctrl Pts',(-89.5326292853278,26.0209789504981,4.1036419704417));
#24108=CARTESIAN_POINT('Ctrl Pts',(-88.9591142806189,23.0380809645772,3.94565880519306));
#24109=CARTESIAN_POINT('Ctrl Pts',(-91.1437864268022,20.9276763640107,3.78767563994443));
#24110=CARTESIAN_POINT('Ctrl Pts',(-94.1050734848669,21.6039741910548,3.6296924746958));
#24111=CARTESIAN_POINT('Ctrl Pts',(-95.1569870893007,24.4535491577124,3.47170930944716));
#24112=CARTESIAN_POINT('Ctrl Pts',(-93.3454055513592,26.891739661045,3.31372614419853));
#24113=CARTESIAN_POINT('Ctrl Pts',(-90.3134954561586,26.7070233795331,3.15574297894989));
#24114=CARTESIAN_POINT('Ctrl Pts',(-88.8113021390385,24.0669449271692,2.99775981370126));
#24115=CARTESIAN_POINT('Ctrl Pts',(-90.2013674504565,21.3661442609453,2.83977664845262));
#24116=CARTESIAN_POINT('Ctrl Pts',(-93.2228521773582,21.0543424461441,2.68179348320399));
#24117=CARTESIAN_POINT('Ctrl Pts',(-95.1351717086425,23.4143489046794,2.52381031795536));
#24118=CARTESIAN_POINT('Ctrl Pts',(-94.2037764083394,26.3055683900265,2.36582715270672));
#24119=CARTESIAN_POINT('Ctrl Pts',(-91.2734951478333,27.1055433482708,2.20784398745809));
#24120=CARTESIAN_POINT('Ctrl Pts',(-89.0021490526171,25.0887157421965,2.04986082220945));
#24121=CARTESIAN_POINT('Ctrl Pts',(-89.4500163995022,22.084321978353,1.89187765696082));
#24122=CARTESIAN_POINT('Ctrl Pts',(-92.2106827481989,20.8176438938541,1.73389449171218));
#24123=CARTESIAN_POINT('Ctrl Pts',(-94.7805041627852,22.4372052713963,1.57591132646355));
#24124=CARTESIAN_POINT('Ctrl Pts',(-94.8277997762312,25.4748183557424,1.41792816121491));
#24125=CARTESIAN_POINT('Ctrl Pts',(-92.3112335155169,27.1736105813594,1.25994499596628));
#24126=CARTESIAN_POINT('Ctrl Pts',(-89.5102242410121,25.9961091691131,1.10196183071765));
#24127=CARTESIAN_POINT('Ctrl Pts',(-88.9719518902951,23.0033770531541,0.943978665469011));
#24128=CARTESIAN_POINT('Ctrl Pts',(-90.4379643297735,21.6198434520492,0.838656555303255));
#24129=CARTESIAN_POINT('Ctrl Pts',(-91.301933573839,21.3888678140614,0.785995500220377));
#24130=CARTESIAN_POINT('Ctrl Pts',(-89.8048028959809,25.8768634390788,10.2140044997796));
#24131=CARTESIAN_POINT('Ctrl Pts',(-89.1837878836397,25.1505184486767,10.1613434446967));
#24132=CARTESIAN_POINT('Ctrl Pts',(-88.730230294745,23.0448125029107,10.056021334531));
#24133=CARTESIAN_POINT('Ctrl Pts',(-91.0156867625841,20.7351875643266,9.89803816928236));
#24134=CARTESIAN_POINT('Ctrl Pts',(-94.1950062090231,21.3936689477181,9.74005500403371));
#24135=CARTESIAN_POINT('Ctrl Pts',(-95.3828721636666,24.4128767408671,9.58207183878509));
#24136=CARTESIAN_POINT('Ctrl Pts',(-93.5026093707802,27.059203920966,9.42408867353644));
#24137=CARTESIAN_POINT('Ctrl Pts',(-90.2593052903592,26.9299391890853,9.26610550828783));
#24138=CARTESIAN_POINT('Ctrl Pts',(-88.5949311131987,24.1435062136747,9.10812234303918));
#24139=CARTESIAN_POINT('Ctrl Pts',(-90.0190410673959,21.2267188897615,8.95013917779055));
#24140=CARTESIAN_POINT('Ctrl Pts',(-93.2399628684865,20.8254848953298,8.79215601254191));
#24141=CARTESIAN_POINT('Ctrl Pts',(-95.3361889343087,23.3035990578312,8.63417284729328));
#24142=CARTESIAN_POINT('Ctrl Pts',(-94.406381237772,26.4133948742932,8.47618968204464));
#24143=CARTESIAN_POINT('Ctrl Pts',(-91.2939019232727,27.3341482798463,8.31820651679601));
#24144=CARTESIAN_POINT('Ctrl Pts',(-88.821878497644,25.2307207244612,8.16022335154738));
#24145=CARTESIAN_POINT('Ctrl Pts',(-89.2325193430214,22.0109848545807,8.00224018629873));
#24146=CARTESIAN_POINT('Ctrl Pts',(-92.1533598039853,20.5953548891583,7.84425702105011));
#24147=CARTESIAN_POINT('Ctrl Pts',(-94.9350975904653,22.2678536211836,7.68627385580147));
#24148=CARTESIAN_POINT('Ctrl Pts',(-95.0546017290973,25.5114685471691,7.52829069055284));
#24149=CARTESIAN_POINT('Ctrl Pts',(-92.4034778158887,27.3841297611198,7.3703075253042));
#24150=CARTESIAN_POINT('Ctrl Pts',(-89.3863857635864,26.187269847629,7.21232436005557));
#24151=CARTESIAN_POINT('Ctrl Pts',(-88.7399310263462,23.0064814901395,7.05434119480693));
#24152=CARTESIAN_POINT('Ctrl Pts',(-91.0504701241054,20.726848349634,6.8963580295583));
#24153=CARTESIAN_POINT('Ctrl Pts',(-94.222265227443,21.4160754670626,6.73837486430966));
#24154=CARTESIAN_POINT('Ctrl Pts',(-95.378389919474,24.4490103349749,6.58039169906103));
#24155=CARTESIAN_POINT('Ctrl Pts',(-93.4701996425288,27.0746775013101,6.42240853381239));
#24156=CARTESIAN_POINT('Ctrl Pts',(-90.2284881089026,26.9115072296366,6.26442536856376));
#24157=CARTESIAN_POINT('Ctrl Pts',(-88.5935983259232,24.1075005242028,6.10644220331512));
#24158=CARTESIAN_POINT('Ctrl Pts',(-90.0484311291595,21.2059871743379,5.9484590380665));
#24159=CARTESIAN_POINT('Ctrl Pts',(-93.2734035094609,20.8387388228742,5.79047587281786));
#24160=CARTESIAN_POINT('Ctrl Pts',(-95.3433554426941,23.3388622597475,5.63249270756922));
#24161=CARTESIAN_POINT('Ctrl Pts',(-94.3807698735207,26.4386601930393,5.47450954232059));
#24162=CARTESIAN_POINT('Ctrl Pts',(-91.2587447682671,27.3265100945794,5.31652637707196));
#24163=CARTESIAN_POINT('Ctrl Pts',(-88.8090634588646,25.1971017993658,5.15854321182332));
#24164=CARTESIAN_POINT('Ctrl Pts',(-89.2536705056942,21.9818813125678,5.00056004657468));
#24165=CARTESIAN_POINT('Ctrl Pts',(-92.1892921421405,20.5971633578073,4.84257688132605));
#24166=CARTESIAN_POINT('Ctrl Pts',(-94.953219344374,22.2989343839906,4.68459371607741));
#24167=CARTESIAN_POINT('Ctrl Pts',(-95.0384758022577,25.5436299841645,4.52661055082878));
#24168=CARTESIAN_POINT('Ctrl Pts',(-92.3677309963625,27.3882005028234,4.36862738558015));
#24169=CARTESIAN_POINT('Ctrl Pts',(-89.3634416282571,26.1595575157663,4.21064422033151));
#24170=CARTESIAN_POINT('Ctrl Pts',(-88.7506006887122,22.9721221579304,4.05266105508288));
#24171=CARTESIAN_POINT('Ctrl Pts',(-91.085075845721,20.7170070735612,3.89467788983424));
#24172=CARTESIAN_POINT('Ctrl Pts',(-94.2494184139642,21.4396786555336,3.73669472458561));
#24173=CARTESIAN_POINT('Ctrl Pts',(-95.3734617543622,24.4846490321267,3.57871155933697));
#24174=CARTESIAN_POINT('Ctrl Pts',(-93.4376600357343,27.0900263048807,3.42072839408834));
#24175=CARTESIAN_POINT('Ctrl Pts',(-90.1978518073486,26.8926440244145,3.26274522883971));
#24176=CARTESIAN_POINT('Ctrl Pts',(-88.5926530657581,24.071535342105,3.10476206359107));
#24177=CARTESIAN_POINT('Ctrl Pts',(-90.0780351821522,21.1855407225702,2.94677889834244));
#24178=CARTESIAN_POINT('Ctrl Pts',(-93.3067031745353,20.8523586513677,2.7887957330938));
#24179=CARTESIAN_POINT('Ctrl Pts',(-95.3501504926354,23.3741907978781,2.63081256784517));
#24180=CARTESIAN_POINT('Ctrl Pts',(-94.354889398786,26.4636612586033,2.47282940259653));
#24181=CARTESIAN_POINT('Ctrl Pts',(-91.2236786962326,27.3184905150265,2.3148462373479));
#24182=CARTESIAN_POINT('Ctrl Pts',(-88.7965863558489,25.1633690014505,2.15686307209926));
#24183=CARTESIAN_POINT('Ctrl Pts',(-89.2751639752712,21.9529638997891,1.99887990685063));
#24184=CARTESIAN_POINT('Ctrl Pts',(-92.2251292682703,20.5994296748226,1.84089674160199));
#24185=CARTESIAN_POINT('Ctrl Pts',(-94.9711633863787,22.3300444069819,1.68291357635336));
#24186=CARTESIAN_POINT('Ctrl Pts',(-95.021702060943,25.5759466785879,1.52493041110472));
#24187=CARTESIAN_POINT('Ctrl Pts',(-92.3325748036253,27.3912251195891,1.36694724585609));
#24188=CARTESIAN_POINT('Ctrl Pts',(-89.3395002696244,26.1329824129964,1.20896408060746));
#24189=CARTESIAN_POINT('Ctrl Pts',(-88.7643185735293,22.9350385986377,1.05098091535882));
#24190=CARTESIAN_POINT('Ctrl Pts',(-90.3308555140066,21.4566360720578,0.945658805193066));
#24191=CARTESIAN_POINT('Ctrl Pts',(-91.2540671456531,21.2098224301578,0.892997750110188));
#24192=CARTESIAN_POINT('Ctrl Pts',(-89.6639373423039,25.9973015569307,10.3210067496694));
#24193=CARTESIAN_POINT('Ctrl Pts',(-89.0030718657857,25.2243470893904,10.2683456945866));
#24194=CARTESIAN_POINT('Ctrl Pts',(-88.520409536926,22.9835182276056,10.1630235844208));
#24195=CARTESIAN_POINT('Ctrl Pts',(-90.9525234917661,20.5256849139446,10.0050404191722));
#24196=CARTESIAN_POINT('Ctrl Pts',(-94.3358595129894,21.2264209743707,9.84705725392353));
#24197=CARTESIAN_POINT('Ctrl Pts',(-95.5999506936451,24.4393709953448,9.6890740886749));
#24198=CARTESIAN_POINT('Ctrl Pts',(-93.5990316467515,27.2555126958586,9.53109092342626));
#24199=CARTESIAN_POINT('Ctrl Pts',(-90.1476051047097,27.1179530605299,9.37310775817762));
#24200=CARTESIAN_POINT('Ctrl Pts',(-88.3764282219687,24.1527149914234,9.215124592929));
#24201=CARTESIAN_POINT('Ctrl Pts',(-89.8919231533181,21.0487577497888,9.05714142768035));
#24202=CARTESIAN_POINT('Ctrl Pts',(-93.3195311476575,20.6217766146216,8.89915826243173));
#24203=CARTESIAN_POINT('Ctrl Pts',(-95.5502718066587,23.2589110869331,8.74117509718308));
#24204=CARTESIAN_POINT('Ctrl Pts',(-94.5607984537914,26.5682621545871,8.58319193193445));
#24205=CARTESIAN_POINT('Ctrl Pts',(-91.2485916883301,27.5481002036266,8.42520876668582));
#24206=CARTESIAN_POINT('Ctrl Pts',(-88.617938794798,25.3096959362796,8.26722560143718));
#24207=CARTESIAN_POINT('Ctrl Pts',(-89.0549304174884,21.8833499742238,8.10924243618856));
#24208=CARTESIAN_POINT('Ctrl Pts',(-92.1632008855268,20.3768791915845,7.95125927093991));
#24209=CARTESIAN_POINT('Ctrl Pts',(-95.1234424759519,22.156701980971,7.79327610569129));
#24210=CARTESIAN_POINT('Ctrl Pts',(-95.2506151818503,25.6084593155026,7.63529294044264));
#24211=CARTESIAN_POINT('Ctrl Pts',(-92.4293689423973,27.6012889909868,7.47730977519402));
#24212=CARTESIAN_POINT('Ctrl Pts',(-89.2186704291244,26.3276267101463,7.31932660994537));
#24213=CARTESIAN_POINT('Ctrl Pts',(-88.5307327633938,22.9427275180138,7.16134344469675));
#24214=CARTESIAN_POINT('Ctrl Pts',(-90.9895388977222,20.516810572774,7.00336027944811));
#24215=CARTESIAN_POINT('Ctrl Pts',(-94.3648677395855,21.250265317566,6.84537711419948));
#24216=CARTESIAN_POINT('Ctrl Pts',(-95.5951808243418,24.4778232781622,6.68739394895084));
#24217=CARTESIAN_POINT('Ctrl Pts',(-93.5645421898479,27.2719792141301,6.5294107837022));
#24218=CARTESIAN_POINT('Ctrl Pts',(-90.1148103881513,27.0983383242962,6.37142761845358));
#24219=CARTESIAN_POINT('Ctrl Pts',(-88.3750099098822,24.1143988208681,6.21344445320493));
#24220=CARTESIAN_POINT('Ctrl Pts',(-89.9231991720716,21.0266956824956,6.05546128795631));
#24221=CARTESIAN_POINT('Ctrl Pts',(-93.355117670839,20.6358810452204,5.89747812270766));
#24222=CARTESIAN_POINT('Ctrl Pts',(-95.5578981890889,23.2964371245891,5.73949495745904));
#24223=CARTESIAN_POINT('Ctrl Pts',(-94.5335436111488,26.5951487460233,5.58151179221039));
#24224=CARTESIAN_POINT('Ctrl Pts',(-91.2111785026033,27.5399718768618,5.42352862696177));
#24225=CARTESIAN_POINT('Ctrl Pts',(-88.6043014164073,25.2739196885051,5.26554546171313));
#24226=CARTESIAN_POINT('Ctrl Pts',(-89.0774388479143,21.8523788611612,5.1075622964645));
#24227=CARTESIAN_POINT('Ctrl Pts',(-92.2014389978195,20.3788037094653,4.94957913121586));
#24228=CARTESIAN_POINT('Ctrl Pts',(-95.1427271007907,22.1897771928657,4.79159596596723));
#24229=CARTESIAN_POINT('Ctrl Pts',(-95.2334544560814,25.6426845483281,4.63361280071859));
#24230=CARTESIAN_POINT('Ctrl Pts',(-92.3913282534434,27.6056209517321,4.47562963546996));
#24231=CARTESIAN_POINT('Ctrl Pts',(-89.1942539711864,26.2981360810345,4.31764647022133));
#24232=CARTESIAN_POINT('Ctrl Pts',(-88.5420870968054,22.9061633512837,4.15966330497268));
#24233=CARTESIAN_POINT('Ctrl Pts',(-91.0263652646397,20.5063377831117,4.00168013972405));
#24234=CARTESIAN_POINT('Ctrl Pts',(-94.3937633430615,21.2753831200124,3.84369697447542));
#24235=CARTESIAN_POINT('Ctrl Pts',(-95.5899364194238,24.515748906541,3.68571380922679));
#24236=CARTESIAN_POINT('Ctrl Pts',(-93.5299145201094,27.2883129487163,3.52773064397815));
#24237=CARTESIAN_POINT('Ctrl Pts',(-90.0822081585387,27.0782646692958,3.36974747872952));
#24238=CARTESIAN_POINT('Ctrl Pts',(-88.3740039924776,24.0761257570407,3.21176431348088));
#24239=CARTESIAN_POINT('Ctrl Pts',(-89.9547029138477,21.0049371841951,3.05378114823225));
#24240=CARTESIAN_POINT('Ctrl Pts',(-93.3905541717124,20.6503748565914,2.89579798298361));
#24241=CARTESIAN_POINT('Ctrl Pts',(-95.5651292766281,23.3340326910768,2.73781481773498));
#24242=CARTESIAN_POINT('Ctrl Pts',(-94.5060023892326,26.6217541271801,2.57983165248634));
#24243=CARTESIAN_POINT('Ctrl Pts',(-91.1738622446318,27.5314376817822,2.42184848723771));
#24244=CARTESIAN_POINT('Ctrl Pts',(-88.5910236590807,25.2380222607046,2.26386532198907));
#24245=CARTESIAN_POINT('Ctrl Pts',(-89.1003115510402,21.8216058212252,2.10588215674044));
#24246=CARTESIAN_POINT('Ctrl Pts',(-92.2395757883417,20.3812154557911,1.94789899149181));
#24247=CARTESIAN_POINT('Ctrl Pts',(-95.1618226099723,22.2228835425676,1.78991582624317));
#24248=CARTESIAN_POINT('Ctrl Pts',(-95.2156043456547,25.6770750014334,1.63193266099454));
#24249=CARTESIAN_POINT('Ctrl Pts',(-92.3539160917337,27.6088396578189,1.4739494957459));
#24250=CARTESIAN_POINT('Ctrl Pts',(-89.1687762982368,26.2698556568796,1.31596633049727));
#24251=CARTESIAN_POINT('Ctrl Pts',(-88.5566852567634,22.8667001441213,1.15798316524863));
#24252=CARTESIAN_POINT('Ctrl Pts',(-90.2237466982397,21.2934286920664,1.05266105508288));
#24253=CARTESIAN_POINT('Ctrl Pts',(-91.2062007174672,21.0307770462543,0.999999999999999));
#24254=CARTESIAN_POINT('Ctrl Pts',(-90.0865340033349,25.635987203375,10.));
#24255=CARTESIAN_POINT('Ctrl Pts',(-90.0249228618548,25.5780878591452,10.));
#24256=CARTESIAN_POINT('Ctrl Pts',(-89.9666808203251,25.517037957366,10.));
#24257=CARTESIAN_POINT('Ctrl Pts',(-89.9118055510373,25.4532222734424,10.));
#24258=CARTESIAN_POINT('Ctrl Pts',(-89.8554775805255,25.3877172106174,10.));
#24259=CARTESIAN_POINT('Ctrl Pts',(-89.8026965604115,25.3192975596955,10.));
#24260=CARTESIAN_POINT('Ctrl Pts',(-89.7534854803736,25.2483309191671,10.));
#24261=CARTESIAN_POINT('Ctrl Pts',(-89.7029129709014,25.1754009794549,10.));
#24262=CARTESIAN_POINT('Ctrl Pts',(-89.6561101247971,25.0997806200714,10.));
#24263=CARTESIAN_POINT('Ctrl Pts',(-89.6131359910394,25.0218257865711,10.));
#24264=CARTESIAN_POINT('Ctrl Pts',(-89.5942445812189,24.9875568769186,10.));
#24265=CARTESIAN_POINT('Ctrl Pts',(-89.576093545669,24.9528363378472,10.));
#24266=CARTESIAN_POINT('Ctrl Pts',(-89.5586903184073,24.9176923367854,10.));
#24267=CARTESIAN_POINT('Ctrl Pts',(-89.5487652975608,24.8976497930708,10.));
#24268=CARTESIAN_POINT('Ctrl Pts',(-89.5390835217552,24.8774695021065,10.));
#24269=CARTESIAN_POINT('Ctrl Pts',(-89.5296466035421,24.8571565405449,10.));
#24270=CARTESIAN_POINT('Ctrl Pts',(-89.5211295714255,24.8388236333292,10.));
#24271=CARTESIAN_POINT('Ctrl Pts',(-89.5128096038927,24.8203769113042,10.));
#24272=CARTESIAN_POINT('Ctrl Pts',(-89.5047015810792,24.8018519373589,10.));
#24273=CARTESIAN_POINT('Ctrl Pts',(-89.4681367628098,24.7183097074791,10.));
#24274=CARTESIAN_POINT('Ctrl Pts',(-89.4358322656984,24.6330839820791,10.));
#24275=CARTESIAN_POINT('Ctrl Pts',(-89.4078131930617,24.5465734751462,10.));
#24276=CARTESIAN_POINT('Ctrl Pts',(-89.3793314409182,24.4586344184821,10.));
#24277=CARTESIAN_POINT('Ctrl Pts',(-89.3552773189935,24.3693670436557,10.));
#24278=CARTESIAN_POINT('Ctrl Pts',(-89.3357162704087,24.2791530221529,10.));
#24279=CARTESIAN_POINT('Ctrl Pts',(-89.3167358111661,24.1916166331482,10.));
#24280=CARTESIAN_POINT('Ctrl Pts',(-89.3019855060178,24.1031880412207,10.));
#24281=CARTESIAN_POINT('Ctrl Pts',(-89.2915659618403,24.0141940291817,10.));
#24282=CARTESIAN_POINT('Ctrl Pts',(-89.2872066009748,23.9769604413456,10.));
#24283=CARTESIAN_POINT('Ctrl Pts',(-89.2836058304791,23.9396276882538,10.));
#24284=CARTESIAN_POINT('Ctrl Pts',(-89.2807733396434,23.9022190875751,10.));
#24285=CARTESIAN_POINT('Ctrl Pts',(-89.2790027503762,23.8788349812521,10.));
#24286=CARTESIAN_POINT('Ctrl Pts',(-89.2775323941369,23.855421232113,10.));
#24287=CARTESIAN_POINT('Ctrl Pts',(-89.2763649279049,23.831983503391,10.));
#24288=CARTESIAN_POINT('Ctrl Pts',(-89.2756806561512,23.8182462531842,10.));
#24289=CARTESIAN_POINT('Ctrl Pts',(-89.2751007108949,23.8045053337837,10.));
#24290=CARTESIAN_POINT('Ctrl Pts',(-89.2746256143469,23.7907701196614,10.));
#24291=CARTESIAN_POINT('Ctrl Pts',(-89.2712677542697,23.6936931626774,10.));
#24292=CARTESIAN_POINT('Ctrl Pts',(-89.2731370867512,23.5967807432359,10.));
#24293=CARTESIAN_POINT('Ctrl Pts',(-89.2802984098264,23.5004551183685,10.));
#24294=CARTESIAN_POINT('Ctrl Pts',(-89.2874597329016,23.4041294935012,10.));
#24295=CARTESIAN_POINT('Ctrl Pts',(-89.2999126116991,23.3083896086995,10.));
#24296=CARTESIAN_POINT('Ctrl Pts',(-89.3177747368199,23.2136387821642,10.));
#24297=CARTESIAN_POINT('Ctrl Pts',(-89.3348522432755,23.1230500173402,10.));
#24298=CARTESIAN_POINT('Ctrl Pts',(-89.3568741021772,23.0333643557258,10.));
#24299=CARTESIAN_POINT('Ctrl Pts',(-89.3835656166833,22.944821137573,10.));
#24300=CARTESIAN_POINT('Ctrl Pts',(-89.3925004778798,22.9151817042656,10.));
#24301=CARTESIAN_POINT('Ctrl Pts',(-89.4019590305019,22.8856703233237,10.));
#24302=CARTESIAN_POINT('Ctrl Pts',(-89.4119322462713,22.8562961512496,10.));
#24303=CARTESIAN_POINT('Ctrl Pts',(-89.4184134249044,22.8372070970455,10.));
#24304=CARTESIAN_POINT('Ctrl Pts',(-89.4251119666747,22.8181759907911,10.));
#24305=CARTESIAN_POINT('Ctrl Pts',(-89.4320255302053,22.7992053804625,10.));
#24306=CARTESIAN_POINT('Ctrl Pts',(-89.4386151870788,22.7811235602558,10.));
#24307=CARTESIAN_POINT('Ctrl Pts',(-89.4454019414807,22.7630924900219,10.));
#24308=CARTESIAN_POINT('Ctrl Pts',(-89.4523729733375,22.7451415275117,10.));
#24309=CARTESIAN_POINT('Ctrl Pts',(-89.4862164573599,22.657991859374,10.));
#24310=CARTESIAN_POINT('Ctrl Pts',(-89.5244382857894,22.5726164812725,10.));
#24311=CARTESIAN_POINT('Ctrl Pts',(-89.5667072739698,22.4892490087878,10.));
#24312=CARTESIAN_POINT('Ctrl Pts',(-89.6105455323263,22.4027864518486,10.));
#24313=CARTESIAN_POINT('Ctrl Pts',(-89.6587371595254,22.3184829337952,10.));
#24314=CARTESIAN_POINT('Ctrl Pts',(-89.7109686726718,22.2366020740164,10.));
#24315=CARTESIAN_POINT('Ctrl Pts',(-89.7637886184407,22.1537987563926,10.));
#24316=CARTESIAN_POINT('Ctrl Pts',(-89.8207403974939,22.0734721714026,10.));
#24317=CARTESIAN_POINT('Ctrl Pts',(-89.8815515974396,21.9959097943086,10.));
#24318=CARTESIAN_POINT('Ctrl Pts',(-89.9232140421765,21.9427709275831,10.));
#24319=CARTESIAN_POINT('Ctrl Pts',(-89.9666890946139,21.8909298240417,10.));
#24320=CARTESIAN_POINT('Ctrl Pts',(-90.0119013664328,21.8404859713398,10.));
#24321=CARTESIAN_POINT('Ctrl Pts',(-90.0240086331394,21.8269777543492,10.));
#24322=CARTESIAN_POINT('Ctrl Pts',(-90.0362418078457,21.8135685183995,10.));
#24323=CARTESIAN_POINT('Ctrl Pts',(-90.0485858239554,21.8002746718516,10.));
#24324=CARTESIAN_POINT('Ctrl Pts',(-90.1172467100136,21.7263305620101,10.));
#24325=CARTESIAN_POINT('Ctrl Pts',(-90.1894214870782,21.6558543370425,10.));
#24326=CARTESIAN_POINT('Ctrl Pts',(-90.2647996929718,21.5891358088469,10.));
#24327=CARTESIAN_POINT('Ctrl Pts',(-90.3277046150347,21.5334575956746,10.));
#24328=CARTESIAN_POINT('Ctrl Pts',(-90.3928415834859,21.4803963685471,10.));
#24329=CARTESIAN_POINT('Ctrl Pts',(-90.4600538268301,21.4301343333567,10.));
#24330=CARTESIAN_POINT('Ctrl Pts',(-90.4819361316924,21.4137705114946,10.));
#24331=CARTESIAN_POINT('Ctrl Pts',(-90.5040385613939,21.3977035152968,10.));
#24332=CARTESIAN_POINT('Ctrl Pts',(-90.5263561317875,21.3819400181443,10.));
#24333=CARTESIAN_POINT('Ctrl Pts',(-90.5491248911564,21.3658578341455,10.));
#24334=CARTESIAN_POINT('Ctrl Pts',(-90.5721229921494,21.3500881169477,10.));
#24335=CARTESIAN_POINT('Ctrl Pts',(-90.5953160059198,21.3346571799234,10.));
#24336=CARTESIAN_POINT('Ctrl Pts',(-90.6802613708273,21.2781407396983,10.));
#24337=CARTESIAN_POINT('Ctrl Pts',(-90.7678730040975,21.2261247337397,10.));
#24338=CARTESIAN_POINT('Ctrl Pts',(-90.8578606394009,21.1789172289357,10.));
#24339=CARTESIAN_POINT('Ctrl Pts',(-90.9411343062963,21.1352318713112,10.));
#24340=CARTESIAN_POINT('Ctrl Pts',(-91.026443472184,21.0956640032536,10.));
#24341=CARTESIAN_POINT('Ctrl Pts',(-91.1135855312338,21.060486601523,10.));
#24342=CARTESIAN_POINT('Ctrl Pts',(-91.14360948864,21.0483665664592,10.));
#24343=CARTESIAN_POINT('Ctrl Pts',(-91.1738512261799,21.0367679981665,10.));
#24344=CARTESIAN_POINT('Ctrl Pts',(-91.2042983602307,21.0256873161864,10.));
#24345=CARTESIAN_POINT('Ctrl Pts',(-94.5182105203766,23.9978055611691,8.38741669750802));
#24346=CARTESIAN_POINT('Ctrl Pts',(-94.5197765073294,23.8252749644444,8.39833391417657));
#24347=CARTESIAN_POINT('Ctrl Pts',(-94.5035405383448,23.6530372868482,8.40925113084511));
#24348=CARTESIAN_POINT('Ctrl Pts',(-94.4684109790521,23.4847436281601,8.42016834751366));
#24349=CARTESIAN_POINT('Ctrl Pts',(-94.2989575631206,22.6729504853336,8.47282940259653));
#24350=CARTESIAN_POINT('Ctrl Pts',(-93.6898919366324,21.95292597104,8.52549045767941));
#24351=CARTESIAN_POINT('Ctrl Pts',(-92.9174342209562,21.6512036660532,8.57815151276229));
#24352=CARTESIAN_POINT('Ctrl Pts',(-92.14497650528,21.3494813610665,8.63081256784517));
#24353=CARTESIAN_POINT('Ctrl Pts',(-91.2091267004159,21.4660612653866,8.68347362292805));
#24354=CARTESIAN_POINT('Ctrl Pts',(-90.5343117980016,21.9480924656251,8.73613467801092));
#24355=CARTESIAN_POINT('Ctrl Pts',(-89.8594968955873,22.4301236658636,8.7887957330938));
#24356=CARTESIAN_POINT('Ctrl Pts',(-89.4457168956229,23.2776061620205,8.84145678817668));
#24357=CARTESIAN_POINT('Ctrl Pts',(-89.480621689974,24.1061512081021,8.89411784325956));
#24358=CARTESIAN_POINT('Ctrl Pts',(-89.5155264843251,24.9346962541837,8.94677889834244));
#24359=CARTESIAN_POINT('Ctrl Pts',(-89.9991160729917,25.7443038501899,8.99943995342532));
#24360=CARTESIAN_POINT('Ctrl Pts',(-90.7120873935215,26.1678868023572,9.0521010085082));
#24361=CARTESIAN_POINT('Ctrl Pts',(-91.4250587140513,26.5914697545244,9.10476206359107));
#24362=CARTESIAN_POINT('Ctrl Pts',(-92.3674117664443,26.6290280628526,9.15742311867395));
#24363=CARTESIAN_POINT('Ctrl Pts',(-93.1117466734529,26.2633575271385,9.21008417375683));
#24364=CARTESIAN_POINT('Ctrl Pts',(-93.8560815804615,25.8976869914244,9.2627452288397));
#24365=CARTESIAN_POINT('Ctrl Pts',(-94.4023983420855,25.128787611668,9.31540628392259));
#24366=CARTESIAN_POINT('Ctrl Pts',(-94.502987472461,24.3057173655401,9.36806733900547));
#24367=CARTESIAN_POINT('Ctrl Pts',(-94.5153073620014,24.2049099077324,9.37451712517299));
#24368=CARTESIAN_POINT('Ctrl Pts',(-94.5209410251377,24.1032898490186,9.38096691134051));
#24369=CARTESIAN_POINT('Ctrl Pts',(-94.5201758362126,24.0015868137836,9.38741669750803));
#24370=CARTESIAN_POINT('Ctrl Pts',(-92.7937992825329,21.0307770462543,10.));
#24371=CARTESIAN_POINT('Ctrl Pts',(-93.7762533017603,21.2934286920664,9.94733894491712));
#24372=CARTESIAN_POINT('Ctrl Pts',(-95.443314608871,22.8667010511062,9.84201683475137));
#24373=CARTESIAN_POINT('Ctrl Pts',(-94.8312238178928,26.2698553838415,9.68403366950273));
#24374=CARTESIAN_POINT('Ctrl Pts',(-91.6460838986403,27.6088399383518,9.5260505042541));
#24375=CARTESIAN_POINT('Ctrl Pts',(-88.7843955634606,25.6770749374766,9.36806733900546));
#24376=CARTESIAN_POINT('Ctrl Pts',(-88.8381773234134,22.2228835564639,9.21008417375683));
#24377=CARTESIAN_POINT('Ctrl Pts',(-91.7604241972829,20.3812153351416,9.05210100850819));
#24378=CARTESIAN_POINT('Ctrl Pts',(-94.8996885260907,21.8216057842524,8.89411784325956));
#24379=CARTESIAN_POINT('Ctrl Pts',(-95.4089764216849,25.2380222823144,8.73613467801093));
#24380=CARTESIAN_POINT('Ctrl Pts',(-92.8261377777637,27.5314377737091,8.57815151276228));
#24381=CARTESIAN_POINT('Ctrl Pts',(-89.493997547754,26.6217541894133,8.42016834751367));
#24382=CARTESIAN_POINT('Ctrl Pts',(-88.4348706359932,23.3340326759415,8.26218518226501));
#24383=CARTESIAN_POINT('Ctrl Pts',(-90.6094457936036,20.6503747732117,8.10420201701639));
#24384=CARTESIAN_POINT('Ctrl Pts',(-94.0452971368402,21.0049371106047,7.94621885176775));
#24385=CARTESIAN_POINT('Ctrl Pts',(-95.6259960969404,24.0761257587368,7.78823568651912));
#24386=CARTESIAN_POINT('Ctrl Pts',(-93.9177918888646,27.0782647453892,7.63025252127048));
#24387=CARTESIAN_POINT('Ctrl Pts',(-90.4700854420894,27.288313029852,7.47226935602185));
#24388=CARTESIAN_POINT('Ctrl Pts',(-88.4100634919605,24.5157489192992,7.31428619077322));
#24389=CARTESIAN_POINT('Ctrl Pts',(-89.6062365978313,21.275383052732,7.15630302552458));
#24390=CARTESIAN_POINT('Ctrl Pts',(-92.9736347594024,20.5063376968639,6.99831986027594));
#24391=CARTESIAN_POINT('Ctrl Pts',(-95.4579129885642,22.9061633242749,6.84033669502732));
#24392=CARTESIAN_POINT('Ctrl Pts',(-94.8057460980851,26.2981361377744,6.68235352977867));
#24393=CARTESIAN_POINT('Ctrl Pts',(-91.6086717368946,27.6056210407497,6.52437036453005));
#24394=CARTESIAN_POINT('Ctrl Pts',(-88.7665454640887,25.6426845888844,6.3663871992814));
#24395=CARTESIAN_POINT('Ctrl Pts',(-88.8572728216189,22.1897771481732,6.20840403403277));
#24396=CARTESIAN_POINT('Ctrl Pts',(-91.7985609972073,20.3788036200624,6.05042086878414));
#24397=CARTESIAN_POINT('Ctrl Pts',(-94.9225612242403,21.852378808139,5.8924377035355));
#24398=CARTESIAN_POINT('Ctrl Pts',(-95.3956986674282,25.2739197199567,5.73445453828687));
#24399=CARTESIAN_POINT('Ctrl Pts',(-92.7888215168717,27.5399719642595,5.57647137303824));
#24400=CARTESIAN_POINT('Ctrl Pts',(-89.466456326301,26.5951488100944,5.4184882077896));
#24401=CARTESIAN_POINT('Ctrl Pts',(-88.4421017230707,23.2964371072189,5.26050504254096));
#24402=CARTESIAN_POINT('Ctrl Pts',(-90.6448822957048,20.6358809621643,5.10252187729233));
#24403=CARTESIAN_POINT('Ctrl Pts',(-94.0768008792021,21.0266956090883,4.9445387120437));
#24404=CARTESIAN_POINT('Ctrl Pts',(-95.6249901796143,24.1143988236926,4.78655554679506));
#24405=CARTESIAN_POINT('Ctrl Pts',(-93.8851896583918,27.0983384007903,4.62857238154643));
#24406=CARTESIAN_POINT('Ctrl Pts',(-90.4354577715253,27.2719792949116,4.47058921629779));
#24407=CARTESIAN_POINT('Ctrl Pts',(-88.4048190868975,24.4778232899584,4.31260605104916));
#24408=CARTESIAN_POINT('Ctrl Pts',(-89.6351322020287,21.2502652496794,4.15462288580053));
#24409=CARTESIAN_POINT('Ctrl Pts',(-93.0104611272249,20.5168104867762,3.99663972055189));
#24410=CARTESIAN_POINT('Ctrl Pts',(-95.4692673222584,22.9427274919151,3.83865655530326));
#24411=CARTESIAN_POINT('Ctrl Pts',(-94.7813296395429,26.3276267676048,3.68067339005461));
#24412=CARTESIAN_POINT('Ctrl Pts',(-91.5706310470027,27.6012890799135,3.52269022480599));
#24413=CARTESIAN_POINT('Ctrl Pts',(-88.7493847378944,25.6084593551841,3.36470705955735));
#24414=CARTESIAN_POINT('Ctrl Pts',(-88.8765574469373,22.156701935519,3.20672389430872));
#24415=CARTESIAN_POINT('Ctrl Pts',(-91.836799110436,20.3768791020246,3.04874072906008));
#24416=CARTESIAN_POINT('Ctrl Pts',(-94.9450696552403,21.883349922176,2.89075756381145));
#24417=CARTESIAN_POINT('Ctrl Pts',(-95.3820612886587,25.3096959682138,2.73277439856281));
#24418=CARTESIAN_POINT('Ctrl Pts',(-92.7514083303166,27.5481002919865,2.57479123331418));
#24419=CARTESIAN_POINT('Ctrl Pts',(-89.4392014827729,26.568262216555,2.41680806806554));
#24420=CARTESIAN_POINT('Ctrl Pts',(-88.4497281061605,23.25891107134,2.25882490281691));
#24421=CARTESIAN_POINT('Ctrl Pts',(-90.6804688187273,20.6217765261787,2.10084173756828));
#24422=CARTESIAN_POINT('Ctrl Pts',(-94.1080769010003,21.0487576862311,1.94285857231964));
#24423=CARTESIAN_POINT('Ctrl Pts',(-95.6235718625379,24.1527149782027,1.78487540707101));
#24424=CARTESIAN_POINT('Ctrl Pts',(-93.8523949517843,27.1179531681002,1.62689224182237));
#24425=CARTESIAN_POINT('Ctrl Pts',(-90.40096829048,27.2555127221398,1.46890907657374));
#24426=CARTESIAN_POINT('Ctrl Pts',(-88.4000492676845,24.4393710995325,1.3109259113251));
#24427=CARTESIAN_POINT('Ctrl Pts',(-89.6641403201721,21.2264207486355,1.15294274607647));
#24428=CARTESIAN_POINT('Ctrl Pts',(-93.0474767585969,20.5256850731752,0.994959580827836));
#24429=CARTESIAN_POINT('Ctrl Pts',(-95.479589838589,22.9835175562679,0.8369764155792));
#24430=CARTESIAN_POINT('Ctrl Pts',(-94.9969281342143,25.2243470893905,0.731654305413444));
#24431=CARTESIAN_POINT('Ctrl Pts',(-94.3360626576961,25.9973015569307,0.678993250330566));
#24432=CARTESIAN_POINT('Ctrl Pts',(-92.7459328543469,21.2098224301578,10.1070022498898));
#24433=CARTESIAN_POINT('Ctrl Pts',(-93.6691444859934,21.4566360720578,10.0543411948069));
#24434=CARTESIAN_POINT('Ctrl Pts',(-95.2356813002075,22.9350394509311,9.94901908464118));
#24435=CARTESIAN_POINT('Ctrl Pts',(-94.6604998395023,26.1329821564226,9.79103591939254));
#24436=CARTESIAN_POINT('Ctrl Pts',(-91.6674251873291,27.3912253832059,9.63305275414391));
#24437=CARTESIAN_POINT('Ctrl Pts',(-88.9782978536527,25.5759466184877,9.47506958889527));
#24438=CARTESIAN_POINT('Ctrl Pts',(-89.0288365510238,22.3300444200403,9.31708642364664));
#24439=CARTESIAN_POINT('Ctrl Pts',(-91.7748707182212,20.5994295614483,9.159103258398));
#24440=CARTESIAN_POINT('Ctrl Pts',(-94.7248360972086,21.9529638650458,9.00112009314937));
#24441=CARTESIAN_POINT('Ctrl Pts',(-95.2034137200466,25.1633690217573,8.84313692790074));
#24442=CARTESIAN_POINT('Ctrl Pts',(-92.7763213248125,27.3184906014102,8.6851537626521));
#24443=CARTESIAN_POINT('Ctrl Pts',(-89.6451105420003,26.4636613170838,8.52717059740347));
#24444=CARTESIAN_POINT('Ctrl Pts',(-88.6498494252551,23.3741907836555,8.36918743215483));
#24445=CARTESIAN_POINT('Ctrl Pts',(-90.6932967928722,20.8523585730158,8.2112042669062));
#24446=CARTESIAN_POINT('Ctrl Pts',(-93.9219648654793,21.1855406534173,8.05322110165756));
#24447=CARTESIAN_POINT('Ctrl Pts',(-95.407347018268,24.0715353436988,7.89523793640893));
#24448=CARTESIAN_POINT('Ctrl Pts',(-93.8021482371961,26.8926440959194,7.73725477116029));
#24449=CARTESIAN_POINT('Ctrl Pts',(-90.562339928744,27.0900263811239,7.57927160591166));
#24450=CARTESIAN_POINT('Ctrl Pts',(-88.6265381623655,24.4846490441156,7.42128844066302));
#24451=CARTESIAN_POINT('Ctrl Pts',(-89.7505815304929,21.4396785923102,7.26330527541439));
#24452=CARTESIAN_POINT('Ctrl Pts',(-92.9149241768713,20.7170069925142,7.10532211016575));
#24453=CARTESIAN_POINT('Ctrl Pts',(-95.2493993915097,22.9721221325502,6.94733894491712));
#24454=CARTESIAN_POINT('Ctrl Pts',(-94.6365584368373,26.1595575690848,6.78935577966849));
#24455=CARTESIAN_POINT('Ctrl Pts',(-91.6322689945581,27.3882005864732,6.63137261441985));
#24456=CARTESIAN_POINT('Ctrl Pts',(-88.9615241227262,25.5436300222753,6.47338944917122));
#24457=CARTESIAN_POINT('Ctrl Pts',(-89.0467805827143,22.298934341993,6.31540628392258));
#24458=CARTESIAN_POINT('Ctrl Pts',(-91.8107078531862,20.5971632737955,6.15742311867395));
#24459=CARTESIAN_POINT('Ctrl Pts',(-94.7463295621093,21.9818812627428,5.99943995342531));
#24460=CARTESIAN_POINT('Ctrl Pts',(-95.1909366199157,25.1971018289209,5.84145678817668));
#24461=CARTESIAN_POINT('Ctrl Pts',(-92.7412552500335,27.3265101767069,5.68347362292804));
#24462=CARTESIAN_POINT('Ctrl Pts',(-89.6192300677009,26.4386602532469,5.52549045767941));
#24463=CARTESIAN_POINT('Ctrl Pts',(-88.6566444747624,23.3388622434248,5.36750729243077));
#24464=CARTESIAN_POINT('Ctrl Pts',(-90.7265964591003,20.8387387448265,5.20952412718215));
#24465=CARTESIAN_POINT('Ctrl Pts',(-93.9515689190225,21.2059871053571,5.05154096193351));
#24466=CARTESIAN_POINT('Ctrl Pts',(-95.4064017581767,24.107500526857,4.89355779668487));
#24467=CARTESIAN_POINT('Ctrl Pts',(-93.7715119348338,26.9115073015181,4.73557463143624));
#24468=CARTESIAN_POINT('Ctrl Pts',(-90.5298003211737,27.0746775772205,4.5775914661876));
#24469=CARTESIAN_POINT('Ctrl Pts',(-88.6216099971176,24.4490103460599,4.41960830093897));
#24470=CARTESIAN_POINT('Ctrl Pts',(-89.777734717692,21.4160754032696,4.26162513569033));
#24471=CARTESIAN_POINT('Ctrl Pts',(-92.9495298993373,20.7268482688219,4.1036419704417));
#24472=CARTESIAN_POINT('Ctrl Pts',(-95.2600690541411,23.0064814656145,3.94565880519306));
#24473=CARTESIAN_POINT('Ctrl Pts',(-94.6136143009402,26.1872699016227,3.78767563994443));
#24474=CARTESIAN_POINT('Ctrl Pts',(-91.5965221741506,27.3841298446842,3.6296924746958));
#24475=CARTESIAN_POINT('Ctrl Pts',(-88.9453981954867,25.5114685844578,3.47170930944717));
#24476=CARTESIAN_POINT('Ctrl Pts',(-89.0649023370739,22.2678535784724,3.31372614419853));
#24477=CARTESIAN_POINT('Ctrl Pts',(-91.8466401922208,20.5953548049989,3.1557429789499));
#24478=CARTESIAN_POINT('Ctrl Pts',(-94.7674807253219,22.0109848056715,2.99775981370126));
#24479=CARTESIAN_POINT('Ctrl Pts',(-95.1781215807801,25.2307207544698,2.83977664845263));
#24480=CARTESIAN_POINT('Ctrl Pts',(-92.7060980942495,27.334148362878,2.68179348320399));
#24481=CARTESIAN_POINT('Ctrl Pts',(-89.5936187026175,26.4133949325244,2.52381031795536));
#24482=CARTESIAN_POINT('Ctrl Pts',(-88.6638109837675,23.3035990431782,2.36582715270672));
#24483=CARTESIAN_POINT('Ctrl Pts',(-90.7600370999255,20.8254848122201,2.20784398745809));
#24484=CARTESIAN_POINT('Ctrl Pts',(-93.9809589836469,21.2267188300363,2.04986082220945));
#24485=CARTESIAN_POINT('Ctrl Pts',(-95.4050689662123,24.1435062012512,1.89187765696082));
#24486=CARTESIAN_POINT('Ctrl Pts',(-93.7406947627281,26.9299392901691,1.73389449171218));
#24487=CARTESIAN_POINT('Ctrl Pts',(-90.4973905702364,27.0592039456624,1.57591132646355));
#24488=CARTESIAN_POINT('Ctrl Pts',(-88.6171277999948,24.4128768387722,1.41792816121492));
#24489=CARTESIAN_POINT('Ctrl Pts',(-89.8049936341991,21.3936687355948,1.25994499596628));
#24490=CARTESIAN_POINT('Ctrl Pts',(-92.9843134726817,20.7351877139554,1.10196183071765));
#24491=CARTESIAN_POINT('Ctrl Pts',(-95.2697691184269,23.044811872055,0.943978665469011));
#24492=CARTESIAN_POINT('Ctrl Pts',(-94.8162121163602,25.1505184486767,0.838656555303255));
#24493=CARTESIAN_POINT('Ctrl Pts',(-94.1951971040191,25.8768634390788,0.785995500220377));
#24494=CARTESIAN_POINT('Ctrl Pts',(-92.698066426161,21.3888678140614,10.2140044997796));
#24495=CARTESIAN_POINT('Ctrl Pts',(-93.5620356702265,21.6198434520493,10.1613434446967));
#24496=CARTESIAN_POINT('Ctrl Pts',(-95.0280479915439,23.0033778507559,10.056021334531));
#24497=CARTESIAN_POINT('Ctrl Pts',(-94.489775861112,25.9961089290038,9.89803816928235));
#24498=CARTESIAN_POINT('Ctrl Pts',(-91.6887664760181,27.1736108280598,9.74005500403372));
#24499=CARTESIAN_POINT('Ctrl Pts',(-89.1722001438447,25.4748182994988,9.58207183878508));
#24500=CARTESIAN_POINT('Ctrl Pts',(-89.2194957786344,22.4372052836166,9.42408867353645));
#24501=CARTESIAN_POINT('Ctrl Pts',(-91.7893172391592,20.8176437877551,9.26610550828781));
#24502=CARTESIAN_POINT('Ctrl Pts',(-94.5499836683268,22.0843219458392,9.10812234303918));
#24503=CARTESIAN_POINT('Ctrl Pts',(-94.9978510184081,25.0887157612002,8.95013917779056));
#24504=CARTESIAN_POINT('Ctrl Pts',(-92.7265048718613,27.1055434291113,8.7921560125419));
#24505=CARTESIAN_POINT('Ctrl Pts',(-89.7962235362468,26.3055684447544,8.63417284729328));
#24506=CARTESIAN_POINT('Ctrl Pts',(-88.8648282145167,23.4143488913694,8.47618968204464));
#24507=CARTESIAN_POINT('Ctrl Pts',(-90.7771477921409,21.05434237282,8.31820651679601));
#24508=CARTESIAN_POINT('Ctrl Pts',(-93.7986325941184,21.36614419623,8.16022335154737));
#24509=CARTESIAN_POINT('Ctrl Pts',(-95.1886979395956,24.0669449286608,8.00224018629874));
#24510=CARTESIAN_POINT('Ctrl Pts',(-93.6865045855277,26.7070234464496,7.84425702105011));
#24511=CARTESIAN_POINT('Ctrl Pts',(-90.6545944153985,26.8917397323958,7.68627385580146));
#24512=CARTESIAN_POINT('Ctrl Pts',(-88.8430128327707,24.453549168932,7.52829069055284));
#24513=CARTESIAN_POINT('Ctrl Pts',(-89.8949264631544,21.6039741318885,7.3703075253042));
#24514=CARTESIAN_POINT('Ctrl Pts',(-92.8562135943403,20.9276762881645,7.21232436005557));
#24515=CARTESIAN_POINT('Ctrl Pts',(-95.0408857944551,23.0380809408256,7.05434119480694));
#24516=CARTESIAN_POINT('Ctrl Pts',(-94.4673707755895,26.0209790003952,6.89635802955829));
#24517=CARTESIAN_POINT('Ctrl Pts',(-91.6558662522217,27.1707801321966,6.73837486430967));
#24518=CARTESIAN_POINT('Ctrl Pts',(-89.1565027813635,25.4445754556661,6.58039169906103));
#24519=CARTESIAN_POINT('Ctrl Pts',(-89.2362883438098,22.4080915358129,6.4224085338124));
#24520=CARTESIAN_POINT('Ctrl Pts',(-91.822854709165,20.8155229275285,6.26442536856376));
#24521=CARTESIAN_POINT('Ctrl Pts',(-94.5700978999785,22.1113837173467,6.10644220331513));
#24522=CARTESIAN_POINT('Ctrl Pts',(-94.9861745724032,25.120283937885,5.94845903806649));
#24523=CARTESIAN_POINT('Ctrl Pts',(-92.6936889831954,27.1130483891544,5.79047587281786));
#24524=CARTESIAN_POINT('Ctrl Pts',(-89.7720038091006,26.2821716963994,5.63249270756922));
#24525=CARTESIAN_POINT('Ctrl Pts',(-88.8711872264539,23.3812873796306,5.47450954232058));
#24526=CARTESIAN_POINT('Ctrl Pts',(-90.8083106224959,21.0415965274887,5.31652637707196));
#24527=CARTESIAN_POINT('Ctrl Pts',(-93.8263369588428,21.385278601626,5.15854321182332));
#24528=CARTESIAN_POINT('Ctrl Pts',(-95.1878133367391,24.1006022300213,5.00056004657468));
#24529=CARTESIAN_POINT('Ctrl Pts',(-93.6578342112759,26.7246762022459,4.84257688132605));
#24530=CARTESIAN_POINT('Ctrl Pts',(-90.6241428708219,26.8773758595294,4.68459371607742));
#24531=CARTESIAN_POINT('Ctrl Pts',(-88.8384009073378,24.4201974021613,4.52661055082877));
#24532=CARTESIAN_POINT('Ctrl Pts',(-89.9203372333551,21.5818855568597,4.36862738558015));
#24533=CARTESIAN_POINT('Ctrl Pts',(-92.8885986714498,20.9368860508676,4.21064422033151));
#24534=CARTESIAN_POINT('Ctrl Pts',(-95.0508707860237,23.0702354393139,4.05266105508288));
#24535=CARTESIAN_POINT('Ctrl Pts',(-94.4458989623375,26.0469130356406,3.89467788983424));
#24536=CARTESIAN_POINT('Ctrl Pts',(-91.6224133012984,27.1669706094549,3.73669472458561));
#24537=CARTESIAN_POINT('Ctrl Pts',(-89.1414116530791,25.4144778137314,3.57871155933698));
#24538=CARTESIAN_POINT('Ctrl Pts',(-89.2532472272103,22.3790052214257,3.42072839408834));
#24539=CARTESIAN_POINT('Ctrl Pts',(-91.8564812740057,20.8138305079731,3.26274522883971));
#24540=CARTESIAN_POINT('Ctrl Pts',(-94.5898917954033,22.1386196891669,3.10476206359107));
#24541=CARTESIAN_POINT('Ctrl Pts',(-94.9741818729016,25.1517455407257,2.94677889834244));
#24542=CARTESIAN_POINT('Ctrl Pts',(-92.6607878581825,27.1201964337696,2.7887957330938));
#24543=CARTESIAN_POINT('Ctrl Pts',(-89.7480359224623,26.2585276484937,2.63081256784517));
#24544=CARTESIAN_POINT('Ctrl Pts',(-88.8778938613744,23.3482870150165,2.47282940259653));
#24545=CARTESIAN_POINT('Ctrl Pts',(-90.8396053811237,21.0291930982615,2.3148462373479));
#24546=CARTESIAN_POINT('Ctrl Pts',(-93.8538410662936,21.4046799738415,2.15686307209927));
#24547=CARTESIAN_POINT('Ctrl Pts',(-95.1865660698866,24.1342974242998,1.99887990685063));
#24548=CARTESIAN_POINT('Ctrl Pts',(-93.628994573672,26.741925412238,1.840896741602));
#24549=CARTESIAN_POINT('Ctrl Pts',(-90.5938128499926,26.862895169185,1.68291357635336));
#24550=CARTESIAN_POINT('Ctrl Pts',(-88.8342063323052,24.386382578012,1.52493041110473));
#24551=CARTESIAN_POINT('Ctrl Pts',(-89.9458469482258,21.5609167225542,1.36694724585609));
#24552=CARTESIAN_POINT('Ctrl Pts',(-92.9211501867667,20.9446903547357,1.20896408060746));
#24553=CARTESIAN_POINT('Ctrl Pts',(-95.0599483982647,23.1061061878421,1.05098091535882));
#24554=CARTESIAN_POINT('Ctrl Pts',(-94.6354960985062,25.076689807963,0.945658805193066));
#24555=CARTESIAN_POINT('Ctrl Pts',(-94.054331550342,25.7564253212269,0.892997750110188));
#24556=CARTESIAN_POINT('Ctrl Pts',(-92.6501999979751,21.5679131979649,10.3210067496694));
#24557=CARTESIAN_POINT('Ctrl Pts',(-93.4549268544596,21.7830508320407,10.2683456945866));
#24558=CARTESIAN_POINT('Ctrl Pts',(-94.8204146828803,23.0717162505807,10.1630235844208));
#24559=CARTESIAN_POINT('Ctrl Pts',(-94.3190518827217,25.8592357015848,10.0050404191722));
#24560=CARTESIAN_POINT('Ctrl Pts',(-91.7101077647069,26.9559962729139,9.84705725392354));
#24561=CARTESIAN_POINT('Ctrl Pts',(-89.3661024340368,25.3736899805099,9.68907408867489));
#24562=CARTESIAN_POINT('Ctrl Pts',(-89.4101550062447,22.544366147193,9.53109092342627));
#24563=CARTESIAN_POINT('Ctrl Pts',(-91.8037637600975,21.0358580140618,9.37310775817762));
#24564=CARTESIAN_POINT('Ctrl Pts',(-94.3751312394447,22.2156800266327,9.215124592929));
#24565=CARTESIAN_POINT('Ctrl Pts',(-94.7922883167697,25.0140625006431,9.05714142768035));
#24566=CARTESIAN_POINT('Ctrl Pts',(-92.6766884189101,26.8925962568123,8.89915826243172));
#24567=CARTESIAN_POINT('Ctrl Pts',(-89.9473365304931,26.1474755724249,8.74117509718309));
#24568=CARTESIAN_POINT('Ctrl Pts',(-89.0798070037785,23.4545069990834,8.58319193193445));
#24569=CARTESIAN_POINT('Ctrl Pts',(-90.8609987914095,21.2563261726241,8.42520876668581));
#24570=CARTESIAN_POINT('Ctrl Pts',(-93.6753003227575,21.5467477390426,8.26722560143719));
#24571=CARTESIAN_POINT('Ctrl Pts',(-94.9700488609232,24.0623545136228,8.10924243618855));
#24572=CARTESIAN_POINT('Ctrl Pts',(-93.5708609338593,26.5214027969798,7.95125927093992));
#24573=CARTESIAN_POINT('Ctrl Pts',(-90.7468489020531,26.6934530836676,7.79327610569128));
#24574=CARTESIAN_POINT('Ctrl Pts',(-89.0594875031757,24.4224492937485,7.63529294044265));
#24575=CARTESIAN_POINT('Ctrl Pts',(-90.0392713958159,21.7682696714666,7.47730977519401));
#24576=CARTESIAN_POINT('Ctrl Pts',(-92.7975030118092,21.1383455838149,7.31932660994537));
#24577=CARTESIAN_POINT('Ctrl Pts',(-94.8323721974005,23.104039749101,7.16134344469675));
#24578=CARTESIAN_POINT('Ctrl Pts',(-94.2981831143417,25.8824004317056,7.0033602794481));
#24579=CARTESIAN_POINT('Ctrl Pts',(-91.6794635098852,26.9533596779201,6.84537711419948));
#24580=CARTESIAN_POINT('Ctrl Pts',(-89.3514814400011,25.3455208890569,6.68739394895083));
#24581=CARTESIAN_POINT('Ctrl Pts',(-89.425796104905,22.5172487296327,6.52941078370221));
#24582=CARTESIAN_POINT('Ctrl Pts',(-91.8350015651438,21.0338825812615,6.37142761845357));
#24583=CARTESIAN_POINT('Ctrl Pts',(-94.3938662378476,22.2408861719505,6.21344445320494));
#24584=CARTESIAN_POINT('Ctrl Pts',(-94.7814125248905,25.0434660468492,6.0554612879563));
#24585=CARTESIAN_POINT('Ctrl Pts',(-92.6461227163573,26.8995866016018,5.89747812270767));
#24586=CARTESIAN_POINT('Ctrl Pts',(-89.9247775505004,26.1256831395519,5.73949495745903));
#24587=CARTESIAN_POINT('Ctrl Pts',(-89.0857299781456,23.4237125158365,5.5815117922104));
#24588=CARTESIAN_POINT('Ctrl Pts',(-90.8900247858914,21.2444543101509,5.42352862696177));
#24589=CARTESIAN_POINT('Ctrl Pts',(-93.7011049986631,21.5645700978948,5.26554546171313));
#24590=CARTESIAN_POINT('Ctrl Pts',(-94.9692249153015,24.0937039331857,5.1075622964645));
#24591=CARTESIAN_POINT('Ctrl Pts',(-93.544156487718,26.5378451029737,4.94957913121586));
#24592=CARTESIAN_POINT('Ctrl Pts',(-90.7184854204702,26.6800741418383,4.79159596596723));
#24593=CARTESIAN_POINT('Ctrl Pts',(-89.0551918175579,24.3913844582627,4.63361280071859));
#24594=CARTESIAN_POINT('Ctrl Pts',(-90.0629397490182,21.7476957104499,4.47562963546996));
#24595=CARTESIAN_POINT('Ctrl Pts',(-92.8276674435623,21.1469238329133,4.31764647022132));
#24596=CARTESIAN_POINT('Ctrl Pts',(-94.8416725179064,23.1339894130133,4.15966330497269));
#24597=CARTESIAN_POINT('Ctrl Pts',(-94.2781836237349,25.9065561696584,4.00168013972405));
#24598=CARTESIAN_POINT('Ctrl Pts',(-91.6483044284461,26.9498113742256,3.84369697447542));
#24599=CARTESIAN_POINT('Ctrl Pts',(-89.3374251106716,25.317487043005,3.68571380922678));
#24600=CARTESIAN_POINT('Ctrl Pts',(-89.4415921173466,22.4901568643791,3.52773064397815));
#24601=CARTESIAN_POINT('Ctrl Pts',(-91.8663223557907,21.0323062109474,3.36974747872952));
#24602=CARTESIAN_POINT('Ctrl Pts',(-94.4123028654849,22.2662545726624,3.21176431348088));
#24603=CARTESIAN_POINT('Ctrl Pts',(-94.770242165023,25.0727703269817,3.05378114823225));
#24604=CARTESIAN_POINT('Ctrl Pts',(-92.6154776221156,26.9062445046611,2.89579798298362));
#24605=CARTESIAN_POINT('Ctrl Pts',(-89.9024531423069,26.103660364463,2.73781481773498));
#24606=CARTESIAN_POINT('Ctrl Pts',(-89.0919767389814,23.3929749868548,2.57983165248635));
#24607=CARTESIAN_POINT('Ctrl Pts',(-90.9191736623217,21.2329013843029,2.42184848723771));
#24608=CARTESIAN_POINT('Ctrl Pts',(-93.7267231489404,21.5826411176466,2.26386532198907));
#24609=CARTESIAN_POINT('Ctrl Pts',(-94.9680631735608,24.1250886473484,2.10588215674044));
#24610=CARTESIAN_POINT('Ctrl Pts',(-93.5172943846158,26.5539115343069,1.94789899149181));
#24611=CARTESIAN_POINT('Ctrl Pts',(-90.690235129749,26.6665863927076,1.78991582624317));
#24612=CARTESIAN_POINT('Ctrl Pts',(-89.0512848646154,24.3598883172517,1.63193266099454));
#24613=CARTESIAN_POINT('Ctrl Pts',(-90.0867002622527,21.7281647095135,1.4739494957459));
#24614=CARTESIAN_POINT('Ctrl Pts',(-92.8579869008516,21.154192995516,1.31596633049727));
#24615=CARTESIAN_POINT('Ctrl Pts',(-94.8501276781025,23.1674005036292,1.15798316524863));
#24616=CARTESIAN_POINT('Ctrl Pts',(-94.4547800806521,25.0028611672492,1.05266105508288));
#24617=CARTESIAN_POINT('Ctrl Pts',(-93.913465996665,25.635987203375,0.999999999999999));
#24618=CARTESIAN_POINT('Ctrl Pts',(-94.5149491154365,24.0017493991467,9.11258330249198));
#24619=CARTESIAN_POINT('Ctrl Pts',(-94.5168561491793,24.2947752403159,9.09410267755477));
#24620=CARTESIAN_POINT('Ctrl Pts',(-94.4695027538977,24.5872051880346,9.07562205261757));
#24621=CARTESIAN_POINT('Ctrl Pts',(-94.3701621542389,24.8607543810029,9.05714142768036));
#24622=CARTESIAN_POINT('Ctrl Pts',(-94.0870883508165,25.6402404193662,9.00448037259748));
#24623=CARTESIAN_POINT('Ctrl Pts',(-93.3818883848633,26.2664183380893,8.9518193175146));
#24624=CARTESIAN_POINT('Ctrl Pts',(-92.5743964204839,26.4553205167196,8.89915826243172));
#24625=CARTESIAN_POINT('Ctrl Pts',(-91.7669044561044,26.6442226953499,8.84649720734884));
#24626=CARTESIAN_POINT('Ctrl Pts',(-90.8571204932987,26.3958491338874,8.79383615226597));
#24627=CARTESIAN_POINT('Ctrl Pts',(-90.2576402574435,25.8228342575992,8.74117509718309));
#24628=CARTESIAN_POINT('Ctrl Pts',(-89.6581600215882,25.2498193813111,8.68851404210021));
#24629=CARTESIAN_POINT('Ctrl Pts',(-89.3689835126833,24.3521631901972,8.63585298701733));
#24630=CARTESIAN_POINT('Ctrl Pts',(-89.5212605561694,23.5369716235638,8.58319193193445));
#24631=CARTESIAN_POINT('Ctrl Pts',(-89.6735375996555,22.7217800569303,8.53053087685158));
#24632=CARTESIAN_POINT('Ctrl Pts',(-90.2672681955325,21.9890531147772,8.47786982176869));
#24633=CARTESIAN_POINT('Ctrl Pts',(-91.0331837486956,21.6710932381038,8.42520876668582));
#24634=CARTESIAN_POINT('Ctrl Pts',(-91.7990993018588,21.3531333614303,8.37254771160294));
#24635=CARTESIAN_POINT('Ctrl Pts',(-92.7371998123082,21.4499405502365,8.31988665652007));
#24636=CARTESIAN_POINT('Ctrl Pts',(-93.4220414905605,21.9176119404029,8.26722560143719));
#24637=CARTESIAN_POINT('Ctrl Pts',(-94.0924008378475,22.375393494611,8.21567816845545));
#24638=CARTESIAN_POINT('Ctrl Pts',(-94.5200994141618,23.1885197854572,8.16413073547371));
#24639=CARTESIAN_POINT('Ctrl Pts',(-94.5215632327497,24.0003195913041,8.11258330249198));
#24640=CARTESIAN_POINT('Ctrl Pts',(-92.7937992825329,21.0307770462543,10.));
#24641=CARTESIAN_POINT('Ctrl Pts',(-92.886852429315,21.0648163030129,10.));
#24642=CARTESIAN_POINT('Ctrl Pts',(-92.9778402996159,21.1036238816581,10.));
#24643=CARTESIAN_POINT('Ctrl Pts',(-93.0665543950992,21.146871551721,10.));
#24644=CARTESIAN_POINT('Ctrl Pts',(-93.1572341761917,21.1910774835146,10.));
#24645=CARTESIAN_POINT('Ctrl Pts',(-93.2455389715861,21.2399230660589,10.));
#24646=CARTESIAN_POINT('Ctrl Pts',(-93.331217194957,21.2931033029543,10.));
#24647=CARTESIAN_POINT('Ctrl Pts',(-93.4136696869558,21.3442813372855,10.));
#24648=CARTESIAN_POINT('Ctrl Pts',(-93.4936899468829,21.399474651453,10.));
#24649=CARTESIAN_POINT('Ctrl Pts',(-93.5710207513935,21.4584414877618,10.));
#24650=CARTESIAN_POINT('Ctrl Pts',(-93.6386852053402,21.510037469532,10.));
#24651=CARTESIAN_POINT('Ctrl Pts',(-93.704290254497,21.5645232522164,10.));
#24652=CARTESIAN_POINT('Ctrl Pts',(-93.7676389322689,21.6217495880709,10.));
#24653=CARTESIAN_POINT('Ctrl Pts',(-93.7817377391777,21.6344858137932,10.));
#24654=CARTESIAN_POINT('Ctrl Pts',(-93.7957273872076,21.6473604850923,10.));
#24655=CARTESIAN_POINT('Ctrl Pts',(-93.8095862319439,21.6603535286729,10.));
#24656=CARTESIAN_POINT('Ctrl Pts',(-93.8820169438681,21.7282592895434,10.));
#24657=CARTESIAN_POINT('Ctrl Pts',(-93.950981982273,21.7994868057952,10.));
#24658=CARTESIAN_POINT('Ctrl Pts',(-94.0162414008102,21.873745473286,10.));
#24659=CARTESIAN_POINT('Ctrl Pts',(-94.0811411486556,21.9475948716335,10.));
#24660=CARTESIAN_POINT('Ctrl Pts',(-94.1423764967312,22.0244428982871,10.));
#24661=CARTESIAN_POINT('Ctrl Pts',(-94.1996678356441,22.1040304952042,10.));
#24662=CARTESIAN_POINT('Ctrl Pts',(-94.2548606489396,22.1807028764161,10.));
#24663=CARTESIAN_POINT('Ctrl Pts',(-94.306393259299,22.2599185451354,10.));
#24664=CARTESIAN_POINT('Ctrl Pts',(-94.3539707411089,22.3414594921653,10.));
#24665=CARTESIAN_POINT('Ctrl Pts',(-94.3739595056304,22.3757173538057,10.));
#24666=CARTESIAN_POINT('Ctrl Pts',(-94.393249578858,22.4103857572211,10.));
#24667=CARTESIAN_POINT('Ctrl Pts',(-94.4118164862111,22.4454488349773,10.));
#24668=CARTESIAN_POINT('Ctrl Pts',(-94.4248530613841,22.4700680373179,10.));
#24669=CARTESIAN_POINT('Ctrl Pts',(-94.4375330822862,22.4948818173567,10.));
#24670=CARTESIAN_POINT('Ctrl Pts',(-94.4498475904497,22.5198846883706,10.));
#24671=CARTESIAN_POINT('Ctrl Pts',(-94.4576000654923,22.5356249949224,10.));
#24672=CARTESIAN_POINT('Ctrl Pts',(-94.4652085569624,22.5514423657842,10.));
#24673=CARTESIAN_POINT('Ctrl Pts',(-94.4726611640941,22.5673143052863,10.));
#24674=CARTESIAN_POINT('Ctrl Pts',(-94.5147817191001,22.6570191413296,10.));
#24675=CARTESIAN_POINT('Ctrl Pts',(-94.5520000635204,22.7486086650705,10.));
#24676=CARTESIAN_POINT('Ctrl Pts',(-94.5840245510179,22.841810410067,10.));
#24677=CARTESIAN_POINT('Ctrl Pts',(-94.6138870174053,22.928719965682,10.));
#24678=CARTESIAN_POINT('Ctrl Pts',(-94.6392330675716,23.0170321958857,10.));
#24679=CARTESIAN_POINT('Ctrl Pts',(-94.6597756784635,23.1065348612349,10.));
#24680=CARTESIAN_POINT('Ctrl Pts',(-94.6612629487322,23.1130147898981,10.));
#24681=CARTESIAN_POINT('Ctrl Pts',(-94.6627250182631,23.1195009595791,10.));
#24682=CARTESIAN_POINT('Ctrl Pts',(-94.6641617673287,23.1259932900522,10.));
#24683=CARTESIAN_POINT('Ctrl Pts',(-94.6847473682253,23.2190147697364,10.));
#24684=CARTESIAN_POINT('Ctrl Pts',(-94.7001391868307,23.3133019772443,10.));
#24685=CARTESIAN_POINT('Ctrl Pts',(-94.710414230246,23.4084468885598,10.));
#24686=CARTESIAN_POINT('Ctrl Pts',(-94.7162318667376,23.4623170753494,10.));
#24687=CARTESIAN_POINT('Ctrl Pts',(-94.7204082723905,23.5164620291754,10.));
#24688=CARTESIAN_POINT('Ctrl Pts',(-94.7229505321312,23.5708049958492,10.));
#24689=CARTESIAN_POINT('Ctrl Pts',(-94.7235978728717,23.5846424553858,10.));
#24690=CARTESIAN_POINT('Ctrl Pts',(-94.7241391083574,23.5984913476866,10.));
#24691=CARTESIAN_POINT('Ctrl Pts',(-94.7245741747776,23.6123381701615,10.));
#24692=CARTESIAN_POINT('Ctrl Pts',(-94.7275029882991,23.7055532725254,10.));
#24693=CARTESIAN_POINT('Ctrl Pts',(-94.7256324130786,23.7988256455609,10.));
#24694=CARTESIAN_POINT('Ctrl Pts',(-94.7190973170423,23.8917800191491,10.));
#24695=CARTESIAN_POINT('Ctrl Pts',(-94.7125517832747,23.9848828576991,10.));
#24696=CARTESIAN_POINT('Ctrl Pts',(-94.7013264378212,24.0776676598214,10.));
#24697=CARTESIAN_POINT('Ctrl Pts',(-94.6855058890551,24.1697452002995,10.));
#24698=CARTESIAN_POINT('Ctrl Pts',(-94.6699125051955,24.2605006130693,10.));
#24699=CARTESIAN_POINT('Ctrl Pts',(-94.6498544727692,24.3505697728504,10.));
#24700=CARTESIAN_POINT('Ctrl Pts',(-94.6253698218263,24.4395547318434,10.));
#24701=CARTESIAN_POINT('Ctrl Pts',(-94.6161277488969,24.4731433454831,10.));
#24702=CARTESIAN_POINT('Ctrl Pts',(-94.6062545684086,24.5065771588648,10.));
#24703=CARTESIAN_POINT('Ctrl Pts',(-94.5957509020197,24.5398334420004,10.));
#24704=CARTESIAN_POINT('Ctrl Pts',(-94.5880549567994,24.564200032081,10.));
#24705=CARTESIAN_POINT('Ctrl Pts',(-94.580020527761,24.5884713017397,10.));
#24706=CARTESIAN_POINT('Ctrl Pts',(-94.5716476124507,24.6126380141342,10.));
#24707=CARTESIAN_POINT('Ctrl Pts',(-94.5664801186889,24.6275529309722,10.));
#24708=CARTESIAN_POINT('Ctrl Pts',(-94.5611866874841,24.6424193347924,10.));
#24709=CARTESIAN_POINT('Ctrl Pts',(-94.5557685057797,24.6572331360837,10.));
#24710=CARTESIAN_POINT('Ctrl Pts',(-94.5240624702071,24.7439203194109,10.));
#24711=CARTESIAN_POINT('Ctrl Pts',(-94.4880796645989,24.8288333308261,10.));
#24712=CARTESIAN_POINT('Ctrl Pts',(-94.4478803904321,24.9115713472888,10.));
#24713=CARTESIAN_POINT('Ctrl Pts',(-94.417730934807,24.9736248596359,10.));
#24714=CARTESIAN_POINT('Ctrl Pts',(-94.385208726487,25.0344544524595,10.));
#24715=CARTESIAN_POINT('Ctrl Pts',(-94.3503241152314,25.0938760326955,10.));
#24716=CARTESIAN_POINT('Ctrl Pts',(-94.3345452312936,25.1207533916281,10.));
#24717=CARTESIAN_POINT('Ctrl Pts',(-94.3182828581177,25.1473424861813,10.));
#24718=CARTESIAN_POINT('Ctrl Pts',(-94.30153717312,25.1736252114009,10.));
#24719=CARTESIAN_POINT('Ctrl Pts',(-94.2924151850668,25.1879423746278,10.));
#24720=CARTESIAN_POINT('Ctrl Pts',(-94.2831549587815,25.2021604667475,10.));
#24721=CARTESIAN_POINT('Ctrl Pts',(-94.2737571738008,25.2162764754097,10.));
#24722=CARTESIAN_POINT('Ctrl Pts',(-94.2261821049897,25.2877369402766,10.));
#24723=CARTESIAN_POINT('Ctrl Pts',(-94.1750818284041,25.3565881459122,10.));
#24724=CARTESIAN_POINT('Ctrl Pts',(-94.1204874011733,25.4224766046402,10.));
#24725=CARTESIAN_POINT('Ctrl Pts',(-94.0743569379003,25.4781501464216,10.));
#24726=CARTESIAN_POINT('Ctrl Pts',(-94.0257310847012,25.5317080232705,10.));
#24727=CARTESIAN_POINT('Ctrl Pts',(-93.974612285206,25.5829128576333,10.));
#24728=CARTESIAN_POINT('Ctrl Pts',(-93.9557804971257,25.6017763403231,10.));
#24729=CARTESIAN_POINT('Ctrl Pts',(-93.9366102390046,25.6203202358367,10.));
#24730=CARTESIAN_POINT('Ctrl Pts',(-93.9171116625783,25.6385402433575,10.));
#24731=CARTESIAN_POINT('Origin',(-92.,24.,5.));
#24732=CARTESIAN_POINT('Origin',(24.,-92.,1.));
#24733=CARTESIAN_POINT('Ctrl Pts',(22.086534003335,-90.364012796625,0.999999999999996));
#24734=CARTESIAN_POINT('Ctrl Pts',(22.0243936079803,-90.4224095095372,0.999999999999996));
#24735=CARTESIAN_POINT('Ctrl Pts',(21.9656285061808,-90.4840599082819,1.));
#24736=CARTESIAN_POINT('Ctrl Pts',(21.9102507399932,-90.5485875659184,1.));
#24737=CARTESIAN_POINT('Ctrl Pts',(21.8535182656837,-90.6146937657734,1.));
#24738=CARTESIAN_POINT('Ctrl Pts',(21.8003404147377,-90.6838202105017,1.));
#24739=CARTESIAN_POINT('Ctrl Pts',(21.7507590223762,-90.7556084413231,1.));
#24740=CARTESIAN_POINT('Ctrl Pts',(21.7378150803192,-90.7743498008507,1.));
#24741=CARTESIAN_POINT('Ctrl Pts',(21.7251164247153,-90.7932727903877,1.));
#24742=CARTESIAN_POINT('Ctrl Pts',(21.712664175894,-90.8123714657101,1.));
#24743=CARTESIAN_POINT('Ctrl Pts',(21.7025035054025,-90.8279554256486,1.));
#24744=CARTESIAN_POINT('Ctrl Pts',(21.6925064617469,-90.8436572537483,1.00000000000001));
#24745=CARTESIAN_POINT('Ctrl Pts',(21.6826824795535,-90.859459161395,1.00000000000001));
#24746=CARTESIAN_POINT('Ctrl Pts',(21.6352350823632,-90.9357784557211,1.00000000000001));
#24747=CARTESIAN_POINT('Ctrl Pts',(21.5917712588655,-91.0145049681213,1.));
#24748=CARTESIAN_POINT('Ctrl Pts',(21.5523257641043,-91.0952462143552,1.));
#24749=CARTESIAN_POINT('Ctrl Pts',(21.5204848603752,-91.1604215725011,1.));
#24750=CARTESIAN_POINT('Ctrl Pts',(21.4912627687126,-91.2269108043057,1.));
#24751=CARTESIAN_POINT('Ctrl Pts',(21.4646949470728,-91.2945252986071,1.));
#24752=CARTESIAN_POINT('Ctrl Pts',(21.453969916315,-91.3218202549228,1.));
#24753=CARTESIAN_POINT('Ctrl Pts',(21.4436776165902,-91.3492987408287,1.));
#24754=CARTESIAN_POINT('Ctrl Pts',(21.4338211709067,-91.3769489152558,1.));
#24755=CARTESIAN_POINT('Ctrl Pts',(21.4286030046016,-91.3915873775532,1.));
#24756=CARTESIAN_POINT('Ctrl Pts',(21.4235075578582,-91.4062726316137,1.));
#24757=CARTESIAN_POINT('Ctrl Pts',(21.4185390502848,-91.4209911044601,1.));
#24758=CARTESIAN_POINT('Ctrl Pts',(21.3890249542532,-91.5084222725943,1.));
#24759=CARTESIAN_POINT('Ctrl Pts',(21.3639471422075,-91.5971333206905,1.00000000000001));
#24760=CARTESIAN_POINT('Ctrl Pts',(21.3433383849555,-91.6867265580416,1.));
#24761=CARTESIAN_POINT('Ctrl Pts',(21.3224107209673,-91.7777061908243,1.));
#24762=CARTESIAN_POINT('Ctrl Pts',(21.3060909929174,-91.8695963327704,1.));
#24763=CARTESIAN_POINT('Ctrl Pts',(21.2944553610685,-91.9620136812046,1.));
#24764=CARTESIAN_POINT('Ctrl Pts',(21.2829108960697,-92.0537069264133,1.));
#24765=CARTESIAN_POINT('Ctrl Pts',(21.2759770698909,-92.1459200787513,1.));
#24766=CARTESIAN_POINT('Ctrl Pts',(21.2737752209329,-92.2382979338272,1.));
#24767=CARTESIAN_POINT('Ctrl Pts',(21.2726800380433,-92.2842459748521,1.));
#24768=CARTESIAN_POINT('Ctrl Pts',(21.2727563056639,-92.3302349753314,1.));
#24769=CARTESIAN_POINT('Ctrl Pts',(21.2740237450673,-92.376221919001,0.999999999999999));
#24770=CARTESIAN_POINT('Ctrl Pts',(21.274440529148,-92.3913442404225,0.999999999999999));
#24771=CARTESIAN_POINT('Ctrl Pts',(21.2749862321654,-92.4064681915453,1.00000000000001));
#24772=CARTESIAN_POINT('Ctrl Pts',(21.2756613706513,-92.4215864144296,1.00000000000001));
#24773=CARTESIAN_POINT('Ctrl Pts',(21.2799353266163,-92.5172921403349,1.00000000000001));
#24774=CARTESIAN_POINT('Ctrl Pts',(21.2893763305713,-92.6124307008699,1.));
#24775=CARTESIAN_POINT('Ctrl Pts',(21.3040485587001,-92.7066037716583,1.));
#24776=CARTESIAN_POINT('Ctrl Pts',(21.3082030637169,-92.7332692850082,1.));
#24777=CARTESIAN_POINT('Ctrl Pts',(21.3127772824124,-92.7598575187067,1.));
#24778=CARTESIAN_POINT('Ctrl Pts',(21.3177733858486,-92.7863596889658,1.));
#24779=CARTESIAN_POINT('Ctrl Pts',(21.3347382842712,-92.8763511457416,1.));
#24780=CARTESIAN_POINT('Ctrl Pts',(21.3565634809548,-92.9653501497144,1.00000000000001));
#24781=CARTESIAN_POINT('Ctrl Pts',(21.3829463368398,-93.053124461382,1.00000000000001));
#24782=CARTESIAN_POINT('Ctrl Pts',(21.4099256760044,-93.1428832401415,1.00000000000001));
#24783=CARTESIAN_POINT('Ctrl Pts',(21.4416712994561,-93.2313620234102,1.));
#24784=CARTESIAN_POINT('Ctrl Pts',(21.4779138149312,-93.3183087529105,1.));
#24785=CARTESIAN_POINT('Ctrl Pts',(21.4905805865845,-93.3486966648463,1.));
#24786=CARTESIAN_POINT('Ctrl Pts',(21.5037971164571,-93.3788973526586,1.));
#24787=CARTESIAN_POINT('Ctrl Pts',(21.5175533367842,-93.4088996997427,1.));
#24788=CARTESIAN_POINT('Ctrl Pts',(21.5245000449418,-93.4240504856619,1.));
#24789=CARTESIAN_POINT('Ctrl Pts',(21.5315843916462,-93.439150688623,1.));
#24790=CARTESIAN_POINT('Ctrl Pts',(21.5388051477107,-93.4541988513293,1.));
#24791=CARTESIAN_POINT('Ctrl Pts',(21.5448146544791,-93.4667227525421,1.));
#24792=CARTESIAN_POINT('Ctrl Pts',(21.5509168026395,-93.4792066765993,1.));
#24793=CARTESIAN_POINT('Ctrl Pts',(21.557106992875,-93.4916425965208,1.));
#24794=CARTESIAN_POINT('Ctrl Pts',(21.6000701102765,-93.5779543037962,1.));
#24795=CARTESIAN_POINT('Ctrl Pts',(21.6473202761047,-93.6620593554308,1.00000000000001));
#24796=CARTESIAN_POINT('Ctrl Pts',(21.6985154201144,-93.7437076709316,1.));
#24797=CARTESIAN_POINT('Ctrl Pts',(21.7507153892901,-93.8269585267468,1.));
#24798=CARTESIAN_POINT('Ctrl Pts',(21.807017032588,-93.9076560355637,1.));
#24799=CARTESIAN_POINT('Ctrl Pts',(21.8671126570016,-93.9855277788831,1.));
#24800=CARTESIAN_POINT('Ctrl Pts',(21.9276763341489,-94.0640060236358,1.));
#24801=CARTESIAN_POINT('Ctrl Pts',(21.9920937838106,-94.1396151518342,1.));
#24802=CARTESIAN_POINT('Ctrl Pts',(22.0600992170831,-94.2120567437253,1.));
#24803=CARTESIAN_POINT('Ctrl Pts',(22.0970259685969,-94.2513923164038,1.));
#24804=CARTESIAN_POINT('Ctrl Pts',(22.1350114303049,-94.2897935419768,1.));
#24805=CARTESIAN_POINT('Ctrl Pts',(22.1740182897571,-94.3272088863493,1.));
#24806=CARTESIAN_POINT('Ctrl Pts',(22.1861457892181,-94.338841572884,1.));
#24807=CARTESIAN_POINT('Ctrl Pts',(22.19837204473,-94.3503789383802,1.));
#24808=CARTESIAN_POINT('Ctrl Pts',(22.2106959996637,-94.3618193694808,1.));
#24809=CARTESIAN_POINT('Ctrl Pts',(22.2219869757007,-94.3723008775767,1.));
#24810=CARTESIAN_POINT('Ctrl Pts',(22.233354235474,-94.3826956656343,1.));
#24811=CARTESIAN_POINT('Ctrl Pts',(22.2447923276406,-94.3929988640766,1.));
#24812=CARTESIAN_POINT('Ctrl Pts',(22.3206014106346,-94.4612861286342,1.));
#24813=CARTESIAN_POINT('Ctrl Pts',(22.3995767828725,-94.525606373815,1.));
#24814=CARTESIAN_POINT('Ctrl Pts',(22.481392277051,-94.5856769718859,1.));
#24815=CARTESIAN_POINT('Ctrl Pts',(22.5632787219117,-94.6457996633891,1.));
#24816=CARTESIAN_POINT('Ctrl Pts',(22.6480107936424,-94.7016661711405,1.));
#24817=CARTESIAN_POINT('Ctrl Pts',(22.7353064390419,-94.7529669283351,1.));
#24818=CARTESIAN_POINT('Ctrl Pts',(22.8208383089763,-94.8032311731532,1.));
#24819=CARTESIAN_POINT('Ctrl Pts',(22.9088318714074,-94.8491129760966,1.));
#24820=CARTESIAN_POINT('Ctrl Pts',(22.999055576298,-94.8902850239913,1.));
#24821=CARTESIAN_POINT('Ctrl Pts',(23.036845885043,-94.9075299864265,1.));
#24822=CARTESIAN_POINT('Ctrl Pts',(23.0750277978348,-94.9239481874739,1.00000000000001));
#24823=CARTESIAN_POINT('Ctrl Pts',(23.1135856932339,-94.9395132002532,1.00000000000001));
#24824=CARTESIAN_POINT('Ctrl Pts',(23.1435994051255,-94.9516291055513,1.00000000000001));
#24825=CARTESIAN_POINT('Ctrl Pts',(23.1738409492154,-94.963228017135,1.));
#24826=CARTESIAN_POINT('Ctrl Pts',(23.2042985533737,-94.9743125149969,1.));
#24827=CARTESIAN_POINT('Ctrl Pts',(24.7937992825328,-94.9692229537457,0.999999999999999));
#24828=CARTESIAN_POINT('Ctrl Pts',(24.8886355742656,-94.9345314145989,0.999999999999998));
#24829=CARTESIAN_POINT('Ctrl Pts',(24.9814286349627,-94.8948494551214,0.999999999999999));
#24830=CARTESIAN_POINT('Ctrl Pts',(25.0719375317936,-94.8504973230204,1.));
#24831=CARTESIAN_POINT('Ctrl Pts',(25.1637179471699,-94.8055221078804,1.));
#24832=CARTESIAN_POINT('Ctrl Pts',(25.2531502379127,-94.7557438784068,1.));
#24833=CARTESIAN_POINT('Ctrl Pts',(25.3399491478545,-94.7014558894208,1.));
#24834=CARTESIAN_POINT('Ctrl Pts',(25.364457897529,-94.6861270018428,1.));
#24835=CARTESIAN_POINT('Ctrl Pts',(25.3887564517354,-94.67043834813,1.));
#24836=CARTESIAN_POINT('Ctrl Pts',(25.412837792733,-94.6543960746657,1.));
#24837=CARTESIAN_POINT('Ctrl Pts',(25.4321685186508,-94.6415185197377,1.));
#24838=CARTESIAN_POINT('Ctrl Pts',(25.4513613841745,-94.6284114764054,1.));
#24839=CARTESIAN_POINT('Ctrl Pts',(25.4703934705292,-94.6150918899927,1.));
#24840=CARTESIAN_POINT('Ctrl Pts',(25.5531011015752,-94.5572090379411,1.));
#24841=CARTESIAN_POINT('Ctrl Pts',(25.632853897381,-94.4952643972528,1.));
#24842=CARTESIAN_POINT('Ctrl Pts',(25.7093855024759,-94.4295552060846,1.));
#24843=CARTESIAN_POINT('Ctrl Pts',(25.7683983469888,-94.378887429332,1.));
#24844=CARTESIAN_POINT('Ctrl Pts',(25.8254952962918,-94.3259804090005,1.));
#24845=CARTESIAN_POINT('Ctrl Pts',(25.8805366461498,-94.2709586395016,1.));
#24846=CARTESIAN_POINT('Ctrl Pts',(25.9098567594312,-94.2416489565302,1.));
#24847=CARTESIAN_POINT('Ctrl Pts',(25.9385932961873,-94.2117390404666,1.));
#24848=CARTESIAN_POINT('Ctrl Pts',(25.9667231095721,-94.1812468751386,1.));
#24849=CARTESIAN_POINT('Ctrl Pts',(25.9763570926068,-94.1708038267102,1.));
#24850=CARTESIAN_POINT('Ctrl Pts',(25.9859191110483,-94.1602932638038,1.));
#24851=CARTESIAN_POINT('Ctrl Pts',(25.9954016781335,-94.1497234370175,1.));
#24852=CARTESIAN_POINT('Ctrl Pts',(26.0611941651552,-94.0763872628137,1.));
#24853=CARTESIAN_POINT('Ctrl Pts',(26.1232544023175,-94.0001047398696,0.999999999999999));
#24854=CARTESIAN_POINT('Ctrl Pts',(26.1813385985981,-93.9211542875407,1.));
#24855=CARTESIAN_POINT('Ctrl Pts',(26.2389163893977,-93.842892162577,1.));
#24856=CARTESIAN_POINT('Ctrl Pts',(26.2925876041462,-93.762007641982,1.));
#24857=CARTESIAN_POINT('Ctrl Pts',(26.3420689684564,-93.6787495211355,1.));
#24858=CARTESIAN_POINT('Ctrl Pts',(26.3901173500934,-93.5979025594445,1.));
#24859=CARTESIAN_POINT('Ctrl Pts',(26.4342152491803,-93.5148167861772,1.));
#24860=CARTESIAN_POINT('Ctrl Pts',(26.4740555020368,-93.429709682334,1.));
#24861=CARTESIAN_POINT('Ctrl Pts',(26.4948667676164,-93.3852524710013,1.));
#24862=CARTESIAN_POINT('Ctrl Pts',(26.5145154386263,-93.3402435934832,1.));
#24863=CARTESIAN_POINT('Ctrl Pts',(26.532952028064,-93.2947138132593,1.));
#24864=CARTESIAN_POINT('Ctrl Pts',(26.5400926949078,-93.2770796953468,1.));
#24865=CARTESIAN_POINT('Ctrl Pts',(26.547051495376,-93.2593674387298,1.));
#24866=CARTESIAN_POINT('Ctrl Pts',(26.5538253857067,-93.2415788398828,1.));
#24867=CARTESIAN_POINT('Ctrl Pts',(26.5589792735639,-93.2280444543052,1.));
#24868=CARTESIAN_POINT('Ctrl Pts',(26.5640260787941,-93.2144657552044,1.));
#24869=CARTESIAN_POINT('Ctrl Pts',(26.5689596304255,-93.2008574378807,1.));
#24870=CARTESIAN_POINT('Ctrl Pts',(26.6006314839344,-93.113496310445,1.));
#24871=CARTESIAN_POINT('Ctrl Pts',(26.6276946267098,-93.0247742554061,0.999999999999999));
#24872=CARTESIAN_POINT('Ctrl Pts',(26.6498977732891,-92.9349146801924,0.999999999999999));
#24873=CARTESIAN_POINT('Ctrl Pts',(26.6549003687673,-92.9146684009979,0.999999999999999));
#24874=CARTESIAN_POINT('Ctrl Pts',(26.6596560432156,-92.8943643360308,0.999999999999998));
#24875=CARTESIAN_POINT('Ctrl Pts',(26.6641615567933,-92.8740049843512,0.999999999999998));
#24876=CARTESIAN_POINT('Ctrl Pts',(26.6845070859586,-92.7820683435573,0.999999999999998));
#24877=CARTESIAN_POINT('Ctrl Pts',(26.6997556148125,-92.6890040030942,0.999999999999999));
#24878=CARTESIAN_POINT('Ctrl Pts',(26.7100170529272,-92.595203704688,1.));
#24879=CARTESIAN_POINT('Ctrl Pts',(26.7207301965764,-92.4972743443061,1.));
#24880=CARTESIAN_POINT('Ctrl Pts',(26.7260075138338,-92.3985415671608,0.999999999999998));
#24881=CARTESIAN_POINT('Ctrl Pts',(26.7259165861328,-92.2994658529915,0.999999999999999));
#24882=CARTESIAN_POINT('Ctrl Pts',(26.7258814692617,-92.2612021661132,0.999999999999999));
#24883=CARTESIAN_POINT('Ctrl Pts',(26.7250450624305,-92.222887581006,0.999999999999999));
#24884=CARTESIAN_POINT('Ctrl Pts',(26.7234091242744,-92.1845498020633,0.999999999999999));
#24885=CARTESIAN_POINT('Ctrl Pts',(26.7228215216315,-92.1707794892028,0.999999999999999));
#24886=CARTESIAN_POINT('Ctrl Pts',(26.722130776784,-92.1570079821017,0.999999999999998));
#24887=CARTESIAN_POINT('Ctrl Pts',(26.7213378612372,-92.1432482330244,0.999999999999999));
#24888=CARTESIAN_POINT('Ctrl Pts',(26.7159862604779,-92.050379977503,0.999999999999999));
#24889=CARTESIAN_POINT('Ctrl Pts',(26.7059789499977,-91.9578988173241,0.999999999999997));
#24890=CARTESIAN_POINT('Ctrl Pts',(26.6914389868445,-91.8661766502431,0.999999999999998));
#24891=CARTESIAN_POINT('Ctrl Pts',(26.676936071269,-91.7746881896765,0.999999999999999));
#24892=CARTESIAN_POINT('Ctrl Pts',(26.6579231603966,-91.683953915049,0.999999999999998));
#24893=CARTESIAN_POINT('Ctrl Pts',(26.6344737838481,-91.5943600002269,0.999999999999998));
#24894=CARTESIAN_POINT('Ctrl Pts',(26.6114257043356,-91.5062993360817,0.999999999999999));
#24895=CARTESIAN_POINT('Ctrl Pts',(26.5840912373207,-91.419339551705,0.999999999999997));
#24896=CARTESIAN_POINT('Ctrl Pts',(26.5524998666087,-91.3338765542973,0.999999999999997));
#24897=CARTESIAN_POINT('Ctrl Pts',(26.536637392274,-91.2909643737748,0.999999999999997));
#24898=CARTESIAN_POINT('Ctrl Pts',(26.5197010773947,-91.2484300966479,0.999999999999998));
#24899=CARTESIAN_POINT('Ctrl Pts',(26.5016912656601,-91.2063276214363,0.999999999999997));
#24900=CARTESIAN_POINT('Ctrl Pts',(26.4963919502112,-91.1939391356146,0.999999999999997));
#24901=CARTESIAN_POINT('Ctrl Pts',(26.490999676596,-91.1815880543971,0.999999999999999));
#24902=CARTESIAN_POINT('Ctrl Pts',(26.4855144190875,-91.1692757996963,0.999999999999999));
#24903=CARTESIAN_POINT('Ctrl Pts',(26.4799210003024,-91.1567207652927,0.999999999999999));
#24904=CARTESIAN_POINT('Ctrl Pts',(26.4742345745685,-91.1442143922703,0.999999999999999));
#24905=CARTESIAN_POINT('Ctrl Pts',(26.468456430893,-91.1317600156219,0.999999999999999));
#24906=CARTESIAN_POINT('Ctrl Pts',(26.4309710579662,-91.0509629673911,0.999999999999999));
#24907=CARTESIAN_POINT('Ctrl Pts',(26.3896159814395,-90.9723227777881,0.999999999999999));
#24908=CARTESIAN_POINT('Ctrl Pts',(26.3444610244852,-90.8961871512465,0.999999999999998));
#24909=CARTESIAN_POINT('Ctrl Pts',(26.3000642489853,-90.8213298919974,0.999999999999998));
#24910=CARTESIAN_POINT('Ctrl Pts',(26.2519936723523,-90.7488931258933,0.999999999999997));
#24911=CARTESIAN_POINT('Ctrl Pts',(26.2002794587303,-90.6792415175287,0.999999999999997));
#24912=CARTESIAN_POINT('Ctrl Pts',(26.1501451852494,-90.6117178613118,0.999999999999997));
#24913=CARTESIAN_POINT('Ctrl Pts',(26.0965860669473,-90.5468113408745,1.));
#24914=CARTESIAN_POINT('Ctrl Pts',(26.0396018951918,-90.4848944918556,1.));
#24915=CARTESIAN_POINT('Ctrl Pts',(26.0184128483334,-90.4618712737448,1.));
#24916=CARTESIAN_POINT('Ctrl Pts',(25.9967499854721,-90.4392618665325,0.999999999999998));
#24917=CARTESIAN_POINT('Ctrl Pts',(25.9746124571306,-90.4170870902725,0.999999999999998));
#24918=CARTESIAN_POINT('Ctrl Pts',(25.9557856680546,-90.3982286238251,0.999999999999998));
#24919=CARTESIAN_POINT('Ctrl Pts',(25.9366155517544,-90.3796845329471,0.999999999999999));
#24920=CARTESIAN_POINT('Ctrl Pts',(25.9171118396844,-90.3614597340102,0.999999999999999));
#24921=CARTESIAN_POINT('Origin',(24.,-92.,12.2084234471775));
#24922=CARTESIAN_POINT('Ctrl Pts',(20.9232328435277,-91.9980626432727,9.70842344717746));
#24923=CARTESIAN_POINT('Ctrl Pts',(20.9222986726779,-91.8738980500464,9.70197366100994));
#24924=CARTESIAN_POINT('Ctrl Pts',(20.9853330132547,-90.7368858898031,9.64286281975954));
#24925=CARTESIAN_POINT('Ctrl Pts',(22.4009680446668,-88.7444871744531,9.53109092342626));
#24926=CARTESIAN_POINT('Ctrl Pts',(25.8523951731073,-88.8820464105141,9.37310775817762));
#24927=CARTESIAN_POINT('Ctrl Pts',(27.6235721938174,-91.847285073477,9.215124592929));
#24928=CARTESIAN_POINT('Ctrl Pts',(26.1080771138749,-94.9512425629647,9.05714142768035));
#24929=CARTESIAN_POINT('Ctrl Pts',(22.6804686869861,-95.3782238204297,8.89915826243172));
#24930=CARTESIAN_POINT('Ctrl Pts',(21.0391556852518,-93.4378982357329,8.78291893559742));
#24931=CARTESIAN_POINT('Ctrl Pts',(20.9237203439564,-92.2133137839327,8.719340663846));
#24932=CARTESIAN_POINT('Ctrl Pts',(20.925632185667,-92.002679085539,8.70842344717746));
#24933=CARTESIAN_POINT('Ctrl Pts',(20.9297109890477,-92.0031050978172,9.79157655282255));
#24934=CARTESIAN_POINT('Ctrl Pts',(20.9347146650535,-91.3096207752369,9.75572892504928));
#24935=CARTESIAN_POINT('Ctrl Pts',(21.5077566649197,-89.5876413967006,9.66722024219313));
#24936=CARTESIAN_POINT('Ctrl Pts',(24.3539160472627,-88.3911616367202,9.5260505042541));
#24937=CARTESIAN_POINT('Ctrl Pts',(27.2156039267669,-90.322924702785,9.36806733900546));
#24938=CARTESIAN_POINT('Ctrl Pts',(27.1618223030447,-93.7771165220753,9.21008417375683));
#24939=CARTESIAN_POINT('Ctrl Pts',(24.2395757220273,-95.6187839878382,9.0521010085082));
#24940=CARTESIAN_POINT('Ctrl Pts',(21.4675381047453,-94.3468885879088,8.91259846819676));
#24941=CARTESIAN_POINT('Ctrl Pts',(20.9339207778366,-92.6595175431003,8.82575698296822));
#24942=CARTESIAN_POINT('Ctrl Pts',(20.9296146841086,-91.99786424691,8.79157655282255));
#24943=CARTESIAN_POINT('Ctrl Pts',(25.913465996665,-90.364012796625,10.));
#24944=CARTESIAN_POINT('Ctrl Pts',(26.4547800806522,-90.9971388327508,9.94733894491712));
#24945=CARTESIAN_POINT('Ctrl Pts',(26.8501256748086,-92.8326016501471,9.84201683475137));
#24946=CARTESIAN_POINT('Ctrl Pts',(24.8579877031057,-94.8458064948082,9.68403366950272));
#24947=CARTESIAN_POINT('Ctrl Pts',(22.0866997272543,-94.2718360144008,9.5260505042541));
#24948=CARTESIAN_POINT('Ctrl Pts',(21.0512847401283,-91.6401113487858,9.36806733900546));
#24949=CARTESIAN_POINT('Ctrl Pts',(22.6902349284037,-89.3334135225916,9.21008417375683));
#24950=CARTESIAN_POINT('Ctrl Pts',(25.5172945659013,-89.4460881205366,9.05210100850819));
#24951=CARTESIAN_POINT('Ctrl Pts',(26.9680634449115,-91.8749113949823,8.89411784325956));
#24952=CARTESIAN_POINT('Ctrl Pts',(25.7267233233057,-94.4173590864694,8.73613467801093));
#24953=CARTESIAN_POINT('Ctrl Pts',(22.9191735544127,-94.7670988996037,8.57815151276228));
#24954=CARTESIAN_POINT('Ctrl Pts',(21.0919764590838,-92.6070250632274,8.42016834751366));
#24955=CARTESIAN_POINT('Ctrl Pts',(21.9024529386513,-89.8963394365792,8.26218518226502));
#24956=CARTESIAN_POINT('Ctrl Pts',(24.6154776819786,-89.0937552116682,8.10420201701638));
#24957=CARTESIAN_POINT('Ctrl Pts',(26.7702424329594,-90.9272295704909,7.94621885176776));
#24958=CARTESIAN_POINT('Ctrl Pts',(26.4123030989785,-93.7337455944376,7.78823568651911));
#24959=CARTESIAN_POINT('Ctrl Pts',(23.8663223428292,-94.9676940765812,7.63025252127049));
#24960=CARTESIAN_POINT('Ctrl Pts',(21.441591869785,-93.5098432815441,7.47226935602184));
#24961=CARTESIAN_POINT('Ctrl Pts',(21.3374248530143,-90.6825128295981,7.31428619077321));
#24962=CARTESIAN_POINT('Ctrl Pts',(23.6483043944151,-89.0501883402777,7.15630302552458));
#24963=CARTESIAN_POINT('Ctrl Pts',(26.2781838441901,-90.0934436458725,6.99831986027595));
#24964=CARTESIAN_POINT('Ctrl Pts',(26.8416727928904,-92.8660106707762,6.84033669502731));
#24965=CARTESIAN_POINT('Ctrl Pts',(24.8276675236541,-94.8530764431805,6.68235352977868));
#24966=CARTESIAN_POINT('Ctrl Pts',(22.0629395615723,-94.2523045074984,6.52437036453004));
#24967=CARTESIAN_POINT('Ctrl Pts',(21.055191532594,-91.6086155038653,6.36638719928141));
#24968=CARTESIAN_POINT('Ctrl Pts',(22.7184852964603,-89.3199255988148,6.20840403403277));
#24969=CARTESIAN_POINT('Ctrl Pts',(25.5441566371433,-89.4621546514439,6.05042086878414));
#24970=CARTESIAN_POINT('Ctrl Pts',(26.9692252026282,-91.9062960577465,5.89243770353551));
#24971=CARTESIAN_POINT('Ctrl Pts',(25.7011051632761,-94.4354301377776,5.73445453828687));
#24972=CARTESIAN_POINT('Ctrl Pts',(22.8900246784809,-94.7555459564984,5.57647137303824));
#24973=CARTESIAN_POINT('Ctrl Pts',(21.0857296961368,-92.5762875399299,5.4184882077896));
#24974=CARTESIAN_POINT('Ctrl Pts',(21.9247773496847,-89.8743166547494,5.26050504254097));
#24975=CARTESIAN_POINT('Ctrl Pts',(24.6461227788815,-89.1004131178103,5.10252187729233));
#24976=CARTESIAN_POINT('Ctrl Pts',(26.781412794043,-90.9565338521763,4.9445387120437));
#24977=CARTESIAN_POINT('Ctrl Pts',(26.3938664694978,-93.759113998276,4.78655554679506));
#24978=CARTESIAN_POINT('Ctrl Pts',(23.8350015491774,-94.9661177057642,4.62857238154643));
#24979=CARTESIAN_POINT('Ctrl Pts',(21.4257958558034,-93.4827514138513,4.4705892162978));
#24980=CARTESIAN_POINT('Ctrl Pts',(21.3514811837096,-90.6544789807379,4.31260605104916));
#24981=CARTESIAN_POINT('Ctrl Pts',(23.6794634788655,-89.0466400362912,4.15462288580053));
#24982=CARTESIAN_POINT('Ctrl Pts',(26.2981833367367,-90.1175993861324,3.99663972055189));
#24983=CARTESIAN_POINT('Ctrl Pts',(26.8323724714771,-92.8959603376101,3.83865655530326));
#24984=CARTESIAN_POINT('Ctrl Pts',(24.7975030889958,-94.8616546930815,3.68067339005462));
#24985=CARTESIAN_POINT('Ctrl Pts',(22.0392712060536,-94.231730544535,3.52269022480599));
#24986=CARTESIAN_POINT('Ctrl Pts',(21.059487218677,-91.5775506652918,3.36470705955735));
#24987=CARTESIAN_POINT('Ctrl Pts',(22.7468487806939,-89.3065466558476,3.20672389430872));
#24988=CARTESIAN_POINT('Ctrl Pts',(25.5708610860458,-89.4785969587254,3.04874072906008));
#24989=CARTESIAN_POINT('Ctrl Pts',(26.9700491479982,-91.9376454809303,2.89075756381145));
#24990=CARTESIAN_POINT('Ctrl Pts',(25.6753004854886,-94.4532524972207,2.73277439856281));
#24991=CARTESIAN_POINT('Ctrl Pts',(22.86099868006,-94.7436740950584,2.57479123331418));
#24992=CARTESIAN_POINT('Ctrl Pts',(21.0798067232474,-92.5454930495189,2.41680806806554));
#24993=CARTESIAN_POINT('Ctrl Pts',(21.9473363281977,-89.8525242277567,2.25882490281691));
#24994=CARTESIAN_POINT('Ctrl Pts',(24.6766884907984,-89.1074034480955,2.10084173756828));
#24995=CARTESIAN_POINT('Ctrl Pts',(26.7922885760843,-90.9859374299123,1.94285857231964));
#24996=CARTESIAN_POINT('Ctrl Pts',(26.3751314870431,-93.7843200921868,1.78487540707101));
#24997=CARTESIAN_POINT('Ctrl Pts',(23.8037637139843,-94.96414237307,1.62689224182237));
#24998=CARTESIAN_POINT('Ctrl Pts',(21.4101547923376,-93.4556338085585,1.46890907657374));
#24999=CARTESIAN_POINT('Ctrl Pts',(21.3661021422765,-90.6263102241947,1.3109259113251));
#25000=CARTESIAN_POINT('Ctrl Pts',(23.7101077338689,-89.0440028274616,1.15294274607647));
#25001=CARTESIAN_POINT('Ctrl Pts',(26.3190522551594,-90.1407651728699,0.994959580827836));
#25002=CARTESIAN_POINT('Ctrl Pts',(26.8204142519502,-92.9282808397392,0.836976415579201));
#25003=CARTESIAN_POINT('Ctrl Pts',(25.4549268544596,-94.2169491679593,0.731654305413445));
#25004=CARTESIAN_POINT('Ctrl Pts',(24.6501999979751,-94.4320868020351,0.678993250330566));
#25005=CARTESIAN_POINT('Ctrl Pts',(26.0543315503421,-90.2435746787731,10.1070022498898));
#25006=CARTESIAN_POINT('Ctrl Pts',(26.6354960985062,-90.923310192037,10.0543411948069));
#25007=CARTESIAN_POINT('Ctrl Pts',(27.0599462474923,-92.893896124491,9.94901908464118));
#25008=CARTESIAN_POINT('Ctrl Pts',(24.9211510480811,-95.0553090980671,9.79103591939255));
#25009=CARTESIAN_POINT('Ctrl Pts',(21.945846373842,-94.4390840546534,9.6330527541439));
#25010=CARTESIAN_POINT('Ctrl Pts',(20.8342061986536,-91.6136170634397,9.47506958889528));
#25011=CARTESIAN_POINT('Ctrl Pts',(22.5938126338247,-89.1371047398789,9.31708642364664));
#25012=CARTESIAN_POINT('Ctrl Pts',(25.6289947683033,-89.2580742171957,9.159103258398));
#25013=CARTESIAN_POINT('Ctrl Pts',(27.1865663612134,-91.8657026211473,9.00112009314937));
#25014=CARTESIAN_POINT('Ctrl Pts',(25.8538412534954,-94.5953202453011,8.84313692790073));
#25015=CARTESIAN_POINT('Ctrl Pts',(22.8396052652705,-94.9708072065457,8.6851537626521));
#25016=CARTESIAN_POINT('Ctrl Pts',(20.8778935608714,-92.6517130387526,8.52717059740347));
#25017=CARTESIAN_POINT('Ctrl Pts',(21.7480357038138,-89.7414721379016,8.36918743215483));
#25018=CARTESIAN_POINT('Ctrl Pts',(24.6607879224527,-88.8798032616766,8.21120426690619));
#25019=CARTESIAN_POINT('Ctrl Pts',(26.9741821605629,-90.8482543491991,8.05322110165757));
#25020=CARTESIAN_POINT('Ctrl Pts',(26.5898920460865,-93.8613804902345,7.89523793640892));
#25021=CARTESIAN_POINT('Ctrl Pts',(23.85648126009,-95.1861698007229,7.7372547711603));
#25022=CARTESIAN_POINT('Ctrl Pts',(21.2532469614236,-93.6209949352398,7.57927160591165));
#25023=CARTESIAN_POINT('Ctrl Pts',(21.1414113764537,-90.5855220494931,7.42128844066304));
#25024=CARTESIAN_POINT('Ctrl Pts',(23.6224132647619,-88.8330290840307,7.26330527541438));
#25025=CARTESIAN_POINT('Ctrl Pts',(26.4458991990222,-89.95308676631,7.10532211016576));
#25026=CARTESIAN_POINT('Ctrl Pts',(27.0508710812515,-92.9297646506441,6.94733894491712));
#25027=CARTESIAN_POINT('Ctrl Pts',(24.8885987574379,-95.0631142455517,6.78935577966849));
#25028=CARTESIAN_POINT('Ctrl Pts',(21.9203370321097,-94.4181146771334,6.63137261441986));
#25029=CARTESIAN_POINT('Ctrl Pts',(20.8384006013954,-91.5798025571788,6.47338944917122));
#25030=CARTESIAN_POINT('Ctrl Pts',(22.6241427376826,-89.1226238620309,6.31540628392259));
#25031=CARTESIAN_POINT('Ctrl Pts',(25.6578343717016,-89.2753235340925,6.15742311867394));
#25032=CARTESIAN_POINT('Ctrl Pts',(27.1878136452183,-91.8993977602433,5.99943995342532));
#25033=CARTESIAN_POINT('Ctrl Pts',(25.8263371355742,-94.6147216513961,5.84145678817668));
#25034=CARTESIAN_POINT('Ctrl Pts',(22.8083105071781,-94.9584037587908,5.68347362292805));
#25035=CARTESIAN_POINT('Ctrl Pts',(20.8711869236843,-92.6187126802411,5.52549045767941));
#25036=CARTESIAN_POINT('Ctrl Pts',(21.7720035935013,-89.7178280827588,5.36750729243077));
#25037=CARTESIAN_POINT('Ctrl Pts',(24.6936890503225,-88.8869513096014,5.20952412718214));
#25038=CARTESIAN_POINT('Ctrl Pts',(26.9861748613701,-90.8797159537069,5.05154096193351));
#25039=CARTESIAN_POINT('Ctrl Pts',(26.5700981486823,-93.8886164654116,4.89355779668487));
#25040=CARTESIAN_POINT('Ctrl Pts',(23.8228546920232,-95.1844773806275,4.73557463143624));
#25041=CARTESIAN_POINT('Ctrl Pts',(21.2362880763696,-93.591908618234,4.5775914661876));
#25042=CARTESIAN_POINT('Ctrl Pts',(21.1565025062044,-90.5554244045433,4.41960830093897));
#25043=CARTESIAN_POINT('Ctrl Pts',(23.6558662189184,-88.8292195609754,4.26162513569033));
#25044=CARTESIAN_POINT('Ctrl Pts',(26.4673710143567,-89.9790208040324,4.1036419704417));
#25045=CARTESIAN_POINT('Ctrl Pts',(27.0408860887086,-92.9619191522691,3.94565880519306));
#25046=CARTESIAN_POINT('Ctrl Pts',(24.8562136772092,-95.0723240091164,3.78767563994443));
#25047=CARTESIAN_POINT('Ctrl Pts',(21.8949262594222,-94.3960261000149,3.6296924746958));
#25048=CARTESIAN_POINT('Ctrl Pts',(20.8430125273277,-91.5464507870927,3.47170930944716));
#25049=CARTESIAN_POINT('Ctrl Pts',(22.6545942851051,-89.1082599879432,3.31372614419853));
#25050=CARTESIAN_POINT('Ctrl Pts',(25.686504748918,-89.2929762912711,3.1557429789499));
#25051=CARTESIAN_POINT('Ctrl Pts',(27.1886982478045,-91.9330550654913,2.99775981370126));
#25052=CARTESIAN_POINT('Ctrl Pts',(25.7986327688294,-94.6338560574266,2.83977664845263));
#25053=CARTESIAN_POINT('Ctrl Pts',(22.7771476725941,-94.9456579145687,2.68179348320399));
#25054=CARTESIAN_POINT('Ctrl Pts',(20.8648279133335,-92.585651160811,2.52381031795536));
#25055=CARTESIAN_POINT('Ctrl Pts',(21.7962233190588,-89.6944313407169,2.36582715270672));
#25056=CARTESIAN_POINT('Ctrl Pts',(24.7265049490419,-88.8944562540726,2.20784398745809));
#25057=CARTESIAN_POINT('Ctrl Pts',(26.997851296813,-90.9112841642428,2.04986082220945));
#25058=CARTESIAN_POINT('Ctrl Pts',(26.5499839341528,-93.9156781817274,1.89187765696082));
#25059=CARTESIAN_POINT('Ctrl Pts',(23.7893171896513,-95.1823566278765,1.73389449171218));
#25060=CARTESIAN_POINT('Ctrl Pts',(21.2194955489797,-93.5627946688774,1.57591132646355));
#25061=CARTESIAN_POINT('Ctrl Pts',(21.1721998306057,-90.5251819202757,1.41792816121491));
#25062=CARTESIAN_POINT('Ctrl Pts',(23.6887664429097,-88.826388206087,1.25994499596628));
#25063=CARTESIAN_POINT('Ctrl Pts',(26.4897762609679,-90.0038920098267,1.10196183071765));
#25064=CARTESIAN_POINT('Ctrl Pts',(27.0280475288895,-92.9966190253592,0.943978665469011));
#25065=CARTESIAN_POINT('Ctrl Pts',(25.5620356702265,-94.3801565479507,0.838656555303256));
#25066=CARTESIAN_POINT('Ctrl Pts',(24.698066426161,-94.6111321859386,0.785995500220377));
#25067=CARTESIAN_POINT('Ctrl Pts',(26.1951971040191,-90.1231365609212,10.2140044997796));
#25068=CARTESIAN_POINT('Ctrl Pts',(26.8162121163602,-90.8494815513233,10.1613434446967));
#25069=CARTESIAN_POINT('Ctrl Pts',(27.269766820176,-92.9551905988348,10.056021334531));
#25070=CARTESIAN_POINT('Ctrl Pts',(24.9843143930565,-95.2648117013261,9.89803816928236));
#25071=CARTESIAN_POINT('Ctrl Pts',(21.8049930204297,-94.6063320949058,9.74005500403372));
#25072=CARTESIAN_POINT('Ctrl Pts',(20.6171276571787,-91.5871227780939,9.58207183878508));
#25073=CARTESIAN_POINT('Ctrl Pts',(22.4973903392457,-88.9407959571659,9.42408867353645));
#25074=CARTESIAN_POINT('Ctrl Pts',(25.7406949707053,-89.070060313855,9.26610550828781));
#25075=CARTESIAN_POINT('Ctrl Pts',(27.4050692775154,-91.856493847312,9.10812234303918));
#25076=CARTESIAN_POINT('Ctrl Pts',(25.9809591836852,-94.773281404133,8.95013917779054));
#25077=CARTESIAN_POINT('Ctrl Pts',(22.7600369761283,-95.1745155134876,8.79215601254191));
#25078=CARTESIAN_POINT('Ctrl Pts',(20.663810662659,-92.6964010142779,8.63417284729327));
#25079=CARTESIAN_POINT('Ctrl Pts',(21.5936184689764,-89.5866048392241,8.47618968204464));
#25080=CARTESIAN_POINT('Ctrl Pts',(24.7060981629267,-88.6658513116848,8.31820651679601));
#25081=CARTESIAN_POINT('Ctrl Pts',(27.1781218881664,-90.7692791279071,8.16022335154737));
#25082=CARTESIAN_POINT('Ctrl Pts',(26.7674809931943,-93.9890153860317,8.00224018629874));
#25083=CARTESIAN_POINT('Ctrl Pts',(23.8466401773509,-95.4046455248643,7.84425702105011));
#25084=CARTESIAN_POINT('Ctrl Pts',(21.0649020530622,-93.7321465889358,7.68627385580147));
#25085=CARTESIAN_POINT('Ctrl Pts',(20.945397899893,-90.488531269388,7.52829069055284));
#25086=CARTESIAN_POINT('Ctrl Pts',(23.5965221351088,-88.6158698277836,7.37030752530419));
#25087=CARTESIAN_POINT('Ctrl Pts',(26.6136145538544,-89.8127298867477,7.21232436005558));
#25088=CARTESIAN_POINT('Ctrl Pts',(27.2600693696125,-92.9935186305118,7.05434119480693));
#25089=CARTESIAN_POINT('Ctrl Pts',(24.9495299912216,-95.2731520479227,6.8963580295583));
#25090=CARTESIAN_POINT('Ctrl Pts',(21.7777345026472,-94.5839248467686,6.73837486430966));
#25091=CARTESIAN_POINT('Ctrl Pts',(20.6216096701967,-91.5509896104921,6.58039169906103));
#25092=CARTESIAN_POINT('Ctrl Pts',(22.529800178905,-88.9253221252473,6.42240853381239));
#25093=CARTESIAN_POINT('Ctrl Pts',(25.77151210626,-89.0884924167409,6.26442536856375));
#25094=CARTESIAN_POINT('Ctrl Pts',(27.4064020878083,-91.8924994627401,6.10644220331513));
#25095=CARTESIAN_POINT('Ctrl Pts',(25.9515691078724,-94.7940131650148,5.94845903806649));
#25096=CARTESIAN_POINT('Ctrl Pts',(22.7265963358753,-95.1612615610832,5.79047587281786));
#25097=CARTESIAN_POINT('Ctrl Pts',(20.6566441512317,-92.6611378205523,5.63249270756922));
#25098=CARTESIAN_POINT('Ctrl Pts',(21.6192298373179,-89.5613395107682,5.47450954232059));
#25099=CARTESIAN_POINT('Ctrl Pts',(24.7412553217635,-88.6734895013924,5.31652637707195));
#25100=CARTESIAN_POINT('Ctrl Pts',(27.1909369286972,-90.8028980552376,5.15854321182332));
#25101=CARTESIAN_POINT('Ctrl Pts',(26.7463298278667,-94.0181189325472,5.00056004657468));
#25102=CARTESIAN_POINT('Ctrl Pts',(23.8107078348689,-95.4028370554907,4.84257688132605));
#25103=CARTESIAN_POINT('Ctrl Pts',(21.0467802969359,-93.701065822617,4.68459371607741));
#25104=CARTESIAN_POINT('Ctrl Pts',(20.9615238286993,-90.4563698283487,4.52661055082878));
#25105=CARTESIAN_POINT('Ctrl Pts',(23.6322689589712,-88.6117990856597,4.36862738558015));
#25106=CARTESIAN_POINT('Ctrl Pts',(26.6365586919768,-89.8404422219323,4.21064422033151));
#25107=CARTESIAN_POINT('Ctrl Pts',(27.2493997059402,-93.0278779669281,4.05266105508288));
#25108=CARTESIAN_POINT('Ctrl Pts',(24.9149242654226,-95.2829933251511,3.89467788983424));
#25109=CARTESIAN_POINT('Ctrl Pts',(21.7505813127907,-94.5603216554948,3.73669472458561));
#25110=CARTESIAN_POINT('Ctrl Pts',(20.6265378359784,-91.5153509088937,3.57871155933697));
#25111=CARTESIAN_POINT('Ctrl Pts',(22.5623397895163,-88.9099733200387,3.42072839408834));
#25112=CARTESIAN_POINT('Ctrl Pts',(25.80214841179,-89.1073556238167,3.2627452288397));
#25113=CARTESIAN_POINT('Ctrl Pts',(27.4073473476108,-91.9284646500524,3.10476206359107));
#25114=CARTESIAN_POINT('Ctrl Pts',(25.9219650521703,-94.8144596176324,2.94677889834244));
#25115=CARTESIAN_POINT('Ctrl Pts',(22.6932966651281,-95.1476417340791,2.7887957330938));
#25116=CARTESIAN_POINT('Ctrl Pts',(20.6498491034196,-92.625809272103,2.63081256784516));
#25117=CARTESIAN_POINT('Ctrl Pts',(21.6451103099198,-89.5363384536772,2.47282940259654));
#25118=CARTESIAN_POINT('Ctrl Pts',(24.7763214072854,-88.6815090600494,2.3148462373479));
#25119=CARTESIAN_POINT('Ctrl Pts',(27.2034140175416,-90.8366308985733,2.15686307209927));
#25120=CARTESIAN_POINT('Ctrl Pts',(26.7248363812625,-94.047036271268,1.99887990685063));
#25121=CARTESIAN_POINT('Ctrl Pts',(23.7748706653183,-95.4005708826832,1.840896741602));
#25122=CARTESIAN_POINT('Ctrl Pts',(21.0288363056219,-93.6699555291963,1.68291357635336));
#25123=CARTESIAN_POINT('Ctrl Pts',(20.9782975189348,-90.4240536163567,1.52493041110473));
#25124=CARTESIAN_POINT('Ctrl Pts',(23.6674251519506,-88.6087735847125,1.36694724585609));
#25125=CARTESIAN_POINT('Ctrl Pts',(26.6605002667764,-89.8670188467833,1.20896408060746));
#25126=CARTESIAN_POINT('Ctrl Pts',(27.2356808058288,-93.0649572109792,1.05098091535882));
#25127=CARTESIAN_POINT('Ctrl Pts',(25.6691444859934,-94.5433639279422,0.945658805193066));
#25128=CARTESIAN_POINT('Ctrl Pts',(24.7459328543469,-94.7901775698421,0.892997750110188));
#25129=CARTESIAN_POINT('Ctrl Pts',(26.3360626576961,-90.0026984430693,10.3210067496694));
#25130=CARTESIAN_POINT('Ctrl Pts',(26.9969281342143,-90.7756529106096,10.2683456945866));
#25131=CARTESIAN_POINT('Ctrl Pts',(27.4795873928596,-93.0164850731786,10.1630235844208));
#25132=CARTESIAN_POINT('Ctrl Pts',(25.0474777380319,-95.4743143045851,10.0050404191722));
#25133=CARTESIAN_POINT('Ctrl Pts',(21.6641396670173,-94.7735801351584,9.84705725392352));
#25134=CARTESIAN_POINT('Ctrl Pts',(20.4000491157039,-91.5606284927479,9.6890740886749));
#25135=CARTESIAN_POINT('Ctrl Pts',(22.4009680446668,-88.7444871744531,9.53109092342626));
#25136=CARTESIAN_POINT('Ctrl Pts',(25.8523951731073,-88.8820464105141,9.37310775817762));
#25137=CARTESIAN_POINT('Ctrl Pts',(27.6235721938174,-91.847285073477,9.215124592929));
#25138=CARTESIAN_POINT('Ctrl Pts',(26.1080771138749,-94.9512425629647,9.05714142768035));
#25139=CARTESIAN_POINT('Ctrl Pts',(22.6804686869861,-95.3782238204297,8.89915826243172));
#25140=CARTESIAN_POINT('Ctrl Pts',(20.4497277644465,-92.7410889898032,8.74117509718309));
#25141=CARTESIAN_POINT('Ctrl Pts',(21.4392012341389,-89.4317375405466,8.58319193193445));
#25142=CARTESIAN_POINT('Ctrl Pts',(24.7514084034007,-88.4518993616932,8.42520876668581));
#25143=CARTESIAN_POINT('Ctrl Pts',(27.3820616157699,-90.6903039066151,8.26722560143718));
#25144=CARTESIAN_POINT('Ctrl Pts',(26.9450699403022,-94.1166502818289,8.10924243618855));
#25145=CARTESIAN_POINT('Ctrl Pts',(23.8367990946118,-95.6231212490058,7.95125927093992));
#25146=CARTESIAN_POINT('Ctrl Pts',(20.8765571447007,-93.8432982426317,7.79327610569128));
#25147=CARTESIAN_POINT('Ctrl Pts',(20.7493844233325,-90.391540489283,7.63529294044265));
#25148=CARTESIAN_POINT('Ctrl Pts',(23.5706310054557,-88.3987105715367,7.47730977519401));
#25149=CARTESIAN_POINT('Ctrl Pts',(26.7813299086865,-89.6723730071853,7.31932660994538));
#25150=CARTESIAN_POINT('Ctrl Pts',(27.4692676579736,-93.0572726103796,7.16134344469675));
#25151=CARTESIAN_POINT('Ctrl Pts',(25.0104612250054,-95.483189850294,7.00336027944811));
#25152=CARTESIAN_POINT('Ctrl Pts',(21.6351319731846,-94.7497350164036,6.84537711419948));
#25153=CARTESIAN_POINT('Ctrl Pts',(20.4048187389981,-91.5221766638055,6.68739394895084));
#25154=CARTESIAN_POINT('Ctrl Pts',(22.4354576201274,-88.7280203884636,6.52941078370221));
#25155=CARTESIAN_POINT('Ctrl Pts',(25.8851898408183,-88.9016612993893,6.37142761845357));
#25156=CARTESIAN_POINT('Ctrl Pts',(27.6249905303984,-91.885601165237,6.21344445320494));
#25157=CARTESIAN_POINT('Ctrl Pts',(26.0768010801705,-94.9733046786333,6.0554612879563));
#25158=CARTESIAN_POINT('Ctrl Pts',(22.6448821645724,-95.3641193633754,5.89747812270767));
#25159=CARTESIAN_POINT('Ctrl Pts',(20.4421013787792,-92.7035629608637,5.73949495745903));
#25160=CARTESIAN_POINT('Ctrl Pts',(21.4664560811345,-89.4048509387775,5.5815117922104));
#25161=CARTESIAN_POINT('Ctrl Pts',(24.7888215932045,-88.4600276931838,5.42352862696176));
#25162=CARTESIAN_POINT('Ctrl Pts',(27.3956989960243,-90.726080156768,5.26554546171313));
#25163=CARTESIAN_POINT('Ctrl Pts',(26.9225615070512,-94.1476213996829,5.10756229646449));
#25164=CARTESIAN_POINT('Ctrl Pts',(23.7985609777147,-95.6211967303539,4.94957913121586));
#25165=CARTESIAN_POINT('Ctrl Pts',(20.8572725175022,-93.8102230269998,4.79159596596722));
#25166=CARTESIAN_POINT('Ctrl Pts',(20.7665451511942,-90.3573152521542,4.6336128007186));
#25167=CARTESIAN_POINT('Ctrl Pts',(23.6086716990241,-88.3943786103439,4.47562963546995));
#25168=CARTESIAN_POINT('Ctrl Pts',(26.8057463695968,-89.7018636398323,4.31764647022133));
#25169=CARTESIAN_POINT('Ctrl Pts',(27.4579133231717,-93.0938367815869,4.15966330497269));
#25170=CARTESIAN_POINT('Ctrl Pts',(24.9736348536359,-95.4936626411861,4.00168013972405));
#25171=CARTESIAN_POINT('Ctrl Pts',(21.6062363661592,-94.7246172109745,3.84369697447542));
#25172=CARTESIAN_POINT('Ctrl Pts',(20.410063144629,-91.4842510306948,3.68571380922679));
#25173=CARTESIAN_POINT('Ctrl Pts',(22.4700852939276,-88.7116866521341,3.52773064397815));
#25174=CARTESIAN_POINT('Ctrl Pts',(25.9177920746621,-88.9217349563625,3.36974747872952));
#25175=CARTESIAN_POINT('Ctrl Pts',(27.6259964474171,-91.9238742346134,3.21176431348088));
#25176=CARTESIAN_POINT('Ctrl Pts',(26.0452973355111,-94.9950631778383,3.05378114823225));
#25177=CARTESIAN_POINT('Ctrl Pts',(22.6094456576622,-95.3496255535895,2.89579798298361));
#25178=CARTESIAN_POINT('Ctrl Pts',(20.4348702935058,-92.665967383395,2.73781481773498));
#25179=CARTESIAN_POINT('Ctrl Pts',(21.4939973007808,-89.3782455666376,2.57983165248634));
#25180=CARTESIAN_POINT('Ctrl Pts',(24.8261378655289,-88.4685618660265,2.42184848723771));
#25181=CARTESIAN_POINT('Ctrl Pts',(27.4089767382702,-90.7619776329038,2.26386532198907));
#25182=CARTESIAN_POINT('Ctrl Pts',(26.8996888283721,-94.1783943608088,2.10588215674044));
#25183=CARTESIAN_POINT('Ctrl Pts',(23.7604241409854,-95.6187851374897,1.9478989914918));
#25184=CARTESIAN_POINT('Ctrl Pts',(20.838177062264,-93.7771163895153,1.78991582624317));
#25185=CARTESIAN_POINT('Ctrl Pts',(20.7843952072639,-90.3229253124378,1.63193266099454));
#25186=CARTESIAN_POINT('Ctrl Pts',(23.6460838609915,-88.3911589633379,1.4739494957459));
#25187=CARTESIAN_POINT('Ctrl Pts',(26.8312242725849,-89.7301456837401,1.31596633049727));
#25188=CARTESIAN_POINT('Ctrl Pts',(27.4433140827682,-93.1332953965992,1.15798316524863));
#25189=CARTESIAN_POINT('Ctrl Pts',(25.7762533017603,-94.7065713079336,1.05266105508288));
#25190=CARTESIAN_POINT('Ctrl Pts',(24.7937992825328,-94.9692229537457,0.999999999999999));
#25191=CARTESIAN_POINT('Ctrl Pts',(25.913465996665,-90.364012796625,10.));
#25192=CARTESIAN_POINT('Ctrl Pts',(25.9750770578958,-90.42191206544,10.));
#25193=CARTESIAN_POINT('Ctrl Pts',(26.0333190151654,-90.4829618973507,10.));
#25194=CARTESIAN_POINT('Ctrl Pts',(26.088194198786,-90.5467775157042,10.));
#25195=CARTESIAN_POINT('Ctrl Pts',(26.1445220900387,-90.6122825213128,10.));
#25196=CARTESIAN_POINT('Ctrl Pts',(26.1973030283134,-90.6807021204442,10.));
#25197=CARTESIAN_POINT('Ctrl Pts',(26.2465140266804,-90.7516687130586,10.));
#25198=CARTESIAN_POINT('Ctrl Pts',(26.2970865251746,-90.8245987087349,10.));
#25199=CARTESIAN_POINT('Ctrl Pts',(26.3438893496051,-90.9002191359304,10.));
#25200=CARTESIAN_POINT('Ctrl Pts',(26.3868634537168,-90.9781740458832,10.));
#25201=CARTESIAN_POINT('Ctrl Pts',(26.4057549128521,-91.0124431022419,10.));
#25202=CARTESIAN_POINT('Ctrl Pts',(26.4239059912884,-91.0471637926723,10.));
#25203=CARTESIAN_POINT('Ctrl Pts',(26.4413092551554,-91.0823079492062,10.));
#25204=CARTESIAN_POINT('Ctrl Pts',(26.4512342776009,-91.102350542658,10.));
#25205=CARTESIAN_POINT('Ctrl Pts',(26.460916053907,-91.1225308841626,10.));
#25206=CARTESIAN_POINT('Ctrl Pts',(26.4703529715556,-91.1428438969994,10.));
#25207=CARTESIAN_POINT('Ctrl Pts',(26.4788699915109,-91.1611768254115,10.));
#25208=CARTESIAN_POINT('Ctrl Pts',(26.4871899465583,-91.1796235689466,10.));
#25209=CARTESIAN_POINT('Ctrl Pts',(26.49529795661,-91.1981485646354,10.));
#25210=CARTESIAN_POINT('Ctrl Pts',(26.5318626758695,-91.2816907978493,10.));
#25211=CARTESIAN_POINT('Ctrl Pts',(26.5641670779443,-91.3669165275728,10.));
#25212=CARTESIAN_POINT('Ctrl Pts',(26.5921860624111,-91.4534270378763,10.));
#25213=CARTESIAN_POINT('Ctrl Pts',(26.620667737277,-91.5413661360929,10.));
#25214=CARTESIAN_POINT('Ctrl Pts',(26.6447217851763,-91.6306335526386,10.));
#25215=CARTESIAN_POINT('Ctrl Pts',(26.6642827659638,-91.7208476134984,10.));
#25216=CARTESIAN_POINT('Ctrl Pts',(26.6832631734456,-91.8083841053703,10.));
#25217=CARTESIAN_POINT('Ctrl Pts',(26.6980134264455,-91.8968127992612,10.));
#25218=CARTESIAN_POINT('Ctrl Pts',(26.708432920618,-91.9858069093381,10.));
#25219=CARTESIAN_POINT('Ctrl Pts',(26.7127922670542,-92.0230405936396,10.));
#25220=CARTESIAN_POINT('Ctrl Pts',(26.7163930212362,-92.0603734428051,10.));
#25221=CARTESIAN_POINT('Ctrl Pts',(26.7192254940143,-92.0977821388405,10.));
#25222=CARTESIAN_POINT('Ctrl Pts',(26.7209960695381,-92.1211662723398,10.));
#25223=CARTESIAN_POINT('Ctrl Pts',(26.7224664121851,-92.1445800482928,10.));
#25224=CARTESIAN_POINT('Ctrl Pts',(26.7236338650196,-92.16801780341,10.));
#25225=CARTESIAN_POINT('Ctrl Pts',(26.7243181282437,-92.1817550554931,10.));
#25226=CARTESIAN_POINT('Ctrl Pts',(26.7248980652474,-92.1954959766348,10.));
#25227=CARTESIAN_POINT('Ctrl Pts',(26.7253731538326,-92.2092311923284,10.));
#25228=CARTESIAN_POINT('Ctrl Pts',(26.7287309598136,-92.3063082235341,10.));
#25229=CARTESIAN_POINT('Ctrl Pts',(26.7268615808529,-92.4032207088423,10.));
#25230=CARTESIAN_POINT('Ctrl Pts',(26.7197002220063,-92.4995463878723,10.));
#25231=CARTESIAN_POINT('Ctrl Pts',(26.7125388631598,-92.5958720669024,10.));
#25232=CARTESIAN_POINT('Ctrl Pts',(26.7000859592924,-92.69161199417,10.));
#25233=CARTESIAN_POINT('Ctrl Pts',(26.6822238228945,-92.7863628481204,10.));
#25234=CARTESIAN_POINT('Ctrl Pts',(26.6651462975084,-92.8769516823811,10.));
#25235=CARTESIAN_POINT('Ctrl Pts',(26.6431244275633,-92.9666373988202,10.));
#25236=CARTESIAN_POINT('Ctrl Pts',(26.6164329081475,-93.0551806589545,10.));
#25237=CARTESIAN_POINT('Ctrl Pts',(26.6074980340548,-93.084820143644,10.));
#25238=CARTESIAN_POINT('Ctrl Pts',(26.5980394679049,-93.1143315742049,10.));
#25239=CARTESIAN_POINT('Ctrl Pts',(26.5880662379445,-93.1437057941631,10.));
#25240=CARTESIAN_POINT('Ctrl Pts',(26.5815849548277,-93.1627951600598,10.));
#25241=CARTESIAN_POINT('Ctrl Pts',(26.574886301904,-93.1818265755705,10.));
#25242=CARTESIAN_POINT('Ctrl Pts',(26.5679726206436,-93.2007974926138,10.));
#25243=CARTESIAN_POINT('Ctrl Pts',(26.5613831133059,-93.2188788869321,10.));
#25244=CARTESIAN_POINT('Ctrl Pts',(26.5545965181547,-93.2369095329036,10.));
#25245=CARTESIAN_POINT('Ctrl Pts',(26.5476256545847,-93.2548600742594,10.));
#25246=CARTESIAN_POINT('Ctrl Pts',(26.5137821756247,-93.3420097885806,10.));
#25247=CARTESIAN_POINT('Ctrl Pts',(26.475560354929,-93.4273852002263,10.));
#25248=CARTESIAN_POINT('Ctrl Pts',(26.4332913756107,-93.5107526953461,10.));
#25249=CARTESIAN_POINT('Ctrl Pts',(26.3894531454603,-93.5972152382575,10.));
#25250=CARTESIAN_POINT('Ctrl Pts',(26.3412615514558,-93.6815187324214,10.));
#25251=CARTESIAN_POINT('Ctrl Pts',(26.2890300743574,-93.7633995605516,10.));
#25252=CARTESIAN_POINT('Ctrl Pts',(26.2362101789054,-93.8462028244383,10.));
#25253=CARTESIAN_POINT('Ctrl Pts',(26.1792584552573,-93.9265293490527,10.));
#25254=CARTESIAN_POINT('Ctrl Pts',(26.1184473134232,-94.0040916613995,10.));
#25255=CARTESIAN_POINT('Ctrl Pts',(26.0767848212129,-94.0572305950965,10.));
#25256=CARTESIAN_POINT('Ctrl Pts',(26.0333097149824,-94.1090717581195,10.));
#25257=CARTESIAN_POINT('Ctrl Pts',(25.9880973827582,-94.1595156628907,10.));
#25258=CARTESIAN_POINT('Ctrl Pts',(25.9759903695684,-94.1730235929258,10.));
#25259=CARTESIAN_POINT('Ctrl Pts',(25.9637574536017,-94.1864325457022,10.));
#25260=CARTESIAN_POINT('Ctrl Pts',(25.9514137007238,-94.1997261136577,10.));
#25261=CARTESIAN_POINT('Ctrl Pts',(25.8827528893147,-94.2736701703296,10.));
#25262=CARTESIAN_POINT('Ctrl Pts',(25.810578186298,-94.3441463401242,10.));
#25263=CARTESIAN_POINT('Ctrl Pts',(25.7352000515214,-94.4108648135128,10.));
#25264=CARTESIAN_POINT('Ctrl Pts',(25.6722951822122,-94.4665429867847,10.));
#25265=CARTESIAN_POINT('Ctrl Pts',(25.6071582640081,-94.5196041737155,10.));
#25266=CARTESIAN_POINT('Ctrl Pts',(25.5399460671016,-94.5698661697058,10.));
#25267=CARTESIAN_POINT('Ctrl Pts',(25.5180638151793,-94.5862299505225,10.));
#25268=CARTESIAN_POINT('Ctrl Pts',(25.4959614387747,-94.6022969068063,10.));
#25269=CARTESIAN_POINT('Ctrl Pts',(25.4736439219636,-94.6180603652556,10.));
#25270=CARTESIAN_POINT('Ctrl Pts',(25.4508750769085,-94.6341426089032,10.));
#25271=CARTESIAN_POINT('Ctrl Pts',(25.4278768876981,-94.649912383158,10.));
#25272=CARTESIAN_POINT('Ctrl Pts',(25.4046837834431,-94.665343374446,10.));
#25273=CARTESIAN_POINT('Ctrl Pts',(25.3197384869509,-94.7218597474041,10.));
#25274=CARTESIAN_POINT('Ctrl Pts',(25.2321269167437,-94.773875691111,10.));
#25275=CARTESIAN_POINT('Ctrl Pts',(25.1421393366132,-94.8210831411639,10.));
#25276=CARTESIAN_POINT('Ctrl Pts',(25.0588657411973,-94.8647684374083,10.));
#25277=CARTESIAN_POINT('Ctrl Pts',(24.9735566410333,-94.9043362525237,10.));
#25278=CARTESIAN_POINT('Ctrl Pts',(24.8864146397765,-94.9395136119409,10.));
#25279=CARTESIAN_POINT('Ctrl Pts',(24.8563906944763,-94.9516336355772,10.));
#25280=CARTESIAN_POINT('Ctrl Pts',(24.8261489679874,-94.9632321934335,10.));
#25281=CARTESIAN_POINT('Ctrl Pts',(24.7957018439802,-94.9743128659187,10.));
#25282=CARTESIAN_POINT('Ctrl Pts',(21.4817891743669,-92.002194435609,8.38741669750802));
#25283=CARTESIAN_POINT('Ctrl Pts',(21.4802231872166,-92.1747250532131,8.39833391417657));
#25284=CARTESIAN_POINT('Ctrl Pts',(21.4964591581217,-92.3469627518866,8.40925113084511));
#25285=CARTESIAN_POINT('Ctrl Pts',(21.5315887215666,-92.5152564315154,8.42016834751366));
#25286=CARTESIAN_POINT('Ctrl Pts',(21.7010421575268,-93.3270496753528,8.47282940259653));
#25287=CARTESIAN_POINT('Ctrl Pts',(22.3101078559698,-94.0470742874782,8.52549045767941));
#25288=CARTESIAN_POINT('Ctrl Pts',(23.0825656666734,-94.3487966246852,8.57815151276228));
#25289=CARTESIAN_POINT('Ctrl Pts',(23.8550234773771,-94.6505189618922,8.63081256784516));
#25290=CARTESIAN_POINT('Ctrl Pts',(24.7908734003414,-94.5339390241808,8.68347362292804));
#25291=CARTESIAN_POINT('Ctrl Pts',(25.4656883820912,-94.0519077734106,8.73613467801092));
#25292=CARTESIAN_POINT('Ctrl Pts',(26.1405033638409,-93.5698765226404,8.7887957330938));
#25293=CARTESIAN_POINT('Ctrl Pts',(26.5542834043762,-92.7223939588113,8.84145678817668));
#25294=CARTESIAN_POINT('Ctrl Pts',(26.5193786114755,-91.8938487978225,8.89411784325956));
#25295=CARTESIAN_POINT('Ctrl Pts',(26.4844738185747,-91.0653036368338,8.94677889834244));
#25296=CARTESIAN_POINT('Ctrl Pts',(26.000884192238,-90.2556958786852,8.99943995342531));
#25297=CARTESIAN_POINT('Ctrl Pts',(25.2879127728201,-89.8321128999534,9.05210100850819));
#25298=CARTESIAN_POINT('Ctrl Pts',(24.5749413534021,-89.4085299212216,9.10476206359107));
#25299=CARTESIAN_POINT('Ctrl Pts',(23.6325881409029,-89.3709717219066,9.15742311867395));
#25300=CARTESIAN_POINT('Ctrl Pts',(22.8882531699407,-89.7366422599481,9.21008417375683));
#25301=CARTESIAN_POINT('Ctrl Pts',(22.1439181989786,-90.1023127979897,9.2627452288397));
#25302=CARTESIAN_POINT('Ctrl Pts',(21.5976014695534,-90.8712120733877,9.31540628392258));
#25303=CARTESIAN_POINT('Ctrl Pts',(21.4970122693619,-91.6942824886893,9.36806733900546));
#25304=CARTESIAN_POINT('Ctrl Pts',(21.4846923712707,-91.7950899672169,9.37451712517298));
#25305=CARTESIAN_POINT('Ctrl Pts',(21.4790586980532,-91.8967100507538,9.3809669113405));
#25306=CARTESIAN_POINT('Ctrl Pts',(21.4798238762261,-91.9984131135315,9.38741669750802));
#25307=CARTESIAN_POINT('Ctrl Pts',(23.2062007174671,-94.9692229537457,10.));
#25308=CARTESIAN_POINT('Ctrl Pts',(22.2237466982397,-94.7065713079336,9.94733894491712));
#25309=CARTESIAN_POINT('Ctrl Pts',(20.556684636792,-93.1333040393725,9.84201683475137));
#25310=CARTESIAN_POINT('Ctrl Pts',(21.1687768340777,-89.7301430813077,9.68403366950273));
#25311=CARTESIAN_POINT('Ctrl Pts',(24.3539160472627,-88.3911616367202,9.5260505042541));
#25312=CARTESIAN_POINT('Ctrl Pts',(27.2156039267669,-90.322924702785,9.36806733900546));
#25313=CARTESIAN_POINT('Ctrl Pts',(27.1618223030447,-93.7771165220753,9.21008417375683));
#25314=CARTESIAN_POINT('Ctrl Pts',(24.2395757220273,-95.6187839878382,9.0521010085082));
#25315=CARTESIAN_POINT('Ctrl Pts',(21.1003119065524,-94.1783940085773,8.89411784325955));
#25316=CARTESIAN_POINT('Ctrl Pts',(20.5910240312662,-90.7619778387773,8.73613467801092));
#25317=CARTESIAN_POINT('Ctrl Pts',(23.1738623478633,-88.4685627419331,8.57815151276229));
#25318=CARTESIAN_POINT('Ctrl Pts',(26.5060020988177,-89.3782461595948,8.42016834751365));
#25319=CARTESIAN_POINT('Ctrl Pts',(27.5651288739417,-92.6659672391889,8.26218518226502));
#25320=CARTESIAN_POINT('Ctrl Pts',(25.3905540118639,-95.3496247591348,8.10420201701639));
#25321=CARTESIAN_POINT('Ctrl Pts',(21.9547031474508,-94.9950624766612,7.94621885176775));
#25322=CARTESIAN_POINT('Ctrl Pts',(20.3740044045684,-91.923874250773,7.78823568651912));
#25323=CARTESIAN_POINT('Ctrl Pts',(22.0822083770023,-88.9217356813896,7.63025252127048));
#25324=CARTESIAN_POINT('Ctrl Pts',(25.5299143458989,-88.7116874252054,7.47226935602185));
#25325=CARTESIAN_POINT('Ctrl Pts',(27.5899360110292,-91.4842511522572,7.31428619077322));
#25326=CARTESIAN_POINT('Ctrl Pts',(26.3937630706594,-94.724616569919,7.15630302552458));
#25327=CARTESIAN_POINT('Ctrl Pts',(23.0263653754403,-95.4936618194068,6.99831986027594));
#25328=CARTESIAN_POINT('Ctrl Pts',(20.5420874902395,-93.093836524243,6.84033669502731));
#25329=CARTESIAN_POINT('Ctrl Pts',(21.194254290432,-89.7018641804574,6.68235352977868));
#25330=CARTESIAN_POINT('Ctrl Pts',(24.3913282089151,-88.3943794585145,6.52437036453004));
#25331=CARTESIAN_POINT('Ctrl Pts',(27.2334540881776,-90.35731563858,6.3663871992814));
#25332=CARTESIAN_POINT('Ctrl Pts',(27.1427267432077,-93.8102226011646,6.20840403403277));
#25333=CARTESIAN_POINT('Ctrl Pts',(24.2014389748999,-95.6211958785123,6.05042086878413));
#25334=CARTESIAN_POINT('Ctrl Pts',(21.0774391804456,-94.1476208944804,5.89243770353551));
#25335=CARTESIAN_POINT('Ctrl Pts',(20.604301802773,-90.7260804564426,5.73445453828686));
#25336=CARTESIAN_POINT('Ctrl Pts',(23.2111785923562,-88.4600285259193,5.57647137303824));
#25337=CARTESIAN_POINT('Ctrl Pts',(26.53354332288,-89.404851549255,5.4184882077896));
#25338=CARTESIAN_POINT('Ctrl Pts',(27.5578977842682,-92.7035627953589,5.26050504254097));
#25339=CARTESIAN_POINT('Ctrl Pts',(25.3551175166524,-95.3641185720074,5.10252187729234));
#25340=CARTESIAN_POINT('Ctrl Pts',(21.9231994083718,-94.973303979199,4.94453871204369));
#25341=CARTESIAN_POINT('Ctrl Pts',(20.3750103223368,-91.8856011921486,4.78655554679507));
#25342=CARTESIAN_POINT('Ctrl Pts',(22.1148106026499,-88.9016620282347,4.62857238154642));
#25343=CARTESIAN_POINT('Ctrl Pts',(25.564542011833,-88.7280211581599,4.4705892162978));
#25344=CARTESIAN_POINT('Ctrl Pts',(27.595180415279,-91.5221767762026,4.31260605104916));
#25345=CARTESIAN_POINT('Ctrl Pts',(26.3648674705088,-94.7497343695717,4.15462288580052));
#25346=CARTESIAN_POINT('Ctrl Pts',(22.9895390126931,-95.4831890308962,3.99663972055189));
#25347=CARTESIAN_POINT('Ctrl Pts',(20.5307331581304,-93.0572723617073,3.83865655530325));
#25348=CARTESIAN_POINT('Ctrl Pts',(21.2186707455856,-89.6723735546569,3.68067339005462));
#25349=CARTESIAN_POINT('Ctrl Pts',(24.429368893546,-88.3987114188411,3.52269022480599));
#25350=CARTESIAN_POINT('Ctrl Pts',(27.2506148119859,-90.3915408673734,3.36470705955735));
#25351=CARTESIAN_POINT('Ctrl Pts',(27.1234421205799,-93.8432978095595,3.20672389430872));
#25352=CARTESIAN_POINT('Ctrl Pts',(24.1632008669201,-95.6231203956682,3.04874072906008));
#25353=CARTESIAN_POINT('Ctrl Pts',(21.0549307526672,-94.1166497859116,2.89075756381145));
#25354=CARTESIAN_POINT('Ctrl Pts',(20.6179391794157,-90.6903042108868,2.73277439856281));
#25355=CARTESIAN_POINT('Ctrl Pts',(23.2485917742673,-88.4519002035991,2.57479123331418));
#25356=CARTESIAN_POINT('Ctrl Pts',(26.5607981614372,-89.4317381309793,2.41680806806554));
#25357=CARTESIAN_POINT('Ctrl Pts',(27.5502714048858,-92.7410888412383,2.25882490281691));
#25358=CARTESIAN_POINT('Ctrl Pts',(25.3195309927208,-95.3782229777193,2.10084173756827));
#25359=CARTESIAN_POINT('Ctrl Pts',(21.8919234036861,-94.9512419574066,1.94285857231964));
#25360=CARTESIAN_POINT('Ctrl Pts',(20.3764286113538,-91.8472849474597,1.78487540707101));
#25361=CARTESIAN_POINT('Ctrl Pts',(22.1476053652116,-88.8820474355396,1.62689224182237));
#25362=CARTESIAN_POINT('Ctrl Pts',(25.5990313571955,-88.7444874247256,1.46890907657374));
#25363=CARTESIAN_POINT('Ctrl Pts',(27.5999505159819,-91.5606294856851,1.3109259113251));
#25364=CARTESIAN_POINT('Ctrl Pts',(26.33585874306,-94.7735779839873,1.15294274607647));
#25365=CARTESIAN_POINT('Ctrl Pts',(22.9525246480966,-95.4743158223952,0.994959580827833));
#25366=CARTESIAN_POINT('Ctrl Pts',(20.5204066563018,-93.0164786759463,0.836976415579198));
#25367=CARTESIAN_POINT('Ctrl Pts',(21.0030718657857,-90.7756529106095,0.731654305413442));
#25368=CARTESIAN_POINT('Ctrl Pts',(21.6639373423039,-90.0026984430693,0.678993250330564));
#25369=CARTESIAN_POINT('Ctrl Pts',(23.2540671456531,-94.7901775698421,10.1070022498898));
#25370=CARTESIAN_POINT('Ctrl Pts',(22.3308555140066,-94.5433639279422,10.0543411948069));
#25371=CARTESIAN_POINT('Ctrl Pts',(20.7643179909424,-93.0649653325897,9.94901908464118));
#25372=CARTESIAN_POINT('Ctrl Pts',(21.339500773154,-89.8670164012787,9.79103591939255));
#25373=CARTESIAN_POINT('Ctrl Pts',(24.3325747618359,-88.6087760968887,9.63305275414391));
#25374=CARTESIAN_POINT('Ctrl Pts',(27.0217016673143,-90.4240530434662,9.47506958889526));
#25375=CARTESIAN_POINT('Ctrl Pts',(26.971163097959,-93.669955653763,9.31708642364665));
#25376=CARTESIAN_POINT('Ctrl Pts',(24.2251292059547,-95.400569802356,9.159103258398));
#25377=CARTESIAN_POINT('Ctrl Pts',(21.2751643093458,-94.0470359402763,9.00112009314937));
#25378=CARTESIAN_POINT('Ctrl Pts',(20.7965867055914,-90.8366310920326,8.84313692790074));
#25379=CARTESIAN_POINT('Ctrl Pts',(23.2236787932392,-88.6815098831386,8.6851537626521));
#25380=CARTESIAN_POINT('Ctrl Pts',(26.3548891258831,-89.536339010879,8.52717059740346));
#25381=CARTESIAN_POINT('Ctrl Pts',(27.3501501142311,-92.6258091365926,8.36918743215483));
#25382=CARTESIAN_POINT('Ctrl Pts',(25.3067030243257,-95.1476409875303,8.2112042669062));
#25383=CARTESIAN_POINT('Ctrl Pts',(22.0780354016688,-94.8144589587367,8.05322110165756));
#25384=CARTESIAN_POINT('Ctrl Pts',(20.5926534529996,-91.9284646652375,7.89523793640892));
#25385=CARTESIAN_POINT('Ctrl Pts',(22.1978520126389,-89.1073563051246,7.7372547711603));
#25386=CARTESIAN_POINT('Ctrl Pts',(25.4376598720287,-88.9099740464932,7.57927160591165));
#25387=CARTESIAN_POINT('Ctrl Pts',(27.3734613705941,-91.5153510231261,7.42128844066303));
#25388=CARTESIAN_POINT('Ctrl Pts',(26.249418157988,-94.5603210530949,7.26330527541438));
#25389=CARTESIAN_POINT('Ctrl Pts',(23.0850759498403,-95.2829925529257,7.10532211016576));
#25390=CARTESIAN_POINT('Ctrl Pts',(20.750601058422,-93.0278777251019,6.94733894491711));
#25391=CARTESIAN_POINT('Ctrl Pts',(21.363441928252,-89.8404427299575,6.78935577966849));
#25392=CARTESIAN_POINT('Ctrl Pts',(24.3677309545192,-88.6117998826852,6.63137261441985));
#25393=CARTESIAN_POINT('Ctrl Pts',(27.0384754565387,-90.4563701914731,6.47338944917122));
#25394=CARTESIAN_POINT('Ctrl Pts',(26.9532190083535,-93.7010654224597,6.31540628392258));
#25395=CARTESIAN_POINT('Ctrl Pts',(24.1892921206031,-95.4028362550155,6.15742311867394));
#25396=CARTESIAN_POINT('Ctrl Pts',(21.2536708181737,-94.0181184578086,5.99943995342532));
#25397=CARTESIAN_POINT('Ctrl Pts',(20.8090638219323,-90.8028983368416,5.84145678817667));
#25398=CARTESIAN_POINT('Ctrl Pts',(23.2587448526078,-88.6734902839137,5.68347362292805));
#25399=CARTESIAN_POINT('Ctrl Pts',(26.3807696026348,-89.5613400844337,5.52549045767941));
#25400=CARTESIAN_POINT('Ctrl Pts',(27.3433550622842,-92.6611376650277,5.36750729243077));
#25401=CARTESIAN_POINT('Ctrl Pts',(25.2734033645719,-95.1612608174347,5.20952412718215));
#25402=CARTESIAN_POINT('Ctrl Pts',(22.0484313512106,-94.7940125077567,5.0515409619335));
#25403=CARTESIAN_POINT('Ctrl Pts',(20.5935987135065,-91.8924994880289,4.89355779668487));
#25404=CARTESIAN_POINT('Ctrl Pts',(22.2284883104669,-89.0884931016367,4.73557463143624));
#25405=CARTESIAN_POINT('Ctrl Pts',(25.4701994752483,-88.9253228485306,4.5775914661876));
#25406=CARTESIAN_POINT('Ctrl Pts',(27.3783895350778,-91.5509897161116,4.41960830093897));
#25407=CARTESIAN_POINT('Ctrl Pts',(26.2222649745918,-94.5839242389409,4.26162513569033));
#25408=CARTESIAN_POINT('Ctrl Pts',(23.0504702321435,-95.273151277935,4.1036419704417));
#25409=CARTESIAN_POINT('Ctrl Pts',(20.73993139728,-92.9935183968345,3.94565880519306));
#25410=CARTESIAN_POINT('Ctrl Pts',(21.3863860609648,-89.8127304012066,3.78767563994443));
#25411=CARTESIAN_POINT('Ctrl Pts',(24.4034777699831,-88.6158706239953,3.6296924746958));
#25412=CARTESIAN_POINT('Ctrl Pts',(27.0546013815359,-90.4885316246794,3.47170930944716));
#25413=CARTESIAN_POINT('Ctrl Pts',(26.9350972565224,-93.7321461819781,3.31372614419853));
#25414=CARTESIAN_POINT('Ctrl Pts',(24.1533597865007,-95.4046447229832,3.15574297894989));
#25415=CARTESIAN_POINT('Ctrl Pts',(21.2325196579888,-93.9890149200185,2.99775981370126));
#25416=CARTESIAN_POINT('Ctrl Pts',(20.8218788590692,-90.769279413831,2.83977664845262));
#25417=CARTESIAN_POINT('Ctrl Pts',(23.2939020040279,-88.6658521028235,2.68179348320399));
#25418=CARTESIAN_POINT('Ctrl Pts',(26.4063809630468,-89.5866053940534,2.52381031795535));
#25419=CARTESIAN_POINT('Ctrl Pts',(27.336188556763,-92.6964008746716,2.36582715270672));
#25420=CARTESIAN_POINT('Ctrl Pts',(25.2399627228924,-95.174514721593,2.20784398745808));
#25421=CARTESIAN_POINT('Ctrl Pts',(22.0190413026667,-94.7732808350901,2.04986082220945));
#25422=CARTESIAN_POINT('Ctrl Pts',(20.5949314791037,-91.8564937288938,1.89187765696081));
#25423=CARTESIAN_POINT('Ctrl Pts',(22.2593055351527,-89.0700612770709,1.73389449171218));
#25424=CARTESIAN_POINT('Ctrl Pts',(25.5026090986845,-88.9407961923469,1.57591132646355));
#25425=CARTESIAN_POINT('Ctrl Pts',(27.3828719967166,-91.5871237111565,1.41792816121491));
#25426=CARTESIAN_POINT('Ctrl Pts',(26.1950054855207,-94.6063300734514,1.25994499596628));
#25427=CARTESIAN_POINT('Ctrl Pts',(23.0156878491875,-95.2648131276117,1.10196183071764));
#25428=CARTESIAN_POINT('Ctrl Pts',(20.7302275878235,-92.9551845873582,0.943978665469009));
#25429=CARTESIAN_POINT('Ctrl Pts',(21.1837878836398,-90.8494815513233,0.838656555303253));
#25430=CARTESIAN_POINT('Ctrl Pts',(21.8048028959809,-90.1231365609212,0.785995500220375));
#25431=CARTESIAN_POINT('Ctrl Pts',(23.301933573839,-94.6111321859386,10.2140044997796));
#25432=CARTESIAN_POINT('Ctrl Pts',(22.4379643297735,-94.3801565479507,10.1613434446967));
#25433=CARTESIAN_POINT('Ctrl Pts',(20.9719513450928,-92.9966266258069,10.056021334531));
#25434=CARTESIAN_POINT('Ctrl Pts',(21.5102247122303,-90.0038897212497,9.89803816928235));
#25435=CARTESIAN_POINT('Ctrl Pts',(24.3112334764091,-88.8263905570572,9.74005500403372));
#25436=CARTESIAN_POINT('Ctrl Pts',(26.8277994078617,-90.5251813841474,9.58207183878508));
#25437=CARTESIAN_POINT('Ctrl Pts',(26.7805038928733,-93.5627947854507,9.42408867353645));
#25438=CARTESIAN_POINT('Ctrl Pts',(24.2106826898821,-95.1823556168738,9.26610550828782));
#25439=CARTESIAN_POINT('Ctrl Pts',(21.4500167121393,-93.9156778719755,9.10812234303918));
#25440=CARTESIAN_POINT('Ctrl Pts',(21.0021493799167,-90.9112843452878,8.95013917779055));
#25441=CARTESIAN_POINT('Ctrl Pts',(23.273495238615,-88.8944570243441,8.79215601254191));
#25442=CARTESIAN_POINT('Ctrl Pts',(26.2037761529486,-89.6944318621631,8.63417284729328));
#25443=CARTESIAN_POINT('Ctrl Pts',(27.1351713545205,-92.5856510339964,8.47618968204464));
#25444=CARTESIAN_POINT('Ctrl Pts',(25.2228520367874,-94.9456572159259,8.31820651679601));
#25445=CARTESIAN_POINT('Ctrl Pts',(22.2013676558868,-94.633855440812,8.16022335154738));
#25446=CARTESIAN_POINT('Ctrl Pts',(20.8113025014308,-91.933055079702,8.00224018629874));
#25447=CARTESIAN_POINT('Ctrl Pts',(22.3134956482754,-89.2929769288594,7.8442570210501));
#25448=CARTESIAN_POINT('Ctrl Pts',(25.3454053981585,-89.1082606677813,7.68627385580147));
#25449=CARTESIAN_POINT('Ctrl Pts',(27.1569867301589,-91.5464508939948,7.52829069055284));
#25450=CARTESIAN_POINT('Ctrl Pts',(26.1050732453166,-94.3960255362711,7.37030752530419));
#25451=CARTESIAN_POINT('Ctrl Pts',(23.1437865242403,-95.0723232864444,7.21232436005558));
#25452=CARTESIAN_POINT('Ctrl Pts',(20.9591146266045,-92.961918925961,7.05434119480693));
#25453=CARTESIAN_POINT('Ctrl Pts',(21.5326295660721,-89.9790212794577,6.8963580295583));
#25454=CARTESIAN_POINT('Ctrl Pts',(24.3441337001234,-88.8292203068559,6.73837486430966));
#25455=CARTESIAN_POINT('Ctrl Pts',(26.8434968248997,-90.5554247443661,6.58039169906103));
#25456=CARTESIAN_POINT('Ctrl Pts',(26.7637112734993,-93.5919082437549,6.4224085338124));
#25457=CARTESIAN_POINT('Ctrl Pts',(24.1771452663062,-95.1844766315186,6.26442536856376));
#25458=CARTESIAN_POINT('Ctrl Pts',(21.4299024559019,-93.888616021137,6.10644220331513));
#25459=CARTESIAN_POINT('Ctrl Pts',(21.0138258410916,-90.8797162172404,5.94845903806649));
#25460=CARTESIAN_POINT('Ctrl Pts',(23.3063111128594,-88.8869520419084,5.79047587281785));
#25461=CARTESIAN_POINT('Ctrl Pts',(26.2279958823895,-89.7178286196122,5.63249270756922));
#25462=CARTESIAN_POINT('Ctrl Pts',(27.1288123403003,-92.6187125346964,5.47450954232059));
#25463=CARTESIAN_POINT('Ctrl Pts',(25.1916892124913,-94.9584030628622,5.31652637707195));
#25464=CARTESIAN_POINT('Ctrl Pts',(22.1736632940494,-94.6147210363142,5.15854321182332));
#25465=CARTESIAN_POINT('Ctrl Pts',(20.8121871046763,-91.8993977839094,5.00056004657468));
#25466=CARTESIAN_POINT('Ctrl Pts',(22.3421660182839,-89.2753241750383,4.84257688132605));
#25467=CARTESIAN_POINT('Ctrl Pts',(25.3758569386636,-89.1226245389013,4.68459371607741));
#25468=CARTESIAN_POINT('Ctrl Pts',(27.1615986548766,-91.5798026560206,4.52661055082878));
#25469=CARTESIAN_POINT('Ctrl Pts',(26.0796624786747,-94.41811410831,4.36862738558014));
#25470=CARTESIAN_POINT('Ctrl Pts',(23.111401451594,-95.0631135249739,4.21064422033151));
#25471=CARTESIAN_POINT('Ctrl Pts',(20.9491296364297,-92.9297644319617,4.05266105508288));
#25472=CARTESIAN_POINT('Ctrl Pts',(21.5541013763441,-89.9530872477562,3.89467788983424));
#25473=CARTESIAN_POINT('Ctrl Pts',(24.3775866464203,-88.8330298291496,3.73669472458561));
#25474=CARTESIAN_POINT('Ctrl Pts',(26.8585879510859,-90.5855223819854,3.57871155933697));
#25475=CARTESIAN_POINT('Ctrl Pts',(26.7467523924649,-93.6209945543966,3.42072839408834));
#25476=CARTESIAN_POINT('Ctrl Pts',(24.1435187060812,-95.1861690502982,3.2627452288397));
#25477=CARTESIAN_POINT('Ctrl Pts',(21.4101085633103,-93.8613800541255,3.10476206359107));
#25478=CARTESIAN_POINT('Ctrl Pts',(21.0258185387226,-90.8482546167753,2.94677889834243));
#25479=CARTESIAN_POINT('Ctrl Pts',(23.3392122337884,-88.8798040020478,2.7887957330938));
#25480=CARTESIAN_POINT('Ctrl Pts',(26.2519637646563,-89.7414726571277,2.63081256784516));
#25481=CARTESIAN_POINT('Ctrl Pts',(27.1221057086401,-92.6517129081048,2.47282940259653));
#25482=CARTESIAN_POINT('Ctrl Pts',(25.1603944530641,-94.9708064654669,2.31484623734789));
#25483=CARTESIAN_POINT('Ctrl Pts',(22.1461592016473,-94.5953197127737,2.15686307209926));
#25484=CARTESIAN_POINT('Ctrl Pts',(20.8134343468535,-91.8657025103278,1.99887990685063));
#25485=CARTESIAN_POINT('Ctrl Pts',(22.3710057050938,-89.2580751186022,1.84089674160199));
#25486=CARTESIAN_POINT('Ctrl Pts',(25.4061868401735,-89.1371049599684,1.68291357635336));
#25487=CARTESIAN_POINT('Ctrl Pts',(27.1657934774512,-91.6136179366278,1.52493041110472));
#25488=CARTESIAN_POINT('Ctrl Pts',(26.0541522279814,-94.4390821629154,1.36694724585609));
#25489=CARTESIAN_POINT('Ctrl Pts',(23.0788510502783,-95.0553104328282,1.20896408060746));
#25490=CARTESIAN_POINT('Ctrl Pts',(20.9400485193453,-92.8938904987702,1.05098091535882));
#25491=CARTESIAN_POINT('Ctrl Pts',(21.3645039014938,-90.923310192037,0.945658805193063));
#25492=CARTESIAN_POINT('Ctrl Pts',(21.9456684496579,-90.2435746787731,0.892997750110186));
#25493=CARTESIAN_POINT('Ctrl Pts',(23.3498000020249,-94.4320868020351,10.3210067496694));
#25494=CARTESIAN_POINT('Ctrl Pts',(22.5450731455404,-94.2169491679593,10.2683456945866));
#25495=CARTESIAN_POINT('Ctrl Pts',(21.1795846992431,-92.9282879190241,10.1630235844208));
#25496=CARTESIAN_POINT('Ctrl Pts',(21.6809486513066,-90.1407630412208,10.0050404191722));
#25497=CARTESIAN_POINT('Ctrl Pts',(24.2898921909822,-89.0440050172257,9.84705725392353));
#25498=CARTESIAN_POINT('Ctrl Pts',(26.6338971484092,-90.6263097248287,9.68907408867489));
#25499=CARTESIAN_POINT('Ctrl Pts',(26.5898446877875,-93.4556339171384,9.53109092342626));
#25500=CARTESIAN_POINT('Ctrl Pts',(24.1962361738095,-94.9641414313917,9.37310775817762));
#25501=CARTESIAN_POINT('Ctrl Pts',(21.6248691149327,-93.7843198036745,9.21512459292899));
#25502=CARTESIAN_POINT('Ctrl Pts',(21.2077120542419,-90.985937598543,9.05714142768035));
#25503=CARTESIAN_POINT('Ctrl Pts',(23.3233116839909,-89.1074041655495,8.89915826243173));
#25504=CARTESIAN_POINT('Ctrl Pts',(26.0526631800141,-89.8525247134473,8.74117509718308));
#25505=CARTESIAN_POINT('Ctrl Pts',(26.9201925948099,-92.5454929314,8.58319193193445));
#25506=CARTESIAN_POINT('Ctrl Pts',(25.1390010492492,-94.7436734443214,8.42520876668582));
#25507=CARTESIAN_POINT('Ctrl Pts',(22.3246999101049,-94.4532519228875,8.26722560143718));
#25508=CARTESIAN_POINT('Ctrl Pts',(21.029951549862,-91.9376454941666,8.10924243618855));
#25509=CARTESIAN_POINT('Ctrl Pts',(22.4291392839119,-89.4785975525942,7.95125927093991));
#25510=CARTESIAN_POINT('Ctrl Pts',(25.2531509242884,-89.3065472890693,7.79327610569128));
#25511=CARTESIAN_POINT('Ctrl Pts',(26.9405120897238,-91.5775507648634,7.63529294044265));
#25512=CARTESIAN_POINT('Ctrl Pts',(25.9607283326452,-94.2317300194472,7.47730977519401));
#25513=CARTESIAN_POINT('Ctrl Pts',(23.2024970986403,-94.8616540199631,7.31932660994538));
#25514=CARTESIAN_POINT('Ctrl Pts',(21.167628194787,-92.8959601268202,7.16134344469674));
#25515=CARTESIAN_POINT('Ctrl Pts',(21.7018172038921,-90.1175998289577,7.00336027944811));
#25516=CARTESIAN_POINT('Ctrl Pts',(24.3205364457276,-89.0466407310266,6.84537711419947));
#25517=CARTESIAN_POINT('Ctrl Pts',(26.6485181932608,-90.6544792972588,6.68739394895084));
#25518=CARTESIAN_POINT('Ctrl Pts',(26.574203538645,-93.4827510650503,6.52941078370221));
#25519=CARTESIAN_POINT('Ctrl Pts',(24.1649984120093,-94.9661170080216,6.37142761845356));
#25520=CARTESIAN_POINT('Ctrl Pts',(21.60613409363,-93.7591135844654,6.21344445320494));
#25521=CARTESIAN_POINT('Ctrl Pts',(21.2185878602508,-90.9565340976392,6.0554612879563));
#25522=CARTESIAN_POINT('Ctrl Pts',(23.353877373111,-89.100413799903,5.89747812270767));
#25523=CARTESIAN_POINT('Ctrl Pts',(26.0752221621443,-89.8743171547908,5.73949495745903));
#25524=CARTESIAN_POINT('Ctrl Pts',(26.9142696183163,-92.5762874043651,5.5815117922104));
#25525=CARTESIAN_POINT('Ctrl Pts',(25.1099750604108,-94.7555453082897,5.42352862696176));
#25526=CARTESIAN_POINT('Ctrl Pts',(22.2988952368883,-94.4354295648718,5.26554546171313));
#25527=CARTESIAN_POINT('Ctrl Pts',(21.030775495846,-91.9062960797898,5.10756229646449));
#25528=CARTESIAN_POINT('Ctrl Pts',(22.4558437261009,-89.4621552484402,4.94957913121586));
#25529=CARTESIAN_POINT('Ctrl Pts',(25.2815144020789,-89.3199262292719,4.79159596596723));
#25530=CARTESIAN_POINT('Ctrl Pts',(26.9448077746754,-91.6086155959298,4.63361280071859));
#25531=CARTESIAN_POINT('Ctrl Pts',(25.9370599827577,-94.252303977679,4.47562963546995));
#25532=CARTESIAN_POINT('Ctrl Pts',(23.1723326710444,-94.8530757720127,4.31764647022132));
#25533=CARTESIAN_POINT('Ctrl Pts',(21.1583278755794,-92.866010467089,4.15966330497269));
#25534=CARTESIAN_POINT('Ctrl Pts',(21.7218166917233,-90.0934440943057,4.00168013972405));
#25535=CARTESIAN_POINT('Ctrl Pts',(24.3516955228574,-89.0501890343038,3.84369697447542));
#25536=CARTESIAN_POINT('Ctrl Pts',(26.6625745206359,-90.6825131392915,3.68571380922678));
#25537=CARTESIAN_POINT('Ctrl Pts',(26.5584075284073,-93.5098429268151,3.52773064397815));
#25538=CARTESIAN_POINT('Ctrl Pts',(24.1336776256617,-94.9676933776133,3.36974747872952));
#25539=CARTESIAN_POINT('Ctrl Pts',(21.5876974686318,-93.7337451882324,3.21176431348088));
#25540=CARTESIAN_POINT('Ctrl Pts',(21.2297582183761,-90.9272298197194,3.05378114823225));
#25541=CARTESIAN_POINT('Ctrl Pts',(23.384522463549,-89.0937559012724,2.89579798298361));
#25542=CARTESIAN_POINT('Ctrl Pts',(26.0975465662659,-89.8963399202019,2.73781481773498));
#25543=CARTESIAN_POINT('Ctrl Pts',(26.9080228605173,-92.6070249415381,2.57983165248634));
#25544=CARTESIAN_POINT('Ctrl Pts',(25.0808261832357,-94.7670982093406,2.42184848723771));
#25545=CARTESIAN_POINT('Ctrl Pts',(22.2732771006279,-94.4173585904574,2.26386532198907));
#25546=CARTESIAN_POINT('Ctrl Pts',(21.0319372146033,-91.8749112917618,2.10588215674044));
#25547=CARTESIAN_POINT('Ctrl Pts',(22.482705875035,-89.4460889601337,1.9478989914918));
#25548=CARTESIAN_POINT('Ctrl Pts',(25.3097645816625,-89.3334137275896,1.78991582624317));
#25549=CARTESIAN_POINT('Ctrl Pts',(26.9487149581859,-91.6401121620993,1.63193266099453));
#25550=CARTESIAN_POINT('Ctrl Pts',(25.913298970442,-94.2718342523794,1.4739494957459));
#25551=CARTESIAN_POINT('Ctrl Pts',(23.1420142513692,-94.8458077380446,1.31596633049727));
#25552=CARTESIAN_POINT('Ctrl Pts',(21.149869450867,-92.8325964101822,1.15798316524863));
#25553=CARTESIAN_POINT('Ctrl Pts',(21.5452199193478,-90.9971388327507,1.05266105508287));
#25554=CARTESIAN_POINT('Ctrl Pts',(22.086534003335,-90.364012796625,0.999999999999996));
#25555=CARTESIAN_POINT('Ctrl Pts',(21.4850512338518,-91.9982506073194,9.11258330249198));
#25556=CARTESIAN_POINT('Ctrl Pts',(21.4831441979475,-91.7052247997765,9.09410267755477));
#25557=CARTESIAN_POINT('Ctrl Pts',(21.5304975843651,-91.4127948855722,9.07562205261756));
#25558=CARTESIAN_POINT('Ctrl Pts',(21.6298381693152,-91.1392457272327,9.05714142768035));
#25559=CARTESIAN_POINT('Ctrl Pts',(21.9129119308249,-90.3597597875452,9.00448037259748));
#25560=CARTESIAN_POINT('Ctrl Pts',(22.6181118074079,-89.7335819765474,8.9518193175146));
#25561=CARTESIAN_POINT('Ctrl Pts',(23.4256036617032,-89.5446798290314,8.89915826243172));
#25562=CARTESIAN_POINT('Ctrl Pts',(24.2330955159986,-89.3557776815154,8.84649720734885));
#25563=CARTESIAN_POINT('Ctrl Pts',(25.1428793480064,-89.6041511974813,8.79383615226596));
#25564=CARTESIAN_POINT('Ctrl Pts',(25.7423594998095,-90.1771659917898,8.74117509718309));
#25565=CARTESIAN_POINT('Ctrl Pts',(26.3418396516127,-90.7501807860982,8.68851404210021));
#25566=CARTESIAN_POINT('Ctrl Pts',(26.6310161232113,-91.6478368587491,8.63585298701733));
#25567=CARTESIAN_POINT('Ctrl Pts',(26.4787391014172,-92.4630283138948,8.58319193193445));
#25568=CARTESIAN_POINT('Ctrl Pts',(26.326462079623,-93.2782197690405,8.53053087685157));
#25569=CARTESIAN_POINT('Ctrl Pts',(25.7327315644361,-94.0109466066809,8.4778698217687));
#25570=CARTESIAN_POINT('Ctrl Pts',(24.9668161169853,-94.3289064385955,8.42520876668582));
#25571=CARTESIAN_POINT('Ctrl Pts',(24.2009006695344,-94.6468662705101,8.37254771160294));
#25572=CARTESIAN_POINT('Ctrl Pts',(23.2628002898197,-94.5500590966988,8.31988665652006));
#25573=CARTESIAN_POINT('Ctrl Pts',(22.5779587065885,-94.082387771673,8.26722560143718));
#25574=CARTESIAN_POINT('Ctrl Pts',(21.907599452313,-93.624606281228,8.21567816845545));
#25575=CARTESIAN_POINT('Ctrl Pts',(21.4799009347915,-92.8114801021923,8.16413073547371));
#25576=CARTESIAN_POINT('Ctrl Pts',(21.4784371162896,-91.9996804085349,8.11258330249198));
#25577=CARTESIAN_POINT('Ctrl Pts',(23.2062007174671,-94.9692229537457,10.));
#25578=CARTESIAN_POINT('Ctrl Pts',(23.113147471668,-94.9351836607662,10.));
#25579=CARTESIAN_POINT('Ctrl Pts',(23.0221595031926,-94.8963760597078,10.));
#25580=CARTESIAN_POINT('Ctrl Pts',(22.9334453118218,-94.8531283773252,10.));
#25581=CARTESIAN_POINT('Ctrl Pts',(22.842765482151,-94.8089224570377,10.));
#25582=CARTESIAN_POINT('Ctrl Pts',(22.7544606379768,-94.7600769016052,10.));
#25583=CARTESIAN_POINT('Ctrl Pts',(22.6687823668502,-94.7068967029881,10.));
#25584=CARTESIAN_POINT('Ctrl Pts',(22.5863298883886,-94.6557187424224,10.));
#25585=CARTESIAN_POINT('Ctrl Pts',(22.5063096394394,-94.60052551816,10.));
#25586=CARTESIAN_POINT('Ctrl Pts',(22.428978843944,-94.5415587834331,10.));
#25587=CARTESIAN_POINT('Ctrl Pts',(22.3613143978855,-94.489962890547,10.));
#25588=CARTESIAN_POINT('Ctrl Pts',(22.2957093551137,-94.4354772056916,10.));
#25589=CARTESIAN_POINT('Ctrl Pts',(22.2323606826166,-94.3782509736056,10.));
#25590=CARTESIAN_POINT('Ctrl Pts',(22.2182619575701,-94.3655148438681,10.));
#25591=CARTESIAN_POINT('Ctrl Pts',(22.2042723901562,-94.3526402704909,10.));
#25592=CARTESIAN_POINT('Ctrl Pts',(22.1904136245077,-94.3396473264407,10.));
#25593=CARTESIAN_POINT('Ctrl Pts',(22.1179828954075,-94.27174168213,10.));
#25594=CARTESIAN_POINT('Ctrl Pts',(22.0490178395323,-94.2005142871089,10.));
#25595=CARTESIAN_POINT('Ctrl Pts',(21.9837584040152,-94.1262557408098,10.));
#25596=CARTESIAN_POINT('Ctrl Pts',(21.9188586588109,-94.0524064852059,10.));
#25597=CARTESIAN_POINT('Ctrl Pts',(21.8576233116571,-93.9755586030696,10.));
#25598=CARTESIAN_POINT('Ctrl Pts',(21.8003319724708,-93.8959711475523,10.));
#25599=CARTESIAN_POINT('Ctrl Pts',(21.7451391407492,-93.8192988773297,10.));
#25600=CARTESIAN_POINT('Ctrl Pts',(21.6936065132598,-93.7400833150407,10.));
#25601=CARTESIAN_POINT('Ctrl Pts',(21.6460290163564,-93.6585424656019,10.));
#25602=CARTESIAN_POINT('Ctrl Pts',(21.6260402555732,-93.6242846622374,10.));
#25603=CARTESIAN_POINT('Ctrl Pts',(21.6067501857392,-93.5896163159495,10.));
#25604=CARTESIAN_POINT('Ctrl Pts',(21.5881832814551,-93.5545532938194,10.));
#25605=CARTESIAN_POINT('Ctrl Pts',(21.5751467282381,-93.5299341679298,10.));
#25606=CARTESIAN_POINT('Ctrl Pts',(21.5624667280488,-93.5051204641926,10.));
#25607=CARTESIAN_POINT('Ctrl Pts',(21.5501522393203,-93.4801176691813,10.));
#25608=CARTESIAN_POINT('Ctrl Pts',(21.5423997338202,-93.4643773237952,10.));
#25609=CARTESIAN_POINT('Ctrl Pts',(21.5347912129392,-93.448559913067,10.));
#25610=CARTESIAN_POINT('Ctrl Pts',(21.5273385775685,-93.4326879328307,10.));
#25611=CARTESIAN_POINT('Ctrl Pts',(21.485218006457,-93.3429831721704,10.));
#25612=CARTESIAN_POINT('Ctrl Pts',(21.4479996497417,-93.2513937088983,10.));
#25613=CARTESIAN_POINT('Ctrl Pts',(21.4159751546732,-93.158192004561,10.));
#25614=CARTESIAN_POINT('Ctrl Pts',(21.3861126932925,-93.0712825219783,10.));
#25615=CARTESIAN_POINT('Ctrl Pts',(21.3607666485933,-92.9829703487196,10.));
#25616=CARTESIAN_POINT('Ctrl Pts',(21.3402240440704,-92.8934677197948,10.));
#25617=CARTESIAN_POINT('Ctrl Pts',(21.3387367653612,-92.8869877549847,10.));
#25618=CARTESIAN_POINT('Ctrl Pts',(21.337274687696,-92.8805015489742,10.));
#25619=CARTESIAN_POINT('Ctrl Pts',(21.335837930805,-92.8740091819891,10.));
#25620=CARTESIAN_POINT('Ctrl Pts',(21.3152523340913,-92.7809877047229,10.));
#25621=CARTESIAN_POINT('Ctrl Pts',(21.2998605243046,-92.68670047643,10.));
#25622=CARTESIAN_POINT('Ctrl Pts',(21.2895854935829,-92.591555525086,10.));
#25623=CARTESIAN_POINT('Ctrl Pts',(21.2837678665552,-92.5376853367153,10.));
#25624=CARTESIAN_POINT('Ctrl Pts',(21.2795914703245,-92.4835403753524,10.));
#25625=CARTESIAN_POINT('Ctrl Pts',(21.2770492198358,-92.4291973958091,10.));
#25626=CARTESIAN_POINT('Ctrl Pts',(21.2764018813561,-92.4153599309664,10.));
#25627=CARTESIAN_POINT('Ctrl Pts',(21.2758606481501,-92.4015110329858,10.));
#25628=CARTESIAN_POINT('Ctrl Pts',(21.2754255840256,-92.3876642045,10.));
#25629=CARTESIAN_POINT('Ctrl Pts',(21.2724967852977,-92.2944490406402,10.));
#25630=CARTESIAN_POINT('Ctrl Pts',(21.2743673782168,-92.2011765908985,10.));
#25631=CARTESIAN_POINT('Ctrl Pts',(21.2809024940929,-92.1082221293118,10.));
#25632=CARTESIAN_POINT('Ctrl Pts',(21.2874480476023,-92.0151192044679,10.));
#25633=CARTESIAN_POINT('Ctrl Pts',(21.298673414762,-91.9223343047028,10.));
#25634=CARTESIAN_POINT('Ctrl Pts',(21.3144939864578,-91.8302566590502,10.));
#25635=CARTESIAN_POINT('Ctrl Pts',(21.3300873891571,-91.7395011645042,10.));
#25636=CARTESIAN_POINT('Ctrl Pts',(21.3501454394612,-91.6494319152931,10.));
#25637=CARTESIAN_POINT('Ctrl Pts',(21.3746301066291,-91.5604468625991,10.));
#25638=CARTESIAN_POINT('Ctrl Pts',(21.3838721759165,-91.5268582490842,10.));
#25639=CARTESIAN_POINT('Ctrl Pts',(21.3937453511932,-91.4934244348921,10.));
#25640=CARTESIAN_POINT('Ctrl Pts',(21.4042490107631,-91.4601681501231,10.));
#25641=CARTESIAN_POINT('Ctrl Pts',(21.4119449035391,-91.4358017090739,10.));
#25642=CARTESIAN_POINT('Ctrl Pts',(21.4199792750966,-91.4115305868297,10.));
#25643=CARTESIAN_POINT('Ctrl Pts',(21.4283521278725,-91.3873640201045,10.));
#25644=CARTESIAN_POINT('Ctrl Pts',(21.433519688148,-91.3724488897959,10.));
#25645=CARTESIAN_POINT('Ctrl Pts',(21.4388131893322,-91.3575822730711,10.));
#25646=CARTESIAN_POINT('Ctrl Pts',(21.4442314441212,-91.3427682605191,10.));
#25647=CARTESIAN_POINT('Ctrl Pts',(21.475937504042,-91.2560809436734,10.));
#25648=CARTESIAN_POINT('Ctrl Pts',(21.5119203351589,-91.1711677990126,10.));
#25649=CARTESIAN_POINT('Ctrl Pts',(21.5521196352014,-91.0884296535818,10.));
#25650=CARTESIAN_POINT('Ctrl Pts',(21.5822691102334,-91.0263760445086,10.));
#25651=CARTESIAN_POINT('Ctrl Pts',(21.6147913381673,-90.9655463573648,10.));
#25652=CARTESIAN_POINT('Ctrl Pts',(21.6496759689102,-90.9061246869587,10.));
#25653=CARTESIAN_POINT('Ctrl Pts',(21.6654548107415,-90.8792473739781,10.));
#25654=CARTESIAN_POINT('Ctrl Pts',(21.6817171386646,-90.8526583243667,10.));
#25655=CARTESIAN_POINT('Ctrl Pts',(21.6984627752329,-90.8263756430687,10.));
#25656=CARTESIAN_POINT('Ctrl Pts',(21.7075848158552,-90.812058379853,10.));
#25657=CARTESIAN_POINT('Ctrl Pts',(21.7168450963549,-90.7978401888656,10.));
#25658=CARTESIAN_POINT('Ctrl Pts',(21.726242936938,-90.7837240829108,10.));
#25659=CARTESIAN_POINT('Ctrl Pts',(21.7738179917341,-90.7122635693628,10.));
#25660=CARTESIAN_POINT('Ctrl Pts',(21.8249182481425,-90.6434123196867,10.));
#25661=CARTESIAN_POINT('Ctrl Pts',(21.8795126484339,-90.5775238241616,10.));
#25662=CARTESIAN_POINT('Ctrl Pts',(21.9256431731989,-90.5218501496029,10.));
#25663=CARTESIAN_POINT('Ctrl Pts',(21.9742690921716,-90.4682921528684,10.));
#25664=CARTESIAN_POINT('Ctrl Pts',(22.0253879613002,-90.4170872144436,10.));
#25665=CARTESIAN_POINT('Ctrl Pts',(22.0442197521512,-90.3982237163382,10.));
#25666=CARTESIAN_POINT('Ctrl Pts',(22.0633900127449,-90.3796798067826,10.));
#25667=CARTESIAN_POINT('Ctrl Pts',(22.0828885913556,-90.3614597865289,10.));
#25668=CARTESIAN_POINT('Origin',(24.,-92.,5.));
#25669=CARTESIAN_POINT('Origin',(24.,92.,1.));
#25670=CARTESIAN_POINT('Ctrl Pts',(22.086534003335,93.635987203375,0.999999999999996));
#25671=CARTESIAN_POINT('Ctrl Pts',(22.0243936537292,93.5775905334555,0.999999999999996));
#25672=CARTESIAN_POINT('Ctrl Pts',(21.9656286004882,93.5159401741294,1.));
#25673=CARTESIAN_POINT('Ctrl Pts',(21.9102508840716,93.4514125531564,1.));
#25674=CARTESIAN_POINT('Ctrl Pts',(21.8535184531584,93.3853063820152,1.));
#25675=CARTESIAN_POINT('Ctrl Pts',(21.8003406478354,93.3161799623012,1.));
#25676=CARTESIAN_POINT('Ctrl Pts',(21.7507593016407,93.2443917538332,1.));
#25677=CARTESIAN_POINT('Ctrl Pts',(21.737815461655,93.2256505304784,1.));
#25678=CARTESIAN_POINT('Ctrl Pts',(21.725116904748,93.2067276794587,1.));
#25679=CARTESIAN_POINT('Ctrl Pts',(21.7126647511951,93.1876291448935,1.));
#25680=CARTESIAN_POINT('Ctrl Pts',(21.7025039315265,93.1720449517797,1.));
#25681=CARTESIAN_POINT('Ctrl Pts',(21.692506743615,93.1563428865691,1.00000000000001));
#25682=CARTESIAN_POINT('Ctrl Pts',(21.6826826224521,93.1405407386175,1.00000000000001));
#25683=CARTESIAN_POINT('Ctrl Pts',(21.6352352783886,93.0642214487416,1.));
#25684=CARTESIAN_POINT('Ctrl Pts',(21.5917715084846,92.9854949382645,1.));
#25685=CARTESIAN_POINT('Ctrl Pts',(21.5523260660392,92.9047536926221,1.));
#25686=CARTESIAN_POINT('Ctrl Pts',(21.5204851858192,92.8395782966339,1.));
#25687=CARTESIAN_POINT('Ctrl Pts',(21.4912631199125,92.7730890245751,1.));
#25688=CARTESIAN_POINT('Ctrl Pts',(21.4646953254222,92.705474488561,1.));
#25689=CARTESIAN_POINT('Ctrl Pts',(21.4539704656061,92.6781799225575,1.));
#25690=CARTESIAN_POINT('Ctrl Pts',(21.4436783241418,92.6507018322004,1.));
#25691=CARTESIAN_POINT('Ctrl Pts',(21.4338220238392,92.6230520580924,1.));
#25692=CARTESIAN_POINT('Ctrl Pts',(21.4286038503028,92.6084135715299,1.));
#25693=CARTESIAN_POINT('Ctrl Pts',(21.423508396409,92.593728292269,1.));
#25694=CARTESIAN_POINT('Ctrl Pts',(21.418539882074,92.5790097941693,1.));
#25695=CARTESIAN_POINT('Ctrl Pts',(21.3890258008439,92.4915786388573,1.));
#25696=CARTESIAN_POINT('Ctrl Pts',(21.3639479991318,92.4028676021535,1.));
#25697=CARTESIAN_POINT('Ctrl Pts',(21.3433392458007,92.3132743760856,1.));
#25698=CARTESIAN_POINT('Ctrl Pts',(21.3224115739842,92.2222947034187,1.));
#25699=CARTESIAN_POINT('Ctrl Pts',(21.3060918366944,92.1304045204495,1.));
#25700=CARTESIAN_POINT('Ctrl Pts',(21.294456192223,92.037987131823,1.));
#25701=CARTESIAN_POINT('Ctrl Pts',(21.2829117114681,91.9462938210629,1.00000000000001));
#25702=CARTESIAN_POINT('Ctrl Pts',(21.2759778687866,91.8540806036969,1.00000000000001));
#25703=CARTESIAN_POINT('Ctrl Pts',(21.2737760007306,91.7617026862606,1.00000000000001));
#25704=CARTESIAN_POINT('Ctrl Pts',(21.2726808057975,91.7157545074694,1.00000000000001));
#25705=CARTESIAN_POINT('Ctrl Pts',(21.2727570661743,91.6697653696922,1.00000000000001));
#25706=CARTESIAN_POINT('Ctrl Pts',(21.2740245030464,91.6237782897535,1.00000000000001));
#25707=CARTESIAN_POINT('Ctrl Pts',(21.274441278932,91.6086561906641,1.00000000000001));
#25708=CARTESIAN_POINT('Ctrl Pts',(21.2749869696768,91.5935324627226,1.00000000000001));
#25709=CARTESIAN_POINT('Ctrl Pts',(21.2756620918863,91.5784144613223,1.00000000000001));
#25710=CARTESIAN_POINT('Ctrl Pts',(21.2799360091138,91.4827086976554,1.00000000000001));
#25711=CARTESIAN_POINT('Ctrl Pts',(21.2893769677446,91.3875701031935,1.));
#25712=CARTESIAN_POINT('Ctrl Pts',(21.304049141918,91.293397004279,1.));
#25713=CARTESIAN_POINT('Ctrl Pts',(21.3082037219408,91.2667309034811,1.));
#25714=CARTESIAN_POINT('Ctrl Pts',(21.312778033191,91.2401420861585,1.));
#25715=CARTESIAN_POINT('Ctrl Pts',(21.3177742468288,91.213639336714,1.));
#25716=CARTESIAN_POINT('Ctrl Pts',(21.3347391581856,91.1236478296194,1.));
#25717=CARTESIAN_POINT('Ctrl Pts',(21.3565643641115,91.0346487842335,1.));
#25718=CARTESIAN_POINT('Ctrl Pts',(21.3829472264989,90.9468744390412,1.));
#25719=CARTESIAN_POINT('Ctrl Pts',(21.4099265677811,90.8571156410763,1.));
#25720=CARTESIAN_POINT('Ctrl Pts',(21.4416721888843,90.7686368464218,1.));
#25721=CARTESIAN_POINT('Ctrl Pts',(21.477914698699,90.6816901122385,1.00000000000001));
#25722=CARTESIAN_POINT('Ctrl Pts',(21.4905815187717,90.6513020777609,1.00000000000001));
#25723=CARTESIAN_POINT('Ctrl Pts',(21.503798101033,90.6211012697161,1.));
#25724=CARTESIAN_POINT('Ctrl Pts',(21.5175543776486,90.5910988047965,1.));
#25725=CARTESIAN_POINT('Ctrl Pts',(21.5245011977626,90.5759477771896,1.));
#25726=CARTESIAN_POINT('Ctrl Pts',(21.531585660728,90.5608473343688,1.));
#25727=CARTESIAN_POINT('Ctrl Pts',(21.5388065373063,90.5457989336951,1.));
#25728=CARTESIAN_POINT('Ctrl Pts',(21.5448162867257,90.5332745377674,1.));
#25729=CARTESIAN_POINT('Ctrl Pts',(21.5509186842686,90.5207901234418,1.));
#25730=CARTESIAN_POINT('Ctrl Pts',(21.5571091309232,90.5083537168634,1.));
#25731=CARTESIAN_POINT('Ctrl Pts',(21.6000723361674,90.4220420307874,1.));
#25732=CARTESIAN_POINT('Ctrl Pts',(21.6473225861462,90.3379370104883,1.00000000000001));
#25733=CARTESIAN_POINT('Ctrl Pts',(21.6985178120761,90.2562887354739,1.));
#25734=CARTESIAN_POINT('Ctrl Pts',(21.7507178509555,90.1730379429873,1.));
#25735=CARTESIAN_POINT('Ctrl Pts',(21.8070195594671,90.09234050566,1.));
#25736=CARTESIAN_POINT('Ctrl Pts',(21.8671152463541,90.0144688409555,1.));
#25737=CARTESIAN_POINT('Ctrl Pts',(21.9276789686894,89.935990698459,1.));
#25738=CARTESIAN_POINT('Ctrl Pts',(21.9920964584949,89.8603816780714,1.));
#25739=CARTESIAN_POINT('Ctrl Pts',(22.0601019288122,89.7879401984298,1.));
#25740=CARTESIAN_POINT('Ctrl Pts',(22.0970286032151,89.7486047902705,1.));
#25741=CARTESIAN_POINT('Ctrl Pts',(22.1350139813229,89.7102037256098,1.));
#25742=CARTESIAN_POINT('Ctrl Pts',(22.1740207512752,89.6727885379724,1.));
#25743=CARTESIAN_POINT('Ctrl Pts',(22.1861506068063,89.6611536135409,1.));
#25744=CARTESIAN_POINT('Ctrl Pts',(22.1983792566453,89.649614047221,0.999999999999999));
#25745=CARTESIAN_POINT('Ctrl Pts',(22.2107056435596,89.6381714533068,0.999999999999999));
#25746=CARTESIAN_POINT('Ctrl Pts',(22.2219939233191,89.6276925350176,0.999999999999999));
#25747=CARTESIAN_POINT('Ctrl Pts',(22.2333584419761,89.6173003020909,1.));
#25748=CARTESIAN_POINT('Ctrl Pts',(22.2447937619035,89.6069996114494,1.));
#25749=CARTESIAN_POINT('Ctrl Pts',(22.3206028372318,89.5387124242319,1.));
#25750=CARTESIAN_POINT('Ctrl Pts',(22.3995782016253,89.4743922577898,1.));
#25751=CARTESIAN_POINT('Ctrl Pts',(22.4813936894611,89.4143217385371,1.));
#25752=CARTESIAN_POINT('Ctrl Pts',(22.5632801173719,89.3541991337043,1.));
#25753=CARTESIAN_POINT('Ctrl Pts',(22.6480121729186,89.2983327116039,1.));
#25754=CARTESIAN_POINT('Ctrl Pts',(22.7353078046389,89.2470320376965,1.));
#25755=CARTESIAN_POINT('Ctrl Pts',(22.8208396627921,89.19676787353,1.00000000000001));
#25756=CARTESIAN_POINT('Ctrl Pts',(22.9088332159369,89.1508861491376,1.));
#25757=CARTESIAN_POINT('Ctrl Pts',(22.9990569156287,89.1097141764903,1.));
#25758=CARTESIAN_POINT('Ctrl Pts',(23.0368467522455,89.0924694600261,1.));
#25759=CARTESIAN_POINT('Ctrl Pts',(23.0750281838879,89.076051483811,1.));
#25760=CARTESIAN_POINT('Ctrl Pts',(23.113585589812,89.0604866736419,1.));
#25761=CARTESIAN_POINT('Ctrl Pts',(23.1435992944682,89.048370775172,1.));
#25762=CARTESIAN_POINT('Ctrl Pts',(23.1738408319514,89.0367718698255,1.));
#25763=CARTESIAN_POINT('Ctrl Pts',(23.2042984301043,89.0256873776386,1.));
#25764=CARTESIAN_POINT('Ctrl Pts',(24.7937992825328,89.0307770462543,0.999999999999999));
#25765=CARTESIAN_POINT('Ctrl Pts',(24.8886355471735,89.0654685754907,0.999999999999998));
#25766=CARTESIAN_POINT('Ctrl Pts',(24.9814285805964,89.1051505313142,0.999999999999997));
#25767=CARTESIAN_POINT('Ctrl Pts',(25.0719374504717,89.1495026644971,0.999999999999998));
#25768=CARTESIAN_POINT('Ctrl Pts',(25.1637178578188,89.1944778901943,0.999999999999999));
#25769=CARTESIAN_POINT('Ctrl Pts',(25.2531501398721,89.2442561371166,0.999999999999999));
#25770=CARTESIAN_POINT('Ctrl Pts',(25.3399490408368,89.2985441486808,1.));
#25771=CARTESIAN_POINT('Ctrl Pts',(25.3644577827616,89.3138730393723,1.));
#25772=CARTESIAN_POINT('Ctrl Pts',(25.3887563292847,89.3295616964546,0.999999999999998));
#25773=CARTESIAN_POINT('Ctrl Pts',(25.4128376626789,89.3456039735087,0.999999999999998));
#25774=CARTESIAN_POINT('Ctrl Pts',(25.4321684184181,89.3584815552504,0.999999999999998));
#25775=CARTESIAN_POINT('Ctrl Pts',(25.4513613133248,89.3715886264076,1.));
#25776=CARTESIAN_POINT('Ctrl Pts',(25.470393428536,89.3849082415597,1.));
#25777=CARTESIAN_POINT('Ctrl Pts',(25.5531010558328,89.4427911281182,1.));
#25778=CARTESIAN_POINT('Ctrl Pts',(25.6328538472513,89.5047358079436,1.));
#25779=CARTESIAN_POINT('Ctrl Pts',(25.7093854476093,89.5704450410727,1.));
#25780=CARTESIAN_POINT('Ctrl Pts',(25.7683982886674,89.621112850351,1.));
#25781=CARTESIAN_POINT('Ctrl Pts',(25.8254952342947,89.6740199049035,1.));
#25782=CARTESIAN_POINT('Ctrl Pts',(25.8805365803869,89.729041709489,1.));
#25783=CARTESIAN_POINT('Ctrl Pts',(25.9098566849157,89.7583514044064,1.));
#25784=CARTESIAN_POINT('Ctrl Pts',(25.9385932131621,89.7882613323854,1.));
#25785=CARTESIAN_POINT('Ctrl Pts',(25.9667230183165,89.8187535094836,1.));
#25786=CARTESIAN_POINT('Ctrl Pts',(25.9763569993312,89.829196562809,1.));
#25787=CARTESIAN_POINT('Ctrl Pts',(25.9859190157893,89.8397071306231,1.));
#25788=CARTESIAN_POINT('Ctrl Pts',(25.9954015809131,89.8502769623014,1.));
#25789=CARTESIAN_POINT('Ctrl Pts',(26.0611940654473,89.9236131828441,1.));
#25790=CARTESIAN_POINT('Ctrl Pts',(26.1232543000056,89.9998957525233,1.));
#25791=CARTESIAN_POINT('Ctrl Pts',(26.1813384938245,90.0788462502489,1.));
#25792=CARTESIAN_POINT('Ctrl Pts',(26.2389162823223,90.1571084204016,1.));
#25793=CARTESIAN_POINT('Ctrl Pts',(26.2925874948895,90.2379929848863,1.));
#25794=CARTESIAN_POINT('Ctrl Pts',(26.3420688573896,90.3212511466106,1.));
#25795=CARTESIAN_POINT('Ctrl Pts',(26.3901172405319,90.402098153486,1.));
#25796=CARTESIAN_POINT('Ctrl Pts',(26.4342151409376,90.4851839694043,1.));
#25797=CARTESIAN_POINT('Ctrl Pts',(26.4740553950964,90.5702911116909,1.));
#25798=CARTESIAN_POINT('Ctrl Pts',(26.4948666592665,90.614748338641,1.));
#25799=CARTESIAN_POINT('Ctrl Pts',(26.5145153290957,90.6597572305164,0.999999999999999));
#25800=CARTESIAN_POINT('Ctrl Pts',(26.5329519176203,90.7052870235978,0.999999999999999));
#25801=CARTESIAN_POINT('Ctrl Pts',(26.5400925813213,90.7229211396022,0.999999999999999));
#25802=CARTESIAN_POINT('Ctrl Pts',(26.547051378829,90.7406333940251,1.));
#25803=CARTESIAN_POINT('Ctrl Pts',(26.5538252663872,90.7584219903797,1.));
#25804=CARTESIAN_POINT('Ctrl Pts',(26.5589791553111,90.7719563824014,1.));
#25805=CARTESIAN_POINT('Ctrl Pts',(26.5640259615885,90.7855350878376,1.));
#25806=CARTESIAN_POINT('Ctrl Pts',(26.5689595142418,90.7991434113625,1.));
#25807=CARTESIAN_POINT('Ctrl Pts',(26.6006313709989,90.8865045694709,1.));
#25808=CARTESIAN_POINT('Ctrl Pts',(26.6276945169744,90.9752266494668,0.999999999999999));
#25809=CARTESIAN_POINT('Ctrl Pts',(26.6498976668617,91.0650862423011,1.));
#25810=CARTESIAN_POINT('Ctrl Pts',(26.6549002607872,91.085332516165,1.));
#25811=CARTESIAN_POINT('Ctrl Pts',(26.659655933915,91.1056365753757,1.));
#25812=CARTESIAN_POINT('Ctrl Pts',(26.6641614464107,91.1259959208575,1.));
#25813=CARTESIAN_POINT('Ctrl Pts',(26.6845069776771,91.2179325652363,1.));
#25814=CARTESIAN_POINT('Ctrl Pts',(26.699755509991,91.3109969010619,1.));
#25815=CARTESIAN_POINT('Ctrl Pts',(26.7100169526549,91.4047971880179,1.));
#25816=CARTESIAN_POINT('Ctrl Pts',(26.7207301009459,91.50272653546,0.999999999999999));
#25817=CARTESIAN_POINT('Ctrl Pts',(26.7260074241422,91.6014592922206,0.999999999999999));
#25818=CARTESIAN_POINT('Ctrl Pts',(26.7259165033721,91.7005349801406,0.999999999999998));
#25819=CARTESIAN_POINT('Ctrl Pts',(26.7258813891798,91.7387986546182,0.999999999999998));
#25820=CARTESIAN_POINT('Ctrl Pts',(26.7250449852701,91.7771132264438,0.999999999999998));
#25821=CARTESIAN_POINT('Ctrl Pts',(26.7234090502603,91.8154509913201,0.999999999999998));
#25822=CARTESIAN_POINT('Ctrl Pts',(26.7228214486219,91.8292213020722,0.999999999999998));
#25823=CARTESIAN_POINT('Ctrl Pts',(26.7221307047635,91.8429928069669,1.));
#25824=CARTESIAN_POINT('Ctrl Pts',(26.7213377901891,91.8567525537414,1.));
#25825=CARTESIAN_POINT('Ctrl Pts',(26.7159861969284,91.9496207774894,1.));
#25826=CARTESIAN_POINT('Ctrl Pts',(26.7059788948232,92.0421019016628,0.999999999999995));
#25827=CARTESIAN_POINT('Ctrl Pts',(26.6914389406466,92.1338240299277,0.999999999999995));
#25828=CARTESIAN_POINT('Ctrl Pts',(26.6769360335326,92.2253124548821,0.999999999999995));
#25829=CARTESIAN_POINT('Ctrl Pts',(26.6579231314149,92.316046691047,1.));
#25830=CARTESIAN_POINT('Ctrl Pts',(26.6344737636544,92.4056405659079,1.));
#25831=CARTESIAN_POINT('Ctrl Pts',(26.6114256904433,92.4937011997024,1.));
#25832=CARTESIAN_POINT('Ctrl Pts',(26.584091228894,92.5806609520556,0.999999999999998));
#25833=CARTESIAN_POINT('Ctrl Pts',(26.552499862565,92.6661239169473,0.999999999999998));
#25834=CARTESIAN_POINT('Ctrl Pts',(26.5366373926815,92.709036075055,0.999999999999998));
#25835=CARTESIAN_POINT('Ctrl Pts',(26.5197010822847,92.7515703297502,0.999999999999998));
#25836=CARTESIAN_POINT('Ctrl Pts',(26.5016912750301,92.7936727826891,0.999999999999998));
#25837=CARTESIAN_POINT('Ctrl Pts',(26.4963919590575,92.806061266263,0.999999999999998));
#25838=CARTESIAN_POINT('Ctrl Pts',(26.4909996848537,92.8184123452205,0.999999999999999));
#25839=CARTESIAN_POINT('Ctrl Pts',(26.485514426691,92.8307245976522,0.999999999999999));
#25840=CARTESIAN_POINT('Ctrl Pts',(26.4799210122187,92.8432796185637,0.999999999999999));
#25841=CARTESIAN_POINT('Ctrl Pts',(26.474234590912,92.8557859781359,0.999999999999996));
#25842=CARTESIAN_POINT('Ctrl Pts',(26.4684564517529,92.8682403414366,0.999999999999996));
#25843=CARTESIAN_POINT('Ctrl Pts',(26.4309710839664,92.9490373551493,0.999999999999997));
#25844=CARTESIAN_POINT('Ctrl Pts',(26.3896160116609,93.0276775110388,0.999999999999999));
#25845=CARTESIAN_POINT('Ctrl Pts',(26.3444610577778,93.1038131058523,0.999999999999999));
#25846=CARTESIAN_POINT('Ctrl Pts',(26.3000642810644,93.1786703410435,0.999999999999999));
#25847=CARTESIAN_POINT('Ctrl Pts',(26.2519937014066,93.2511070845464,0.999999999999997));
#25848=CARTESIAN_POINT('Ctrl Pts',(26.200279482717,93.3207586728076,0.999999999999998));
#25849=CARTESIAN_POINT('Ctrl Pts',(26.1501451977981,93.388282318324,0.999999999999998));
#25850=CARTESIAN_POINT('Ctrl Pts',(26.0965860652472,93.4531888297271,1.));
#25851=CARTESIAN_POINT('Ctrl Pts',(26.0396018761895,93.5151056722102,1.));
#25852=CARTESIAN_POINT('Ctrl Pts',(26.0184128642862,93.5381288429192,1.));
#25853=CARTESIAN_POINT('Ctrl Pts',(25.9967500378082,93.5607382046918,0.999999999999995));
#25854=CARTESIAN_POINT('Ctrl Pts',(25.9746125472697,93.5829129376406,0.999999999999995));
#25855=CARTESIAN_POINT('Ctrl Pts',(25.9557857592069,93.6017713984426,0.999999999999995));
#25856=CARTESIAN_POINT('Ctrl Pts',(25.9366156438111,93.6203154841753,0.999999999999998));
#25857=CARTESIAN_POINT('Ctrl Pts',(25.9171119325404,93.6385402784441,0.999999999999998));
#25858=CARTESIAN_POINT('Origin',(24.,92.,12.2084234471775));
#25859=CARTESIAN_POINT('Ctrl Pts',(20.9232326966468,92.0019373937314,9.70842344717745));
#25860=CARTESIAN_POINT('Ctrl Pts',(20.9222985312732,92.1261020010043,9.70197366100993));
#25861=CARTESIAN_POINT('Ctrl Pts',(20.9853329189178,93.2631142772851,9.64286281975953));
#25862=CARTESIAN_POINT('Ctrl Pts',(22.4009679157595,95.2555128800838,9.53109092342627));
#25863=CARTESIAN_POINT('Ctrl Pts',(25.8523952892237,95.1179538105413,9.37310775817762));
#25864=CARTESIAN_POINT('Ctrl Pts',(27.6235723677573,92.1527148994824,9.215124592929));
#25865=CARTESIAN_POINT('Ctrl Pts',(26.1080772256066,89.0487573061685,9.05714142768035));
#25866=CARTESIAN_POINT('Ctrl Pts',(22.6804686178369,88.6217759976465,8.89915826243173));
#25867=CARTESIAN_POINT('Ctrl Pts',(21.0391555349925,90.5621016925695,8.78291893559742));
#25868=CARTESIAN_POINT('Ctrl Pts',(20.9237201879855,91.786686207045,8.719340663846));
#25869=CARTESIAN_POINT('Ctrl Pts',(20.925632029797,91.9973209161002,8.70842344717745));
#25870=CARTESIAN_POINT('Ctrl Pts',(20.929711085108,91.9968960951898,9.79157655282254));
#25871=CARTESIAN_POINT('Ctrl Pts',(20.9347146766409,92.6903800819212,9.75572892504927));
#25872=CARTESIAN_POINT('Ctrl Pts',(21.5077563627457,94.4123579721078,9.66722024219313));
#25873=CARTESIAN_POINT('Ctrl Pts',(24.3539160756188,95.60883918843,9.5260505042541));
#25874=CARTESIAN_POINT('Ctrl Pts',(27.2156041936735,93.6770751085582,9.36806733900546));
#25875=CARTESIAN_POINT('Ctrl Pts',(27.1618224985939,90.2228835192267,9.21008417375683));
#25876=CARTESIAN_POINT('Ctrl Pts',(24.2395757642923,88.3812156575976,9.05210100850819));
#25877=CARTESIAN_POINT('Ctrl Pts',(21.4675379096604,89.6531112748897,8.91259846819677));
#25878=CARTESIAN_POINT('Ctrl Pts',(20.9339205520176,91.3404824212939,8.82575698296822));
#25879=CARTESIAN_POINT('Ctrl Pts',(20.9296144608475,92.0021357572271,8.79157655282255));
#25880=CARTESIAN_POINT('Ctrl Pts',(25.9134659966651,93.6359872033749,10.));
#25881=CARTESIAN_POINT('Ctrl Pts',(26.4547800806522,93.0028611672492,9.94733894491712));
#25882=CARTESIAN_POINT('Ctrl Pts',(26.850124624194,91.1673972202025,9.84201683475137));
#25883=CARTESIAN_POINT('Ctrl Pts',(24.8579881232767,89.1541937717729,9.68403366950273));
#25884=CARTESIAN_POINT('Ctrl Pts',(22.0866994468078,89.7281636060897,9.5260505042541));
#25885=CARTESIAN_POINT('Ctrl Pts',(21.0512846745644,92.3598888261915,9.36806733900546));
#25886=CARTESIAN_POINT('Ctrl Pts',(22.6902348228159,94.6665865220793,9.21008417375683));
#25887=CARTESIAN_POINT('Ctrl Pts',(25.5172946610121,94.5539120605297,9.0521010085082));
#25888=CARTESIAN_POINT('Ctrl Pts',(26.9680635873854,92.1250885828686,8.89411784325955));
#25889=CARTESIAN_POINT('Ctrl Pts',(25.726723414825,89.5826408063379,8.73613467801094));
#25890=CARTESIAN_POINT('Ctrl Pts',(22.9191734977727,89.2329009513827,8.57815151276228));
#25891=CARTESIAN_POINT('Ctrl Pts',(21.0919763121477,91.3929749104687,8.42016834751366));
#25892=CARTESIAN_POINT('Ctrl Pts',(21.9024528317436,94.1036606678714,8.26218518226502));
#25893=CARTESIAN_POINT('Ctrl Pts',(24.6154777134031,94.9062449372411,8.10420201701639));
#25894=CARTESIAN_POINT('Ctrl Pts',(26.7702425736135,93.0727704833333,7.94621885176775));
#25895=CARTESIAN_POINT('Ctrl Pts',(26.4123032215513,90.2662543178418,7.78823568651912));
#25896=CARTESIAN_POINT('Ctrl Pts',(23.866322336025,89.0323057724808,7.63025252127049));
#25897=CARTESIAN_POINT('Ctrl Pts',(21.441591739827,90.4901566418531,7.47226935602184));
#25898=CARTESIAN_POINT('Ctrl Pts',(21.3374247177567,93.3174872372793,7.31428619077322));
#25899=CARTESIAN_POINT('Ctrl Pts',(23.6483043765504,94.9498118095941,7.15630302552458));
#25900=CARTESIAN_POINT('Ctrl Pts',(26.2781839599184,93.9065564509649,6.99831986027594));
#25901=CARTESIAN_POINT('Ctrl Pts',(26.8416729372437,91.1339892852382,6.84033669502732));
#25902=CARTESIAN_POINT('Ctrl Pts',(24.8276675656985,89.1469234118836,6.68235352977867));
#25903=CARTESIAN_POINT('Ctrl Pts',(22.0629394631722,89.7476953780895,6.52437036453004));
#25904=CARTESIAN_POINT('Ctrl Pts',(21.0551913830017,92.3913845160155,6.36638719928141));
#25905=CARTESIAN_POINT('Ctrl Pts',(22.7184852313611,94.68007453733,6.20840403403277));
#25906=CARTESIAN_POINT('Ctrl Pts',(25.5441567155844,94.5378454774748,6.05042086878414));
#25907=CARTESIAN_POINT('Ctrl Pts',(26.9692253534609,92.0937039470137,5.8924377035355));
#25908=CARTESIAN_POINT('Ctrl Pts',(25.7011052496899,89.5645697385057,5.73445453828687));
#25909=CARTESIAN_POINT('Ctrl Pts',(22.8900246220956,89.2444539035236,5.57647137303823));
#25910=CARTESIAN_POINT('Ctrl Pts',(21.0857295480958,91.4237124307955,5.4184882077896));
#25911=CARTESIAN_POINT('Ctrl Pts',(21.9247772442663,94.1256834532324,5.26050504254097));
#25912=CARTESIAN_POINT('Ctrl Pts',(24.6461228117037,94.8995870294848,5.10252187729233));
#25913=CARTESIAN_POINT('Ctrl Pts',(26.7814129353351,93.0434662008304,4.9445387120437));
#25914=CARTESIAN_POINT('Ctrl Pts',(26.3938665911029,90.2408859123632,4.78655554679506));
#25915=CARTESIAN_POINT('Ctrl Pts',(23.8350015407958,89.0338821435612,4.62857238154643));
#25916=CARTESIAN_POINT('Ctrl Pts',(21.425795725037,90.5172485108267,4.4705892162978));
#25917=CARTESIAN_POINT('Ctrl Pts',(21.3514810491689,93.3455210876134,4.31260605104916));
#25918=CARTESIAN_POINT('Ctrl Pts',(23.6794634625817,94.953360113734,4.15462288580053));
#25919=CARTESIAN_POINT('Ctrl Pts',(26.2981834534832,93.8824007094939,3.99663972055189));
#25920=CARTESIAN_POINT('Ctrl Pts',(26.8323726153541,91.1040396168705,3.83865655530326));
#25921=CARTESIAN_POINT('Ctrl Pts',(24.7975031295149,89.1383451615613,3.68067339005462));
#25922=CARTESIAN_POINT('Ctrl Pts',(22.0392711064376,89.7682693420747,3.52269022480599));
#25923=CARTESIAN_POINT('Ctrl Pts',(21.0594870693288,92.42244935621,3.36470705955735));
#25924=CARTESIAN_POINT('Ctrl Pts',(22.7468487169864,94.6934534808946,3.20672389430872));
#25925=CARTESIAN_POINT('Ctrl Pts',(25.5708611659362,94.5214031695169,3.04874072906008));
#25926=CARTESIAN_POINT('Ctrl Pts',(26.9700492986992,92.0623545219302,2.89075756381145));
#25927=CARTESIAN_POINT('Ctrl Pts',(25.6753005709136,89.5467473787502,2.73277439856282));
#25928=CARTESIAN_POINT('Ctrl Pts',(22.8609986216085,89.2563257644252,2.57479123331418));
#25929=CARTESIAN_POINT('Ctrl Pts',(21.0798065759794,91.45450692496,2.41680806806555));
#25930=CARTESIAN_POINT('Ctrl Pts',(21.9473362220071,94.1474758771513,2.25882490281691));
#25931=CARTESIAN_POINT('Ctrl Pts',(24.6766885285288,94.8925967067901,2.10084173756828));
#25932=CARTESIAN_POINT('Ctrl Pts',(26.792288712224,93.0140626065851,1.94285857231964));
#25933=CARTESIAN_POINT('Ctrl Pts',(26.3751316170022,90.2156798453631,1.78487540707101));
#25934=CARTESIAN_POINT('Ctrl Pts',(23.8037636898017,89.0358574238383,1.62689224182237));
#25935=CARTESIAN_POINT('Ctrl Pts',(21.410154680019,90.5443662144373,1.46890907657374));
#25936=CARTESIAN_POINT('Ctrl Pts',(21.3661019891308,93.3736896687444,1.3109259113251));
#25937=CARTESIAN_POINT('Ctrl Pts',(23.7101077177223,94.9559976441495,1.15294274607647));
#25938=CARTESIAN_POINT('Ctrl Pts',(26.3190524504206,93.8592343694375,0.994959580827835));
#25939=CARTESIAN_POINT('Ctrl Pts',(26.8204140260175,91.0717206863196,0.836976415579202));
#25940=CARTESIAN_POINT('Ctrl Pts',(25.4549268544596,89.7830508320407,0.731654305413445));
#25941=CARTESIAN_POINT('Ctrl Pts',(24.6501999979751,89.5679131979649,0.678993250330566));
#25942=CARTESIAN_POINT('Ctrl Pts',(26.0543315503421,93.7564253212268,10.1070022498898));
#25943=CARTESIAN_POINT('Ctrl Pts',(26.6354960985062,93.0766898079629,10.0543411948069));
#25944=CARTESIAN_POINT('Ctrl Pts',(27.0599451195336,91.1061026626961,9.94901908464117));
#25945=CARTESIAN_POINT('Ctrl Pts',(24.9211514991843,88.944691188139,9.79103591939255));
#25946=CARTESIAN_POINT('Ctrl Pts',(21.9458460727495,89.5609155378986,9.63305275414391));
#25947=CARTESIAN_POINT('Ctrl Pts',(20.8342061282629,92.3863831244189,9.47506958889527));
#25948=CARTESIAN_POINT('Ctrl Pts',(22.5938125204638,94.8628953080809,9.31708642364664));
#25949=CARTESIAN_POINT('Ctrl Pts',(25.6289948704159,94.7419259772003,9.159103258398));
#25950=CARTESIAN_POINT('Ctrl Pts',(27.186566514176,92.1342973550732,9.00112009314937));
#25951=CARTESIAN_POINT('Ctrl Pts',(25.8538413517522,89.4046796396148,8.84313692790074));
#25952=CARTESIAN_POINT('Ctrl Pts',(22.8396052044608,89.0291926334707,8.6851537626521));
#25953=CARTESIAN_POINT('Ctrl Pts',(20.8778934031181,91.348286933007,8.52717059740347));
#25954=CARTESIAN_POINT('Ctrl Pts',(21.7480355890358,94.2585279742383,8.36918743215483));
#25955=CARTESIAN_POINT('Ctrl Pts',(24.6607879561905,95.1201968981952,8.2112042669062));
#25956=CARTESIAN_POINT('Ctrl Pts',(26.9741823115717,93.1517457085875,8.05322110165757));
#25957=CARTESIAN_POINT('Ctrl Pts',(26.5898921776827,90.1386194155869,7.89523793640892));
#25958=CARTESIAN_POINT('Ctrl Pts',(23.856481252785,88.8138300372275,7.7372547711603));
#25959=CARTESIAN_POINT('Ctrl Pts',(21.2532468218983,90.3790049825179,7.57927160591166));
#25960=CARTESIAN_POINT('Ctrl Pts',(21.1414112312387,93.4144780223077,7.42128844066303));
#25961=CARTESIAN_POINT('Ctrl Pts',(23.6224132455821,95.1669710768744,7.26330527541439));
#25962=CARTESIAN_POINT('Ctrl Pts',(26.4458993232703,94.0469133376563,7.10532211016575));
#25963=CARTESIAN_POINT('Ctrl Pts',(27.0508712362317,91.0702353021323,6.94733894491713));
#25964=CARTESIAN_POINT('Ctrl Pts',(24.8885988025775,88.9368855988426,6.78935577966848));
#25965=CARTESIAN_POINT('Ctrl Pts',(21.9203369264656,89.5818852000315,6.63137261441985));
#25966=CARTESIAN_POINT('Ctrl Pts',(20.8384004407904,92.4201974641658,6.47338944917122));
#25967=CARTESIAN_POINT('Ctrl Pts',(22.624142667791,94.8773762841363,6.31540628392259));
#25968=CARTESIAN_POINT('Ctrl Pts',(25.6578344559174,94.7246766043172,6.15742311867394));
#25969=CARTESIAN_POINT('Ctrl Pts',(27.187813807155,92.1006022448672,5.99943995342532));
#25970=CARTESIAN_POINT('Ctrl Pts',(25.8263372283496,89.3852782157793,5.84145678817669));
#25971=CARTESIAN_POINT('Ctrl Pts',(22.8083104466418,89.0415960909264,5.68347362292804));
#25972=CARTESIAN_POINT('Ctrl Pts',(20.8711867647448,91.381287288329,5.52549045767941));
#25973=CARTESIAN_POINT('Ctrl Pts',(21.7720034803222,94.2821720331726,5.36750729243078));
#25974=CARTESIAN_POINT('Ctrl Pts',(24.693689085561,95.1130488485371,5.20952412718214));
#25975=CARTESIAN_POINT('Ctrl Pts',(26.9861750130638,93.1202841032021,5.05154096193351));
#25976=CARTESIAN_POINT('Ctrl Pts',(26.5700982792397,90.111383438649,4.89355779668487));
#25977=CARTESIAN_POINT('Ctrl Pts',(23.8228546830245,88.8155224576056,4.73557463143624));
#25978=CARTESIAN_POINT('Ctrl Pts',(21.2362879359765,90.4080913008988,4.57759146618761));
#25979=CARTESIAN_POINT('Ctrl Pts',(21.1565023617591,93.44457566884,4.41960830093897));
#25980=CARTESIAN_POINT('Ctrl Pts',(23.6558662014358,95.1707806000944,4.26162513569034));
#25981=CARTESIAN_POINT('Ctrl Pts',(26.4673711396979,94.0209792986338,4.1036419704417));
#25982=CARTESIAN_POINT('Ctrl Pts',(27.0408862431775,91.0380807988605,3.94565880519307));
#25983=CARTESIAN_POINT('Ctrl Pts',(24.8562137207113,88.9276758348256,3.78767563994443));
#25984=CARTESIAN_POINT('Ctrl Pts',(21.8949261524726,89.6039737782472,3.6296924746958));
#25985=CARTESIAN_POINT('Ctrl Pts',(20.8430123669848,92.453549235992,3.47170930944716));
#25986=CARTESIAN_POINT('Ctrl Pts',(22.6545942167076,94.8917401588658,3.31372614419853));
#25987=CARTESIAN_POINT('Ctrl Pts',(25.6865048346897,94.7070238464122,3.15574297894989));
#25988=CARTESIAN_POINT('Ctrl Pts',(27.1886984095998,92.0669449375797,2.99775981370126));
#25989=CARTESIAN_POINT('Ctrl Pts',(25.7986328605433,89.3661438094137,2.83977664845263));
#25990=CARTESIAN_POINT('Ctrl Pts',(22.7771476098395,89.0543419345702,2.68179348320399));
#25991=CARTESIAN_POINT('Ctrl Pts',(20.864827755224,91.4143488117893,2.52381031795536));
#25992=CARTESIAN_POINT('Ctrl Pts',(21.7962232050505,94.305568771914,2.36582715270672));
#25993=CARTESIAN_POINT('Ctrl Pts',(24.7265049895499,95.1055439122155,2.20784398745809));
#25994=CARTESIAN_POINT('Ctrl Pts',(26.9978514429749,93.0887158749414,2.04986082220945));
#25995=CARTESIAN_POINT('Ctrl Pts',(26.5499840736792,90.0843217512249,1.89187765696082));
#25996=CARTESIAN_POINT('Ctrl Pts',(23.7893171636885,88.8176431540805,1.73389449171218));
#25997=CARTESIAN_POINT('Ctrl Pts',(21.2194954283924,90.4372053558113,1.57591132646355));
#25998=CARTESIAN_POINT('Ctrl Pts',(21.1721996661856,93.4748179647817,1.41792816121491));
#25999=CARTESIAN_POINT('Ctrl Pts',(23.6887664255745,95.1736123002431,1.25994499596628));
#26000=CARTESIAN_POINT('Ctrl Pts',(26.4897764706038,93.9961074987864,1.10196183071765));
#26001=CARTESIAN_POINT('Ctrl Pts',(27.0280472863242,91.0033826130449,0.943978665469013));
#26002=CARTESIAN_POINT('Ctrl Pts',(25.5620356702265,89.6198434520492,0.838656555303256));
#26003=CARTESIAN_POINT('Ctrl Pts',(24.698066426161,89.3888678140614,0.785995500220377));
#26004=CARTESIAN_POINT('Ctrl Pts',(26.1951971040191,93.8768634390787,10.2140044997796));
#26005=CARTESIAN_POINT('Ctrl Pts',(26.8162121163603,93.1505184486766,10.1613434446967));
#26006=CARTESIAN_POINT('Ctrl Pts',(27.2697656148731,91.0448081051896,10.056021334531));
#26007=CARTESIAN_POINT('Ctrl Pts',(24.9843148750919,88.7351886045053,9.89803816928235));
#26008=CARTESIAN_POINT('Ctrl Pts',(21.8049926986913,89.3936674697073,9.74005500403372));
#26009=CARTESIAN_POINT('Ctrl Pts',(20.6171275819614,92.4128774226463,9.58207183878508));
#26010=CARTESIAN_POINT('Ctrl Pts',(22.4973902181116,95.0592040940823,9.42408867353646));
#26011=CARTESIAN_POINT('Ctrl Pts',(25.7406950798198,94.9299398938708,9.26610550828781));
#26012=CARTESIAN_POINT('Ctrl Pts',(27.4050694409667,92.1435061272778,9.10812234303919));
#26013=CARTESIAN_POINT('Ctrl Pts',(25.9809592886793,89.2267184728917,8.95013917779054));
#26014=CARTESIAN_POINT('Ctrl Pts',(22.7600369111489,88.8254843155586,8.79215601254192));
#26015=CARTESIAN_POINT('Ctrl Pts',(20.6638104940885,91.3035989555452,8.63417284729328));
#26016=CARTESIAN_POINT('Ctrl Pts',(21.593618346328,94.4133952806054,8.47618968204464));
#26017=CARTESIAN_POINT('Ctrl Pts',(24.706098198978,95.3341488591492,8.31820651679601));
#26018=CARTESIAN_POINT('Ctrl Pts',(27.1781220495298,93.2307209338419,8.16022335154737));
#26019=CARTESIAN_POINT('Ctrl Pts',(26.7674811338141,90.0109845133321,8.00224018629874));
#26020=CARTESIAN_POINT('Ctrl Pts',(23.846640169545,88.5953543019741,7.84425702105011));
#26021=CARTESIAN_POINT('Ctrl Pts',(21.0649019039697,90.2678533231826,7.68627385580147));
#26022=CARTESIAN_POINT('Ctrl Pts',(20.9453977447207,93.5114688073361,7.52829069055284));
#26023=CARTESIAN_POINT('Ctrl Pts',(23.5965221146138,95.3841303441547,7.3703075253042));
#26024=CARTESIAN_POINT('Ctrl Pts',(26.6136146866221,94.1872702243476,7.21232436005557));
#26025=CARTESIAN_POINT('Ctrl Pts',(27.2600695352198,91.0064813190264,7.05434119480693));
#26026=CARTESIAN_POINT('Ctrl Pts',(24.9495300394564,88.7268477858015,6.8963580295583));
#26027=CARTESIAN_POINT('Ctrl Pts',(21.7777343897591,89.4160750219737,6.73837486430966));
#26028=CARTESIAN_POINT('Ctrl Pts',(20.6216094985791,92.449010412316,6.58039169906103));
#26029=CARTESIAN_POINT('Ctrl Pts',(22.5298001042209,95.0746780309427,6.42240853381239));
#26030=CARTESIAN_POINT('Ctrl Pts',(25.7715121962504,94.9115077311594,6.26442536856376));
#26031=CARTESIAN_POINT('Ctrl Pts',(27.406402260849,92.1075005427209,6.10644220331512));
#26032=CARTESIAN_POINT('Ctrl Pts',(25.9515692070094,89.205986693053,5.94845903806649));
#26033=CARTESIAN_POINT('Ctrl Pts',(22.7265962711881,88.8387382783291,5.79047587281786));
#26034=CARTESIAN_POINT('Ctrl Pts',(20.6566439813937,91.3388621458626,5.63249270756922));
#26035=CARTESIAN_POINT('Ctrl Pts',(21.6192297163781,94.4386606131126,5.47450954232059));
#26036=CARTESIAN_POINT('Ctrl Pts',(24.7412553594183,95.3265106675896,5.31652637707196));
#26037=CARTESIAN_POINT('Ctrl Pts',(27.1909370907926,93.1971020055737,5.15854321182332));
#26038=CARTESIAN_POINT('Ctrl Pts',(26.7463299673765,89.9818809649348,5.00056004657469));
#26039=CARTESIAN_POINT('Ctrl Pts',(23.8107078252533,88.5971627716501,4.84257688132604));
#26040=CARTESIAN_POINT('Ctrl Pts',(21.046780146916,90.2989340909708,4.68459371607742));
#26041=CARTESIAN_POINT('Ctrl Pts',(20.9615236743494,93.5436302500665,4.52661055082878));
#26042=CARTESIAN_POINT('Ctrl Pts',(23.6322689402899,95.3882010864546,4.36862738558015));
#26043=CARTESIAN_POINT('Ctrl Pts',(26.6365588259126,94.1595578877736,4.21064422033151));
#26044=CARTESIAN_POINT('Ctrl Pts',(27.249399871001,90.9721219808506,4.05266105508288));
#26045=CARTESIAN_POINT('Ctrl Pts',(24.9149243119076,88.7170065080898,3.89467788983424));
#26046=CARTESIAN_POINT('Ctrl Pts',(21.7505811985076,89.4396782144198,3.73669472458561));
#26047=CARTESIAN_POINT('Ctrl Pts',(20.6265376646408,92.4846491157738,3.57871155933697));
#26048=CARTESIAN_POINT('Ctrl Pts',(22.5623397164288,95.0900268368369,3.42072839408834));
#26049=CARTESIAN_POINT('Ctrl Pts',(25.8021485034432,94.8926445233076,3.2627452288397));
#26050=CARTESIAN_POINT('Ctrl Pts',(27.4073475205004,92.0715353532292,3.10476206359107));
#26051=CARTESIAN_POINT('Ctrl Pts',(25.921965150173,89.1855402400772,2.94677889834244));
#26052=CARTESIAN_POINT('Ctrl Pts',(22.6932965980704,88.8523581047152,2.7887957330938));
#26053=CARTESIAN_POINT('Ctrl Pts',(20.6498489344685,91.3741906986186,2.63081256784517));
#26054=CARTESIAN_POINT('Ctrl Pts',(21.645110188094,94.4636616666768,2.47282940259653));
#26055=CARTESIAN_POINT('Ctrl Pts',(24.7763214505711,95.318491117641,2.3148462373479));
#26056=CARTESIAN_POINT('Ctrl Pts',(27.2034141737259,93.1633691432978,2.15686307209926));
#26057=CARTESIAN_POINT('Ctrl Pts',(26.7248365303562,89.9529636570868,1.99887990685063));
#26058=CARTESIAN_POINT('Ctrl Pts',(23.7748706375752,88.5994288843227,1.84089674160199));
#26059=CARTESIAN_POINT('Ctrl Pts',(21.0288361767659,90.3300444971853,1.68291357635336));
#26060=CARTESIAN_POINT('Ctrl Pts',(20.9782973432405,93.5759462608191,1.52493041110473));
#26061=CARTESIAN_POINT('Ctrl Pts',(23.6674251334267,95.3912269563368,1.36694724585609));
#26062=CARTESIAN_POINT('Ctrl Pts',(26.6605004907871,94.1329806281353,1.20896408060746));
#26063=CARTESIAN_POINT('Ctrl Pts',(27.2356805466308,90.9350445397703,1.05098091535882));
#26064=CARTESIAN_POINT('Ctrl Pts',(25.6691444859934,89.4566360720578,0.945658805193066));
#26065=CARTESIAN_POINT('Ctrl Pts',(24.7459328543469,89.2098224301578,0.892997750110188));
#26066=CARTESIAN_POINT('Ctrl Pts',(26.3360626576962,93.9973015569306,10.3210067496694));
#26067=CARTESIAN_POINT('Ctrl Pts',(26.9969281342143,93.2243470893904,10.2683456945866));
#26068=CARTESIAN_POINT('Ctrl Pts',(27.4795861102127,90.9835135476831,10.1630235844208));
#26069=CARTESIAN_POINT('Ctrl Pts',(25.0474782509994,88.5256860208715,10.0050404191722));
#26070=CARTESIAN_POINT('Ctrl Pts',(21.664139324633,89.2264194015161,9.84705725392353));
#26071=CARTESIAN_POINT('Ctrl Pts',(20.4000490356599,92.4393717208737,9.68907408867489));
#26072=CARTESIAN_POINT('Ctrl Pts',(22.4009679157595,95.2555128800838,9.53109092342627));
#26073=CARTESIAN_POINT('Ctrl Pts',(25.8523952892237,95.1179538105413,9.37310775817762));
#26074=CARTESIAN_POINT('Ctrl Pts',(27.6235723677573,92.1527148994824,9.215124592929));
#26075=CARTESIAN_POINT('Ctrl Pts',(26.1080772256066,89.0487573061685,9.05714142768035));
#26076=CARTESIAN_POINT('Ctrl Pts',(22.6804686178369,88.6217759976465,8.89915826243173));
#26077=CARTESIAN_POINT('Ctrl Pts',(20.4497275850589,91.2589109780836,8.74117509718308));
#26078=CARTESIAN_POINT('Ctrl Pts',(21.4392011036202,94.5682625869723,8.58319193193445));
#26079=CARTESIAN_POINT('Ctrl Pts',(24.7514084417654,95.5481008201034,8.42520876668582));
#26080=CARTESIAN_POINT('Ctrl Pts',(27.382061787488,93.3096961590962,8.26722560143718));
#26081=CARTESIAN_POINT('Ctrl Pts',(26.9450700899455,89.8833496110771,8.10924243618856));
#26082=CARTESIAN_POINT('Ctrl Pts',(23.8367990863051,88.3768785667208,7.95125927093992));
#26083=CARTESIAN_POINT('Ctrl Pts',(20.876556986041,90.1567016638474,7.79327610569128));
#26084=CARTESIAN_POINT('Ctrl Pts',(20.7493842582027,93.6084595923645,7.63529294044265));
#26085=CARTESIAN_POINT('Ctrl Pts',(23.5706309836456,95.601289611435,7.47730977519401));
#26086=CARTESIAN_POINT('Ctrl Pts',(26.7813300499739,94.327627111039,7.31932660994538));
#26087=CARTESIAN_POINT('Ctrl Pts',(27.4692678342079,90.9427273359204,7.16134344469674));
#26088=CARTESIAN_POINT('Ctrl Pts',(25.0104612763354,88.5168099727604,7.00336027944811));
#26089=CARTESIAN_POINT('Ctrl Pts',(21.6351318530525,89.2502648439158,6.84537711419948));
#26090=CARTESIAN_POINT('Ctrl Pts',(20.4048185563677,92.4778233604662,6.68739394895084));
#26091=CARTESIAN_POINT('Ctrl Pts',(22.4354575406508,95.2719797777492,6.5294107837022));
#26092=CARTESIAN_POINT('Ctrl Pts',(25.8851899365834,95.0983388580017,6.37142761845357));
#26093=CARTESIAN_POINT('Ctrl Pts',(27.624990714543,92.1143988405745,6.21344445320494));
#26094=CARTESIAN_POINT('Ctrl Pts',(26.0768011856691,89.0266951703267,6.0554612879563));
#26095=CARTESIAN_POINT('Ctrl Pts',(22.6448820957342,88.6358804657318,5.89747812270767));
#26096=CARTESIAN_POINT('Ctrl Pts',(20.4421011980427,91.2964370033963,5.73949495745903));
#26097=CARTESIAN_POINT('Ctrl Pts',(21.4664559524339,94.5951491930526,5.5815117922104));
#26098=CARTESIAN_POINT('Ctrl Pts',(24.7888216332756,95.5399724866421,5.42352862696176));
#26099=CARTESIAN_POINT('Ctrl Pts',(27.3956991685213,93.2739199079453,5.26554546171313));
#26100=CARTESIAN_POINT('Ctrl Pts',(26.9225616555133,89.8523784912207,5.1075622964645));
#26101=CARTESIAN_POINT('Ctrl Pts',(23.798560967482,88.3788030856943,4.94957913121586));
#26102=CARTESIAN_POINT('Ctrl Pts',(20.8572723578555,90.189776881043,4.79159596596723));
#26103=CARTESIAN_POINT('Ctrl Pts',(20.7665449869397,93.642684831293,4.63361280071859));
#26104=CARTESIAN_POINT('Ctrl Pts',(23.608671679144,95.6056215728149,4.47562963546996));
#26105=CARTESIAN_POINT('Ctrl Pts',(26.8057465121274,94.2981364769134,4.31764647022132));
#26106=CARTESIAN_POINT('Ctrl Pts',(27.4579134988245,90.9061631628407,4.15966330497269));
#26107=CARTESIAN_POINT('Ctrl Pts',(24.973634903104,88.5063371813541,4.00168013972405));
#26108=CARTESIAN_POINT('Ctrl Pts',(21.6062362445426,89.2753826505923,3.84369697447542));
#26109=CARTESIAN_POINT('Ctrl Pts',(20.4100629622968,92.5157489955558,3.68571380922678));
#26110=CARTESIAN_POINT('Ctrl Pts',(22.47008521615,95.288313514808,3.52773064397815));
#26111=CARTESIAN_POINT('Ctrl Pts',(25.9177921721966,95.0782652002028,3.36974747872952));
#26112=CARTESIAN_POINT('Ctrl Pts',(27.625996631401,92.0761257688787,3.21176431348088));
#26113=CARTESIAN_POINT('Ctrl Pts',(26.0452974398026,89.0049366707406,3.05378114823225));
#26114=CARTESIAN_POINT('Ctrl Pts',(22.6094455863014,88.6503742748602,2.89579798298361));
#26115=CARTESIAN_POINT('Ctrl Pts',(20.4348701137131,91.3340325854478,2.73781481773498));
#26116=CARTESIAN_POINT('Ctrl Pts',(21.4939971711375,94.6217545614396,2.57983165248634));
#26117=CARTESIAN_POINT('Ctrl Pts',(24.8261379115922,95.5314383230663,2.42184848723771));
#26118=CARTESIAN_POINT('Ctrl Pts',(27.4089769044768,93.2380224116542,2.26386532198907));
#26119=CARTESIAN_POINT('Ctrl Pts',(26.8996889870333,89.8216055629486,2.10588215674044));
#26120=CARTESIAN_POINT('Ctrl Pts',(23.760424111462,88.3812146145649,1.94789899149181));
#26121=CARTESIAN_POINT('Ctrl Pts',(20.8381769251394,90.2228836385593,1.78991582624317));
#26122=CARTESIAN_POINT('Ctrl Pts',(20.7843950202953,93.6770745568564,1.63193266099454));
#26123=CARTESIAN_POINT('Ctrl Pts',(23.6460838412789,95.6088416124304,1.47394949574591));
#26124=CARTESIAN_POINT('Ctrl Pts',(26.8312245109703,94.2698537574842,1.31596633049727));
#26125=CARTESIAN_POINT('Ctrl Pts',(27.4433138069374,90.8667064664957,1.15798316524863));
#26126=CARTESIAN_POINT('Ctrl Pts',(25.7762533017603,89.2934286920663,1.05266105508288));
#26127=CARTESIAN_POINT('Ctrl Pts',(24.7937992825328,89.0307770462543,0.999999999999999));
#26128=CARTESIAN_POINT('Ctrl Pts',(25.9134659966651,93.6359872033749,10.));
#26129=CARTESIAN_POINT('Ctrl Pts',(25.9750770243707,93.5780879660653,10.));
#26130=CARTESIAN_POINT('Ctrl Pts',(26.0333189464395,93.5170381633422,10.));
#26131=CARTESIAN_POINT('Ctrl Pts',(26.0881940942714,93.4532225723798,10.));
#26132=CARTESIAN_POINT('Ctrl Pts',(26.1445219524098,93.3877175906754,10.));
#26133=CARTESIAN_POINT('Ctrl Pts',(26.1973028564924,93.3192980131808,10.));
#26134=CARTESIAN_POINT('Ctrl Pts',(26.2465138207378,93.2483314405832,10.));
#26135=CARTESIAN_POINT('Ctrl Pts',(26.2970863146455,93.1754014215236,10.));
#26136=CARTESIAN_POINT('Ctrl Pts',(26.3438891300209,93.0997809659943,10.));
#26137=CARTESIAN_POINT('Ctrl Pts',(26.3868632217464,93.0218260240972,10.));
#26138=CARTESIAN_POINT('Ctrl Pts',(26.4057547014839,92.9875569064464,10.));
#26139=CARTESIAN_POINT('Ctrl Pts',(26.4239057978364,92.95283615278,10.));
#26140=CARTESIAN_POINT('Ctrl Pts',(26.4413090769957,92.9176919312917,10.));
#26141=CARTESIAN_POINT('Ctrl Pts',(26.4512341001089,92.8976493170593,10.));
#26142=CARTESIAN_POINT('Ctrl Pts',(26.460915876624,92.8774689544388,10.));
#26143=CARTESIAN_POINT('Ctrl Pts',(26.4703527940365,92.857155920179,10.));
#26144=CARTESIAN_POINT('Ctrl Pts',(26.4788698089222,92.8388229828856,10.));
#26145=CARTESIAN_POINT('Ctrl Pts',(26.4871897587641,92.8203762303378,10.));
#26146=CARTESIAN_POINT('Ctrl Pts',(26.4952977634944,92.8018512255385,10.));
#26147=CARTESIAN_POINT('Ctrl Pts',(26.5318624413855,92.7183089909258,10.));
#26148=CARTESIAN_POINT('Ctrl Pts',(26.5641668037515,92.6330832593894,10.));
#26149=CARTESIAN_POINT('Ctrl Pts',(26.5921857513776,92.5465727476703,10.));
#26150=CARTESIAN_POINT('Ctrl Pts',(26.620667393952,92.4586336320905,10.));
#26151=CARTESIAN_POINT('Ctrl Pts',(26.6447214109184,92.3693661981114,10.));
#26152=CARTESIAN_POINT('Ctrl Pts',(26.6642823633745,92.2791521208042,10.));
#26153=CARTESIAN_POINT('Ctrl Pts',(26.6832627492248,92.191615585952,10.));
#26154=CARTESIAN_POINT('Ctrl Pts',(26.698012980431,92.1031868494578,10.));
#26155=CARTESIAN_POINT('Ctrl Pts',(26.7084324537049,92.0141926984168,10.));
#26156=CARTESIAN_POINT('Ctrl Pts',(26.7127917941084,91.9769589738208,10.));
#26157=CARTESIAN_POINT('Ctrl Pts',(26.716392541471,91.9396260845242,10.));
#26158=CARTESIAN_POINT('Ctrl Pts',(26.7192250067013,91.9022173486574,10.));
#26159=CARTESIAN_POINT('Ctrl Pts',(26.7209955764808,91.8788332038123,10.));
#26160=CARTESIAN_POINT('Ctrl Pts',(26.7224659134468,91.8554194166649,10.));
#26161=CARTESIAN_POINT('Ctrl Pts',(26.723633360682,91.831981650528,10.));
#26162=CARTESIAN_POINT('Ctrl Pts',(26.7243176203471,91.8182443975509,10.));
#26163=CARTESIAN_POINT('Ctrl Pts',(26.7248975539059,91.8045034755717,10.));
#26164=CARTESIAN_POINT('Ctrl Pts',(26.7253726391654,91.7907682591116,10.));
#26165=CARTESIAN_POINT('Ctrl Pts',(26.7287304225257,91.693691196935,10.));
#26166=CARTESIAN_POINT('Ctrl Pts',(26.7268610241309,91.5967786841457,10.));
#26167=CARTESIAN_POINT('Ctrl Pts',(26.7196996503277,91.5004529825227,10.));
#26168=CARTESIAN_POINT('Ctrl Pts',(26.7125382765246,91.4041272808997,10.));
#26169=CARTESIAN_POINT('Ctrl Pts',(26.7000853621757,91.3083873359242,10.));
#26170=CARTESIAN_POINT('Ctrl Pts',(26.6822232210627,91.2136364705516,10.));
#26171=CARTESIAN_POINT('Ctrl Pts',(26.6651456877558,91.1230476072669,10.));
#26172=CARTESIAN_POINT('Ctrl Pts',(26.6431238131837,91.0333618679074,10.));
#26173=CARTESIAN_POINT('Ctrl Pts',(26.6164322917029,90.9448185902174,10.));
#26174=CARTESIAN_POINT('Ctrl Pts',(26.607497412219,90.9151790840601,10.));
#26175=CARTESIAN_POINT('Ctrl Pts',(26.5980388404141,90.8856676327678,10.));
#26176=CARTESIAN_POINT('Ctrl Pts',(26.5880656045218,90.8562933928029,10.));
#26177=CARTESIAN_POINT('Ctrl Pts',(26.5815842777575,90.8372038967034,10.));
#26178=CARTESIAN_POINT('Ctrl Pts',(26.5748855784003,90.8181723520075,10.));
#26179=CARTESIAN_POINT('Ctrl Pts',(26.5679718479592,90.7992013068406,10.));
#26180=CARTESIAN_POINT('Ctrl Pts',(26.5613824030662,90.7811200903749,10.));
#26181=CARTESIAN_POINT('Ctrl Pts',(26.5545958744166,90.763089621577,10.));
#26182=CARTESIAN_POINT('Ctrl Pts',(26.5476250811218,90.7451392560968,10.));
#26183=CARTESIAN_POINT('Ctrl Pts',(26.5137816042599,90.6579895224725,10.));
#26184=CARTESIAN_POINT('Ctrl Pts',(26.4755597867788,90.5726140968035,10.));
#26185=CARTESIAN_POINT('Ctrl Pts',(26.4332908111474,90.4892465922176,10.));
#26186=CARTESIAN_POINT('Ctrl Pts',(26.389452592761,90.4027840551495,10.));
#26187=CARTESIAN_POINT('Ctrl Pts',(26.3412610126046,90.3184805709489,10.));
#26188=CARTESIAN_POINT('Ctrl Pts',(26.2890295505471,90.2365997560241,10.));
#26189=CARTESIAN_POINT('Ctrl Pts',(26.236209676095,90.1537965145679,10.));
#26190=CARTESIAN_POINT('Ctrl Pts',(26.1792579755727,90.073470015158,10.));
#26191=CARTESIAN_POINT('Ctrl Pts',(26.1184468579959,89.9959077298432,10.));
#26192=CARTESIAN_POINT('Ctrl Pts',(26.0767843459152,89.9427687681253,10.));
#26193=CARTESIAN_POINT('Ctrl Pts',(26.0333092171723,89.8909275802125,10.));
#26194=CARTESIAN_POINT('Ctrl Pts',(25.9880968596718,89.8404836536506,10.));
#26195=CARTESIAN_POINT('Ctrl Pts',(25.9759899524187,89.8269758435267,10.));
#26196=CARTESIAN_POINT('Ctrl Pts',(25.9637571445712,89.8135670090811,10.));
#26197=CARTESIAN_POINT('Ctrl Pts',(25.9514135016898,89.8002735575422,10.));
#26198=CARTESIAN_POINT('Ctrl Pts',(25.8827527214455,89.7263295230642,10.));
#26199=CARTESIAN_POINT('Ctrl Pts',(25.8105780493431,89.6558533763024,10.));
#26200=CARTESIAN_POINT('Ctrl Pts',(25.7351999442575,89.5891349257962,10.));
#26201=CARTESIAN_POINT('Ctrl Pts',(25.6722950969812,89.5334567691903,10.));
#26202=CARTESIAN_POINT('Ctrl Pts',(25.6071581997643,89.4803955990503,10.));
#26203=CARTESIAN_POINT('Ctrl Pts',(25.5399460222554,89.4301336194353,10.));
#26204=CARTESIAN_POINT('Ctrl Pts',(25.5180637924313,89.4137698557527,10.));
#26205=CARTESIAN_POINT('Ctrl Pts',(25.4959614382739,89.3977029161308,10.));
#26206=CARTESIAN_POINT('Ctrl Pts',(25.4736439438293,89.3819394738383,10.));
#26207=CARTESIAN_POINT('Ctrl Pts',(25.4508750630273,89.3658572053077,10.));
#26208=CARTESIAN_POINT('Ctrl Pts',(25.427876837014,89.3500874072515,10.));
#26209=CARTESIAN_POINT('Ctrl Pts',(25.40468369501,89.3346563933276,10.));
#26210=CARTESIAN_POINT('Ctrl Pts',(25.3197384270948,89.2781400484641,10.));
#26211=CARTESIAN_POINT('Ctrl Pts',(25.2321268832309,89.2261241307586,10.));
#26212=CARTESIAN_POINT('Ctrl Pts',(25.1421393261502,89.1789167035765,10.));
#26213=CARTESIAN_POINT('Ctrl Pts',(25.058865760574,89.1352314329607,10.));
#26214=CARTESIAN_POINT('Ctrl Pts',(24.9735566878463,89.0956636399533,10.));
#26215=CARTESIAN_POINT('Ctrl Pts',(24.8864147107142,89.0604862982088,10.));
#26216=CARTESIAN_POINT('Ctrl Pts',(24.856390770472,89.0483662793479,10.));
#26217=CARTESIAN_POINT('Ctrl Pts',(24.8261490486008,89.0367677258533,10.));
#26218=CARTESIAN_POINT('Ctrl Pts',(24.7957019287906,89.0256870573369,10.));
#26219=CARTESIAN_POINT('Ctrl Pts',(21.481789046694,91.9978055657336,8.38741669750803));
#26220=CARTESIAN_POINT('Ctrl Pts',(21.480223059461,91.8252749393967,8.39833391417657));
#26221=CARTESIAN_POINT('Ctrl Pts',(21.4964590311695,91.653037231908,8.40925113084512));
#26222=CARTESIAN_POINT('Ctrl Pts',(21.5315885963512,91.4847435435215,8.42016834751366));
#26223=CARTESIAN_POINT('Ctrl Pts',(21.7010420406894,90.67295025744,8.47282940259653));
#26224=CARTESIAN_POINT('Ctrl Pts',(22.310107769231,89.9529256044114,8.52549045767941));
#26225=CARTESIAN_POINT('Ctrl Pts',(23.0825656196773,89.6512032537229,8.57815151276229));
#26226=CARTESIAN_POINT('Ctrl Pts',(23.8550234701235,89.3494809030345,8.63081256784517));
#26227=CARTESIAN_POINT('Ctrl Pts',(24.7908734424742,89.4660608546862,8.68347362292805));
#26228=CARTESIAN_POINT('Ctrl Pts',(25.4656884574097,89.9480921266005,8.73613467801093));
#26229=CARTESIAN_POINT('Ctrl Pts',(26.1405034723451,90.4301233985148,8.78879573309381));
#26230=CARTESIAN_POINT('Ctrl Pts',(26.5542835298653,91.2776059906917,8.84145678817668));
#26231=CARTESIAN_POINT('Ctrl Pts',(26.5193787375631,92.1061511997237,8.89411784325956));
#26232=CARTESIAN_POINT('Ctrl Pts',(26.484473945261,92.9346964087556,8.94677889834243));
#26233=CARTESIAN_POINT('Ctrl Pts',(26.0008843031365,93.7443042346426,8.99943995342532));
#26234=CARTESIAN_POINT('Ctrl Pts',(25.2879128423749,94.1678872245111,9.0521010085082));
#26235=CARTESIAN_POINT('Ctrl Pts',(24.5749413816134,94.5914702143796,9.10476206359107));
#26236=CARTESIAN_POINT('Ctrl Pts',(23.6325881022146,94.6290283682295,9.15742311867395));
#26237=CARTESIAN_POINT('Ctrl Pts',(22.8882531044733,94.2633578291731,9.21008417375683));
#26238=CARTESIAN_POINT('Ctrl Pts',(22.1439181067321,93.8976872901167,9.2627452288397));
#26239=CARTESIAN_POINT('Ctrl Pts',(21.5976013906482,93.1287880581541,9.31540628392258));
#26240=CARTESIAN_POINT('Ctrl Pts',(21.4970121613136,92.3057175721559,9.36806733900546));
#26241=CARTESIAN_POINT('Ctrl Pts',(21.484692259653,92.2049100849695,9.37451712517298));
#26242=CARTESIAN_POINT('Ctrl Pts',(21.4790585822288,92.1032899910618,9.3809669113405));
#26243=CARTESIAN_POINT('Ctrl Pts',(21.4798237559162,92.0015869167785,9.38741669750802));
#26244=CARTESIAN_POINT('Ctrl Pts',(23.2062007174671,89.0307770462543,10.));
#26245=CARTESIAN_POINT('Ctrl Pts',(22.2237466982397,89.2934286920664,9.94733894491712));
#26246=CARTESIAN_POINT('Ctrl Pts',(20.556685031954,90.8666986268702,9.84201683475136));
#26247=CARTESIAN_POINT('Ctrl Pts',(21.1687764925373,94.2698561140494,9.68403366950273));
#26248=CARTESIAN_POINT('Ctrl Pts',(24.3539160756188,95.60883918843,9.5260505042541));
#26249=CARTESIAN_POINT('Ctrl Pts',(27.2156041936735,93.6770751085582,9.36806733900546));
#26250=CARTESIAN_POINT('Ctrl Pts',(27.1618224985939,90.2228835192267,9.21008417375683));
#26251=CARTESIAN_POINT('Ctrl Pts',(24.2395757642923,88.3812156575976,9.05210100850819));
#26252=CARTESIAN_POINT('Ctrl Pts',(21.1003116800245,89.8216058830164,8.89411784325956));
#26253=CARTESIAN_POINT('Ctrl Pts',(20.5910237941294,93.238022224588,8.73613467801092));
#26254=CARTESIAN_POINT('Ctrl Pts',(23.1738622820844,95.5314375280541,8.57815151276229));
#26255=CARTESIAN_POINT('Ctrl Pts',(26.5060022838615,94.621754023121,8.42016834751365));
#26256=CARTESIAN_POINT('Ctrl Pts',(27.5651291305171,91.3340327163824,8.26218518226502));
#26257=CARTESIAN_POINT('Ctrl Pts',(25.3905541137142,88.6503749960184,8.10420201701638));
#26258=CARTESIAN_POINT('Ctrl Pts',(21.9547029986072,89.0049373072501,7.94621885176775));
#26259=CARTESIAN_POINT('Ctrl Pts',(20.3740041419998,92.0761257542051,7.78823568651912));
#26260=CARTESIAN_POINT('Ctrl Pts',(22.0822082378054,95.0782645420543,7.63025252127048));
#26261=CARTESIAN_POINT('Ctrl Pts',(25.5299144568995,95.2883128130433,7.47226935602185));
#26262=CARTESIAN_POINT('Ctrl Pts',(27.5899362712429,92.5157488852068,7.31428619077321));
#26263=CARTESIAN_POINT('Ctrl Pts',(26.3937632442238,89.2753832325168,7.15630302552458));
#26264=CARTESIAN_POINT('Ctrl Pts',(23.0263653048422,88.5063379273328,6.99831986027595));
#26265=CARTESIAN_POINT('Ctrl Pts',(20.542087239558,90.9061633964473,6.84033669502731));
#26266=CARTESIAN_POINT('Ctrl Pts',(21.1942540870207,94.2981359861555,6.68235352977868));
#26267=CARTESIAN_POINT('Ctrl Pts',(24.3913282372869,95.6056208028792,6.52437036453004));
#26268=CARTESIAN_POINT('Ctrl Pts',(27.2334543225922,93.6426844805108,6.36638719928141));
#26269=CARTESIAN_POINT('Ctrl Pts',(27.1427269710462,90.1897772675991,6.20840403403277));
#26270=CARTESIAN_POINT('Ctrl Pts',(24.2014389895034,88.3788038589624,6.05042086878413));
#26271=CARTESIAN_POINT('Ctrl Pts',(21.077438968569,89.8523789498237,5.8924377035355));
#26272=CARTESIAN_POINT('Ctrl Pts',(20.6043015565953,93.2739196359127,5.73445453828687));
#26273=CARTESIAN_POINT('Ctrl Pts',(23.2111785351691,95.5399717307178,5.57647137303823));
#26274=CARTESIAN_POINT('Ctrl Pts',(26.5335435065542,94.5951486388852,5.4184882077896));
#26275=CARTESIAN_POINT('Ctrl Pts',(27.5578980422048,91.2964371536349,5.26050504254097));
#26276=CARTESIAN_POINT('Ctrl Pts',(25.3551176148943,88.6358811841043,5.10252187729233));
#26277=CARTESIAN_POINT('Ctrl Pts',(21.9231992578101,89.0266958052455,4.94453871204369));
#26278=CARTESIAN_POINT('Ctrl Pts',(20.3750100595362,92.1143988161452,4.78655554679506));
#26279=CARTESIAN_POINT('Ctrl Pts',(22.1148104659795,95.0983381963849,4.62857238154642));
#26280=CARTESIAN_POINT('Ctrl Pts',(25.5645421252575,95.2719790790493,4.47058921629779));
#26281=CARTESIAN_POINT('Ctrl Pts',(27.5951806759185,92.4778232584365,4.31260605104916));
#26282=CARTESIAN_POINT('Ctrl Pts',(26.3648676419543,89.2502654310841,4.15462288580052));
#26283=CARTESIAN_POINT('Ctrl Pts',(22.9895389394378,88.5168107165773,3.99663972055189));
#26284=CARTESIAN_POINT('Ctrl Pts',(20.5307329066189,90.9427275616556,3.83865655530325));
#26285=CARTESIAN_POINT('Ctrl Pts',(21.2186705439485,94.3276266140658,3.68067339005462));
#26286=CARTESIAN_POINT('Ctrl Pts',(24.4293689246723,95.601288842286,3.52269022480598));
#26287=CARTESIAN_POINT('Ctrl Pts',(27.2506150476498,93.6084592491481,3.36470705955735));
#26288=CARTESIAN_POINT('Ctrl Pts',(27.1234423470096,90.1567020569745,3.20672389430872));
#26289=CARTESIAN_POINT('Ctrl Pts',(24.1632008787755,88.3768793413442,3.04874072906008));
#26290=CARTESIAN_POINT('Ctrl Pts',(21.0549305391037,89.8833500612564,2.89075756381145));
#26291=CARTESIAN_POINT('Ctrl Pts',(20.6179389343519,93.309695882881,2.73277439856281));
#26292=CARTESIAN_POINT('Ctrl Pts',(23.2485917195109,95.548100055872,2.57479123331418));
#26293=CARTESIAN_POINT('Ctrl Pts',(26.5607983477153,94.5682620509693,2.41680806806554));
#26294=CARTESIAN_POINT('Ctrl Pts',(27.5502716608787,91.2589111130016,2.25882490281691));
#26295=CARTESIAN_POINT('Ctrl Pts',(25.3195310914441,88.6217767625239,2.10084173756827));
#26296=CARTESIAN_POINT('Ctrl Pts',(21.891923244154,89.0487578560498,1.94285857231964));
#26297=CARTESIAN_POINT('Ctrl Pts',(20.376428363266,92.1527150135633,1.78487540707101));
#26298=CARTESIAN_POINT('Ctrl Pts',(22.1476051992024,95.1179528805984,1.62689224182237));
#26299=CARTESIAN_POINT('Ctrl Pts',(25.5990315417433,95.2555126520043,1.46890907657374));
#26300=CARTESIAN_POINT('Ctrl Pts',(27.5999506290771,92.4393708209745,1.3109259113251));
#26301=CARTESIAN_POINT('Ctrl Pts',(26.3358592338276,89.2264213520665,1.15294274607647));
#26302=CARTESIAN_POINT('Ctrl Pts',(22.9525239108491,88.5256846472501,0.994959580827833));
#26303=CARTESIAN_POINT('Ctrl Pts',(20.5204084922262,90.9835193506338,0.836976415579198));
#26304=CARTESIAN_POINT('Ctrl Pts',(21.0030718657858,93.2243470893905,0.731654305413442));
#26305=CARTESIAN_POINT('Ctrl Pts',(21.6639373423039,93.9973015569307,0.678993250330564));
#26306=CARTESIAN_POINT('Ctrl Pts',(23.254067145653,89.2098224301579,10.1070022498898));
#26307=CARTESIAN_POINT('Ctrl Pts',(22.3308555140066,89.4566360720578,10.0543411948069));
#26308=CARTESIAN_POINT('Ctrl Pts',(20.7643183622759,90.9350371728775,9.94901908464117));
#26309=CARTESIAN_POINT('Ctrl Pts',(21.3395004522086,94.1329828425986,9.79103591939255));
#26310=CARTESIAN_POINT('Ctrl Pts',(24.332574788482,95.3912246785046,9.6330527541439));
#26311=CARTESIAN_POINT('Ctrl Pts',(27.0217019181264,93.5759467792531,9.47506958889527));
#26312=CARTESIAN_POINT('Ctrl Pts',(26.9711632817165,90.3300443850485,9.31708642364663));
#26313=CARTESIAN_POINT('Ctrl Pts',(24.2251292456712,88.5994298644601,9.15910325839801));
#26314=CARTESIAN_POINT('Ctrl Pts',(21.2751640964776,89.9529639578542,9.00112009314937));
#26315=CARTESIAN_POINT('Ctrl Pts',(20.7965864827541,93.1633689675119,8.84313692790073));
#26316=CARTESIAN_POINT('Ctrl Pts',(23.2236787314268,95.3184903705681,8.6851537626521));
#26317=CARTESIAN_POINT('Ctrl Pts',(26.3548892997688,94.4636611608191,8.52717059740346));
#26318=CARTESIAN_POINT('Ctrl Pts',(27.3501503553349,91.3741908216577,8.36918743215484));
#26319=CARTESIAN_POINT('Ctrl Pts',(25.3067031200343,88.8523587823873,8.21120426690619));
#26320=CARTESIAN_POINT('Ctrl Pts',(22.0780352618005,89.1855408382048,8.05322110165756));
#26321=CARTESIAN_POINT('Ctrl Pts',(20.592653206264,92.0715353394405,7.89523793640893));
#26322=CARTESIAN_POINT('Ctrl Pts',(22.1978518818355,94.8926439048456,7.73725477116029));
#26323=CARTESIAN_POINT('Ctrl Pts',(25.4376599763359,95.0900261773889,7.57927160591166));
#26324=CARTESIAN_POINT('Ctrl Pts',(27.3734616151168,92.4846490120789,7.42128844066302));
#26325=CARTESIAN_POINT('Ctrl Pts',(26.2494183210864,89.439678761254,7.26330527541439));
#26326=CARTESIAN_POINT('Ctrl Pts',(23.0850758834993,88.7170072090857,7.10532211016575));
#26327=CARTESIAN_POINT('Ctrl Pts',(20.7506008228567,90.9721222003707,6.94733894491712));
#26328=CARTESIAN_POINT('Ctrl Pts',(21.3634417371065,94.1595574266086,6.78935577966849));
#26329=CARTESIAN_POINT('Ctrl Pts',(24.3677309811802,95.3882003629463,6.63137261441985));
#26330=CARTESIAN_POINT('Ctrl Pts',(27.038475676818,93.5436299204366,6.47338944917122));
#26331=CARTESIAN_POINT('Ctrl Pts',(26.9532192224532,90.2989344542175,6.31540628392258));
#26332=CARTESIAN_POINT('Ctrl Pts',(24.1892921343259,88.5971634982897,6.15742311867395));
#26333=CARTESIAN_POINT('Ctrl Pts',(21.2536706190734,89.9818813958839,5.99943995342532));
#26334=CARTESIAN_POINT('Ctrl Pts',(20.8090635905992,93.1971017499447,5.84145678817668));
#26335=CARTESIAN_POINT('Ctrl Pts',(23.2587447988691,95.3265099572479,5.68347362292804));
#26336=CARTESIAN_POINT('Ctrl Pts',(26.3807697752333,94.4386600923617,5.52549045767941));
#26337=CARTESIAN_POINT('Ctrl Pts',(27.3433553046672,91.3388622870417,5.36750729243078));
#26338=CARTESIAN_POINT('Ctrl Pts',(25.2734034568897,88.8387389533836,5.20952412718214));
#26339=CARTESIAN_POINT('Ctrl Pts',(22.0484312097279,89.205987289686,5.05154096193351));
#26340=CARTESIAN_POINT('Ctrl Pts',(20.5935984665529,92.1075005197647,4.89355779668487));
#26341=CARTESIAN_POINT('Ctrl Pts',(22.2284881820378,94.9115071094384,4.73557463143624));
#26342=CARTESIAN_POINT('Ctrl Pts',(25.4701995818333,95.0746773743747,4.5775914661876));
#26343=CARTESIAN_POINT('Ctrl Pts',(27.3783897800007,92.4490103164387,4.41960830093897));
#26344=CARTESIAN_POINT('Ctrl Pts',(26.2222651356991,89.4160755737354,4.26162513569033));
#26345=CARTESIAN_POINT('Ctrl Pts',(23.0504701633055,88.726848484766,4.1036419704417));
#26346=CARTESIAN_POINT('Ctrl Pts',(20.7399311609349,91.0064815311496,3.94565880519306));
#26347=CARTESIAN_POINT('Ctrl Pts',(21.3863858714865,94.1872697573423,3.78767563994443));
#26348=CARTESIAN_POINT('Ctrl Pts',(24.4034777992324,95.3841296213856,3.6296924746958));
#26349=CARTESIAN_POINT('Ctrl Pts',(27.0546016029892,93.5114684848159,3.47170930944716));
#26350=CARTESIAN_POINT('Ctrl Pts',(26.9350974692983,90.267853692604,3.31372614419853));
#26351=CARTESIAN_POINT('Ctrl Pts',(24.1533597976412,88.5953550298875,3.15574297894989));
#26352=CARTESIAN_POINT('Ctrl Pts',(21.2325194573032,90.0109849363652,2.99775981370126));
#26353=CARTESIAN_POINT('Ctrl Pts',(20.8218786287828,93.2307206742826,2.83977664845262));
#26354=CARTESIAN_POINT('Ctrl Pts',(23.2939019525734,95.3341481410013,2.68179348320399));
#26355=CARTESIAN_POINT('Ctrl Pts',(26.4063811380923,94.4133947769235,2.52381031795535));
#26356=CARTESIAN_POINT('Ctrl Pts',(27.3361887973193,91.3035990823277,2.36582715270672));
#26357=CARTESIAN_POINT('Ctrl Pts',(25.2399628156627,88.8254850343136,2.20784398745808));
#26358=CARTESIAN_POINT('Ctrl Pts',(22.0190411527544,89.2267189896149,2.04986082220945));
#26359=CARTESIAN_POINT('Ctrl Pts',(20.5949312459756,92.1435062344795,1.89187765696082));
#26360=CARTESIAN_POINT('Ctrl Pts',(22.259305379154,94.9299390200038,1.73389449171218));
#26361=CARTESIAN_POINT('Ctrl Pts',(25.502609272104,95.0592038797561,1.57591132646355));
#26362=CARTESIAN_POINT('Ctrl Pts',(27.382872102992,92.4128765770114,1.41792816121491));
#26363=CARTESIAN_POINT('Ctrl Pts',(26.1950059466948,89.3936693026388,1.25994499596628));
#26364=CARTESIAN_POINT('Ctrl Pts',(23.0156871563963,88.7351873137138,1.10196183071764));
#26365=CARTESIAN_POINT('Ctrl Pts',(20.7302293130409,91.04481355822,0.94397866546901));
#26366=CARTESIAN_POINT('Ctrl Pts',(21.1837878836398,93.1505184486768,0.838656555303253));
#26367=CARTESIAN_POINT('Ctrl Pts',(21.8048028959809,93.8768634390788,0.785995500220375));
#26368=CARTESIAN_POINT('Ctrl Pts',(23.3019335738389,89.3888678140614,10.2140044997796));
#26369=CARTESIAN_POINT('Ctrl Pts',(22.4379643297735,89.6198434520493,10.1613434446967));
#26370=CARTESIAN_POINT('Ctrl Pts',(20.9719516925979,91.0033757188849,10.056021334531));
#26371=CARTESIAN_POINT('Ctrl Pts',(21.5102244118799,93.9961095711478,9.89803816928235));
#26372=CARTESIAN_POINT('Ctrl Pts',(24.3112335013453,95.1736101685792,9.74005500403372));
#26373=CARTESIAN_POINT('Ctrl Pts',(26.8277996425793,93.4748184499478,9.58207183878509));
#26374=CARTESIAN_POINT('Ctrl Pts',(26.780504064839,90.4372052508703,9.42408867353644));
#26375=CARTESIAN_POINT('Ctrl Pts',(24.21068272705,88.8176440713225,9.26610550828783));
#26376=CARTESIAN_POINT('Ctrl Pts',(21.4500165129308,90.0843220326922,9.10812234303918));
#26377=CARTESIAN_POINT('Ctrl Pts',(21.0021491713788,93.0887157104357,8.95013917779055));
#26378=CARTESIAN_POINT('Ctrl Pts',(23.2734951807691,95.1055432130824,8.79215601254191));
#26379=CARTESIAN_POINT('Ctrl Pts',(26.2037763156761,94.305568298517,8.63417284729328));
#26380=CARTESIAN_POINT('Ctrl Pts',(27.1351715801527,91.4143489269332,8.47618968204464));
#26381=CARTESIAN_POINT('Ctrl Pts',(25.2228521263544,89.054342568756,8.31820651679601));
#26382=CARTESIAN_POINT('Ctrl Pts',(22.2013675249939,89.3661443691598,8.16022335154737));
#26383=CARTESIAN_POINT('Ctrl Pts',(20.8113022705282,92.0669449246757,8.00224018629874));
#26384=CARTESIAN_POINT('Ctrl Pts',(22.3134955258657,94.707023267637,7.8442570210501));
#26385=CARTESIAN_POINT('Ctrl Pts',(25.3454054957724,94.8917395417344,7.68627385580147));
#26386=CARTESIAN_POINT('Ctrl Pts',(27.1569869589906,92.4535491389511,7.52829069055284));
#26387=CARTESIAN_POINT('Ctrl Pts',(26.105073397949,89.603974289991,7.37030752530419));
#26388=CARTESIAN_POINT('Ctrl Pts',(23.1437864621564,88.9276764908387,7.21232436005557));
#26389=CARTESIAN_POINT('Ctrl Pts',(20.9591144061554,91.038081004294,7.05434119480692));
#26390=CARTESIAN_POINT('Ctrl Pts',(21.5326293871924,94.0209788670617,6.8963580295583));
#26391=CARTESIAN_POINT('Ctrl Pts',(24.3441337250736,95.1707799230134,6.73837486430966));
#26392=CARTESIAN_POINT('Ctrl Pts',(26.8434970310438,93.4445753603625,6.58039169906103));
#26393=CARTESIAN_POINT('Ctrl Pts',(26.7637114738602,90.4080916408359,6.42240853381239));
#26394=CARTESIAN_POINT('Ctrl Pts',(24.1771452791484,88.8155231376169,6.26442536856376));
#26395=CARTESIAN_POINT('Ctrl Pts',(21.4299022695778,90.1113838419441,6.10644220331513));
#26396=CARTESIAN_POINT('Ctrl Pts',(21.0138256246031,93.1202838639768,5.94845903806649));
#26397=CARTESIAN_POINT('Ctrl Pts',(23.3063110625691,95.113048183778,5.79047587281785));
#26398=CARTESIAN_POINT('Ctrl Pts',(26.2279960439124,94.2821715458382,5.63249270756922));
#26399=CARTESIAN_POINT('Ctrl Pts',(27.1288125671295,91.3812874204487,5.47450954232058));
#26400=CARTESIAN_POINT('Ctrl Pts',(25.1916892988851,89.0415967226626,5.31652637707195));
#26401=CARTESIAN_POINT('Ctrl Pts',(22.1736631616456,89.3852787741264,5.15854321182332));
#26402=CARTESIAN_POINT('Ctrl Pts',(20.8121868735697,92.1006022233842,5.00056004657468));
#26403=CARTESIAN_POINT('Ctrl Pts',(22.3421658980961,94.7246760224918,4.84257688132605));
#26404=CARTESIAN_POINT('Ctrl Pts',(25.375857038409,94.8773756697003,4.68459371607741));
#26405=CARTESIAN_POINT('Ctrl Pts',(27.1615988840828,92.4201973744409,4.52661055082878));
#26406=CARTESIAN_POINT('Ctrl Pts',(26.0796626294438,89.5818857163869,4.36862738558014));
#26407=CARTESIAN_POINT('Ctrl Pts',(23.1114013871733,88.9368862529545,4.21064422033151));
#26408=CARTESIAN_POINT('Ctrl Pts',(20.9491294152507,91.0702355006436,4.05266105508287));
#26409=CARTESIAN_POINT('Ctrl Pts',(21.5541011990246,94.0469129006186,3.89467788983424));
#26410=CARTESIAN_POINT('Ctrl Pts',(24.3775866737926,95.1669704004854,3.7366947245856));
#26411=CARTESIAN_POINT('Ctrl Pts',(26.8585881583285,93.4144777204836,3.57871155933697));
#26412=CARTESIAN_POINT('Ctrl Pts',(26.7467525915869,90.3790053282334,3.42072839408834));
#26413=CARTESIAN_POINT('Ctrl Pts',(24.1435187165069,88.8138307184307,3.2627452288397));
#26414=CARTESIAN_POINT('Ctrl Pts',(21.4101083755027,90.138619811474,3.10476206359106));
#26415=CARTESIAN_POINT('Ctrl Pts',(21.0258183232138,93.1517454656843,2.94677889834244));
#26416=CARTESIAN_POINT('Ctrl Pts',(23.3392121856357,95.1201962261306,2.78879573309379));
#26417=CARTESIAN_POINT('Ctrl Pts',(26.2519639284692,94.2585275028778,2.63081256784517));
#26418=CARTESIAN_POINT('Ctrl Pts',(27.1221059337601,91.3482870516537,2.47282940259653));
#26419=CARTESIAN_POINT('Ctrl Pts',(25.1603945398812,89.0291933061033,2.3148462373479));
#26420=CARTESIAN_POINT('Ctrl Pts',(22.1461590613549,89.4046801231798,2.15686307209926));
#26421=CARTESIAN_POINT('Ctrl Pts',(20.8134341286852,92.134297455396,1.99887990685063));
#26422=CARTESIAN_POINT('Ctrl Pts',(22.3710055591055,94.741925159409,1.84089674160199));
#26423=CARTESIAN_POINT('Ctrl Pts',(25.4061870024647,94.8628951075081,1.68291357635336));
#26424=CARTESIAN_POINT('Ctrl Pts',(27.1657935769071,92.3863823330482,1.52493041110472));
#26425=CARTESIAN_POINT('Ctrl Pts',(26.0541526595619,89.560917253211,1.36694724585609));
#26426=CARTESIAN_POINT('Ctrl Pts',(23.0788504019435,88.9446899801776,1.20896408060745));
#26427=CARTESIAN_POINT('Ctrl Pts',(20.9400501338557,91.106107765806,1.05098091535882));
#26428=CARTESIAN_POINT('Ctrl Pts',(21.3645039014938,93.076689807963,0.945658805193063));
#26429=CARTESIAN_POINT('Ctrl Pts',(21.945668449658,93.7564253212269,0.892997750110186));
#26430=CARTESIAN_POINT('Ctrl Pts',(23.3498000020249,89.5679131979649,10.3210067496694));
#26431=CARTESIAN_POINT('Ctrl Pts',(22.5450731455404,89.7830508320407,10.2683456945866));
#26432=CARTESIAN_POINT('Ctrl Pts',(21.1795850229198,91.0717142648921,10.1630235844208));
#26433=CARTESIAN_POINT('Ctrl Pts',(21.6809483715512,93.859236299697,10.0050404191722));
#26434=CARTESIAN_POINT('Ctrl Pts',(24.2898922142086,94.9559956586539,9.84705725392353));
#26435=CARTESIAN_POINT('Ctrl Pts',(26.6338973670321,93.3736901206426,9.68907408867489));
#26436=CARTESIAN_POINT('Ctrl Pts',(26.5898448479616,90.5443661166922,9.53109092342625));
#26437=CARTESIAN_POINT('Ctrl Pts',(24.1962362084288,89.0358582781851,9.37310775817764));
#26438=CARTESIAN_POINT('Ctrl Pts',(21.6248689293839,90.2156801075301,9.21512459292898));
#26439=CARTESIAN_POINT('Ctrl Pts',(21.2077118600035,93.0140624533595,9.05714142768036));
#26440=CARTESIAN_POINT('Ctrl Pts',(23.3233116301114,94.8925960555965,8.89915826243172));
#26441=CARTESIAN_POINT('Ctrl Pts',(26.0526633315834,94.1474754362151,8.74117509718309));
#26442=CARTESIAN_POINT('Ctrl Pts',(26.9201928049705,91.4545070322085,8.58319193193445));
#26443=CARTESIAN_POINT('Ctrl Pts',(25.1390011326746,89.2563263551249,8.42520876668581));
#26444=CARTESIAN_POINT('Ctrl Pts',(22.3246997881873,89.5467479001147,8.26722560143719));
#26445=CARTESIAN_POINT('Ctrl Pts',(21.0299513347924,92.0623545099109,8.10924243618855));
#26446=CARTESIAN_POINT('Ctrl Pts',(22.4291391698959,94.5214026304284,7.95125927093991));
#26447=CARTESIAN_POINT('Ctrl Pts',(25.2531510152088,94.69345290608,7.79327610569128));
#26448=CARTESIAN_POINT('Ctrl Pts',(26.9405123028645,92.4224492658233,7.63529294044264));
#26449=CARTESIAN_POINT('Ctrl Pts',(25.9607284748115,89.7682698187282,7.47730977519401));
#26450=CARTESIAN_POINT('Ctrl Pts',(23.2024970408135,89.1383457725916,7.31932660994538));
#26451=CARTESIAN_POINT('Ctrl Pts',(21.1676279894541,91.1040398082174,7.16134344469674));
#26452=CARTESIAN_POINT('Ctrl Pts',(21.7018170372782,93.8824003075146,7.00336027944811));
#26453=CARTESIAN_POINT('Ctrl Pts',(24.3205364689669,94.9533594830808,6.84537711419947));
#26454=CARTESIAN_POINT('Ctrl Pts',(26.6485183852695,93.3455208002881,6.68739394895084));
#26455=CARTESIAN_POINT('Ctrl Pts',(26.5742037252672,90.5172488274544,6.5294107837022));
#26456=CARTESIAN_POINT('Ctrl Pts',(24.1649984239709,89.0338827769442,6.37142761845357));
#26457=CARTESIAN_POINT('Ctrl Pts',(21.6061339200822,90.2408862880042,6.21344445320494));
#26458=CARTESIAN_POINT('Ctrl Pts',(21.218587658607,93.0434659780088,6.0554612879563));
#26459=CARTESIAN_POINT('Ctrl Pts',(23.3538773262692,94.8995864103082,5.89747812270766));
#26460=CARTESIAN_POINT('Ctrl Pts',(26.0752223125915,94.1256829993147,5.73949495745903));
#26461=CARTESIAN_POINT('Ctrl Pts',(26.9142698295919,91.4237125538557,5.5815117922104));
#26462=CARTESIAN_POINT('Ctrl Pts',(25.1099751408805,89.2444544919418,5.42352862696176));
#26463=CARTESIAN_POINT('Ctrl Pts',(22.2988951135634,89.5645702585668,5.26554546171313));
#26464=CARTESIAN_POINT('Ctrl Pts',(21.0307752805864,92.0937039270037,5.10756229646449));
#26465=CARTESIAN_POINT('Ctrl Pts',(22.4558436141543,94.5378449355453,4.94957913121586));
#26466=CARTESIAN_POINT('Ctrl Pts',(25.2815144949848,94.6800739650258,4.79159596596722));
#26467=CARTESIAN_POINT('Ctrl Pts',(26.9448079881649,92.3913844324431,4.63361280071859));
#26468=CARTESIAN_POINT('Ctrl Pts',(25.9370601231886,89.7476958590382,4.47562963546995));
#26469=CARTESIAN_POINT('Ctrl Pts',(23.172332611041,89.1469240211431,4.31764647022132));
#26470=CARTESIAN_POINT('Ctrl Pts',(21.1583276695667,91.1339894701376,4.15966330497269));
#26471=CARTESIAN_POINT('Ctrl Pts',(21.7218165265627,93.9065560438949,4.00168013972405));
#26472=CARTESIAN_POINT('Ctrl Pts',(24.3516955483528,94.9498111795851,3.84369697447542));
#26473=CARTESIAN_POINT('Ctrl Pts',(26.6625747136679,93.3174869561512,3.68571380922678));
#26474=CARTESIAN_POINT('Ctrl Pts',(26.5584077138756,90.4901569638631,3.52773064397815));
#26475=CARTESIAN_POINT('Ctrl Pts',(24.1336776353725,89.0323064069738,3.36974747872951));
#26476=CARTESIAN_POINT('Ctrl Pts',(21.5876972937022,90.266254686583,3.21176431348088));
#26477=CARTESIAN_POINT('Ctrl Pts',(21.2297580176447,93.0727702570857,3.05378114823224));
#26478=CARTESIAN_POINT('Ctrl Pts',(23.3845224186982,94.90624431126,2.89579798298361));
#26479=CARTESIAN_POINT('Ctrl Pts',(26.0975467188461,94.103660228832,2.73781481773498));
#26480=CARTESIAN_POINT('Ctrl Pts',(26.9080230702008,91.3929750209798,2.57983165248634));
#26481=CARTESIAN_POINT('Ctrl Pts',(25.0808262640998,89.232901577893,2.42184848723771));
#26482=CARTESIAN_POINT('Ctrl Pts',(22.2732769699553,89.5826412567449,2.26386532198907));
#26483=CARTESIAN_POINT('Ctrl Pts',(21.0319370113949,92.1250886763122,2.10588215674044));
#26484=CARTESIAN_POINT('Ctrl Pts',(22.4827057390571,94.5539112988145,1.9478989914918));
#26485=CARTESIAN_POINT('Ctrl Pts',(25.3097647328254,94.6665863352599,1.78991582624317));
#26486=CARTESIAN_POINT('Ctrl Pts',(26.948715050822,92.3598880890851,1.63193266099453));
#26487=CARTESIAN_POINT('Ctrl Pts',(25.9132993724291,89.7281652037832,1.4739494957459));
#26488=CARTESIAN_POINT('Ctrl Pts',(23.1420136474907,89.1541926466413,1.31596633049726));
#26489=CARTESIAN_POINT('Ctrl Pts',(21.1498709546704,91.1674019733922,1.15798316524863));
#26490=CARTESIAN_POINT('Ctrl Pts',(21.5452199193479,93.0028611672493,1.05266105508287));
#26491=CARTESIAN_POINT('Ctrl Pts',(22.086534003335,93.635987203375,0.999999999999996));
#26492=CARTESIAN_POINT('Ctrl Pts',(21.4850510509789,92.0017493960693,9.11258330249198));
#26493=CARTESIAN_POINT('Ctrl Pts',(21.4831440162074,92.2947752212131,9.09410267755477));
#26494=CARTESIAN_POINT('Ctrl Pts',(21.5304974072668,92.5872051529597,9.07562205261756));
#26495=CARTESIAN_POINT('Ctrl Pts',(21.6298379999182,92.8607543294275,9.05714142768035));
#26496=CARTESIAN_POINT('Ctrl Pts',(21.9129117833728,93.6402403207719,9.00448037259747));
#26497=CARTESIAN_POINT('Ctrl Pts',(22.6181117067421,94.2664181881842,8.95181931751459));
#26498=CARTESIAN_POINT('Ctrl Pts',(23.4256036186721,94.4553203519934,8.89915826243172));
#26499=CARTESIAN_POINT('Ctrl Pts',(24.2330955306021,94.6442225158027,8.84649720734884));
#26500=CARTESIAN_POINT('Ctrl Pts',(25.1428794310927,94.3958489760089,8.79383615226596));
#26501=CARTESIAN_POINT('Ctrl Pts',(25.7423596269026,93.8228341387776,8.74117509718308));
#26502=CARTESIAN_POINT('Ctrl Pts',(26.3418398227124,93.2498193015462,8.6885140421002));
#26503=CARTESIAN_POINT('Ctrl Pts',(26.6310163138414,92.3521631668773,8.63585298701732));
#26504=CARTESIAN_POINT('Ctrl Pts',(26.47873928069,91.5369716533623,8.58319193193445));
#26505=CARTESIAN_POINT('Ctrl Pts',(26.3264622475385,90.7217801398473,8.53053087685157));
#26506=CARTESIAN_POINT('Ctrl Pts',(25.7327316901066,89.9890532474861,8.47786982176869));
#26507=CARTESIAN_POINT('Ctrl Pts',(24.9668161873094,89.6710933921371,8.42520876668581));
#26508=CARTESIAN_POINT('Ctrl Pts',(24.2009006845121,89.3531335367881,8.37254771160293));
#26509=CARTESIAN_POINT('Ctrl Pts',(23.2628002363497,89.4499407184514,8.31988665652006));
#26510=CARTESIAN_POINT('Ctrl Pts',(22.5779586033693,89.9176120775824,8.26722560143718));
#26511=CARTESIAN_POINT('Ctrl Pts',(21.9075993003968,90.3753936014114,8.21567816845545));
#26512=CARTESIAN_POINT('Ctrl Pts',(21.4799007520941,91.1885198389857,8.16413073547371));
#26513=CARTESIAN_POINT('Ctrl Pts',(21.4784369335473,92.0003195913806,8.11258330249198));
#26514=CARTESIAN_POINT('Ctrl Pts',(23.2062007174671,89.0307770462543,10.));
#26515=CARTESIAN_POINT('Ctrl Pts',(23.1131475235312,89.064816320262,10.));
#26516=CARTESIAN_POINT('Ctrl Pts',(23.0221596064779,89.1036239095806,10.));
#26517=CARTESIAN_POINT('Ctrl Pts',(22.9334454653316,89.1468715855098,10.));
#26518=CARTESIAN_POINT('Ctrl Pts',(22.8427656611047,89.1910775118239,10.));
#26519=CARTESIAN_POINT('Ctrl Pts',(22.7544608424803,89.2399230814568,10.));
#26520=CARTESIAN_POINT('Ctrl Pts',(22.6687825963672,89.2931033001226,10.));
#26521=CARTESIAN_POINT('Ctrl Pts',(22.586330110816,89.3442812993241,10.));
#26522=CARTESIAN_POINT('Ctrl Pts',(22.5063098561179,89.3994745706755,10.));
#26523=CARTESIAN_POINT('Ctrl Pts',(22.4289790559017,89.458441358607,10.));
#26524=CARTESIAN_POINT('Ctrl Pts',(22.3613146057126,89.5100372980471,10.));
#26525=CARTESIAN_POINT('Ctrl Pts',(22.2957095595976,89.5645230341413,10.));
#26526=CARTESIAN_POINT('Ctrl Pts',(22.2323608843388,89.6217493205767,10.));
#26527=CARTESIAN_POINT('Ctrl Pts',(22.218262116408,89.6344855005946,10.));
#26528=CARTESIAN_POINT('Ctrl Pts',(22.2042725067628,89.6473601252669,10.));
#26529=CARTESIAN_POINT('Ctrl Pts',(22.1904136996835,89.6603531214548,10.));
#26530=CARTESIAN_POINT('Ctrl Pts',(22.1179829795791,89.7282588268171,10.));
#26531=CARTESIAN_POINT('Ctrl Pts',(22.0490179328543,89.799486285336,10.));
#26532=CARTESIAN_POINT('Ctrl Pts',(21.9837585062309,89.8737448951122,10.));
#26533=CARTESIAN_POINT('Ctrl Pts',(21.918858759645,89.9475942254794,10.));
#26534=CARTESIAN_POINT('Ctrl Pts',(21.8576234120103,90.0244421833075,10.));
#26535=CARTESIAN_POINT('Ctrl Pts',(21.800332072969,90.1040297128831,10.));
#26536=CARTESIAN_POINT('Ctrl Pts',(21.7451392509027,90.1807020412326,10.));
#26537=CARTESIAN_POINT('Ctrl Pts',(21.6936066323894,90.2599176592597,10.));
#26538=CARTESIAN_POINT('Ctrl Pts',(21.6460291433951,90.341458559806,10.));
#26539=CARTESIAN_POINT('Ctrl Pts',(21.626040380651,90.3757163936978,10.));
#26540=CARTESIAN_POINT('Ctrl Pts',(21.606750309037,90.4103847699114,10.));
#26541=CARTESIAN_POINT('Ctrl Pts',(21.5881834031431,90.4454478211808,10.));
#26542=CARTESIAN_POINT('Ctrl Pts',(21.5751468384104,90.4700669871428,10.));
#26543=CARTESIAN_POINT('Ctrl Pts',(21.5624668273574,90.4948807308745,10.));
#26544=CARTESIAN_POINT('Ctrl Pts',(21.5501523284354,90.5198835657242,10.));
#26545=CARTESIAN_POINT('Ctrl Pts',(21.5423998388932,90.5356238907609,10.));
#26546=CARTESIAN_POINT('Ctrl Pts',(21.5347913334218,90.551441280599,10.));
#26547=CARTESIAN_POINT('Ctrl Pts',(21.5273387128466,90.5673132394905,10.));
#26548=CARTESIAN_POINT('Ctrl Pts',(21.4852181501849,90.6570180396091,10.));
#26549=CARTESIAN_POINT('Ctrl Pts',(21.4479997999212,90.748607534526,10.));
#26550=CARTESIAN_POINT('Ctrl Pts',(21.4159753088276,90.8418092601306,10.));
#26551=CARTESIAN_POINT('Ctrl Pts',(21.3861128448267,90.9287187809577,10.));
#26552=CARTESIAN_POINT('Ctrl Pts',(21.360766797266,91.0170309840337,10.));
#26553=CARTESIAN_POINT('Ctrl Pts',(21.340224189409,91.1065336320268,10.));
#26554=CARTESIAN_POINT('Ctrl Pts',(21.3387369151257,91.1130135778824,10.));
#26555=CARTESIAN_POINT('Ctrl Pts',(21.3372748417258,91.1194997648427,10.));
#26556=CARTESIAN_POINT('Ctrl Pts',(21.3358380889382,91.125992112682,10.));
#26557=CARTESIAN_POINT('Ctrl Pts',(21.3152524900323,91.219013591207,10.));
#26558=CARTESIAN_POINT('Ctrl Pts',(21.2998606756254,91.3133008086048,10.));
#26559=CARTESIAN_POINT('Ctrl Pts',(21.2895856382541,91.4084457389737,10.));
#26560=CARTESIAN_POINT('Ctrl Pts',(21.2837680062684,91.4623159265151,10.));
#26561=CARTESIAN_POINT('Ctrl Pts',(21.2795916051018,91.5164608839292,10.));
#26562=CARTESIAN_POINT('Ctrl Pts',(21.2770493497667,91.5708038567304,10.));
#26563=CARTESIAN_POINT('Ctrl Pts',(21.2764020101031,91.5846413187856,10.));
#26564=CARTESIAN_POINT('Ctrl Pts',(21.2758607757032,91.5984902137829,10.));
#26565=CARTESIAN_POINT('Ctrl Pts',(21.2754257103763,91.612337039112,10.));
#26566=CARTESIAN_POINT('Ctrl Pts',(21.2724969038989,91.7055521707492,10.));
#26567=CARTESIAN_POINT('Ctrl Pts',(21.2743674875468,91.7988245803011,10.));
#26568=CARTESIAN_POINT('Ctrl Pts',(21.28090259303,91.8917789957835,10.));
#26569=CARTESIAN_POINT('Ctrl Pts',(21.287448136198,91.9848818754176,10.));
#26570=CARTESIAN_POINT('Ctrl Pts',(21.2986734919875,92.0776667240288,10.));
#26571=CARTESIAN_POINT('Ctrl Pts',(21.3144940516725,92.1697443145829,10.));
#26572=CARTESIAN_POINT('Ctrl Pts',(21.330087444504,92.2604997662911,10.));
#26573=CARTESIAN_POINT('Ctrl Pts',(21.3501454854448,92.3505689686558,10.));
#26574=CARTESIAN_POINT('Ctrl Pts',(21.3746301441159,92.4395539722668,10.));
#26575=CARTESIAN_POINT('Ctrl Pts',(21.3838722153142,92.4731425858555,10.));
#26576=CARTESIAN_POINT('Ctrl Pts',(21.3937453933244,92.5065763996315,10.));
#26577=CARTESIAN_POINT('Ctrl Pts',(21.4042490564703,92.5398326835533,10.));
#26578=CARTESIAN_POINT('Ctrl Pts',(21.4119449767332,92.5641992027144,10.));
#26579=CARTESIAN_POINT('Ctrl Pts',(21.4199793784173,92.5884704022233,10.));
#26580=CARTESIAN_POINT('Ctrl Pts',(21.4283522639682,92.6126370452986,10.));
#26581=CARTESIAN_POINT('Ctrl Pts',(21.4335197893842,92.6275520637297,10.));
#26582=CARTESIAN_POINT('Ctrl Pts',(21.4388132538925,92.6424185688738,10.));
#26583=CARTESIAN_POINT('Ctrl Pts',(21.4442314703781,92.6572324707066,10.));
#26584=CARTESIAN_POINT('Ctrl Pts',(21.4759375175441,92.7439197176034,10.));
#26585=CARTESIAN_POINT('Ctrl Pts',(21.511920335298,92.8288327924596,10.));
#26586=CARTESIAN_POINT('Ctrl Pts',(21.552119621785,92.9115708703277,10.));
#26587=CARTESIAN_POINT('Ctrl Pts',(21.5822690866502,92.9736244287288,10.));
#26588=CARTESIAN_POINT('Ctrl Pts',(21.6147913043088,93.0344540664617,10.));
#26589=CARTESIAN_POINT('Ctrl Pts',(21.6496759248426,93.0938756896316,10.));
#26590=CARTESIAN_POINT('Ctrl Pts',(21.6654547887392,93.1207530266977,10.));
#26591=CARTESIAN_POINT('Ctrl Pts',(21.6817171403762,93.1473420998653,10.));
#26592=CARTESIAN_POINT('Ctrl Pts',(21.6984628023229,93.1736248041848,10.));
#26593=CARTESIAN_POINT('Ctrl Pts',(21.7075848153972,93.1879420150059,10.));
#26594=CARTESIAN_POINT('Ctrl Pts',(21.7168450674866,93.2021601541862,10.));
#26595=CARTESIAN_POINT('Ctrl Pts',(21.7262428789321,93.2162762091593,10.));
#26596=CARTESIAN_POINT('Ctrl Pts',(21.7738179410717,93.2877366972111,10.));
#26597=CARTESIAN_POINT('Ctrl Pts',(21.8249182080518,93.3565879238228,10.));
#26598=CARTESIAN_POINT('Ctrl Pts',(21.8795126224576,93.4224764000789,10.));
#26599=CARTESIAN_POINT('Ctrl Pts',(21.9256431150068,93.4781500050822,10.));
#26600=CARTESIAN_POINT('Ctrl Pts',(21.9742689995204,93.5317079390157,10.));
#26601=CARTESIAN_POINT('Ctrl Pts',(22.0253878321675,93.58291282293,10.));
#26602=CARTESIAN_POINT('Ctrl Pts',(22.0442196215672,93.6017763129624,10.));
#26603=CARTESIAN_POINT('Ctrl Pts',(22.0633898808657,93.6203202151646,10.));
#26604=CARTESIAN_POINT('Ctrl Pts',(22.0828884583321,93.6385402287508,10.));
#26605=CARTESIAN_POINT('Origin',(24.,92.,5.));
#26606=CARTESIAN_POINT('Origin',(92.,-24.,1.));
#26607=CARTESIAN_POINT('Ctrl Pts',(90.0865340033349,-22.3640127966251,1.));
#26608=CARTESIAN_POINT('Ctrl Pts',(90.0243936079936,-22.4224095095248,1.));
#26609=CARTESIAN_POINT('Ctrl Pts',(89.9656285062059,-22.4840599082556,1.));
#26610=CARTESIAN_POINT('Ctrl Pts',(89.9102507400287,-22.5485875658771,1.));
#26611=CARTESIAN_POINT('Ctrl Pts',(89.8535182657226,-22.6146937657251,1.));
#26612=CARTESIAN_POINT('Ctrl Pts',(89.8003404147793,-22.6838202104461,1.00000000000001));
#26613=CARTESIAN_POINT('Ctrl Pts',(89.7507590224199,-22.7556084412598,1.00000000000001));
#26614=CARTESIAN_POINT('Ctrl Pts',(89.7378150803961,-22.7743498007381,1.00000000000001));
#26615=CARTESIAN_POINT('Ctrl Pts',(89.7251164248241,-22.793272790225,1.));
#26616=CARTESIAN_POINT('Ctrl Pts',(89.7126641760334,-22.8123714654963,1.));
#26617=CARTESIAN_POINT('Ctrl Pts',(89.7025035055584,-22.8279554254061,1.));
#26618=CARTESIAN_POINT('Ctrl Pts',(89.6925064619188,-22.8436572534766,1.));
#26619=CARTESIAN_POINT('Ctrl Pts',(89.6826824797406,-22.8594591610939,1.));
#26620=CARTESIAN_POINT('Ctrl Pts',(89.6352350825432,-22.9357784554084,1.));
#26621=CARTESIAN_POINT('Ctrl Pts',(89.5917712590377,-23.0145049677974,1.00000000000001));
#26622=CARTESIAN_POINT('Ctrl Pts',(89.5523257642681,-23.09524621402,1.00000000000001));
#26623=CARTESIAN_POINT('Ctrl Pts',(89.5204848605231,-23.1604215721755,1.00000000000001));
#26624=CARTESIAN_POINT('Ctrl Pts',(89.4912627688458,-23.2269108039903,1.));
#26625=CARTESIAN_POINT('Ctrl Pts',(89.4646949471924,-23.2945252983029,1.));
#26626=CARTESIAN_POINT('Ctrl Pts',(89.453969916764,-23.3218202537706,1.00000000000001));
#26627=CARTESIAN_POINT('Ctrl Pts',(89.4436776173418,-23.3492987388173,1.));
#26628=CARTESIAN_POINT('Ctrl Pts',(89.4338211719337,-23.3769489123748,1.));
#26629=CARTESIAN_POINT('Ctrl Pts',(89.4286030055382,-23.3915873748747,1.));
#26630=CARTESIAN_POINT('Ctrl Pts',(89.4235075587072,-23.4062726291406,1.00000000000001));
#26631=CARTESIAN_POINT('Ctrl Pts',(89.41853905105,-23.4209911021932,1.00000000000001));
#26632=CARTESIAN_POINT('Ctrl Pts',(89.3890249549379,-23.5084222703165,1.00000000000001));
#26633=CARTESIAN_POINT('Ctrl Pts',(89.3639471428126,-23.5971333184058,1.));
#26634=CARTESIAN_POINT('Ctrl Pts',(89.3433383854818,-23.6867265557536,1.));
#26635=CARTESIAN_POINT('Ctrl Pts',(89.3224107214163,-23.7777061885211,1.));
#26636=CARTESIAN_POINT('Ctrl Pts',(89.3060909932886,-23.8695963304555,1.));
#26637=CARTESIAN_POINT('Ctrl Pts',(89.294455361361,-23.962013678881,1.));
#26638=CARTESIAN_POINT('Ctrl Pts',(89.282910896282,-24.0537069240991,1.));
#26639=CARTESIAN_POINT('Ctrl Pts',(89.275977070024,-24.1459200764499,1.));
#26640=CARTESIAN_POINT('Ctrl Pts',(89.2737752209874,-24.2382979315414,1.));
#26641=CARTESIAN_POINT('Ctrl Pts',(89.2726800380544,-24.2842459727554,1.));
#26642=CARTESIAN_POINT('Ctrl Pts',(89.272756305641,-24.330234973425,1.00000000000001));
#26643=CARTESIAN_POINT('Ctrl Pts',(89.2740237450201,-24.3762219172853,1.00000000000001));
#26644=CARTESIAN_POINT('Ctrl Pts',(89.2744405290818,-24.3913442383727,1.00000000000001));
#26645=CARTESIAN_POINT('Ctrl Pts',(89.2749862320744,-24.4064681891601,1.));
#26646=CARTESIAN_POINT('Ctrl Pts',(89.2756613705299,-24.4215864117119,1.));
#26647=CARTESIAN_POINT('Ctrl Pts',(89.2799353263961,-24.5172921376071,1.));
#26648=CARTESIAN_POINT('Ctrl Pts',(89.2893763302497,-24.6124306981363,1.00000000000001));
#26649=CARTESIAN_POINT('Ctrl Pts',(89.3040485582739,-24.7066037689229,1.00000000000001));
#26650=CARTESIAN_POINT('Ctrl Pts',(89.3082030634041,-24.73326928319,1.00000000000001));
#26651=CARTESIAN_POINT('Ctrl Pts',(89.3127772822415,-24.7598575178004,1.));
#26652=CARTESIAN_POINT('Ctrl Pts',(89.3177733858486,-24.7863596889658,1.));
#26653=CARTESIAN_POINT('Ctrl Pts',(89.3347382842714,-24.8763511457426,1.));
#26654=CARTESIAN_POINT('Ctrl Pts',(89.3565634809553,-24.9653501497165,1.));
#26655=CARTESIAN_POINT('Ctrl Pts',(89.3829463368407,-25.053124461385,1.));
#26656=CARTESIAN_POINT('Ctrl Pts',(89.4099256760068,-25.1428832401492,1.));
#26657=CARTESIAN_POINT('Ctrl Pts',(89.4416712994606,-25.2313620234223,1.));
#26658=CARTESIAN_POINT('Ctrl Pts',(89.477913814938,-25.318308752927,1.));
#26659=CARTESIAN_POINT('Ctrl Pts',(89.4905805865942,-25.348696664869,1.));
#26660=CARTESIAN_POINT('Ctrl Pts',(89.5037971164698,-25.3788973526874,1.));
#26661=CARTESIAN_POINT('Ctrl Pts',(89.5175533368002,-25.4088996997776,1.));
#26662=CARTESIAN_POINT('Ctrl Pts',(89.5245000449555,-25.4240504856912,1.));
#26663=CARTESIAN_POINT('Ctrl Pts',(89.5315843916574,-25.4391506886467,1.));
#26664=CARTESIAN_POINT('Ctrl Pts',(89.5388051477195,-25.4541988513475,1.));
#26665=CARTESIAN_POINT('Ctrl Pts',(89.5448146544974,-25.46672275258,1.));
#26666=CARTESIAN_POINT('Ctrl Pts',(89.5509168026676,-25.4792066766568,1.));
#26667=CARTESIAN_POINT('Ctrl Pts',(89.5571069929132,-25.4916425965977,1.));
#26668=CARTESIAN_POINT('Ctrl Pts',(89.6000701103193,-25.5779543038758,1.));
#26669=CARTESIAN_POINT('Ctrl Pts',(89.6473202761524,-25.6620593555128,1.));
#26670=CARTESIAN_POINT('Ctrl Pts',(89.6985154201672,-25.7437076710158,1.));
#26671=CARTESIAN_POINT('Ctrl Pts',(89.7507153893452,-25.8269585268285,1.));
#26672=CARTESIAN_POINT('Ctrl Pts',(89.8070170326452,-25.9076560356431,1.));
#26673=CARTESIAN_POINT('Ctrl Pts',(89.8671126570608,-25.9855277789599,1.));
#26674=CARTESIAN_POINT('Ctrl Pts',(89.927676334208,-26.0640060237073,1.));
#26675=CARTESIAN_POINT('Ctrl Pts',(89.9920937838692,-26.1396151519006,1.));
#26676=CARTESIAN_POINT('Ctrl Pts',(90.0600992171408,-26.2120567437867,1.));
#26677=CARTESIAN_POINT('Ctrl Pts',(90.0970259686533,-26.2513923164617,1.));
#26678=CARTESIAN_POINT('Ctrl Pts',(90.1350114303598,-26.2897935420312,1.));
#26679=CARTESIAN_POINT('Ctrl Pts',(90.1740182898104,-26.3272088864004,1.));
#26680=CARTESIAN_POINT('Ctrl Pts',(90.1861457891855,-26.3388415728522,1.));
#26681=CARTESIAN_POINT('Ctrl Pts',(90.1983720446101,-26.3503789382668,1.));
#26682=CARTESIAN_POINT('Ctrl Pts',(90.2106959994552,-26.3618193692872,1.));
#26683=CARTESIAN_POINT('Ctrl Pts',(90.2219869755512,-26.3723008774397,1.));
#26684=CARTESIAN_POINT('Ctrl Pts',(90.2333542353844,-26.3826956655534,1.));
#26685=CARTESIAN_POINT('Ctrl Pts',(90.2447923276116,-26.3929988640505,1.));
#26686=CARTESIAN_POINT('Ctrl Pts',(90.3206014106021,-26.4612861286066,1.));
#26687=CARTESIAN_POINT('Ctrl Pts',(90.3995767828363,-26.5256063737863,0.999999999999999));
#26688=CARTESIAN_POINT('Ctrl Pts',(90.4813922770108,-26.5856769718563,0.999999999999999));
#26689=CARTESIAN_POINT('Ctrl Pts',(90.5632787218729,-26.6457996633627,1.));
#26690=CARTESIAN_POINT('Ctrl Pts',(90.6480107936052,-26.701666171117,1.));
#26691=CARTESIAN_POINT('Ctrl Pts',(90.7353064390064,-26.7529669283143,1.));
#26692=CARTESIAN_POINT('Ctrl Pts',(90.8208383089426,-26.803231173135,1.));
#26693=CARTESIAN_POINT('Ctrl Pts',(90.9088318713758,-26.8491129760809,1.));
#26694=CARTESIAN_POINT('Ctrl Pts',(90.9990555762685,-26.8902850239778,1.));
#26695=CARTESIAN_POINT('Ctrl Pts',(91.0368458850231,-26.9075299864179,1.));
#26696=CARTESIAN_POINT('Ctrl Pts',(91.0750277978247,-26.9239481874698,1.));
#26697=CARTESIAN_POINT('Ctrl Pts',(91.1135856932338,-26.9395132002532,1.));
#26698=CARTESIAN_POINT('Ctrl Pts',(91.1435994051254,-26.9516291055512,1.));
#26699=CARTESIAN_POINT('Ctrl Pts',(91.1738409492154,-26.9632280171349,1.));
#26700=CARTESIAN_POINT('Ctrl Pts',(91.2042985533737,-26.9743125149969,1.));
#26701=CARTESIAN_POINT('Ctrl Pts',(92.7937992825329,-26.9692229537457,1.));
#26702=CARTESIAN_POINT('Ctrl Pts',(92.8886355742527,-26.9345314146036,1.));
#26703=CARTESIAN_POINT('Ctrl Pts',(92.9814286349373,-26.8948494551323,0.999999999999998));
#26704=CARTESIAN_POINT('Ctrl Pts',(93.0719375317565,-26.8504973230386,0.999999999999999));
#26705=CARTESIAN_POINT('Ctrl Pts',(93.1637179471412,-26.8055221078961,1.));
#26706=CARTESIAN_POINT('Ctrl Pts',(93.253150237892,-26.7557438784191,1.));
#26707=CARTESIAN_POINT('Ctrl Pts',(93.3399491478414,-26.701455889429,1.));
#26708=CARTESIAN_POINT('Ctrl Pts',(93.3644578975098,-26.6861270018551,1.));
#26709=CARTESIAN_POINT('Ctrl Pts',(93.38875645171,-26.6704383481465,0.999999999999999));
#26710=CARTESIAN_POINT('Ctrl Pts',(93.4128377927018,-26.6543960746865,0.999999999999999));
#26711=CARTESIAN_POINT('Ctrl Pts',(93.4321685183665,-26.6415185199275,0.999999999999999));
#26712=CARTESIAN_POINT('Ctrl Pts',(93.4513613836409,-26.62841147677,1.));
#26713=CARTESIAN_POINT('Ctrl Pts',(93.4703934697505,-26.6150918905377,1.));
#26714=CARTESIAN_POINT('Ctrl Pts',(93.5531011008219,-26.5572090385068,0.999999999999999));
#26715=CARTESIAN_POINT('Ctrl Pts',(93.6328538966534,-26.4952643978376,0.999999999999999));
#26716=CARTESIAN_POINT('Ctrl Pts',(93.7093855017744,-26.4295552066869,1.));
#26717=CARTESIAN_POINT('Ctrl Pts',(93.7683983463317,-26.3788874299269,1.));
#26718=CARTESIAN_POINT('Ctrl Pts',(93.8254952956778,-26.3259804095853,1.));
#26719=CARTESIAN_POINT('Ctrl Pts',(93.8805366455773,-26.2709586400739,1.));
#26720=CARTESIAN_POINT('Ctrl Pts',(93.9098567587088,-26.2416489572678,1.));
#26721=CARTESIAN_POINT('Ctrl Pts',(93.9385932953215,-26.2117390413757,1.));
#26722=CARTESIAN_POINT('Ctrl Pts',(93.9667231085696,-26.1812468762253,1.));
#26723=CARTESIAN_POINT('Ctrl Pts',(93.976357091693,-26.1708038277108,1.));
#26724=CARTESIAN_POINT('Ctrl Pts',(93.9859191102224,-26.1602932647167,0.999999999999999));
#26725=CARTESIAN_POINT('Ctrl Pts',(93.9954016773941,-26.1497234378417,0.999999999999999));
#26726=CARTESIAN_POINT('Ctrl Pts',(94.0611941644384,-26.0763872636661,0.999999999999999));
#26727=CARTESIAN_POINT('Ctrl Pts',(94.1232544016247,-26.0001047407494,1.));
#26728=CARTESIAN_POINT('Ctrl Pts',(94.1813385979309,-25.9211542884475,1.));
#26729=CARTESIAN_POINT('Ctrl Pts',(94.2389163888163,-25.8428921634285,1.));
#26730=CARTESIAN_POINT('Ctrl Pts',(94.2925876036441,-25.7620076427722,1.));
#26731=CARTESIAN_POINT('Ctrl Pts',(94.3420689680264,-25.6787495218591,1.));
#26732=CARTESIAN_POINT('Ctrl Pts',(94.3901173496858,-25.5979025601834,0.999999999999999));
#26733=CARTESIAN_POINT('Ctrl Pts',(94.4342152487962,-25.5148167869307,1.));
#26734=CARTESIAN_POINT('Ctrl Pts',(94.4740555016775,-25.4297096831016,1.));
#26735=CARTESIAN_POINT('Ctrl Pts',(94.4948667673004,-25.3852524717113,1.));
#26736=CARTESIAN_POINT('Ctrl Pts',(94.5145154383506,-25.3402435941338,1.));
#26737=CARTESIAN_POINT('Ctrl Pts',(94.5329520278252,-25.2947138138489,1.));
#26738=CARTESIAN_POINT('Ctrl Pts',(94.5400926945258,-25.2770796963019,1.));
#26739=CARTESIAN_POINT('Ctrl Pts',(94.5470514948584,-25.2593674400535,1.));
#26740=CARTESIAN_POINT('Ctrl Pts',(94.5538253850611,-25.2415788415781,1.));
#26741=CARTESIAN_POINT('Ctrl Pts',(94.5589792730445,-25.2280444556963,1.));
#26742=CARTESIAN_POINT('Ctrl Pts',(94.5640260783963,-25.2144657562887,0.999999999999999));
#26743=CARTESIAN_POINT('Ctrl Pts',(94.5689596301442,-25.2008574386567,0.999999999999999));
#26744=CARTESIAN_POINT('Ctrl Pts',(94.6006314836872,-25.1134963112103,0.999999999999999));
#26745=CARTESIAN_POINT('Ctrl Pts',(94.6276946264954,-25.0247742561595,0.999999999999998));
#26746=CARTESIAN_POINT('Ctrl Pts',(94.6498977731061,-24.9349146809329,0.999999999999998));
#26747=CARTESIAN_POINT('Ctrl Pts',(94.6549003686514,-24.914668401493,0.999999999999998));
#26748=CARTESIAN_POINT('Ctrl Pts',(94.6596560431607,-24.894364336279,1.));
#26749=CARTESIAN_POINT('Ctrl Pts',(94.6641615567933,-24.8740049843512,1.));
#26750=CARTESIAN_POINT('Ctrl Pts',(94.684507085955,-24.7820683435733,1.));
#26751=CARTESIAN_POINT('Ctrl Pts',(94.6997556148072,-24.6890040031268,1.));
#26752=CARTESIAN_POINT('Ctrl Pts',(94.7100170529218,-24.5952037047372,1.));
#26753=CARTESIAN_POINT('Ctrl Pts',(94.7207301965731,-24.4972743443535,1.));
#26754=CARTESIAN_POINT('Ctrl Pts',(94.7260075138323,-24.3985415672063,0.999999999999998));
#26755=CARTESIAN_POINT('Ctrl Pts',(94.7259165861328,-24.299465853035,0.999999999999998));
#26756=CARTESIAN_POINT('Ctrl Pts',(94.7258814692624,-24.2612021661271,0.999999999999998));
#26757=CARTESIAN_POINT('Ctrl Pts',(94.7250450624305,-24.2228875809902,0.999999999999998));
#26758=CARTESIAN_POINT('Ctrl Pts',(94.7234091242725,-24.1845498020178,0.999999999999997));
#26759=CARTESIAN_POINT('Ctrl Pts',(94.7228215216315,-24.1707794892095,0.999999999999997));
#26760=CARTESIAN_POINT('Ctrl Pts',(94.7221307767868,-24.1570079821605,1.));
#26761=CARTESIAN_POINT('Ctrl Pts',(94.7213378612436,-24.1432482331353,1.));
#26762=CARTESIAN_POINT('Ctrl Pts',(94.7159862604884,-24.0503799776195,1.));
#26763=CARTESIAN_POINT('Ctrl Pts',(94.7059789500127,-23.9578988174462,0.999999999999996));
#26764=CARTESIAN_POINT('Ctrl Pts',(94.6914389868646,-23.8661766503703,0.999999999999997));
#26765=CARTESIAN_POINT('Ctrl Pts',(94.6769360712931,-23.7746881898014,0.999999999999998));
#26766=CARTESIAN_POINT('Ctrl Pts',(94.6579231604244,-23.6839539151715,1.));
#26767=CARTESIAN_POINT('Ctrl Pts',(94.6344737838795,-23.5943600003469,1.));
#26768=CARTESIAN_POINT('Ctrl Pts',(94.6114257043808,-23.5062993362386,0.999999999999998));
#26769=CARTESIAN_POINT('Ctrl Pts',(94.5840912373833,-23.4193395518976,1.));
#26770=CARTESIAN_POINT('Ctrl Pts',(94.5524998666925,-23.3338765545241,1.));
#26771=CARTESIAN_POINT('Ctrl Pts',(94.5366373923581,-23.2909643739907,1.));
#26772=CARTESIAN_POINT('Ctrl Pts',(94.5197010774786,-23.2484300968532,1.));
#26773=CARTESIAN_POINT('Ctrl Pts',(94.5016912657434,-23.206327621631,1.));
#26774=CARTESIAN_POINT('Ctrl Pts',(94.4963919504663,-23.1939391362082,1.));
#26775=CARTESIAN_POINT('Ctrl Pts',(94.4909996770287,-23.1815880553872,1.));
#26776=CARTESIAN_POINT('Ctrl Pts',(94.485514419704,-23.1692758010802,1.));
#26777=CARTESIAN_POINT('Ctrl Pts',(94.4799210007597,-23.1567207663004,1.));
#26778=CARTESIAN_POINT('Ctrl Pts',(94.4742345748605,-23.1442143929032,1.));
#26779=CARTESIAN_POINT('Ctrl Pts',(94.4684564310145,-23.1317600158838,1.));
#26780=CARTESIAN_POINT('Ctrl Pts',(94.4309710580974,-23.0509629676511,1.));
#26781=CARTESIAN_POINT('Ctrl Pts',(94.3896159815805,-22.9723227780457,1.));
#26782=CARTESIAN_POINT('Ctrl Pts',(94.3444610246362,-22.8961871515012,0.999999999999999));
#26783=CARTESIAN_POINT('Ctrl Pts',(94.3000642491435,-22.8213298922449,0.999999999999999));
#26784=CARTESIAN_POINT('Ctrl Pts',(94.2519936725177,-22.7488931261332,1.));
#26785=CARTESIAN_POINT('Ctrl Pts',(94.2002794589025,-22.6792415177607,1.));
#26786=CARTESIAN_POINT('Ctrl Pts',(94.1501451854236,-22.61171786153,1.));
#26787=CARTESIAN_POINT('Ctrl Pts',(94.0965860671228,-22.5468113410791,0.999999999999999));
#26788=CARTESIAN_POINT('Ctrl Pts',(94.0396018953678,-22.4848944920469,0.999999999999999));
#26789=CARTESIAN_POINT('Ctrl Pts',(94.0184128484534,-22.4618712738701,0.999999999999999));
#26790=CARTESIAN_POINT('Ctrl Pts',(93.9967499855334,-22.439261866594,0.999999999999998));
#26791=CARTESIAN_POINT('Ctrl Pts',(93.9746124571306,-22.4170870902725,0.999999999999998));
#26792=CARTESIAN_POINT('Ctrl Pts',(93.9557856680546,-22.3982286238251,0.999999999999998));
#26793=CARTESIAN_POINT('Ctrl Pts',(93.9366155517544,-22.3796845329471,0.999999999999999));
#26794=CARTESIAN_POINT('Ctrl Pts',(93.9171118396844,-22.3614597340103,0.999999999999999));
#26795=CARTESIAN_POINT('Origin',(92.,-24.,12.2084234471775));
#26796=CARTESIAN_POINT('Ctrl Pts',(88.9232328435277,-23.9980626432726,9.70842344717746));
#26797=CARTESIAN_POINT('Ctrl Pts',(88.9222986726779,-23.8738980500463,9.70197366100994));
#26798=CARTESIAN_POINT('Ctrl Pts',(88.9853330132547,-22.7368858898031,9.64286281975954));
#26799=CARTESIAN_POINT('Ctrl Pts',(90.4009680446667,-20.744487174453,9.53109092342626));
#26800=CARTESIAN_POINT('Ctrl Pts',(93.8523951731074,-20.8820464105141,9.37310775817762));
#26801=CARTESIAN_POINT('Ctrl Pts',(95.6235721938174,-23.847285073477,9.215124592929));
#26802=CARTESIAN_POINT('Ctrl Pts',(94.1080771138749,-26.9512425629647,9.05714142768035));
#26803=CARTESIAN_POINT('Ctrl Pts',(90.680468686986,-27.3782238204297,8.89915826243172));
#26804=CARTESIAN_POINT('Ctrl Pts',(89.0391556852518,-25.4378982357328,8.78291893559742));
#26805=CARTESIAN_POINT('Ctrl Pts',(88.9237203439564,-24.2133137839327,8.719340663846));
#26806=CARTESIAN_POINT('Ctrl Pts',(88.925632185667,-24.0026790855389,8.70842344717745));
#26807=CARTESIAN_POINT('Ctrl Pts',(88.9297109890477,-24.0031050978172,9.79157655282255));
#26808=CARTESIAN_POINT('Ctrl Pts',(88.9347146650535,-23.3096207752369,9.75572892504928));
#26809=CARTESIAN_POINT('Ctrl Pts',(89.5077566649198,-21.5876413967006,9.66722024219312));
#26810=CARTESIAN_POINT('Ctrl Pts',(92.3539160472627,-20.3911616367203,9.52605050425409));
#26811=CARTESIAN_POINT('Ctrl Pts',(95.215603926767,-22.3229247027849,9.36806733900546));
#26812=CARTESIAN_POINT('Ctrl Pts',(95.1618223030446,-25.7771165220753,9.21008417375683));
#26813=CARTESIAN_POINT('Ctrl Pts',(92.2395757220273,-27.6187839878381,9.0521010085082));
#26814=CARTESIAN_POINT('Ctrl Pts',(89.4675381047452,-26.3468885879089,8.91259846819676));
#26815=CARTESIAN_POINT('Ctrl Pts',(88.9339207778366,-24.6595175431003,8.82575698296822));
#26816=CARTESIAN_POINT('Ctrl Pts',(88.9296146841086,-23.99786424691,8.79157655282255));
#26817=CARTESIAN_POINT('Ctrl Pts',(93.9134659966651,-22.3640127966251,10.));
#26818=CARTESIAN_POINT('Ctrl Pts',(94.4547800806522,-22.9971388327508,9.94733894491712));
#26819=CARTESIAN_POINT('Ctrl Pts',(94.8501256748086,-24.8326016501471,9.84201683475137));
#26820=CARTESIAN_POINT('Ctrl Pts',(92.8579877031057,-26.8458064948082,9.68403366950272));
#26821=CARTESIAN_POINT('Ctrl Pts',(90.0866997272543,-26.2718360144009,9.5260505042541));
#26822=CARTESIAN_POINT('Ctrl Pts',(89.0512847401284,-23.6401113487857,9.36806733900546));
#26823=CARTESIAN_POINT('Ctrl Pts',(90.6902349284037,-21.3334135225917,9.21008417375683));
#26824=CARTESIAN_POINT('Ctrl Pts',(93.5172945659013,-21.4460881205366,9.05210100850819));
#26825=CARTESIAN_POINT('Ctrl Pts',(94.9680634449115,-23.8749113949824,8.89411784325956));
#26826=CARTESIAN_POINT('Ctrl Pts',(93.7267233233056,-26.4173590864694,8.73613467801093));
#26827=CARTESIAN_POINT('Ctrl Pts',(90.9191735544127,-26.7670988996036,8.57815151276228));
#26828=CARTESIAN_POINT('Ctrl Pts',(89.0919764590838,-24.6070250632274,8.42016834751366));
#26829=CARTESIAN_POINT('Ctrl Pts',(89.9024529386512,-21.8963394365791,8.26218518226502));
#26830=CARTESIAN_POINT('Ctrl Pts',(92.6154776819786,-21.0937552116683,8.10420201701638));
#26831=CARTESIAN_POINT('Ctrl Pts',(94.7702424329595,-22.9272295704909,7.94621885176776));
#26832=CARTESIAN_POINT('Ctrl Pts',(94.4123030989785,-25.7337455944376,7.78823568651911));
#26833=CARTESIAN_POINT('Ctrl Pts',(91.8663223428291,-26.9676940765812,7.63025252127049));
#26834=CARTESIAN_POINT('Ctrl Pts',(89.441591869785,-25.509843281544,7.47226935602184));
#26835=CARTESIAN_POINT('Ctrl Pts',(89.3374248530143,-22.6825128295981,7.31428619077321));
#26836=CARTESIAN_POINT('Ctrl Pts',(91.648304394415,-21.0501883402777,7.15630302552458));
#26837=CARTESIAN_POINT('Ctrl Pts',(94.2781838441901,-22.0934436458725,6.99831986027595));
#26838=CARTESIAN_POINT('Ctrl Pts',(94.8416727928904,-24.8660106707762,6.84033669502731));
#26839=CARTESIAN_POINT('Ctrl Pts',(92.8276675236541,-26.8530764431805,6.68235352977868));
#26840=CARTESIAN_POINT('Ctrl Pts',(90.0629395615723,-26.2523045074983,6.52437036453004));
#26841=CARTESIAN_POINT('Ctrl Pts',(89.055191532594,-23.6086155038654,6.36638719928141));
#26842=CARTESIAN_POINT('Ctrl Pts',(90.7184852964603,-21.3199255988147,6.20840403403277));
#26843=CARTESIAN_POINT('Ctrl Pts',(93.5441566371434,-21.4621546514439,6.05042086878414));
#26844=CARTESIAN_POINT('Ctrl Pts',(94.9692252026282,-23.9062960577466,5.89243770353551));
#26845=CARTESIAN_POINT('Ctrl Pts',(93.7011051632761,-26.4354301377776,5.73445453828687));
#26846=CARTESIAN_POINT('Ctrl Pts',(90.8900246784809,-26.7555459564984,5.57647137303824));
#26847=CARTESIAN_POINT('Ctrl Pts',(89.0857296961368,-24.5762875399298,5.4184882077896));
#26848=CARTESIAN_POINT('Ctrl Pts',(89.9247773496848,-21.8743166547494,5.26050504254097));
#26849=CARTESIAN_POINT('Ctrl Pts',(92.6461227788815,-21.1004131178103,5.10252187729233));
#26850=CARTESIAN_POINT('Ctrl Pts',(94.781412794043,-22.9565338521763,4.9445387120437));
#26851=CARTESIAN_POINT('Ctrl Pts',(94.3938664694978,-25.7591139982761,4.78655554679506));
#26852=CARTESIAN_POINT('Ctrl Pts',(91.8350015491773,-26.9661177057641,4.62857238154643));
#26853=CARTESIAN_POINT('Ctrl Pts',(89.4257958558034,-25.4827514138513,4.4705892162978));
#26854=CARTESIAN_POINT('Ctrl Pts',(89.3514811837096,-22.6544789807379,4.31260605104916));
#26855=CARTESIAN_POINT('Ctrl Pts',(91.6794634788654,-21.0466400362912,4.15462288580053));
#26856=CARTESIAN_POINT('Ctrl Pts',(94.2981833367367,-22.1175993861324,3.99663972055189));
#26857=CARTESIAN_POINT('Ctrl Pts',(94.832372471477,-24.8959603376103,3.83865655530326));
#26858=CARTESIAN_POINT('Ctrl Pts',(92.7975030889959,-26.8616546930814,3.68067339005462));
#26859=CARTESIAN_POINT('Ctrl Pts',(90.0392712060535,-26.2317305445351,3.52269022480599));
#26860=CARTESIAN_POINT('Ctrl Pts',(89.059487218677,-23.5775506652917,3.36470705955735));
#26861=CARTESIAN_POINT('Ctrl Pts',(90.7468487806939,-21.3065466558477,3.20672389430872));
#26862=CARTESIAN_POINT('Ctrl Pts',(93.570861086046,-21.4785969587254,3.04874072906008));
#26863=CARTESIAN_POINT('Ctrl Pts',(94.9700491479981,-23.9376454809303,2.89075756381145));
#26864=CARTESIAN_POINT('Ctrl Pts',(93.6753004854887,-26.4532524972207,2.73277439856281));
#26865=CARTESIAN_POINT('Ctrl Pts',(90.86099868006,-26.7436740950583,2.57479123331418));
#26866=CARTESIAN_POINT('Ctrl Pts',(89.0798067232475,-24.545493049519,2.41680806806554));
#26867=CARTESIAN_POINT('Ctrl Pts',(89.9473363281977,-21.8525242277567,2.25882490281691));
#26868=CARTESIAN_POINT('Ctrl Pts',(92.6766884907985,-21.1074034480955,2.10084173756828));
#26869=CARTESIAN_POINT('Ctrl Pts',(94.7922885760843,-22.9859374299123,1.94285857231964));
#26870=CARTESIAN_POINT('Ctrl Pts',(94.3751314870431,-25.7843200921868,1.78487540707101));
#26871=CARTESIAN_POINT('Ctrl Pts',(91.8037637139842,-26.96414237307,1.62689224182237));
#26872=CARTESIAN_POINT('Ctrl Pts',(89.4101547923377,-25.4556338085585,1.46890907657374));
#26873=CARTESIAN_POINT('Ctrl Pts',(89.3661021422764,-22.6263102241946,1.3109259113251));
#26874=CARTESIAN_POINT('Ctrl Pts',(91.7101077338689,-21.0440028274616,1.15294274607647));
#26875=CARTESIAN_POINT('Ctrl Pts',(94.3190522551594,-22.14076517287,0.994959580827836));
#26876=CARTESIAN_POINT('Ctrl Pts',(94.8204142519502,-24.9282808397392,0.836976415579201));
#26877=CARTESIAN_POINT('Ctrl Pts',(93.4549268544596,-26.2169491679593,0.731654305413445));
#26878=CARTESIAN_POINT('Ctrl Pts',(92.6501999979751,-26.4320868020351,0.678993250330566));
#26879=CARTESIAN_POINT('Ctrl Pts',(94.0543315503421,-22.2435746787732,10.1070022498898));
#26880=CARTESIAN_POINT('Ctrl Pts',(94.6354960985062,-22.9233101920371,10.0543411948069));
#26881=CARTESIAN_POINT('Ctrl Pts',(95.0599462474923,-24.8938961244909,9.94901908464118));
#26882=CARTESIAN_POINT('Ctrl Pts',(92.9211510480811,-27.0553090980672,9.79103591939255));
#26883=CARTESIAN_POINT('Ctrl Pts',(89.9458463738419,-26.4390840546533,9.6330527541439));
#26884=CARTESIAN_POINT('Ctrl Pts',(88.8342061986536,-23.6136170634398,9.47506958889528));
#26885=CARTESIAN_POINT('Ctrl Pts',(90.5938126338247,-21.1371047398788,9.31708642364664));
#26886=CARTESIAN_POINT('Ctrl Pts',(93.6289947683033,-21.2580742171958,9.159103258398));
#26887=CARTESIAN_POINT('Ctrl Pts',(95.1865663612134,-23.8657026211472,9.00112009314937));
#26888=CARTESIAN_POINT('Ctrl Pts',(93.8538412534954,-26.5953202453012,8.84313692790073));
#26889=CARTESIAN_POINT('Ctrl Pts',(90.8396052652705,-26.9708072065457,8.6851537626521));
#26890=CARTESIAN_POINT('Ctrl Pts',(88.8778935608714,-24.6517130387526,8.52717059740347));
#26891=CARTESIAN_POINT('Ctrl Pts',(89.7480357038138,-21.7414721379016,8.36918743215483));
#26892=CARTESIAN_POINT('Ctrl Pts',(92.6607879224527,-20.8798032616766,8.21120426690619));
#26893=CARTESIAN_POINT('Ctrl Pts',(94.9741821605629,-22.848254349199,8.05322110165757));
#26894=CARTESIAN_POINT('Ctrl Pts',(94.5898920460865,-25.8613804902347,7.89523793640892));
#26895=CARTESIAN_POINT('Ctrl Pts',(91.85648126009,-27.1861698007228,7.7372547711603));
#26896=CARTESIAN_POINT('Ctrl Pts',(89.2532469614236,-25.6209949352399,7.57927160591165));
#26897=CARTESIAN_POINT('Ctrl Pts',(89.1414113764536,-22.5855220494931,7.42128844066304));
#26898=CARTESIAN_POINT('Ctrl Pts',(91.6224132647619,-20.8330290840307,7.26330527541438));
#26899=CARTESIAN_POINT('Ctrl Pts',(94.4458991990223,-21.9530867663101,7.10532211016576));
#26900=CARTESIAN_POINT('Ctrl Pts',(95.0508710812514,-24.929764650644,6.94733894491712));
#26901=CARTESIAN_POINT('Ctrl Pts',(92.8885987574378,-27.0631142455517,6.78935577966849));
#26902=CARTESIAN_POINT('Ctrl Pts',(89.9203370321098,-26.4181146771334,6.63137261441986));
#26903=CARTESIAN_POINT('Ctrl Pts',(88.8384006013953,-23.5798025571787,6.47338944917122));
#26904=CARTESIAN_POINT('Ctrl Pts',(90.6241427376827,-21.122623862031,6.31540628392259));
#26905=CARTESIAN_POINT('Ctrl Pts',(93.6578343717016,-21.2753235340925,6.15742311867394));
#26906=CARTESIAN_POINT('Ctrl Pts',(95.1878136452183,-23.8993977602433,5.99943995342532));
#26907=CARTESIAN_POINT('Ctrl Pts',(93.8263371355742,-26.6147216513962,5.84145678817668));
#26908=CARTESIAN_POINT('Ctrl Pts',(90.8083105071782,-26.9584037587908,5.68347362292805));
#26909=CARTESIAN_POINT('Ctrl Pts',(88.8711869236842,-24.6187126802411,5.52549045767941));
#26910=CARTESIAN_POINT('Ctrl Pts',(89.7720035935014,-21.7178280827588,5.36750729243077));
#26911=CARTESIAN_POINT('Ctrl Pts',(92.6936890503225,-20.8869513096014,5.20952412718214));
#26912=CARTESIAN_POINT('Ctrl Pts',(94.9861748613701,-22.8797159537069,5.05154096193351));
#26913=CARTESIAN_POINT('Ctrl Pts',(94.5700981486823,-25.8886164654117,4.89355779668487));
#26914=CARTESIAN_POINT('Ctrl Pts',(91.8228546920231,-27.1844773806274,4.73557463143624));
#26915=CARTESIAN_POINT('Ctrl Pts',(89.2362880763697,-25.5919086182341,4.5775914661876));
#26916=CARTESIAN_POINT('Ctrl Pts',(89.1565025062044,-22.5554244045433,4.41960830093897));
#26917=CARTESIAN_POINT('Ctrl Pts',(91.6558662189183,-20.8292195609755,4.26162513569033));
#26918=CARTESIAN_POINT('Ctrl Pts',(94.4673710143567,-21.9790208040324,4.1036419704417));
#26919=CARTESIAN_POINT('Ctrl Pts',(95.0408860887087,-24.9619191522692,3.94565880519306));
#26920=CARTESIAN_POINT('Ctrl Pts',(92.8562136772091,-27.0723240091163,3.78767563994443));
#26921=CARTESIAN_POINT('Ctrl Pts',(89.8949262594222,-26.3960261000149,3.6296924746958));
#26922=CARTESIAN_POINT('Ctrl Pts',(88.8430125273276,-23.5464507870927,3.47170930944716));
#26923=CARTESIAN_POINT('Ctrl Pts',(90.6545942851052,-21.1082599879431,3.31372614419853));
#26924=CARTESIAN_POINT('Ctrl Pts',(93.6865047489179,-21.2929762912711,3.1557429789499));
#26925=CARTESIAN_POINT('Ctrl Pts',(95.1886982478045,-23.9330550654913,2.99775981370126));
#26926=CARTESIAN_POINT('Ctrl Pts',(93.7986327688294,-26.6338560574266,2.83977664845263));
#26927=CARTESIAN_POINT('Ctrl Pts',(90.7771476725941,-26.9456579145687,2.68179348320399));
#26928=CARTESIAN_POINT('Ctrl Pts',(88.8648279133335,-24.585651160811,2.52381031795536));
#26929=CARTESIAN_POINT('Ctrl Pts',(89.7962233190588,-21.694431340717,2.36582715270672));
#26930=CARTESIAN_POINT('Ctrl Pts',(92.7265049490419,-20.8944562540725,2.20784398745809));
#26931=CARTESIAN_POINT('Ctrl Pts',(94.9978512968129,-22.9112841642428,2.04986082220945));
#26932=CARTESIAN_POINT('Ctrl Pts',(94.5499839341528,-25.9156781817275,1.89187765696082));
#26933=CARTESIAN_POINT('Ctrl Pts',(91.7893171896512,-27.1823566278765,1.73389449171218));
#26934=CARTESIAN_POINT('Ctrl Pts',(89.2194955489798,-25.5627946688775,1.57591132646355));
#26935=CARTESIAN_POINT('Ctrl Pts',(89.1721998306056,-22.5251819202756,1.41792816121491));
#26936=CARTESIAN_POINT('Ctrl Pts',(91.6887664429098,-20.8263882060871,1.25994499596628));
#26937=CARTESIAN_POINT('Ctrl Pts',(94.4897762609678,-22.0038920098267,1.10196183071765));
#26938=CARTESIAN_POINT('Ctrl Pts',(95.0280475288895,-24.9966190253592,0.943978665469011));
#26939=CARTESIAN_POINT('Ctrl Pts',(93.5620356702265,-26.3801565479508,0.838656555303256));
#26940=CARTESIAN_POINT('Ctrl Pts',(92.698066426161,-26.6111321859386,0.785995500220377));
#26941=CARTESIAN_POINT('Ctrl Pts',(94.1951971040191,-22.1231365609213,10.2140044997796));
#26942=CARTESIAN_POINT('Ctrl Pts',(94.8162121163602,-22.8494815513233,10.1613434446967));
#26943=CARTESIAN_POINT('Ctrl Pts',(95.269766820176,-24.9551905988348,10.056021334531));
#26944=CARTESIAN_POINT('Ctrl Pts',(92.9843143930565,-27.2648117013262,9.89803816928236));
#26945=CARTESIAN_POINT('Ctrl Pts',(89.8049930204297,-26.6063320949058,9.74005500403372));
#26946=CARTESIAN_POINT('Ctrl Pts',(88.6171276571787,-23.5871227780939,9.58207183878508));
#26947=CARTESIAN_POINT('Ctrl Pts',(90.4973903392457,-20.9407959571659,9.42408867353645));
#26948=CARTESIAN_POINT('Ctrl Pts',(93.7406949707054,-21.070060313855,9.26610550828781));
#26949=CARTESIAN_POINT('Ctrl Pts',(95.4050692775153,-23.8564938473121,9.10812234303918));
#26950=CARTESIAN_POINT('Ctrl Pts',(93.9809591836852,-26.7732814041329,8.95013917779054));
#26951=CARTESIAN_POINT('Ctrl Pts',(90.7600369761282,-27.1745155134877,8.79215601254191));
#26952=CARTESIAN_POINT('Ctrl Pts',(88.663810662659,-24.6964010142779,8.63417284729327));
#26953=CARTESIAN_POINT('Ctrl Pts',(89.5936184689763,-21.5866048392241,8.47618968204464));
#26954=CARTESIAN_POINT('Ctrl Pts',(92.7060981629268,-20.6658513116849,8.31820651679601));
#26955=CARTESIAN_POINT('Ctrl Pts',(95.1781218881664,-22.7692791279071,8.16022335154737));
#26956=CARTESIAN_POINT('Ctrl Pts',(94.7674809931943,-25.9890153860317,8.00224018629874));
#26957=CARTESIAN_POINT('Ctrl Pts',(91.8466401773509,-27.4046455248644,7.84425702105011));
#26958=CARTESIAN_POINT('Ctrl Pts',(89.0649020530621,-25.7321465889358,7.68627385580147));
#26959=CARTESIAN_POINT('Ctrl Pts',(88.9453978998932,-22.488531269388,7.52829069055284));
#26960=CARTESIAN_POINT('Ctrl Pts',(91.5965221351087,-20.6158698277837,7.37030752530419));
#26961=CARTESIAN_POINT('Ctrl Pts',(94.6136145538545,-21.8127298867477,7.21232436005558));
#26962=CARTESIAN_POINT('Ctrl Pts',(95.2600693696124,-24.9935186305119,7.05434119480693));
#26963=CARTESIAN_POINT('Ctrl Pts',(92.9495299912217,-27.2731520479229,6.8963580295583));
#26964=CARTESIAN_POINT('Ctrl Pts',(89.7777345026471,-26.5839248467685,6.73837486430966));
#26965=CARTESIAN_POINT('Ctrl Pts',(88.6216096701968,-23.5509896104921,6.58039169906103));
#26966=CARTESIAN_POINT('Ctrl Pts',(90.529800178905,-20.9253221252473,6.42240853381239));
#26967=CARTESIAN_POINT('Ctrl Pts',(93.77151210626,-21.088492416741,6.26442536856375));
#26968=CARTESIAN_POINT('Ctrl Pts',(95.4064020878083,-23.8924994627401,6.10644220331513));
#26969=CARTESIAN_POINT('Ctrl Pts',(93.9515691078723,-26.7940131650148,5.94845903806649));
#26970=CARTESIAN_POINT('Ctrl Pts',(90.7265963358753,-27.1612615610831,5.79047587281786));
#26971=CARTESIAN_POINT('Ctrl Pts',(88.6566441512317,-24.6611378205524,5.63249270756922));
#26972=CARTESIAN_POINT('Ctrl Pts',(89.6192298373179,-21.5613395107681,5.47450954232059));
#26973=CARTESIAN_POINT('Ctrl Pts',(92.7412553217636,-20.6734895013926,5.31652637707195));
#26974=CARTESIAN_POINT('Ctrl Pts',(95.1909369286972,-22.8028980552375,5.15854321182332));
#26975=CARTESIAN_POINT('Ctrl Pts',(94.7463298278668,-26.0181189325473,5.00056004657468));
#26976=CARTESIAN_POINT('Ctrl Pts',(91.8107078348689,-27.4028370554907,4.84257688132605));
#26977=CARTESIAN_POINT('Ctrl Pts',(89.0467802969359,-25.7010658226169,4.68459371607741));
#26978=CARTESIAN_POINT('Ctrl Pts',(88.9615238286993,-22.4563698283487,4.52661055082878));
#26979=CARTESIAN_POINT('Ctrl Pts',(91.6322689589712,-20.6117990856598,4.36862738558015));
#26980=CARTESIAN_POINT('Ctrl Pts',(94.6365586919768,-21.8404422219323,4.21064422033151));
#26981=CARTESIAN_POINT('Ctrl Pts',(95.2493997059401,-25.0278779669281,4.05266105508288));
#26982=CARTESIAN_POINT('Ctrl Pts',(92.9149242654226,-27.2829933251512,3.89467788983424));
#26983=CARTESIAN_POINT('Ctrl Pts',(89.7505813127906,-26.5603216554947,3.73669472458561));
#26984=CARTESIAN_POINT('Ctrl Pts',(88.6265378359784,-23.5153509088937,3.57871155933697));
#26985=CARTESIAN_POINT('Ctrl Pts',(90.5623397895163,-20.9099733200387,3.42072839408834));
#26986=CARTESIAN_POINT('Ctrl Pts',(93.8021484117901,-21.1073556238168,3.2627452288397));
#26987=CARTESIAN_POINT('Ctrl Pts',(95.4073473476108,-23.9284646500523,3.10476206359107));
#26988=CARTESIAN_POINT('Ctrl Pts',(93.9219650521703,-26.8144596176325,2.94677889834244));
#26989=CARTESIAN_POINT('Ctrl Pts',(90.693296665128,-27.1476417340791,2.7887957330938));
#26990=CARTESIAN_POINT('Ctrl Pts',(88.6498491034197,-24.6258092721029,2.63081256784516));
#26991=CARTESIAN_POINT('Ctrl Pts',(89.6451103099197,-21.5363384536773,2.47282940259654));
#26992=CARTESIAN_POINT('Ctrl Pts',(92.7763214072855,-20.6815090600495,2.3148462373479));
#26993=CARTESIAN_POINT('Ctrl Pts',(95.2034140175415,-22.8366308985733,2.15686307209927));
#26994=CARTESIAN_POINT('Ctrl Pts',(94.7248363812625,-26.0470362712681,1.99887990685063));
#26995=CARTESIAN_POINT('Ctrl Pts',(91.7748706653183,-27.4005708826831,1.840896741602));
#26996=CARTESIAN_POINT('Ctrl Pts',(89.0288363056218,-25.6699555291964,1.68291357635336));
#26997=CARTESIAN_POINT('Ctrl Pts',(88.9782975189349,-22.4240536163567,1.52493041110473));
#26998=CARTESIAN_POINT('Ctrl Pts',(91.6674251519505,-20.6087735847125,1.36694724585609));
#26999=CARTESIAN_POINT('Ctrl Pts',(94.6605002667765,-21.8670188467834,1.20896408060746));
#27000=CARTESIAN_POINT('Ctrl Pts',(95.2356808058288,-25.0649572109792,1.05098091535882));
#27001=CARTESIAN_POINT('Ctrl Pts',(93.6691444859934,-26.5433639279422,0.945658805193066));
#27002=CARTESIAN_POINT('Ctrl Pts',(92.7459328543469,-26.7901775698422,0.892997750110188));
#27003=CARTESIAN_POINT('Ctrl Pts',(94.3360626576961,-22.0026984430694,10.3210067496694));
#27004=CARTESIAN_POINT('Ctrl Pts',(94.9969281342143,-22.7756529106096,10.2683456945866));
#27005=CARTESIAN_POINT('Ctrl Pts',(95.4795873928596,-25.0164850731786,10.1630235844208));
#27006=CARTESIAN_POINT('Ctrl Pts',(93.0474777380319,-27.4743143045852,10.0050404191722));
#27007=CARTESIAN_POINT('Ctrl Pts',(89.6641396670172,-26.7735801351583,9.84705725392352));
#27008=CARTESIAN_POINT('Ctrl Pts',(88.4000491157039,-23.5606284927479,9.6890740886749));
#27009=CARTESIAN_POINT('Ctrl Pts',(90.4009680446667,-20.744487174453,9.53109092342626));
#27010=CARTESIAN_POINT('Ctrl Pts',(93.8523951731074,-20.8820464105141,9.37310775817762));
#27011=CARTESIAN_POINT('Ctrl Pts',(95.6235721938174,-23.847285073477,9.215124592929));
#27012=CARTESIAN_POINT('Ctrl Pts',(94.1080771138749,-26.9512425629647,9.05714142768035));
#27013=CARTESIAN_POINT('Ctrl Pts',(90.680468686986,-27.3782238204297,8.89915826243172));
#27014=CARTESIAN_POINT('Ctrl Pts',(88.4497277644466,-24.7410889898031,8.74117509718309));
#27015=CARTESIAN_POINT('Ctrl Pts',(89.4392012341389,-21.4317375405466,8.58319193193445));
#27016=CARTESIAN_POINT('Ctrl Pts',(92.7514084034007,-20.4518993616932,8.42520876668581));
#27017=CARTESIAN_POINT('Ctrl Pts',(95.38206161577,-22.6903039066152,8.26722560143718));
#27018=CARTESIAN_POINT('Ctrl Pts',(94.9450699403021,-26.1166502818288,8.10924243618855));
#27019=CARTESIAN_POINT('Ctrl Pts',(91.8367990946118,-27.6231212490059,7.95125927093992));
#27020=CARTESIAN_POINT('Ctrl Pts',(88.8765571447008,-25.8432982426317,7.79327610569128));
#27021=CARTESIAN_POINT('Ctrl Pts',(88.7493844233324,-22.3915404892829,7.63529294044265));
#27022=CARTESIAN_POINT('Ctrl Pts',(91.5706310054557,-20.3987105715367,7.47730977519401));
#27023=CARTESIAN_POINT('Ctrl Pts',(94.7813299086865,-21.6723730071853,7.31932660994538));
#27024=CARTESIAN_POINT('Ctrl Pts',(95.4692676579736,-25.0572726103797,7.16134344469675));
#27025=CARTESIAN_POINT('Ctrl Pts',(93.0104612250053,-27.483189850294,7.00336027944811));
#27026=CARTESIAN_POINT('Ctrl Pts',(89.6351319731846,-26.7497350164036,6.84537711419948));
#27027=CARTESIAN_POINT('Ctrl Pts',(88.4048187389981,-23.5221766638054,6.68739394895084));
#27028=CARTESIAN_POINT('Ctrl Pts',(90.4354576201273,-20.7280203884636,6.52941078370221));
#27029=CARTESIAN_POINT('Ctrl Pts',(93.8851898408184,-20.9016612993894,6.37142761845357));
#27030=CARTESIAN_POINT('Ctrl Pts',(95.6249905303983,-23.885601165237,6.21344445320494));
#27031=CARTESIAN_POINT('Ctrl Pts',(94.0768010801705,-26.9733046786334,6.0554612879563));
#27032=CARTESIAN_POINT('Ctrl Pts',(90.6448821645723,-27.3641193633755,5.89747812270767));
#27033=CARTESIAN_POINT('Ctrl Pts',(88.4421013787792,-24.7035629608637,5.73949495745903));
#27034=CARTESIAN_POINT('Ctrl Pts',(89.4664560811345,-21.4048509387775,5.5815117922104));
#27035=CARTESIAN_POINT('Ctrl Pts',(92.7888215932045,-20.4600276931837,5.42352862696176));
#27036=CARTESIAN_POINT('Ctrl Pts',(95.3956989960243,-22.7260801567682,5.26554546171313));
#27037=CARTESIAN_POINT('Ctrl Pts',(94.9225615070513,-26.1476213996829,5.10756229646449));
#27038=CARTESIAN_POINT('Ctrl Pts',(91.7985609777146,-27.6211967303539,4.94957913121586));
#27039=CARTESIAN_POINT('Ctrl Pts',(88.8572725175023,-25.8102230269998,4.79159596596722));
#27040=CARTESIAN_POINT('Ctrl Pts',(88.7665451511941,-22.3573152521541,4.6336128007186));
#27041=CARTESIAN_POINT('Ctrl Pts',(91.6086716990242,-20.394378610344,4.47562963546995));
#27042=CARTESIAN_POINT('Ctrl Pts',(94.8057463695968,-21.7018636398323,4.31764647022133));
#27043=CARTESIAN_POINT('Ctrl Pts',(95.4579133231718,-25.0938367815869,4.15966330497269));
#27044=CARTESIAN_POINT('Ctrl Pts',(92.9736348536358,-27.493662641186,4.00168013972405));
#27045=CARTESIAN_POINT('Ctrl Pts',(89.6062363661592,-26.7246172109746,3.84369697447542));
#27046=CARTESIAN_POINT('Ctrl Pts',(88.4100631446291,-23.4842510306947,3.68571380922679));
#27047=CARTESIAN_POINT('Ctrl Pts',(90.4700852939275,-20.7116866521342,3.52773064397815));
#27048=CARTESIAN_POINT('Ctrl Pts',(93.9177920746623,-20.9217349563625,3.36974747872952));
#27049=CARTESIAN_POINT('Ctrl Pts',(95.625996447417,-23.9238742346134,3.21176431348088));
#27050=CARTESIAN_POINT('Ctrl Pts',(94.0452973355112,-26.9950631778383,3.05378114823225));
#27051=CARTESIAN_POINT('Ctrl Pts',(90.6094456576621,-27.3496255535896,2.89579798298361));
#27052=CARTESIAN_POINT('Ctrl Pts',(88.4348702935058,-24.6659673833949,2.73781481773498));
#27053=CARTESIAN_POINT('Ctrl Pts',(89.4939973007808,-21.3782455666376,2.57983165248634));
#27054=CARTESIAN_POINT('Ctrl Pts',(92.8261378655289,-20.4685618660265,2.42184848723771));
#27055=CARTESIAN_POINT('Ctrl Pts',(95.4089767382702,-22.7619776329039,2.26386532198907));
#27056=CARTESIAN_POINT('Ctrl Pts',(94.899688828372,-26.1783943608088,2.10588215674044));
#27057=CARTESIAN_POINT('Ctrl Pts',(91.7604241409854,-27.6187851374898,1.9478989914918));
#27058=CARTESIAN_POINT('Ctrl Pts',(88.8381770622638,-25.7771163895153,1.78991582624317));
#27059=CARTESIAN_POINT('Ctrl Pts',(88.784395207264,-22.3229253124378,1.63193266099454));
#27060=CARTESIAN_POINT('Ctrl Pts',(91.6460838609914,-20.3911589633379,1.4739494957459));
#27061=CARTESIAN_POINT('Ctrl Pts',(94.8312242725849,-21.7301456837402,1.31596633049727));
#27062=CARTESIAN_POINT('Ctrl Pts',(95.4433140827682,-25.1332953965992,1.15798316524863));
#27063=CARTESIAN_POINT('Ctrl Pts',(93.7762533017603,-26.7065713079336,1.05266105508288));
#27064=CARTESIAN_POINT('Ctrl Pts',(92.7937992825328,-26.9692229537457,0.999999999999999));
#27065=CARTESIAN_POINT('Ctrl Pts',(93.9134659966651,-22.3640127966251,10.));
#27066=CARTESIAN_POINT('Ctrl Pts',(93.9750770578955,-22.4219120654398,10.));
#27067=CARTESIAN_POINT('Ctrl Pts',(94.0333190151648,-22.4829618973501,10.));
#27068=CARTESIAN_POINT('Ctrl Pts',(94.0881941987852,-22.5467775157033,10.));
#27069=CARTESIAN_POINT('Ctrl Pts',(94.1445220900365,-22.6122825213101,10.));
#27070=CARTESIAN_POINT('Ctrl Pts',(94.19730302831,-22.6807021204397,10.));
#27071=CARTESIAN_POINT('Ctrl Pts',(94.246514026676,-22.7516687130522,10.));
#27072=CARTESIAN_POINT('Ctrl Pts',(94.2970865251706,-22.8245987087286,10.));
#27073=CARTESIAN_POINT('Ctrl Pts',(94.3438893496014,-22.9002191359243,10.));
#27074=CARTESIAN_POINT('Ctrl Pts',(94.3868634537135,-22.9781740458772,10.));
#27075=CARTESIAN_POINT('Ctrl Pts',(94.4057549128497,-23.0124431022373,10.));
#27076=CARTESIAN_POINT('Ctrl Pts',(94.4239059912867,-23.0471637926691,10.));
#27077=CARTESIAN_POINT('Ctrl Pts',(94.4413092551545,-23.0823079492044,10.));
#27078=CARTESIAN_POINT('Ctrl Pts',(94.4512342776001,-23.1023505426566,10.));
#27079=CARTESIAN_POINT('Ctrl Pts',(94.4609160539065,-23.1225308841615,10.));
#27080=CARTESIAN_POINT('Ctrl Pts',(94.4703529715552,-23.1428438969986,10.));
#27081=CARTESIAN_POINT('Ctrl Pts',(94.4788699915235,-23.1611768254387,10.));
#27082=CARTESIAN_POINT('Ctrl Pts',(94.4871899465833,-23.1796235690021,10.));
#27083=CARTESIAN_POINT('Ctrl Pts',(94.4952979566468,-23.1981485647195,10.));
#27084=CARTESIAN_POINT('Ctrl Pts',(94.5318626759043,-23.2816907979364,10.));
#27085=CARTESIAN_POINT('Ctrl Pts',(94.5641670779769,-23.366916527663,10.));
#27086=CARTESIAN_POINT('Ctrl Pts',(94.5921860624412,-23.4534270379695,10.));
#27087=CARTESIAN_POINT('Ctrl Pts',(94.6206677373038,-23.5413661361863,10.));
#27088=CARTESIAN_POINT('Ctrl Pts',(94.6447217851998,-23.6306335527319,10.));
#27089=CARTESIAN_POINT('Ctrl Pts',(94.664282765984,-23.7208476135917,10.));
#27090=CARTESIAN_POINT('Ctrl Pts',(94.6832631734611,-23.8083841054565,10.));
#27091=CARTESIAN_POINT('Ctrl Pts',(94.6980134264571,-23.8968127993399,10.));
#27092=CARTESIAN_POINT('Ctrl Pts',(94.7084329206264,-23.9858069094092,10.));
#27093=CARTESIAN_POINT('Ctrl Pts',(94.7127922670595,-24.0230405936937,10.));
#27094=CARTESIAN_POINT('Ctrl Pts',(94.7163930212393,-24.0603734428421,10.));
#27095=CARTESIAN_POINT('Ctrl Pts',(94.7192254940158,-24.0977821388602,10.));
#27096=CARTESIAN_POINT('Ctrl Pts',(94.7209960695383,-24.121166272346,10.));
#27097=CARTESIAN_POINT('Ctrl Pts',(94.7224664121845,-24.1445800482853,10.));
#27098=CARTESIAN_POINT('Ctrl Pts',(94.7236338650185,-24.168017803389,10.));
#27099=CARTESIAN_POINT('Ctrl Pts',(94.7243181282436,-24.1817550554887,10.));
#27100=CARTESIAN_POINT('Ctrl Pts',(94.724898065248,-24.1954959766469,10.));
#27101=CARTESIAN_POINT('Ctrl Pts',(94.7253731538336,-24.2092311923572,10.));
#27102=CARTESIAN_POINT('Ctrl Pts',(94.7287309598134,-24.306308223558,10.));
#27103=CARTESIAN_POINT('Ctrl Pts',(94.726861580852,-24.4032207088614,10.));
#27104=CARTESIAN_POINT('Ctrl Pts',(94.7197002220053,-24.4995463878866,10.));
#27105=CARTESIAN_POINT('Ctrl Pts',(94.7125388631585,-24.5958720669118,10.));
#27106=CARTESIAN_POINT('Ctrl Pts',(94.7000859592916,-24.6916119941747,10.));
#27107=CARTESIAN_POINT('Ctrl Pts',(94.6822238228945,-24.7863628481204,10.));
#27108=CARTESIAN_POINT('Ctrl Pts',(94.6651462975085,-24.8769516823807,10.));
#27109=CARTESIAN_POINT('Ctrl Pts',(94.6431244275635,-24.9666373988193,10.));
#27110=CARTESIAN_POINT('Ctrl Pts',(94.6164329081479,-25.0551806589533,10.));
#27111=CARTESIAN_POINT('Ctrl Pts',(94.6074980340553,-25.0848201436421,10.));
#27112=CARTESIAN_POINT('Ctrl Pts',(94.5980394679057,-25.1143315742024,10.));
#27113=CARTESIAN_POINT('Ctrl Pts',(94.5880662379456,-25.14370579416,10.));
#27114=CARTESIAN_POINT('Ctrl Pts',(94.5815849548301,-25.1627951600529,10.));
#27115=CARTESIAN_POINT('Ctrl Pts',(94.5748863019078,-25.1818265755599,10.));
#27116=CARTESIAN_POINT('Ctrl Pts',(94.5679726206488,-25.2007974925995,10.));
#27117=CARTESIAN_POINT('Ctrl Pts',(94.5613831132945,-25.2188788869637,10.));
#27118=CARTESIAN_POINT('Ctrl Pts',(94.5545965181257,-25.2369095329808,10.));
#27119=CARTESIAN_POINT('Ctrl Pts',(94.5476256545372,-25.2548600743819,10.));
#27120=CARTESIAN_POINT('Ctrl Pts',(94.5137821755734,-25.3420097887006,10.));
#27121=CARTESIAN_POINT('Ctrl Pts',(94.4755603548741,-25.4273852003437,10.));
#27122=CARTESIAN_POINT('Ctrl Pts',(94.4332913755525,-25.5107526954609,10.));
#27123=CARTESIAN_POINT('Ctrl Pts',(94.3894531453979,-25.5972152383712,10.));
#27124=CARTESIAN_POINT('Ctrl Pts',(94.3412615513892,-25.6815187325337,10.));
#27125=CARTESIAN_POINT('Ctrl Pts',(94.2890300742868,-25.7633995606624,10.));
#27126=CARTESIAN_POINT('Ctrl Pts',(94.2362101788303,-25.8462028245481,10.));
#27127=CARTESIAN_POINT('Ctrl Pts',(94.1792584551776,-25.9265293491613,10.));
#27128=CARTESIAN_POINT('Ctrl Pts',(94.1184473133391,-26.0040916615067,10.));
#27129=CARTESIAN_POINT('Ctrl Pts',(94.0767848210946,-26.0572305952426,10.));
#27130=CARTESIAN_POINT('Ctrl Pts',(94.0333097148272,-26.1090717583023,10.));
#27131=CARTESIAN_POINT('Ctrl Pts',(93.9880973825635,-26.159515663108,10.));
#27132=CARTESIAN_POINT('Ctrl Pts',(93.9759903694326,-26.1730235930748,10.));
#27133=CARTESIAN_POINT('Ctrl Pts',(93.9637574535261,-26.1864325457838,10.));
#27134=CARTESIAN_POINT('Ctrl Pts',(93.9514137007096,-26.199726113673,10.));
#27135=CARTESIAN_POINT('Ctrl Pts',(93.8827528892985,-26.273670170346,10.));
#27136=CARTESIAN_POINT('Ctrl Pts',(93.8105781862797,-26.3441463401416,10.));
#27137=CARTESIAN_POINT('Ctrl Pts',(93.7352000515009,-26.4108648135309,10.));
#27138=CARTESIAN_POINT('Ctrl Pts',(93.6722951821929,-26.4665429868008,10.));
#27139=CARTESIAN_POINT('Ctrl Pts',(93.6071582639901,-26.5196041737296,10.));
#27140=CARTESIAN_POINT('Ctrl Pts',(93.5399460670852,-26.5698661697182,10.));
#27141=CARTESIAN_POINT('Ctrl Pts',(93.5180638151575,-26.5862299505385,10.));
#27142=CARTESIAN_POINT('Ctrl Pts',(93.4959614387476,-26.6022969068259,10.));
#27143=CARTESIAN_POINT('Ctrl Pts',(93.473643921931,-26.6180603652787,10.));
#27144=CARTESIAN_POINT('Ctrl Pts',(93.4508750768599,-26.6341426089371,10.));
#27145=CARTESIAN_POINT('Ctrl Pts',(93.4278768876333,-26.6499123832023,10.));
#27146=CARTESIAN_POINT('Ctrl Pts',(93.4046837833618,-26.6653433745001,10.));
#27147=CARTESIAN_POINT('Ctrl Pts',(93.3197384868702,-26.7218597474537,10.));
#27148=CARTESIAN_POINT('Ctrl Pts',(93.2321269166639,-26.7738756911564,10.));
#27149=CARTESIAN_POINT('Ctrl Pts',(93.1421393365345,-26.8210831412052,10.));
#27150=CARTESIAN_POINT('Ctrl Pts',(93.0588657411436,-26.8647684374332,10.));
#27151=CARTESIAN_POINT('Ctrl Pts',(92.9735566410059,-26.9043362525348,10.));
#27152=CARTESIAN_POINT('Ctrl Pts',(92.8864146397764,-26.9395136119409,10.));
#27153=CARTESIAN_POINT('Ctrl Pts',(92.8563906944762,-26.9516336355772,10.));
#27154=CARTESIAN_POINT('Ctrl Pts',(92.8261489679874,-26.9632321934336,10.));
#27155=CARTESIAN_POINT('Ctrl Pts',(92.7957018439802,-26.9743128659187,10.));
#27156=CARTESIAN_POINT('Ctrl Pts',(89.4817891743669,-24.002194435609,8.38741669750802));
#27157=CARTESIAN_POINT('Ctrl Pts',(89.4802231872165,-24.1747250532131,8.39833391417657));
#27158=CARTESIAN_POINT('Ctrl Pts',(89.4964591581217,-24.3469627518866,8.40925113084511));
#27159=CARTESIAN_POINT('Ctrl Pts',(89.5315887215665,-24.5152564315154,8.42016834751366));
#27160=CARTESIAN_POINT('Ctrl Pts',(89.7010421575268,-25.3270496753528,8.47282940259653));
#27161=CARTESIAN_POINT('Ctrl Pts',(90.3101078559698,-26.0470742874782,8.52549045767941));
#27162=CARTESIAN_POINT('Ctrl Pts',(91.0825656666734,-26.3487966246852,8.57815151276229));
#27163=CARTESIAN_POINT('Ctrl Pts',(91.855023477377,-26.6505189618922,8.63081256784516));
#27164=CARTESIAN_POINT('Ctrl Pts',(92.7908734003413,-26.5339390241808,8.68347362292804));
#27165=CARTESIAN_POINT('Ctrl Pts',(93.4656883820911,-26.0519077734106,8.73613467801092));
#27166=CARTESIAN_POINT('Ctrl Pts',(94.1405033638409,-25.5698765226404,8.7887957330938));
#27167=CARTESIAN_POINT('Ctrl Pts',(94.5542834043762,-24.7223939588114,8.84145678817668));
#27168=CARTESIAN_POINT('Ctrl Pts',(94.5193786114755,-23.8938487978226,8.89411784325956));
#27169=CARTESIAN_POINT('Ctrl Pts',(94.4844738185748,-23.0653036368338,8.94677889834244));
#27170=CARTESIAN_POINT('Ctrl Pts',(94.000884192238,-22.2556958786852,8.99943995342531));
#27171=CARTESIAN_POINT('Ctrl Pts',(93.2879127728201,-21.8321128999534,9.05210100850819));
#27172=CARTESIAN_POINT('Ctrl Pts',(92.5749413534021,-21.4085299212216,9.10476206359107));
#27173=CARTESIAN_POINT('Ctrl Pts',(91.6325881409029,-21.3709717219067,9.15742311867395));
#27174=CARTESIAN_POINT('Ctrl Pts',(90.8882531699407,-21.7366422599482,9.21008417375683));
#27175=CARTESIAN_POINT('Ctrl Pts',(90.1439181989786,-22.1023127979897,9.2627452288397));
#27176=CARTESIAN_POINT('Ctrl Pts',(89.5976014695535,-22.8712120733877,9.31540628392258));
#27177=CARTESIAN_POINT('Ctrl Pts',(89.4970122693619,-23.6942824886892,9.36806733900546));
#27178=CARTESIAN_POINT('Ctrl Pts',(89.4846923712707,-23.7950899672168,9.37451712517298));
#27179=CARTESIAN_POINT('Ctrl Pts',(89.4790586980532,-23.8967100507537,9.3809669113405));
#27180=CARTESIAN_POINT('Ctrl Pts',(89.4798238762261,-23.9984131135314,9.38741669750802));
#27181=CARTESIAN_POINT('Ctrl Pts',(91.2062007174671,-26.9692229537457,10.));
#27182=CARTESIAN_POINT('Ctrl Pts',(90.2237466982397,-26.7065713079336,9.94733894491712));
#27183=CARTESIAN_POINT('Ctrl Pts',(88.5566846367919,-25.1333040393726,9.84201683475137));
#27184=CARTESIAN_POINT('Ctrl Pts',(89.1687768340778,-21.7301430813076,9.68403366950273));
#27185=CARTESIAN_POINT('Ctrl Pts',(92.3539160472627,-20.3911616367203,9.52605050425409));
#27186=CARTESIAN_POINT('Ctrl Pts',(95.215603926767,-22.3229247027849,9.36806733900546));
#27187=CARTESIAN_POINT('Ctrl Pts',(95.1618223030446,-25.7771165220753,9.21008417375683));
#27188=CARTESIAN_POINT('Ctrl Pts',(92.2395757220273,-27.6187839878381,9.0521010085082));
#27189=CARTESIAN_POINT('Ctrl Pts',(89.1003119065523,-26.1783940085773,8.89411784325955));
#27190=CARTESIAN_POINT('Ctrl Pts',(88.5910240312662,-22.7619778387773,8.73613467801093));
#27191=CARTESIAN_POINT('Ctrl Pts',(91.1738623478633,-20.4685627419331,8.57815151276229));
#27192=CARTESIAN_POINT('Ctrl Pts',(94.5060020988175,-21.3782461595948,8.42016834751366));
#27193=CARTESIAN_POINT('Ctrl Pts',(95.5651288739418,-24.665967239189,8.26218518226502));
#27194=CARTESIAN_POINT('Ctrl Pts',(93.3905540118639,-27.3496247591347,8.10420201701638));
#27195=CARTESIAN_POINT('Ctrl Pts',(89.9547031474507,-26.9950624766613,7.94621885176775));
#27196=CARTESIAN_POINT('Ctrl Pts',(88.3740044045685,-23.923874250773,7.78823568651912));
#27197=CARTESIAN_POINT('Ctrl Pts',(90.0822083770022,-20.9217356813897,7.63025252127048));
#27198=CARTESIAN_POINT('Ctrl Pts',(93.5299143458989,-20.7116874252053,7.47226935602185));
#27199=CARTESIAN_POINT('Ctrl Pts',(95.5899360110292,-23.4842511522573,7.31428619077322));
#27200=CARTESIAN_POINT('Ctrl Pts',(94.3937630706594,-26.7246165699189,7.15630302552457));
#27201=CARTESIAN_POINT('Ctrl Pts',(91.0263653754403,-27.4936618194068,6.99831986027595));
#27202=CARTESIAN_POINT('Ctrl Pts',(88.5420874902395,-25.0938365242431,6.84033669502731));
#27203=CARTESIAN_POINT('Ctrl Pts',(89.194254290432,-21.7018641804574,6.68235352977868));
#27204=CARTESIAN_POINT('Ctrl Pts',(92.3913282089151,-20.3943794585145,6.52437036453004));
#27205=CARTESIAN_POINT('Ctrl Pts',(95.2334540881775,-22.3573156385801,6.36638719928141));
#27206=CARTESIAN_POINT('Ctrl Pts',(95.1427267432077,-25.8102226011645,6.20840403403277));
#27207=CARTESIAN_POINT('Ctrl Pts',(92.2014389749,-27.6211958785123,6.05042086878414));
#27208=CARTESIAN_POINT('Ctrl Pts',(89.0774391804456,-26.1476208944803,5.89243770353551));
#27209=CARTESIAN_POINT('Ctrl Pts',(88.604301802773,-22.7260804564427,5.73445453828687));
#27210=CARTESIAN_POINT('Ctrl Pts',(91.2111785923562,-20.4600285259192,5.57647137303824));
#27211=CARTESIAN_POINT('Ctrl Pts',(94.53354332288,-21.4048515492551,5.4184882077896));
#27212=CARTESIAN_POINT('Ctrl Pts',(95.5578977842681,-24.7035627953589,5.26050504254097));
#27213=CARTESIAN_POINT('Ctrl Pts',(93.3551175166525,-27.3641185720073,5.10252187729233));
#27214=CARTESIAN_POINT('Ctrl Pts',(89.9231994083719,-26.9733039791991,4.9445387120437));
#27215=CARTESIAN_POINT('Ctrl Pts',(88.3750103223367,-23.8856011921486,4.78655554679506));
#27216=CARTESIAN_POINT('Ctrl Pts',(90.1148106026499,-20.9016620282348,4.62857238154643));
#27217=CARTESIAN_POINT('Ctrl Pts',(93.5645420118329,-20.7280211581598,4.4705892162978));
#27218=CARTESIAN_POINT('Ctrl Pts',(95.595180415279,-23.5221767762025,4.31260605104916));
#27219=CARTESIAN_POINT('Ctrl Pts',(94.3648674705089,-26.7497343695717,4.15462288580053));
#27220=CARTESIAN_POINT('Ctrl Pts',(90.9895390126931,-27.4831890308961,3.99663972055189));
#27221=CARTESIAN_POINT('Ctrl Pts',(88.5307331581303,-25.0572723617073,3.83865655530326));
#27222=CARTESIAN_POINT('Ctrl Pts',(89.2186707455856,-21.6723735546569,3.68067339005462));
#27223=CARTESIAN_POINT('Ctrl Pts',(92.429368893546,-20.3987114188412,3.52269022480599));
#27224=CARTESIAN_POINT('Ctrl Pts',(95.2506148119859,-22.3915408673733,3.36470705955735));
#27225=CARTESIAN_POINT('Ctrl Pts',(95.1234421205799,-25.8432978095596,3.20672389430872));
#27226=CARTESIAN_POINT('Ctrl Pts',(92.1632008669202,-27.6231203956681,3.04874072906009));
#27227=CARTESIAN_POINT('Ctrl Pts',(89.0549307526673,-26.1166497859116,2.89075756381145));
#27228=CARTESIAN_POINT('Ctrl Pts',(88.6179391794157,-22.6903042108869,2.73277439856282));
#27229=CARTESIAN_POINT('Ctrl Pts',(91.2485917742672,-20.451900203599,2.57479123331418));
#27230=CARTESIAN_POINT('Ctrl Pts',(94.5607981614372,-21.4317381309793,2.41680806806555));
#27231=CARTESIAN_POINT('Ctrl Pts',(95.5502714048858,-24.7410888412383,2.25882490281692));
#27232=CARTESIAN_POINT('Ctrl Pts',(93.3195309927209,-27.3782229777192,2.10084173756828));
#27233=CARTESIAN_POINT('Ctrl Pts',(89.8919234036862,-26.9512419574066,1.94285857231965));
#27234=CARTESIAN_POINT('Ctrl Pts',(88.3764286113539,-23.8472849474598,1.78487540707101));
#27235=CARTESIAN_POINT('Ctrl Pts',(90.1476053652115,-20.8820474355396,1.62689224182238));
#27236=CARTESIAN_POINT('Ctrl Pts',(93.5990313571954,-20.7444874247256,1.46890907657374));
#27237=CARTESIAN_POINT('Ctrl Pts',(95.5999505159819,-23.5606294856849,1.31092591132511));
#27238=CARTESIAN_POINT('Ctrl Pts',(94.33585874306,-26.7735779839873,1.15294274607647));
#27239=CARTESIAN_POINT('Ctrl Pts',(90.9525246480968,-27.4743158223952,0.994959580827838));
#27240=CARTESIAN_POINT('Ctrl Pts',(88.5204066563018,-25.0164786759465,0.836976415579204));
#27241=CARTESIAN_POINT('Ctrl Pts',(89.0030718657857,-22.7756529106096,0.731654305413447));
#27242=CARTESIAN_POINT('Ctrl Pts',(89.6639373423039,-22.0026984430693,0.678993250330568));
#27243=CARTESIAN_POINT('Ctrl Pts',(91.254067145653,-26.7901775698421,10.1070022498898));
#27244=CARTESIAN_POINT('Ctrl Pts',(90.3308555140066,-26.5433639279422,10.0543411948069));
#27245=CARTESIAN_POINT('Ctrl Pts',(88.7643179909425,-25.0649653325897,9.94901908464118));
#27246=CARTESIAN_POINT('Ctrl Pts',(89.3395007731539,-21.8670164012787,9.79103591939254));
#27247=CARTESIAN_POINT('Ctrl Pts',(92.332574761836,-20.6087760968887,9.63305275414391));
#27248=CARTESIAN_POINT('Ctrl Pts',(95.0217016673144,-22.4240530434662,9.47506958889527));
#27249=CARTESIAN_POINT('Ctrl Pts',(94.9711630979589,-25.669955653763,9.31708642364664));
#27250=CARTESIAN_POINT('Ctrl Pts',(92.2251292059548,-27.400569802356,9.159103258398));
#27251=CARTESIAN_POINT('Ctrl Pts',(89.2751643093457,-26.0470359402764,9.00112009314937));
#27252=CARTESIAN_POINT('Ctrl Pts',(88.7965867055915,-22.8366310920326,8.84313692790073));
#27253=CARTESIAN_POINT('Ctrl Pts',(91.2236787932393,-20.6815098831386,8.6851537626521));
#27254=CARTESIAN_POINT('Ctrl Pts',(94.354889125883,-21.536339010879,8.52717059740346));
#27255=CARTESIAN_POINT('Ctrl Pts',(95.3501501142311,-24.6258091365927,8.36918743215484));
#27256=CARTESIAN_POINT('Ctrl Pts',(93.3067030243257,-27.1476409875303,8.21120426690619));
#27257=CARTESIAN_POINT('Ctrl Pts',(90.0780354016687,-26.8144589587366,8.05322110165756));
#27258=CARTESIAN_POINT('Ctrl Pts',(88.5926534529997,-23.9284646652375,7.89523793640893));
#27259=CARTESIAN_POINT('Ctrl Pts',(90.1978520126387,-21.1073563051245,7.7372547711603));
#27260=CARTESIAN_POINT('Ctrl Pts',(93.4376598720287,-20.9099740464933,7.57927160591166));
#27261=CARTESIAN_POINT('Ctrl Pts',(95.3734613705941,-23.515351023126,7.42128844066303));
#27262=CARTESIAN_POINT('Ctrl Pts',(94.249418157988,-26.560321053095,7.26330527541439));
#27263=CARTESIAN_POINT('Ctrl Pts',(91.0850759498403,-27.2829925529256,7.10532211016575));
#27264=CARTESIAN_POINT('Ctrl Pts',(88.750601058422,-25.0278777251021,6.94733894491712));
#27265=CARTESIAN_POINT('Ctrl Pts',(89.363441928252,-21.8404427299575,6.78935577966849));
#27266=CARTESIAN_POINT('Ctrl Pts',(92.3677309545194,-20.6117998826853,6.63137261441986));
#27267=CARTESIAN_POINT('Ctrl Pts',(95.0384754565385,-22.456370191473,6.47338944917121));
#27268=CARTESIAN_POINT('Ctrl Pts',(94.9532190083536,-25.7010654224598,6.31540628392259));
#27269=CARTESIAN_POINT('Ctrl Pts',(92.189292120603,-27.4028362550155,6.15742311867395));
#27270=CARTESIAN_POINT('Ctrl Pts',(89.2536708181738,-26.0181184578087,5.99943995342532));
#27271=CARTESIAN_POINT('Ctrl Pts',(88.8090638219323,-22.8028983368416,5.84145678817668));
#27272=CARTESIAN_POINT('Ctrl Pts',(91.2587448526078,-20.6734902839138,5.68347362292805));
#27273=CARTESIAN_POINT('Ctrl Pts',(94.3807696026347,-21.5613400844336,5.52549045767941));
#27274=CARTESIAN_POINT('Ctrl Pts',(95.3433550622842,-24.6611376650276,5.36750729243078));
#27275=CARTESIAN_POINT('Ctrl Pts',(93.273403364572,-27.1612608174348,5.20952412718215));
#27276=CARTESIAN_POINT('Ctrl Pts',(90.0484313512107,-26.7940125077567,5.05154096193351));
#27277=CARTESIAN_POINT('Ctrl Pts',(88.5935987135065,-23.892499488029,4.89355779668487));
#27278=CARTESIAN_POINT('Ctrl Pts',(90.2284883104669,-21.0884931016366,4.73557463143624));
#27279=CARTESIAN_POINT('Ctrl Pts',(93.4701994752482,-20.9253228485305,4.57759146618761));
#27280=CARTESIAN_POINT('Ctrl Pts',(95.3783895350779,-23.5509897161116,4.41960830093897));
#27281=CARTESIAN_POINT('Ctrl Pts',(94.2222649745917,-26.5839242389408,4.26162513569034));
#27282=CARTESIAN_POINT('Ctrl Pts',(91.0504702321437,-27.273151277935,4.1036419704417));
#27283=CARTESIAN_POINT('Ctrl Pts',(88.73993139728,-24.9935183968346,3.94565880519307));
#27284=CARTESIAN_POINT('Ctrl Pts',(89.3863860609648,-21.8127304012065,3.78767563994443));
#27285=CARTESIAN_POINT('Ctrl Pts',(92.4034777699831,-20.6158706239954,3.6296924746958));
#27286=CARTESIAN_POINT('Ctrl Pts',(95.0546013815359,-22.4885316246793,3.47170930944716));
#27287=CARTESIAN_POINT('Ctrl Pts',(94.9350972565224,-25.7321461819781,3.31372614419853));
#27288=CARTESIAN_POINT('Ctrl Pts',(92.1533597865007,-27.4046447229832,3.1557429789499));
#27289=CARTESIAN_POINT('Ctrl Pts',(89.2325196579888,-25.9890149200186,2.99775981370126));
#27290=CARTESIAN_POINT('Ctrl Pts',(88.8218788590692,-22.7692794138311,2.83977664845263));
#27291=CARTESIAN_POINT('Ctrl Pts',(91.2939020040278,-20.6658521028235,2.681793483204));
#27292=CARTESIAN_POINT('Ctrl Pts',(94.4063809630467,-21.5866053940535,2.52381031795536));
#27293=CARTESIAN_POINT('Ctrl Pts',(95.336188556763,-24.6964008746715,2.36582715270673));
#27294=CARTESIAN_POINT('Ctrl Pts',(93.2399627228925,-27.174514721593,2.20784398745809));
#27295=CARTESIAN_POINT('Ctrl Pts',(90.0190413026668,-26.7732808350902,2.04986082220945));
#27296=CARTESIAN_POINT('Ctrl Pts',(88.5949314791037,-23.8564937288939,1.89187765696082));
#27297=CARTESIAN_POINT('Ctrl Pts',(90.2593055351526,-21.070061277071,1.73389449171219));
#27298=CARTESIAN_POINT('Ctrl Pts',(93.5026090986844,-20.9407961923469,1.57591132646355));
#27299=CARTESIAN_POINT('Ctrl Pts',(95.3828719967165,-23.5871237111563,1.41792816121492));
#27300=CARTESIAN_POINT('Ctrl Pts',(94.1950054855208,-26.6063300734514,1.25994499596628));
#27301=CARTESIAN_POINT('Ctrl Pts',(91.0156878491876,-27.2648131276116,1.10196183071765));
#27302=CARTESIAN_POINT('Ctrl Pts',(88.7302275878235,-24.9551845873584,0.943978665469013));
#27303=CARTESIAN_POINT('Ctrl Pts',(89.1837878836397,-22.8494815513233,0.838656555303258));
#27304=CARTESIAN_POINT('Ctrl Pts',(89.8048028959809,-22.1231365609212,0.785995500220379));
#27305=CARTESIAN_POINT('Ctrl Pts',(91.301933573839,-26.6111321859386,10.2140044997796));
#27306=CARTESIAN_POINT('Ctrl Pts',(90.4379643297735,-26.3801565479507,10.1613434446967));
#27307=CARTESIAN_POINT('Ctrl Pts',(88.9719513450928,-24.9966266258069,10.056021334531));
#27308=CARTESIAN_POINT('Ctrl Pts',(89.5102247122303,-22.0038897212497,9.89803816928235));
#27309=CARTESIAN_POINT('Ctrl Pts',(92.3112334764091,-20.8263905570572,9.74005500403372));
#27310=CARTESIAN_POINT('Ctrl Pts',(94.8277994078618,-22.5251813841475,9.58207183878509));
#27311=CARTESIAN_POINT('Ctrl Pts',(94.7805038928732,-25.5627947854507,9.42408867353645));
#27312=CARTESIAN_POINT('Ctrl Pts',(92.2106826898821,-27.1823556168738,9.26610550828782));
#27313=CARTESIAN_POINT('Ctrl Pts',(89.4500167121391,-25.9156778719754,9.10812234303918));
#27314=CARTESIAN_POINT('Ctrl Pts',(89.0021493799168,-22.9112843452878,8.95013917779054));
#27315=CARTESIAN_POINT('Ctrl Pts',(91.2734952386149,-20.8944570243441,8.79215601254192));
#27316=CARTESIAN_POINT('Ctrl Pts',(94.2037761529487,-21.6944318621631,8.63417284729327));
#27317=CARTESIAN_POINT('Ctrl Pts',(95.1351713545205,-24.5856510339964,8.47618968204465));
#27318=CARTESIAN_POINT('Ctrl Pts',(93.2228520367874,-26.9456572159258,8.31820651679601));
#27319=CARTESIAN_POINT('Ctrl Pts',(90.2013676558868,-26.6338554408121,8.16022335154738));
#27320=CARTESIAN_POINT('Ctrl Pts',(88.8113025014309,-23.933055079702,8.00224018629874));
#27321=CARTESIAN_POINT('Ctrl Pts',(90.3134956482753,-21.2929769288594,7.84425702105011));
#27322=CARTESIAN_POINT('Ctrl Pts',(93.3454053981585,-21.1082606677813,7.68627385580147));
#27323=CARTESIAN_POINT('Ctrl Pts',(95.156986730159,-23.5464508939947,7.52829069055284));
#27324=CARTESIAN_POINT('Ctrl Pts',(94.1050732453165,-26.3960255362711,7.37030752530419));
#27325=CARTESIAN_POINT('Ctrl Pts',(91.1437865242403,-27.0723232864443,7.21232436005558));
#27326=CARTESIAN_POINT('Ctrl Pts',(88.9591146266045,-24.9619189259611,7.05434119480693));
#27327=CARTESIAN_POINT('Ctrl Pts',(89.5326295660721,-21.9790212794576,6.8963580295583));
#27328=CARTESIAN_POINT('Ctrl Pts',(92.3441337001234,-20.8292203068559,6.73837486430967));
#27329=CARTESIAN_POINT('Ctrl Pts',(94.8434968248997,-22.555424744366,6.58039169906103));
#27330=CARTESIAN_POINT('Ctrl Pts',(94.7637112734992,-25.591908243755,6.4224085338124));
#27331=CARTESIAN_POINT('Ctrl Pts',(92.1771452663062,-27.1844766315186,6.26442536856375));
#27332=CARTESIAN_POINT('Ctrl Pts',(89.4299024559019,-25.888616021137,6.10644220331513));
#27333=CARTESIAN_POINT('Ctrl Pts',(89.0138258410916,-22.8797162172404,5.94845903806648));
#27334=CARTESIAN_POINT('Ctrl Pts',(91.3063111128593,-20.8869520419083,5.79047587281787));
#27335=CARTESIAN_POINT('Ctrl Pts',(94.2279958823895,-21.7178286196122,5.63249270756922));
#27336=CARTESIAN_POINT('Ctrl Pts',(95.1288123403003,-24.6187125346963,5.47450954232059));
#27337=CARTESIAN_POINT('Ctrl Pts',(93.1916892124914,-26.9584030628623,5.31652637707196));
#27338=CARTESIAN_POINT('Ctrl Pts',(90.1736632940495,-26.6147210363142,5.15854321182332));
#27339=CARTESIAN_POINT('Ctrl Pts',(88.8121871046762,-23.8993977839094,5.00056004657468));
#27340=CARTESIAN_POINT('Ctrl Pts',(90.342166018284,-21.2753241750384,4.84257688132606));
#27341=CARTESIAN_POINT('Ctrl Pts',(93.3758569386635,-21.1226245389013,4.68459371607742));
#27342=CARTESIAN_POINT('Ctrl Pts',(95.1615986548766,-23.5798026560206,4.52661055082878));
#27343=CARTESIAN_POINT('Ctrl Pts',(94.0796624786748,-26.41811410831,4.36862738558015));
#27344=CARTESIAN_POINT('Ctrl Pts',(91.1114014515939,-27.0631135249739,4.21064422033152));
#27345=CARTESIAN_POINT('Ctrl Pts',(88.9491296364298,-24.9297644319618,4.05266105508287));
#27346=CARTESIAN_POINT('Ctrl Pts',(89.5541013763441,-21.9530872477561,3.89467788983425));
#27347=CARTESIAN_POINT('Ctrl Pts',(92.3775866464202,-20.8330298291496,3.73669472458561));
#27348=CARTESIAN_POINT('Ctrl Pts',(94.858587951086,-22.5855223819854,3.57871155933698));
#27349=CARTESIAN_POINT('Ctrl Pts',(94.7467523924648,-25.6209945543966,3.42072839408834));
#27350=CARTESIAN_POINT('Ctrl Pts',(92.1435187060813,-27.1861690502982,3.26274522883971));
#27351=CARTESIAN_POINT('Ctrl Pts',(89.4101085633103,-25.8613800541255,3.10476206359107));
#27352=CARTESIAN_POINT('Ctrl Pts',(89.0258185387226,-22.8482546167753,2.94677889834244));
#27353=CARTESIAN_POINT('Ctrl Pts',(91.3392122337884,-20.8798040020479,2.78879573309381));
#27354=CARTESIAN_POINT('Ctrl Pts',(94.2519637646563,-21.7414726571277,2.63081256784517));
#27355=CARTESIAN_POINT('Ctrl Pts',(95.1221057086401,-24.6517129081048,2.47282940259654));
#27356=CARTESIAN_POINT('Ctrl Pts',(93.1603944530641,-26.9708064654667,2.3148462373479));
#27357=CARTESIAN_POINT('Ctrl Pts',(90.1461592016474,-26.5953197127739,2.15686307209927));
#27358=CARTESIAN_POINT('Ctrl Pts',(88.8134343468535,-23.8657025103278,1.99887990685063));
#27359=CARTESIAN_POINT('Ctrl Pts',(90.3710057050937,-21.2580751186024,1.840896741602));
#27360=CARTESIAN_POINT('Ctrl Pts',(93.4061868401735,-21.1371049599683,1.68291357635336));
#27361=CARTESIAN_POINT('Ctrl Pts',(95.1657934774511,-23.6136179366278,1.52493041110473));
#27362=CARTESIAN_POINT('Ctrl Pts',(94.0541522279815,-26.4390821629154,1.3669472458561));
#27363=CARTESIAN_POINT('Ctrl Pts',(91.0788510502784,-27.0553104328281,1.20896408060746));
#27364=CARTESIAN_POINT('Ctrl Pts',(88.9400485193453,-24.8938904987703,1.05098091535883));
#27365=CARTESIAN_POINT('Ctrl Pts',(89.3645039014938,-22.9233101920371,0.945658805193069));
#27366=CARTESIAN_POINT('Ctrl Pts',(89.9456684496579,-22.2435746787732,0.89299775011019));
#27367=CARTESIAN_POINT('Ctrl Pts',(91.3498000020249,-26.4320868020351,10.3210067496694));
#27368=CARTESIAN_POINT('Ctrl Pts',(90.5450731455404,-26.2169491679593,10.2683456945866));
#27369=CARTESIAN_POINT('Ctrl Pts',(89.1795846992432,-24.9282879190241,10.1630235844208));
#27370=CARTESIAN_POINT('Ctrl Pts',(89.6809486513065,-22.1407630412207,10.0050404191722));
#27371=CARTESIAN_POINT('Ctrl Pts',(92.2898921909823,-21.0440050172257,9.84705725392353));
#27372=CARTESIAN_POINT('Ctrl Pts',(94.6338971484091,-22.6263097248287,9.68907408867489));
#27373=CARTESIAN_POINT('Ctrl Pts',(94.5898446877876,-25.4556339171384,9.53109092342626));
#27374=CARTESIAN_POINT('Ctrl Pts',(92.1962361738095,-26.9641414313917,9.37310775817763));
#27375=CARTESIAN_POINT('Ctrl Pts',(89.6248691149327,-25.7843198036745,9.21512459292898));
#27376=CARTESIAN_POINT('Ctrl Pts',(89.207712054242,-22.985937598543,9.05714142768036));
#27377=CARTESIAN_POINT('Ctrl Pts',(91.3233116839909,-21.1074041655496,8.89915826243172));
#27378=CARTESIAN_POINT('Ctrl Pts',(94.052663180014,-21.8525247134472,8.74117509718308));
#27379=CARTESIAN_POINT('Ctrl Pts',(94.9201925948099,-24.5454929314001,8.58319193193446));
#27380=CARTESIAN_POINT('Ctrl Pts',(93.1390010492492,-26.7436734443214,8.42520876668581));
#27381=CARTESIAN_POINT('Ctrl Pts',(90.3246999101047,-26.4532519228875,8.26722560143719));
#27382=CARTESIAN_POINT('Ctrl Pts',(89.0299515498622,-23.9376454941666,8.10924243618855));
#27383=CARTESIAN_POINT('Ctrl Pts',(90.4291392839118,-21.4785975525943,7.95125927093992));
#27384=CARTESIAN_POINT('Ctrl Pts',(93.2531509242885,-21.3065472890693,7.79327610569128));
#27385=CARTESIAN_POINT('Ctrl Pts',(94.9405120897237,-23.5775507648634,7.63529294044265));
#27386=CARTESIAN_POINT('Ctrl Pts',(93.9607283326452,-26.2317300194472,7.47730977519401));
#27387=CARTESIAN_POINT('Ctrl Pts',(91.2024970986403,-26.8616540199631,7.31932660994538));
#27388=CARTESIAN_POINT('Ctrl Pts',(89.167628194787,-24.8959601268202,7.16134344469675));
#27389=CARTESIAN_POINT('Ctrl Pts',(89.7018172038921,-22.1175998289577,7.00336027944811));
#27390=CARTESIAN_POINT('Ctrl Pts',(92.3205364457276,-21.0466407310267,6.84537711419948));
#27391=CARTESIAN_POINT('Ctrl Pts',(94.6485181932608,-22.6544792972589,6.68739394895083));
#27392=CARTESIAN_POINT('Ctrl Pts',(94.574203538645,-25.4827510650502,6.52941078370221));
#27393=CARTESIAN_POINT('Ctrl Pts',(92.1649984120093,-26.9661170080217,6.37142761845357));
#27394=CARTESIAN_POINT('Ctrl Pts',(89.6061340936301,-25.7591135844653,6.21344445320494));
#27395=CARTESIAN_POINT('Ctrl Pts',(89.2185878602508,-22.9565340976394,6.0554612879563));
#27396=CARTESIAN_POINT('Ctrl Pts',(91.353877373111,-21.1004137999029,5.89747812270767));
#27397=CARTESIAN_POINT('Ctrl Pts',(94.0752221621442,-21.8743171547908,5.73949495745903));
#27398=CARTESIAN_POINT('Ctrl Pts',(94.9142696183164,-24.576287404365,5.5815117922104));
#27399=CARTESIAN_POINT('Ctrl Pts',(93.1099750604108,-26.7555453082897,5.42352862696177));
#27400=CARTESIAN_POINT('Ctrl Pts',(90.2988952368883,-26.4354295648718,5.26554546171313));
#27401=CARTESIAN_POINT('Ctrl Pts',(89.0307754958461,-23.9062960797898,5.10756229646449));
#27402=CARTESIAN_POINT('Ctrl Pts',(90.4558437261009,-21.4621552484402,4.94957913121587));
#27403=CARTESIAN_POINT('Ctrl Pts',(93.2815144020789,-21.319926229272,4.79159596596723));
#27404=CARTESIAN_POINT('Ctrl Pts',(94.9448077746754,-23.6086155959297,4.6336128007186));
#27405=CARTESIAN_POINT('Ctrl Pts',(93.9370599827578,-26.2523039776791,4.47562963546996));
#27406=CARTESIAN_POINT('Ctrl Pts',(91.1723326710444,-26.8530757720127,4.31764647022133));
#27407=CARTESIAN_POINT('Ctrl Pts',(89.1583278755794,-24.8660104670891,4.15966330497269));
#27408=CARTESIAN_POINT('Ctrl Pts',(89.7218166917233,-22.0934440943058,4.00168013972406));
#27409=CARTESIAN_POINT('Ctrl Pts',(92.3516955228573,-21.0501890343038,3.84369697447542));
#27410=CARTESIAN_POINT('Ctrl Pts',(94.6625745206359,-22.6825131392915,3.68571380922679));
#27411=CARTESIAN_POINT('Ctrl Pts',(94.5584075284074,-25.5098429268151,3.52773064397815));
#27412=CARTESIAN_POINT('Ctrl Pts',(92.1336776256617,-26.9676933776133,3.36974747872952));
#27413=CARTESIAN_POINT('Ctrl Pts',(89.5876974686318,-25.7337451882325,3.21176431348088));
#27414=CARTESIAN_POINT('Ctrl Pts',(89.2297582183761,-22.9272298197195,3.05378114823225));
#27415=CARTESIAN_POINT('Ctrl Pts',(91.384522463549,-21.0937559012723,2.89579798298361));
#27416=CARTESIAN_POINT('Ctrl Pts',(94.0975465662658,-21.8963399202019,2.73781481773498));
#27417=CARTESIAN_POINT('Ctrl Pts',(94.9080228605173,-24.6070249415381,2.57983165248635));
#27418=CARTESIAN_POINT('Ctrl Pts',(93.0808261832357,-26.7670982093405,2.42184848723771));
#27419=CARTESIAN_POINT('Ctrl Pts',(90.273277100628,-26.4173585904575,2.26386532198908));
#27420=CARTESIAN_POINT('Ctrl Pts',(89.0319372146034,-23.8749112917619,2.10588215674044));
#27421=CARTESIAN_POINT('Ctrl Pts',(90.4827058750349,-21.4460889601337,1.94789899149181));
#27422=CARTESIAN_POINT('Ctrl Pts',(93.3097645816624,-21.3334137275896,1.78991582624317));
#27423=CARTESIAN_POINT('Ctrl Pts',(94.9487149581859,-23.6401121620991,1.63193266099454));
#27424=CARTESIAN_POINT('Ctrl Pts',(93.9132989704421,-26.2718342523794,1.47394949574591));
#27425=CARTESIAN_POINT('Ctrl Pts',(91.1420142513693,-26.8458077380446,1.31596633049727));
#27426=CARTESIAN_POINT('Ctrl Pts',(89.149869450867,-24.8325964101823,1.15798316524864));
#27427=CARTESIAN_POINT('Ctrl Pts',(89.5452199193478,-22.9971388327508,1.05266105508288));
#27428=CARTESIAN_POINT('Ctrl Pts',(90.0865340033349,-22.3640127966251,1.));
#27429=CARTESIAN_POINT('Ctrl Pts',(89.4850512338518,-23.9982506073194,9.11258330249198));
#27430=CARTESIAN_POINT('Ctrl Pts',(89.4831441979475,-23.7052247997765,9.09410267755477));
#27431=CARTESIAN_POINT('Ctrl Pts',(89.5304975843651,-23.4127948855722,9.07562205261757));
#27432=CARTESIAN_POINT('Ctrl Pts',(89.6298381693152,-23.1392457272327,9.05714142768036));
#27433=CARTESIAN_POINT('Ctrl Pts',(89.9129119308249,-22.3597597875452,9.00448037259748));
#27434=CARTESIAN_POINT('Ctrl Pts',(90.6181118074079,-21.7335819765474,8.9518193175146));
#27435=CARTESIAN_POINT('Ctrl Pts',(91.4256036617033,-21.5446798290314,8.89915826243172));
#27436=CARTESIAN_POINT('Ctrl Pts',(92.2330955159986,-21.3557776815155,8.84649720734885));
#27437=CARTESIAN_POINT('Ctrl Pts',(93.1428793480063,-21.6041511974813,8.79383615226596));
#27438=CARTESIAN_POINT('Ctrl Pts',(93.7423594998095,-22.1771659917897,8.74117509718309));
#27439=CARTESIAN_POINT('Ctrl Pts',(94.3418396516127,-22.7501807860982,8.68851404210021));
#27440=CARTESIAN_POINT('Ctrl Pts',(94.6310161232113,-23.6478368587491,8.63585298701733));
#27441=CARTESIAN_POINT('Ctrl Pts',(94.4787391014172,-24.4630283138948,8.58319193193445));
#27442=CARTESIAN_POINT('Ctrl Pts',(94.326462079623,-25.2782197690405,8.53053087685158));
#27443=CARTESIAN_POINT('Ctrl Pts',(93.7327315644362,-26.0109466066809,8.4778698217687));
#27444=CARTESIAN_POINT('Ctrl Pts',(92.9668161169853,-26.3289064385955,8.42520876668582));
#27445=CARTESIAN_POINT('Ctrl Pts',(92.2009006695344,-26.6468662705101,8.37254771160294));
#27446=CARTESIAN_POINT('Ctrl Pts',(91.2628002898196,-26.5500590966988,8.31988665652006));
#27447=CARTESIAN_POINT('Ctrl Pts',(90.5779587065884,-26.082387771673,8.26722560143718));
#27448=CARTESIAN_POINT('Ctrl Pts',(89.907599452313,-25.624606281228,8.21567816845545));
#27449=CARTESIAN_POINT('Ctrl Pts',(89.4799009347916,-24.8114801021923,8.16413073547372));
#27450=CARTESIAN_POINT('Ctrl Pts',(89.4784371162896,-23.999680408535,8.11258330249198));
#27451=CARTESIAN_POINT('Ctrl Pts',(91.2062007174671,-26.9692229537457,10.));
#27452=CARTESIAN_POINT('Ctrl Pts',(91.1131474716668,-26.9351836607658,10.));
#27453=CARTESIAN_POINT('Ctrl Pts',(91.0221595031901,-26.8963760597068,10.));
#27454=CARTESIAN_POINT('Ctrl Pts',(90.9334453118182,-26.8531283773235,10.));
#27455=CARTESIAN_POINT('Ctrl Pts',(90.8427654821472,-26.8089224570357,10.));
#27456=CARTESIAN_POINT('Ctrl Pts',(90.7544606379728,-26.7600769016029,10.));
#27457=CARTESIAN_POINT('Ctrl Pts',(90.668782366846,-26.7068967029855,10.));
#27458=CARTESIAN_POINT('Ctrl Pts',(90.5863298883847,-26.6557187424198,10.));
#27459=CARTESIAN_POINT('Ctrl Pts',(90.5063096394357,-26.6005255181573,10.));
#27460=CARTESIAN_POINT('Ctrl Pts',(90.4289788439406,-26.5415587834304,10.));
#27461=CARTESIAN_POINT('Ctrl Pts',(90.3613143978823,-26.4899628905444,10.));
#27462=CARTESIAN_POINT('Ctrl Pts',(90.2957093551107,-26.435477205689,10.));
#27463=CARTESIAN_POINT('Ctrl Pts',(90.2323606826138,-26.3782509736031,10.));
#27464=CARTESIAN_POINT('Ctrl Pts',(90.2182619575677,-26.3655148438658,10.));
#27465=CARTESIAN_POINT('Ctrl Pts',(90.2042723901541,-26.3526402704889,10.));
#27466=CARTESIAN_POINT('Ctrl Pts',(90.190413624506,-26.339647326439,10.));
#27467=CARTESIAN_POINT('Ctrl Pts',(90.117982895404,-26.2717416821266,10.));
#27468=CARTESIAN_POINT('Ctrl Pts',(90.0490178395273,-26.2005142871037,10.));
#27469=CARTESIAN_POINT('Ctrl Pts',(89.9837584040089,-26.1262557408025,10.));
#27470=CARTESIAN_POINT('Ctrl Pts',(89.9188586588048,-26.0524064851986,10.));
#27471=CARTESIAN_POINT('Ctrl Pts',(89.8576233116514,-25.9755586030621,10.));
#27472=CARTESIAN_POINT('Ctrl Pts',(89.8003319724653,-25.8959711475448,10.));
#27473=CARTESIAN_POINT('Ctrl Pts',(89.7451391407445,-25.8192988773226,10.));
#27474=CARTESIAN_POINT('Ctrl Pts',(89.6936065132557,-25.7400833150341,10.));
#27475=CARTESIAN_POINT('Ctrl Pts',(89.6460290163529,-25.6585424655959,10.));
#27476=CARTESIAN_POINT('Ctrl Pts',(89.626040255569,-25.6242846622301,10.));
#27477=CARTESIAN_POINT('Ctrl Pts',(89.6067501857345,-25.5896163159409,10.));
#27478=CARTESIAN_POINT('Ctrl Pts',(89.5881832814499,-25.5545532938095,10.));
#27479=CARTESIAN_POINT('Ctrl Pts',(89.5751467282293,-25.529934167913,10.));
#27480=CARTESIAN_POINT('Ctrl Pts',(89.5624667280368,-25.505120464169,10.));
#27481=CARTESIAN_POINT('Ctrl Pts',(89.5501522393051,-25.4801176691506,10.));
#27482=CARTESIAN_POINT('Ctrl Pts',(89.5423997338152,-25.4643773237844,10.));
#27483=CARTESIAN_POINT('Ctrl Pts',(89.5347912129438,-25.4485599130764,10.));
#27484=CARTESIAN_POINT('Ctrl Pts',(89.5273385775824,-25.4326879328603,10.));
#27485=CARTESIAN_POINT('Ctrl Pts',(89.4852180064675,-25.3429831721955,10.));
#27486=CARTESIAN_POINT('Ctrl Pts',(89.4479996497494,-25.2513937089187,10.));
#27487=CARTESIAN_POINT('Ctrl Pts',(89.4159751546784,-25.1581920045764,10.));
#27488=CARTESIAN_POINT('Ctrl Pts',(89.3861126932969,-25.0712825219929,10.));
#27489=CARTESIAN_POINT('Ctrl Pts',(89.3607666485969,-24.9829703487333,10.));
#27490=CARTESIAN_POINT('Ctrl Pts',(89.3402240440734,-24.8934677198076,10.));
#27491=CARTESIAN_POINT('Ctrl Pts',(89.3387367653631,-24.8869877549932,10.));
#27492=CARTESIAN_POINT('Ctrl Pts',(89.337274687697,-24.8805015489785,10.));
#27493=CARTESIAN_POINT('Ctrl Pts',(89.335837930805,-24.874009181989,10.));
#27494=CARTESIAN_POINT('Ctrl Pts',(89.315252334091,-24.7809877047218,10.));
#27495=CARTESIAN_POINT('Ctrl Pts',(89.2998605243042,-24.6867004764278,10.));
#27496=CARTESIAN_POINT('Ctrl Pts',(89.2895854935825,-24.5915555250827,10.));
#27497=CARTESIAN_POINT('Ctrl Pts',(89.2837678665547,-24.5376853367106,10.));
#27498=CARTESIAN_POINT('Ctrl Pts',(89.279591470324,-24.4835403753464,10.));
#27499=CARTESIAN_POINT('Ctrl Pts',(89.2770492198354,-24.4291973958018,10.));
#27500=CARTESIAN_POINT('Ctrl Pts',(89.2764018813574,-24.4153599309944,10.));
#27501=CARTESIAN_POINT('Ctrl Pts',(89.2758606481526,-24.4015110330491,10.));
#27502=CARTESIAN_POINT('Ctrl Pts',(89.2754255840287,-24.3876642045987,10.));
#27503=CARTESIAN_POINT('Ctrl Pts',(89.2724967852974,-24.2944490407395,10.));
#27504=CARTESIAN_POINT('Ctrl Pts',(89.2743673782132,-24.2011765909983,10.));
#27505=CARTESIAN_POINT('Ctrl Pts',(89.2809024940859,-24.1082221294119,10.));
#27506=CARTESIAN_POINT('Ctrl Pts',(89.287448047592,-24.0151192045669,10.));
#27507=CARTESIAN_POINT('Ctrl Pts',(89.2986734147484,-23.9223343048006,10.));
#27508=CARTESIAN_POINT('Ctrl Pts',(89.3144939864412,-23.8302566591467,10.));
#27509=CARTESIAN_POINT('Ctrl Pts',(89.3300873891373,-23.7395011646005,10.));
#27510=CARTESIAN_POINT('Ctrl Pts',(89.3501454394382,-23.649431915389,10.));
#27511=CARTESIAN_POINT('Ctrl Pts',(89.3746301066029,-23.5604468626945,10.));
#27512=CARTESIAN_POINT('Ctrl Pts',(89.3838721758798,-23.5268582492132,10.));
#27513=CARTESIAN_POINT('Ctrl Pts',(89.3937453511447,-23.4934244350543,10.));
#27514=CARTESIAN_POINT('Ctrl Pts',(89.4042490107015,-23.4601681503182,10.));
#27515=CARTESIAN_POINT('Ctrl Pts',(89.4119449034304,-23.4358017094118,10.));
#27516=CARTESIAN_POINT('Ctrl Pts',(89.4199792749368,-23.4115305873094,10.));
#27517=CARTESIAN_POINT('Ctrl Pts',(89.4283521276576,-23.3873640207246,10.));
#27518=CARTESIAN_POINT('Ctrl Pts',(89.4335196879868,-23.3724488902498,10.));
#27519=CARTESIAN_POINT('Ctrl Pts',(89.4388131892276,-23.3575822733592,10.));
#27520=CARTESIAN_POINT('Ctrl Pts',(89.4442314440759,-23.3427682606429,10.));
#27521=CARTESIAN_POINT('Ctrl Pts',(89.4759375039964,-23.2560809437852,10.));
#27522=CARTESIAN_POINT('Ctrl Pts',(89.511920335114,-23.1711677991127,10.));
#27523=CARTESIAN_POINT('Ctrl Pts',(89.5521196351583,-23.0884296536704,10.));
#27524=CARTESIAN_POINT('Ctrl Pts',(89.5822691101916,-23.0263760445887,10.));
#27525=CARTESIAN_POINT('Ctrl Pts',(89.6147913381275,-22.9655463574365,10.));
#27526=CARTESIAN_POINT('Ctrl Pts',(89.6496759688728,-22.9061246870224,10.));
#27527=CARTESIAN_POINT('Ctrl Pts',(89.6654548106757,-22.8792473740884,10.));
#27528=CARTESIAN_POINT('Ctrl Pts',(89.6817171385687,-22.8526583245227,10.));
#27529=CARTESIAN_POINT('Ctrl Pts',(89.6984627751052,-22.8263756432691,10.));
#27530=CARTESIAN_POINT('Ctrl Pts',(89.7075848157606,-22.8120583799984,10.));
#27531=CARTESIAN_POINT('Ctrl Pts',(89.7168450962946,-22.7978401889566,10.));
#27532=CARTESIAN_POINT('Ctrl Pts',(89.726242936913,-22.7837240829482,10.));
#27533=CARTESIAN_POINT('Ctrl Pts',(89.7738179917087,-22.7122635693982,10.));
#27534=CARTESIAN_POINT('Ctrl Pts',(89.8249182481167,-22.6434123197201,10.));
#27535=CARTESIAN_POINT('Ctrl Pts',(89.8795126484078,-22.577523824193,10.));
#27536=CARTESIAN_POINT('Ctrl Pts',(89.9256431731806,-22.5218501496231,10.));
#27537=CARTESIAN_POINT('Ctrl Pts',(89.974269092162,-22.4682921528781,10.));
#27538=CARTESIAN_POINT('Ctrl Pts',(90.0253879613002,-22.4170872144436,10.));
#27539=CARTESIAN_POINT('Ctrl Pts',(90.0442197521512,-22.3982237163382,10.));
#27540=CARTESIAN_POINT('Ctrl Pts',(90.0633900127449,-22.3796798067826,10.));
#27541=CARTESIAN_POINT('Ctrl Pts',(90.0828885913555,-22.3614597865289,10.));
#27542=CARTESIAN_POINT('Origin',(92.,-24.,5.));
#27543=CARTESIAN_POINT('Origin',(-24.,-92.,1.));
#27544=CARTESIAN_POINT('Ctrl Pts',(-25.913465996665,-90.364012796625,0.999999999999996));
#27545=CARTESIAN_POINT('Ctrl Pts',(-25.9756062673146,-90.4224093923451,
0.999999999999996));
#27546=CARTESIAN_POINT('Ctrl Pts',(-26.034371236743,-90.4840596836494,0.999999999999993));
#27547=CARTESIAN_POINT('Ctrl Pts',(-26.089748867249,-90.5485872413642,0.999999999999997));
#27548=CARTESIAN_POINT('Ctrl Pts',(-26.1464812232126,-90.6146933629207,
1.));
#27549=CARTESIAN_POINT('Ctrl Pts',(-26.1996589497415,-90.6838197394388,
1.));
#27550=CARTESIAN_POINT('Ctrl Pts',(-26.2492402162037,-90.7556079093069,
1.));
#27551=CARTESIAN_POINT('Ctrl Pts',(-26.2621838799929,-90.77434889761,1.));
#27552=CARTESIAN_POINT('Ctrl Pts',(-26.2748822665281,-90.7932715095309,
1.));
#27553=CARTESIAN_POINT('Ctrl Pts',(-26.287334255627,-90.8123698011315,1.));
#27554=CARTESIAN_POINT('Ctrl Pts',(-26.29749533292,-90.8279543969398,1.));
#27555=CARTESIAN_POINT('Ctrl Pts',(-26.3074927699566,-90.8436568716418,
1.));
#27556=CARTESIAN_POINT('Ctrl Pts',(-26.3173171311148,-90.8594594346009,
1.));
#27557=CARTESIAN_POINT('Ctrl Pts',(-26.3647643834219,-90.9357787168166,
1.));
#27558=CARTESIAN_POINT('Ctrl Pts',(-26.4082280607616,-91.014505223999,1.00000000000001));
#27559=CARTESIAN_POINT('Ctrl Pts',(-26.4476734128481,-91.0952464686478,
1.00000000000001));
#27560=CARTESIAN_POINT('Ctrl Pts',(-26.479514252443,-91.1604219299776,1.00000000000001));
#27561=CARTESIAN_POINT('Ctrl Pts',(-26.5087362738458,-91.2269112715432,
1.));
#27562=CARTESIAN_POINT('Ctrl Pts',(-26.5353040214271,-91.2945258795828,
1.));
#27563=CARTESIAN_POINT('Ctrl Pts',(-26.5460285866473,-91.3218197731108,
1.));
#27564=CARTESIAN_POINT('Ctrl Pts',(-26.5563204553652,-91.3492971819707,
1.));
#27565=CARTESIAN_POINT('Ctrl Pts',(-26.5661765051131,-91.3769462663626,
1.));
#27566=CARTESIAN_POINT('Ctrl Pts',(-26.5713946913052,-91.391584795397,1.));
#27567=CARTESIAN_POINT('Ctrl Pts',(-26.5764901577044,-91.4062701187452,
1.00000000000001));
#27568=CARTESIAN_POINT('Ctrl Pts',(-26.5814586838643,-91.4209886610266,
1.00000000000001));
#27569=CARTESIAN_POINT('Ctrl Pts',(-26.6109727393212,-91.5084197943558,
1.00000000000001));
#27570=CARTESIAN_POINT('Ctrl Pts',(-26.6360505229659,-91.5971308115395,
1.));
#27571=CARTESIAN_POINT('Ctrl Pts',(-26.6566592692921,-91.6867240182697,
1.));
#27572=CARTESIAN_POINT('Ctrl Pts',(-26.6775869543672,-91.7777037598634,
1.));
#27573=CARTESIAN_POINT('Ctrl Pts',(-26.6939067073515,-91.8695940137173,
1.00000000000001));
#27574=CARTESIAN_POINT('Ctrl Pts',(-26.7055423733552,-91.9620114717871,
1.00000000000001));
#27575=CARTESIAN_POINT('Ctrl Pts',(-26.7170868810523,-92.0537048957565,
1.00000000000001));
#27576=CARTESIAN_POINT('Ctrl Pts',(-26.724020751965,-92.1459182254205,1.));
#27577=CARTESIAN_POINT('Ctrl Pts',(-26.7262226527309,-92.2382962505423,
1.));
#27578=CARTESIAN_POINT('Ctrl Pts',(-26.7273178683138,-92.2842446666544,
1.));
#27579=CARTESIAN_POINT('Ctrl Pts',(-26.7272416203271,-92.3302340409407,
1.));
#27580=CARTESIAN_POINT('Ctrl Pts',(-26.7259741877374,-92.3762213556111,
1.));
#27581=CARTESIAN_POINT('Ctrl Pts',(-26.7255574259114,-92.3913430728443,
1.));
#27582=CARTESIAN_POINT('Ctrl Pts',(-26.7250117562314,-92.4064664174684,
1.00000000000001));
#27583=CARTESIAN_POINT('Ctrl Pts',(-26.7243366619654,-92.4215840384697,
1.00000000000001));
#27584=CARTESIAN_POINT('Ctrl Pts',(-26.7200628111856,-92.5172898673486,
1.00000000000001));
#27585=CARTESIAN_POINT('Ctrl Pts',(-26.7106219303704,-92.6124285203872,
1.));
#27586=CARTESIAN_POINT('Ctrl Pts',(-26.6959498489085,-92.7066016678489,
1.));
#27587=CARTESIAN_POINT('Ctrl Pts',(-26.6917951398295,-92.7332687792454,
1.));
#27588=CARTESIAN_POINT('Ctrl Pts',(-26.6872206693378,-92.7598586005847,
1.00000000000001));
#27589=CARTESIAN_POINT('Ctrl Pts',(-26.682224266105,-92.7863623464052,1.));
#27590=CARTESIAN_POINT('Ctrl Pts',(-26.6652593323816,-92.8763539404211,
1.));
#27591=CARTESIAN_POINT('Ctrl Pts',(-26.6434341104625,-92.9653530573532,
1.));
#27592=CARTESIAN_POINT('Ctrl Pts',(-26.617051236812,-93.0531274604727,1.));
#27593=CARTESIAN_POINT('Ctrl Pts',(-26.5900718918307,-93.1428862916619,
1.));
#27594=CARTESIAN_POINT('Ctrl Pts',(-26.5583262747371,-93.2313651060399,
1.));
#27595=CARTESIAN_POINT('Ctrl Pts',(-26.5220837746486,-93.3183118483727,
1.));
#27596=CARTESIAN_POINT('Ctrl Pts',(-26.5094168709692,-93.3487000944288,
1.));
#27597=CARTESIAN_POINT('Ctrl Pts',(-26.496200198248,-93.3789011100651,1.00000000000001));
#27598=CARTESIAN_POINT('Ctrl Pts',(-26.4824438244401,-93.4089037784374,
1.00000000000001));
#27599=CARTESIAN_POINT('Ctrl Pts',(-26.4754968109029,-93.424055223596,1.00000000000001));
#27600=CARTESIAN_POINT('Ctrl Pts',(-26.4684121470773,-93.4391560808108,
1.00000000000001));
#27601=CARTESIAN_POINT('Ctrl Pts',(-26.4611910622915,-93.4542048926094,
1.00000000000001));
#27602=CARTESIAN_POINT('Ctrl Pts',(-26.4551808929969,-93.4667301446008,
1.00000000000001));
#27603=CARTESIAN_POINT('Ctrl Pts',(-26.4490780639285,-93.479215407299,1.00000000000001));
#27604=CARTESIAN_POINT('Ctrl Pts',(-26.4428871735715,-93.4916526560001,
1.00000000000001));
#27605=CARTESIAN_POINT('Ctrl Pts',(-26.3999238163837,-93.5779643054661,
1.00000000000001));
#27606=CARTESIAN_POINT('Ctrl Pts',(-26.3526734208407,-93.6620692716443,
0.999999999999998));
#27607=CARTESIAN_POINT('Ctrl Pts',(-26.3014780532023,-93.7437174767272,
0.999999999999999));
#27608=CARTESIAN_POINT('Ctrl Pts',(-26.2492778937103,-93.8269681598294,
1.));
#27609=CARTESIAN_POINT('Ctrl Pts',(-26.1929760723445,-93.9076654736707,
1.));
#27610=CARTESIAN_POINT('Ctrl Pts',(-26.1328802773408,-93.9855370025748,
1.));
#27611=CARTESIAN_POINT('Ctrl Pts',(-26.0723164767454,-94.0640149684343,
1.));
#27612=CARTESIAN_POINT('Ctrl Pts',(-26.0078989173972,-94.1396238025829,
1.));
#27613=CARTESIAN_POINT('Ctrl Pts',(-25.9398933828955,-94.2120650883093,
1.));
#27614=CARTESIAN_POINT('Ctrl Pts',(-25.9029668417263,-94.2514002121243,
1.));
#27615=CARTESIAN_POINT('Ctrl Pts',(-25.8649816080713,-94.2898009986756,
1.));
#27616=CARTESIAN_POINT('Ctrl Pts',(-25.8259749927721,-94.3272159154238,
1.));
#27617=CARTESIAN_POINT('Ctrl Pts',(-25.8138410599859,-94.3388547126263,
1.));
#27618=CARTESIAN_POINT('Ctrl Pts',(-25.8016082666696,-94.3503980875446,
1.));
#27619=CARTESIAN_POINT('Ctrl Pts',(-25.7892776711008,-94.3618444242613,
1.));
#27620=CARTESIAN_POINT('Ctrl Pts',(-25.7779940533511,-94.3723188646422,
1.));
#27621=CARTESIAN_POINT('Ctrl Pts',(-25.7666342742199,-94.382706679586,0.999999999999998));
#27622=CARTESIAN_POINT('Ctrl Pts',(-25.7552037476042,-94.3930030340632,
0.999999999999998));
#27623=CARTESIAN_POINT('Ctrl Pts',(-25.6793946851099,-94.4612900873433,
0.999999999999999));
#27624=CARTESIAN_POINT('Ctrl Pts',(-25.6004193338813,-94.5256101174112,
1.));
#27625=CARTESIAN_POINT('Ctrl Pts',(-25.5186038566385,-94.585680500128,1.));
#27626=CARTESIAN_POINT('Ctrl Pts',(-25.4367174576773,-94.6458029548355,
1.));
#27627=CARTESIAN_POINT('Ctrl Pts',(-25.351985429782,-94.7016692285508,1.));
#27628=CARTESIAN_POINT('Ctrl Pts',(-25.2646898214108,-94.7529697581317,
1.));
#27629=CARTESIAN_POINT('Ctrl Pts',(-25.1791579833755,-94.8032337825095,
0.999999999999999));
#27630=CARTESIAN_POINT('Ctrl Pts',(-25.0911644460643,-94.8491153707221,
1.));
#27631=CARTESIAN_POINT('Ctrl Pts',(-25.0009407551715,-94.8902872128736,
1.00000000000001));
#27632=CARTESIAN_POINT('Ctrl Pts',(-24.9631517387227,-94.9075315020941,
1.00000000000001));
#27633=CARTESIAN_POINT('Ctrl Pts',(-24.9249711429332,-94.923949087781,1.));
#27634=CARTESIAN_POINT('Ctrl Pts',(-24.8864145873395,-94.9395135460182,
1.));
#27635=CARTESIAN_POINT('Ctrl Pts',(-24.8564008951788,-94.9516294326939,
1.));
#27636=CARTESIAN_POINT('Ctrl Pts',(-24.8261593691065,-94.9632283272653,
1.));
#27637=CARTESIAN_POINT('Ctrl Pts',(-24.7957017813267,-94.9743128096467,
1.));
#27638=CARTESIAN_POINT('Ctrl Pts',(-23.2062007174672,-94.9692229537457,
0.999999999999999));
#27639=CARTESIAN_POINT('Ctrl Pts',(-23.1113643951015,-94.9345314033933,
0.999999999999999));
#27640=CARTESIAN_POINT('Ctrl Pts',(-23.0185713035646,-94.8948494397886,
0.999999999999999));
#27641=CARTESIAN_POINT('Ctrl Pts',(-22.9280623762531,-94.8504973089186,
1.));
#27642=CARTESIAN_POINT('Ctrl Pts',(-22.8362819518079,-94.8055221057291,
1.));
#27643=CARTESIAN_POINT('Ctrl Pts',(-22.7468496512481,-94.7557438960029,
1.));
#27644=CARTESIAN_POINT('Ctrl Pts',(-22.6600507311628,-94.7014559325677,
1.));
#27645=CARTESIAN_POINT('Ctrl Pts',(-22.6355419727356,-94.6861270485212,
1.));
#27646=CARTESIAN_POINT('Ctrl Pts',(-22.6112434098515,-94.67043839863,1.));
#27647=CARTESIAN_POINT('Ctrl Pts',(-22.587162060266,-94.6543961292366,1.));
#27648=CARTESIAN_POINT('Ctrl Pts',(-22.5678313680127,-94.641518604595,1.));
#27649=CARTESIAN_POINT('Ctrl Pts',(-22.5486385356581,-94.6284115926912,
1.));
#27650=CARTESIAN_POINT('Ctrl Pts',(-22.5296064818783,-94.6150920387402,
1.));
#27651=CARTESIAN_POINT('Ctrl Pts',(-22.4468988465926,-94.5572092257188,
1.));
#27652=CARTESIAN_POINT('Ctrl Pts',(-22.3671460458253,-94.4952646292979,
1.));
#27653=CARTESIAN_POINT('Ctrl Pts',(-22.2906144353731,-94.4295554855911,
1.));
#27654=CARTESIAN_POINT('Ctrl Pts',(-22.2316015869558,-94.3788877456299,
1.));
#27655=CARTESIAN_POINT('Ctrl Pts',(-22.174504633498,-94.3259807640076,1.));
#27656=CARTESIAN_POINT('Ctrl Pts',(-22.1194632793834,-94.270959034197,1.));
#27657=CARTESIAN_POINT('Ctrl Pts',(-22.0901431561929,-94.2416493647283,
1.));
#27658=CARTESIAN_POINT('Ctrl Pts',(-22.0614066098028,-94.2117394621323,
1.));
#27659=CARTESIAN_POINT('Ctrl Pts',(-22.0332767871003,-94.181247310107,1.));
#27660=CARTESIAN_POINT('Ctrl Pts',(-22.0236428018515,-94.1708042672935,
1.));
#27661=CARTESIAN_POINT('Ctrl Pts',(-22.014080781236,-94.1602937100153,1.));
#27662=CARTESIAN_POINT('Ctrl Pts',(-22.0045982120006,-94.1497238888402,
1.));
#27663=CARTESIAN_POINT('Ctrl Pts',(-21.9388057221636,-94.0763877670595,
1.));
#27664=CARTESIAN_POINT('Ctrl Pts',(-21.8767454820535,-94.0001052969862,
0.999999999999998));
#27665=CARTESIAN_POINT('Ctrl Pts',(-21.8186612829854,-93.9211548960136,
0.999999999999999));
#27666=CARTESIAN_POINT('Ctrl Pts',(-21.7610834895644,-93.8428928221512,
0.999999999999999));
#27667=CARTESIAN_POINT('Ctrl Pts',(-21.7074122723325,-93.7620083511859,
0.999999999999998));
#27668=CARTESIAN_POINT('Ctrl Pts',(-21.6579309059598,-93.6787502765599,
0.999999999999997));
#27669=CARTESIAN_POINT('Ctrl Pts',(-21.609882526023,-93.5979033659812,0.999999999999997));
#27670=CARTESIAN_POINT('Ctrl Pts',(-21.5657846284247,-93.5148176409593,
1.));
#27671=CARTESIAN_POINT('Ctrl Pts',(-21.5259443770376,-93.4297105806012,
1.));
#27672=CARTESIAN_POINT('Ctrl Pts',(-21.5051331098544,-93.3852533869181,
1.));
#27673=CARTESIAN_POINT('Ctrl Pts',(-21.4854844375003,-93.3402445256234,
1.));
#27674=CARTESIAN_POINT('Ctrl Pts',(-21.4670478470219,-93.2947147599259,
1.));
#27675=CARTESIAN_POINT('Ctrl Pts',(-21.4599071766554,-93.2770806399357,
1.));
#27676=CARTESIAN_POINT('Ctrl Pts',(-21.452948372869,-93.259368380918,1.));
#27677=CARTESIAN_POINT('Ctrl Pts',(-21.4461744794312,-93.2415797793335,
1.));
#27678=CARTESIAN_POINT('Ctrl Pts',(-21.44102059279,-93.2280454010747,1.));
#27679=CARTESIAN_POINT('Ctrl Pts',(-21.4359737887531,-93.2144667091695,
1.));
#27680=CARTESIAN_POINT('Ctrl Pts',(-21.4310402382862,-93.2008583988899,
1.));
#27681=CARTESIAN_POINT('Ctrl Pts',(-21.3993683884323,-93.1134973061374,
1.));
#27682=CARTESIAN_POINT('Ctrl Pts',(-21.3723052492582,-93.0247752793144,
1.00000000000001));
#27683=CARTESIAN_POINT('Ctrl Pts',(-21.3501021064032,-92.9349157240161,
1.));
#27684=CARTESIAN_POINT('Ctrl Pts',(-21.3450995091274,-92.9146694386377,
1.));
#27685=CARTESIAN_POINT('Ctrl Pts',(-21.3403438331481,-92.8943653670041,
1.));
#27686=CARTESIAN_POINT('Ctrl Pts',(-21.3358383183128,-92.8740060081578,
1.));
#27687=CARTESIAN_POINT('Ctrl Pts',(-21.3154927915296,-92.7820693714265,
1.));
#27688=CARTESIAN_POINT('Ctrl Pts',(-21.300244266593,-92.6890050257244,1.));
#27689=CARTESIAN_POINT('Ctrl Pts',(-21.2899828336258,-92.5952047143721,
1.));
#27690=CARTESIAN_POINT('Ctrl Pts',(-21.2792696952259,-92.4972753393334,
1.));
#27691=CARTESIAN_POINT('Ctrl Pts',(-21.2739923846859,-92.3985425391084,
1.));
#27692=CARTESIAN_POINT('Ctrl Pts',(-21.2740833202269,-92.2994667952251,
1.));
#27693=CARTESIAN_POINT('Ctrl Pts',(-21.2741184401282,-92.2612030942814,
1.));
#27694=CARTESIAN_POINT('Ctrl Pts',(-21.2749548502656,-92.2228884941123,
0.999999999999998));
#27695=CARTESIAN_POINT('Ctrl Pts',(-21.2765907919834,-92.1845506992199,
0.999999999999998));
#27696=CARTESIAN_POINT('Ctrl Pts',(-21.2771783957654,-92.1707803839174,
0.999999999999998));
#27697=CARTESIAN_POINT('Ctrl Pts',(-21.2778691417354,-92.1570088742633,
1.));
#27698=CARTESIAN_POINT('Ctrl Pts',(-21.2786620583866,-92.1432491225241,
1.));
#27699=CARTESIAN_POINT('Ctrl Pts',(-21.2840136676365,-92.050380831051,1.));
#27700=CARTESIAN_POINT('Ctrl Pts',(-21.2940209875981,-91.9578996301337,
1.));
#27701=CARTESIAN_POINT('Ctrl Pts',(-21.3085609609126,-91.8661774191351,
1.));
#27702=CARTESIAN_POINT('Ctrl Pts',(-21.3230638860674,-91.7746889182712,
1.));
#27703=CARTESIAN_POINT('Ctrl Pts',(-21.3420768068504,-91.6839546001225,
0.999999999999999));
#27704=CARTESIAN_POINT('Ctrl Pts',(-21.3655261933471,-91.5943606400854,
1.));
#27705=CARTESIAN_POINT('Ctrl Pts',(-21.3885742799942,-91.506299941598,1.));
#27706=CARTESIAN_POINT('Ctrl Pts',(-21.4159087531981,-91.4193401209881,
0.999999999999999));
#27707=CARTESIAN_POINT('Ctrl Pts',(-21.4475001288737,-91.3338770867914,
0.999999999999999));
#27708=CARTESIAN_POINT('Ctrl Pts',(-21.463362608245,-91.2909648809136,0.999999999999999));
#27709=CARTESIAN_POINT('Ctrl Pts',(-21.480298928196,-91.248430578413,1.));
#27710=CARTESIAN_POINT('Ctrl Pts',(-21.498308744999,-91.2063280780076,1.));
#27711=CARTESIAN_POINT('Ctrl Pts',(-21.5036080596924,-91.1939395900253,
1.));
#27712=CARTESIAN_POINT('Ctrl Pts',(-21.5090003324731,-91.1815885066313,
0.999999999999998));
#27713=CARTESIAN_POINT('Ctrl Pts',(-21.5144855890668,-91.169276249741,0.999999999999998));
#27714=CARTESIAN_POINT('Ctrl Pts',(-21.5200790128479,-91.156721199797,0.999999999999998));
#27715=CARTESIAN_POINT('Ctrl Pts',(-21.5257654437118,-91.1442148112825,
0.999999999999997));
#27716=CARTESIAN_POINT('Ctrl Pts',(-21.5315435926219,-91.1317604192609,
0.999999999999997));
#27717=CARTESIAN_POINT('Ctrl Pts',(-21.5690289713544,-91.0509633319802,
0.999999999999998));
#27718=CARTESIAN_POINT('Ctrl Pts',(-21.6103840526462,-90.9723231042384,
0.999999999999998));
#27719=CARTESIAN_POINT('Ctrl Pts',(-21.6555390130635,-90.8961874418052,
0.999999999999998));
#27720=CARTESIAN_POINT('Ctrl Pts',(-21.6999357871794,-90.8213301553416,
0.999999999999998));
#27721=CARTESIAN_POINT('Ctrl Pts',(-21.7480063603779,-90.7488933636716,
0.999999999999999));
#27722=CARTESIAN_POINT('Ctrl Pts',(-21.7997205682537,-90.6792417325679,
0.999999999999999));
#27723=CARTESIAN_POINT('Ctrl Pts',(-21.8498548287834,-90.6117180642475,
1.));
#27724=CARTESIAN_POINT('Ctrl Pts',(-21.9034139309536,-90.5468115335925,
1.));
#27725=CARTESIAN_POINT('Ctrl Pts',(-21.9603980831221,-90.4848946771838,
1.));
#27726=CARTESIAN_POINT('Ctrl Pts',(-21.98158716959,-90.4618714053732,1.));
#27727=CARTESIAN_POINT('Ctrl Pts',(-22.0032500736797,-90.4392619466834,
1.));
#27728=CARTESIAN_POINT('Ctrl Pts',(-22.0253876448586,-90.417087121357,1.));
#27729=CARTESIAN_POINT('Ctrl Pts',(-22.0442144350809,-90.3982286485253,
1.));
#27730=CARTESIAN_POINT('Ctrl Pts',(-22.0633845524044,-90.3796845518288,
0.999999999999999));
#27731=CARTESIAN_POINT('Ctrl Pts',(-22.0828882653786,-90.3614597476137,
0.999999999999999));
#27732=CARTESIAN_POINT('Origin',(-24.,-92.,12.2084234471775));
#27733=CARTESIAN_POINT('Ctrl Pts',(-27.0767669904684,-91.998062685181,9.70842344717746));
#27734=CARTESIAN_POINT('Ctrl Pts',(-27.0777011675186,-91.8738981078455,
9.70197366100994));
#27735=CARTESIAN_POINT('Ctrl Pts',(-27.0146668802256,-90.7368860788636,
9.64286281975954));
#27736=CARTESIAN_POINT('Ctrl Pts',(-25.5990318095031,-88.7444872358932,
9.53109092342626));
#27737=CARTESIAN_POINT('Ctrl Pts',(-22.1476049582095,-88.8820466605266,
9.37310775817762));
#27738=CARTESIAN_POINT('Ctrl Pts',(-20.3764280027803,-91.847285042836,9.21512459292899));
#27739=CARTESIAN_POINT('Ctrl Pts',(-21.8919230124438,-94.9512424150719,
9.05714142768036));
#27740=CARTESIAN_POINT('Ctrl Pts',(-25.3195312348388,-95.3782236147545,
8.89915826243172));
#27741=CARTESIAN_POINT('Ctrl Pts',(-26.9608441448919,-93.4378981546875,
8.78291893559742));
#27742=CARTESIAN_POINT('Ctrl Pts',(-27.0762794797313,-92.213313773738,8.719340663846));
#27743=CARTESIAN_POINT('Ctrl Pts',(-27.0743676381347,-92.0026790873961,
8.70842344717746));
#27744=CARTESIAN_POINT('Ctrl Pts',(-27.0702887490762,-92.0031018432153,
9.79157655282255));
#27745=CARTESIAN_POINT('Ctrl Pts',(-27.0652853033504,-91.3096184359041,
9.75572892504928));
#27746=CARTESIAN_POINT('Ctrl Pts',(-26.4922441588307,-89.5876431146109,
9.66722024219313));
#27747=CARTESIAN_POINT('Ctrl Pts',(-23.6460838755241,-88.3911593875009,
9.52605050425409));
#27748=CARTESIAN_POINT('Ctrl Pts',(-20.7843953448966,-90.3229252160129,
9.36806733900547));
#27749=CARTESIAN_POINT('Ctrl Pts',(-20.8381771631847,-93.7771164103054,
9.21008417375682));
#27750=CARTESIAN_POINT('Ctrl Pts',(-23.7604241627304,-95.6187849549087,
9.05210100850819));
#27751=CARTESIAN_POINT('Ctrl Pts',(-26.5324624275929,-94.346888962543,8.91259846819677));
#27752=CARTESIAN_POINT('Ctrl Pts',(-27.0660798384141,-92.6595176403423,
8.82575698296822));
#27753=CARTESIAN_POINT('Ctrl Pts',(-27.0703859251749,-91.9978642356407,
8.79157655282255));
#27754=CARTESIAN_POINT('Ctrl Pts',(-22.0865340033349,-90.364012796625,10.));
#27755=CARTESIAN_POINT('Ctrl Pts',(-21.5452199193478,-90.9971388327508,
9.94733894491712));
#27756=CARTESIAN_POINT('Ctrl Pts',(-21.1498731367063,-92.8326003723509,
9.84201683475137));
#27757=CARTESIAN_POINT('Ctrl Pts',(-23.1420127726733,-94.8458067969654,
9.68403366950273));
#27758=CARTESIAN_POINT('Ctrl Pts',(-25.9132999553889,-94.2718355849706,
9.5260505042541));
#27759=CARTESIAN_POINT('Ctrl Pts',(-26.948715185934,-91.6401115468636,9.36806733900547));
#27760=CARTESIAN_POINT('Ctrl Pts',(-25.3097649521471,-89.3334135729173,
9.21008417375683));
#27761=CARTESIAN_POINT('Ctrl Pts',(-22.4827055416601,-89.4460883253215,
9.05210100850819));
#27762=CARTESIAN_POINT('Ctrl Pts',(-21.0319367161215,-91.8749113698844,
8.89411784325956));
#27763=CARTESIAN_POINT('Ctrl Pts',(-22.2732767801618,-94.4173589653306,
8.73613467801093));
#27764=CARTESIAN_POINT('Ctrl Pts',(-25.0808263815541,-94.7670987311353,
8.57815151276229));
#27765=CARTESIAN_POINT('Ctrl Pts',(-26.9080233748187,-92.6070250335036,
8.42016834751366));
#27766=CARTESIAN_POINT('Ctrl Pts',(-26.0975469404961,-89.8963395546467,
8.26218518226502));
#27767=CARTESIAN_POINT('Ctrl Pts',(-23.384522353545,-89.0937553800026,8.10420201701639));
#27768=CARTESIAN_POINT('Ctrl Pts',(-21.2297577260391,-90.9272296313332,
7.94621885176776));
#27769=CARTESIAN_POINT('Ctrl Pts',(-21.5876970395809,-93.733745495277,7.78823568651912));
#27770=CARTESIAN_POINT('Ctrl Pts',(-24.1336776494793,-94.9676939059565,
7.63025252127048));
#27771=CARTESIAN_POINT('Ctrl Pts',(-26.5584079833072,-93.5098431949504,
7.47226935602185));
#27772=CARTESIAN_POINT('Ctrl Pts',(-26.662574994087,-90.6825129051978,7.31428619077321));
#27773=CARTESIAN_POINT('Ctrl Pts',(-24.3516955853902,-89.0501885096969,
7.15630302552458));
#27774=CARTESIAN_POINT('Ctrl Pts',(-21.7218162866321,-90.0934437553397,
6.99831986027595));
#27775=CARTESIAN_POINT('Ctrl Pts',(-21.1583273702903,-92.8660106210542,
6.84033669502731));
#27776=CARTESIAN_POINT('Ctrl Pts',(-23.1723325238739,-94.8530762793412,
6.68235352977868));
#27777=CARTESIAN_POINT('Ctrl Pts',(-25.9370603271938,-94.2523043781638,
6.52437036453004));
#27778=CARTESIAN_POINT('Ctrl Pts',(-26.944808298303,-91.6086155263393,6.36638719928141));
#27779=CARTESIAN_POINT('Ctrl Pts',(-25.2815146299499,-89.3199257527161,
6.20840403403277));
#27780=CARTESIAN_POINT('Ctrl Pts',(-22.4558434515285,-89.4621547971772,
6.05042086878414));
#27781=CARTESIAN_POINT('Ctrl Pts',(-21.0307749678768,-91.9062960631275,
5.8924377035355));
#27782=CARTESIAN_POINT('Ctrl Pts',(-22.2988949344083,-94.4354299979253,
5.73445453828687));
#27783=CARTESIAN_POINT('Ctrl Pts',(-25.1099752577798,-94.7555457982637,
5.57647137303824));
#27784=CARTESIAN_POINT('Ctrl Pts',(-26.9142701365138,-92.576287506837,5.4184882077896));
#27785=CARTESIAN_POINT('Ctrl Pts',(-26.0752225311475,-89.8743167768149,
5.26050504254097));
#27786=CARTESIAN_POINT('Ctrl Pts',(-23.3538772582214,-89.1004132843165,
5.10252187729234));
#27787=CARTESIAN_POINT('Ctrl Pts',(-21.2185873656771,-90.9565339120964,
4.94453871204369));
#27788=CARTESIAN_POINT('Ctrl Pts',(-21.6061336679678,-93.7591138972605,
4.78655554679507));
#27789=CARTESIAN_POINT('Ctrl Pts',(-24.1649984413479,-94.9661175354377,
4.62857238154642));
#27790=CARTESIAN_POINT('Ctrl Pts',(-26.574203996375,-93.4827513287052,4.4705892162978));
#27791=CARTESIAN_POINT('Ctrl Pts',(-26.6485186642022,-90.6544790580041,
4.31260605104916));
#27792=CARTESIAN_POINT('Ctrl Pts',(-24.3205365027268,-89.0466402058835,
4.15462288580052));
#27793=CARTESIAN_POINT('Ctrl Pts',(-21.7018167952366,-90.1175994942308,
3.99663972055189));
#27794=CARTESIAN_POINT('Ctrl Pts',(-21.1676276911652,-92.8959602861542,
3.83865655530326));
#27795=CARTESIAN_POINT('Ctrl Pts',(-23.2024969568081,-94.8616545287659,
3.68067339005462));
#27796=CARTESIAN_POINT('Ctrl Pts',(-25.9607286813379,-94.2317304163557,
3.52269022480599));
#27797=CARTESIAN_POINT('Ctrl Pts',(-26.9405126124961,-91.5775506895979,
3.36470705955735));
#27798=CARTESIAN_POINT('Ctrl Pts',(-25.2531511472893,-89.3065468104243,
3.20672389430872));
#27799=CARTESIAN_POINT('Ctrl Pts',(-22.4291390042644,-89.4785971036944,
3.04874072906008));
#27800=CARTESIAN_POINT('Ctrl Pts',(-21.0299510223576,-91.937645484163,2.89075756381145));
#27801=CARTESIAN_POINT('Ctrl Pts',(-22.3246996110788,-94.453252357017,2.73277439856282));
#27802=CARTESIAN_POINT('Ctrl Pts',(-25.1390012538636,-94.7436739362117,
2.57479123331418));
#27803=CARTESIAN_POINT('Ctrl Pts',(-26.9201931102794,-92.5454930206752,
2.41680806806555));
#27804=CARTESIAN_POINT('Ctrl Pts',(-26.0526635517577,-89.8525243463365,
2.25882490281691));
#27805=CARTESIAN_POINT('Ctrl Pts',(-23.3233115518592,-89.1074036232017,
2.10084173756828));
#27806=CARTESIAN_POINT('Ctrl Pts',(-21.2077115778015,-90.9859374711348,
1.94285857231964));
#27807=CARTESIAN_POINT('Ctrl Pts',(-21.624868659881,-93.7843200216542,1.78487540707101));
#27808=CARTESIAN_POINT('Ctrl Pts',(-24.1962362586587,-94.964142143379,1.62689224182237));
#27809=CARTESIAN_POINT('Ctrl Pts',(-26.5898450807175,-93.4556338347463,
1.46890907657374));
#27810=CARTESIAN_POINT('Ctrl Pts',(-26.6338976845917,-90.6263101028394,
1.3109259113251));
#27811=CARTESIAN_POINT('Ctrl Pts',(-24.2898922478439,-89.0440033611201,
1.15294274607647));
#27812=CARTESIAN_POINT('Ctrl Pts',(-21.6809479657765,-90.1407646543606,
0.994959580827837));
#27813=CARTESIAN_POINT('Ctrl Pts',(-21.1795854924137,-92.928282565981,0.836976415579201));
#27814=CARTESIAN_POINT('Ctrl Pts',(-22.5450731455404,-94.2169491679593,
0.731654305413445));
#27815=CARTESIAN_POINT('Ctrl Pts',(-23.3498000020249,-94.4320868020351,
0.678993250330566));
#27816=CARTESIAN_POINT('Ctrl Pts',(-21.9456684496579,-90.2435746787731,
10.1070022498898));
#27817=CARTESIAN_POINT('Ctrl Pts',(-21.3645039014938,-90.9233101920371,
10.0543411948069));
#27818=CARTESIAN_POINT('Ctrl Pts',(-20.9400524765287,-92.8938947526259,
9.94901908464118));
#27819=CARTESIAN_POINT('Ctrl Pts',(-23.0788494627237,-95.0553094224687,
9.79103591939254));
#27820=CARTESIAN_POINT('Ctrl Pts',(-26.0541532854381,-94.4390835936093,
9.63305275414391));
#27821=CARTESIAN_POINT('Ctrl Pts',(-27.1657937219656,-91.6136172760999,
9.47506958889528));
#27822=CARTESIAN_POINT('Ctrl Pts',(-25.4061872379324,-89.1371047939092,
9.31708642364664));
#27823=CARTESIAN_POINT('Ctrl Pts',(-22.3710053471766,-89.2580744370565,
9.159103258398));
#27824=CARTESIAN_POINT('Ctrl Pts',(-20.8134338116745,-91.8657025942017,
9.00112009314937));
#27825=CARTESIAN_POINT('Ctrl Pts',(-22.1461588575891,-94.5953201152443,
8.84313692790073));
#27826=CARTESIAN_POINT('Ctrl Pts',(-25.1603946659823,-94.9708070256751,
8.68515376265211));
#27827=CARTESIAN_POINT('Ctrl Pts',(-27.1221062608033,-92.6517130068406,
8.52717059740346));
#27828=CARTESIAN_POINT('Ctrl Pts',(-26.2519641664366,-89.741472264661,8.36918743215484));
#27829=CARTESIAN_POINT('Ctrl Pts',(-23.3392121156861,-88.8798034424032,
8.21120426690619));
#27830=CARTESIAN_POINT('Ctrl Pts',(-21.0258180101408,-90.8482544145204,
8.05322110165756));
#27831=CARTESIAN_POINT('Ctrl Pts',(-21.4101081026736,-93.861380383774,7.89523793640894));
#27832=CARTESIAN_POINT('Ctrl Pts',(-24.1435187316522,-95.186169617537,7.73725477116029));
#27833=CARTESIAN_POINT('Ctrl Pts',(-26.7467528808536,-93.6209948422715,
7.57927160591167));
#27834=CARTESIAN_POINT('Ctrl Pts',(-26.8585884593915,-90.5855221306583,
7.42128844066302));
#27835=CARTESIAN_POINT('Ctrl Pts',(-24.3775867135566,-88.8330292659221,
7.26330527541439));
#27836=CARTESIAN_POINT('Ctrl Pts',(-21.5541009414308,-89.9530868838363,
7.10532211016575));
#27837=CARTESIAN_POINT('Ctrl Pts',(-20.9491290939422,-92.9297645972614,
6.94733894491712));
#27838=CARTESIAN_POINT('Ctrl Pts',(-23.111401293589,-95.0631140696508,6.78935577966849));
#27839=CARTESIAN_POINT('Ctrl Pts',(-26.0796628484675,-94.4181145382775,
6.63137261441986));
#27840=CARTESIAN_POINT('Ctrl Pts',(-27.1615992170526,-91.579802581307,6.47338944917121));
#27841=CARTESIAN_POINT('Ctrl Pts',(-25.37585718331,-89.1226240272624,6.31540628392259));
#27842=CARTESIAN_POINT('Ctrl Pts',(-22.342165723498,-89.2753236905542,6.15742311867395));
#27843=CARTESIAN_POINT('Ctrl Pts',(-20.812186537839,-91.8993977660205,5.99943995342531));
#27844=CARTESIAN_POINT('Ctrl Pts',(-22.1736629693016,-94.6147215012481,
5.84145678817668));
#27845=CARTESIAN_POINT('Ctrl Pts',(-25.1916894243902,-94.9584035889072,
5.68347362292805));
#27846=CARTESIAN_POINT('Ctrl Pts',(-27.1288128966464,-92.618712644712,5.52549045767941));
#27847=CARTESIAN_POINT('Ctrl Pts',(-26.227996278558,-89.7178282138104,5.36750729243077));
#27848=CARTESIAN_POINT('Ctrl Pts',(-23.3063109895119,-88.8869514883655,
5.20952412718215));
#27849=CARTESIAN_POINT('Ctrl Pts',(-21.0138253101083,-90.8797160180383,
5.05154096193351));
#27850=CARTESIAN_POINT('Ctrl Pts',(-21.4299019989033,-93.8886163569595,
4.89355779668488));
#27851=CARTESIAN_POINT('Ctrl Pts',(-24.1771452978046,-95.1844771977619,
4.73557463143624));
#27852=CARTESIAN_POINT('Ctrl Pts',(-26.7637117649264,-93.5919085268197,
4.5775914661876));
#27853=CARTESIAN_POINT('Ctrl Pts',(-26.8434973305109,-90.5554244874977,
4.41960830093897));
#27854=CARTESIAN_POINT('Ctrl Pts',(-24.3441337613188,-88.8292197430528,
4.26162513569033));
#27855=CARTESIAN_POINT('Ctrl Pts',(-21.5326291273322,-89.9790209200889,
4.10364197044171));
#27856=CARTESIAN_POINT('Ctrl Pts',(-20.9591140859071,-92.9619190970249,
3.94565880519306));
#27857=CARTESIAN_POINT('Ctrl Pts',(-23.1437863719668,-95.0723238327043,
3.78767563994443));
#27858=CARTESIAN_POINT('Ctrl Pts',(-26.1050736196794,-94.3960259623991,
3.6296924746958));
#27859=CARTESIAN_POINT('Ctrl Pts',(-27.1569872914167,-91.5464508131884,
3.47170930944716));
#27860=CARTESIAN_POINT('Ctrl Pts',(-25.3454056375763,-89.1082601538994,
3.31372614419853));
#27861=CARTESIAN_POINT('Ctrl Pts',(-22.3134953480408,-89.2929764469124,
3.15574297894989));
#27862=CARTESIAN_POINT('Ctrl Pts',(-20.8113019350926,-91.9330550689619,
2.99775981370126));
#27863=CARTESIAN_POINT('Ctrl Pts',(-22.2013673348471,-94.6338559069014,
2.83977664845262));
#27864=CARTESIAN_POINT('Ctrl Pts',(-25.2228522564652,-94.9456577440281,
2.68179348320399));
#27865=CARTESIAN_POINT('Ctrl Pts',(-27.1351719079378,-92.5856511298438,
2.52381031795535));
#27866=CARTESIAN_POINT('Ctrl Pts',(-26.2037765520592,-89.6944314680265,
2.36582715270672));
#27867=CARTESIAN_POINT('Ctrl Pts',(-23.2734950967561,-88.8944564420696,
2.20784398745809));
#27868=CARTESIAN_POINT('Ctrl Pts',(-21.0021488684016,-90.9112842085001,
2.04986082220945));
#27869=CARTESIAN_POINT('Ctrl Pts',(-21.4500162235876,-93.9156781060024,
1.89187765696082));
#27870=CARTESIAN_POINT('Ctrl Pts',(-24.2106827809777,-95.1823563812763,
1.73389449171218));
#27871=CARTESIAN_POINT('Ctrl Pts',(-26.78050431473,-93.562794696993,1.57591132646355));
#27872=CARTESIAN_POINT('Ctrl Pts',(-26.827799983517,-90.5251817899866,1.41792816121491));
#27873=CARTESIAN_POINT('Ctrl Pts',(-24.3112335374568,-88.8263887790323,
1.25994499596628));
#27874=CARTESIAN_POINT('Ctrl Pts',(-21.5102239762329,-90.0038914531458,
1.10196183071765));
#27875=CARTESIAN_POINT('Ctrl Pts',(-20.9719521966549,-92.9966208786834,
0.943978665469012));
#27876=CARTESIAN_POINT('Ctrl Pts',(-22.4379643297735,-94.3801565479507,
0.838656555303256));
#27877=CARTESIAN_POINT('Ctrl Pts',(-23.301933573839,-94.6111321859386,0.785995500220377));
#27878=CARTESIAN_POINT('Ctrl Pts',(-21.8048028959809,-90.1231365609213,
10.2140044997796));
#27879=CARTESIAN_POINT('Ctrl Pts',(-21.1837878836397,-90.8494815513233,
10.1613434446967));
#27880=CARTESIAN_POINT('Ctrl Pts',(-20.730231816351,-92.9551891329009,10.056021334531));
#27881=CARTESIAN_POINT('Ctrl Pts',(-23.0156861527743,-95.2648120479719,
9.89803816928236));
#27882=CARTESIAN_POINT('Ctrl Pts',(-26.1950066154872,-94.606331602248,9.74005500403371));
#27883=CARTESIAN_POINT('Ctrl Pts',(-27.3828722579974,-91.5871230053361,
9.58207183878509));
#27884=CARTESIAN_POINT('Ctrl Pts',(-25.5026095237177,-88.9407960149012,
9.42408867353644));
#27885=CARTESIAN_POINT('Ctrl Pts',(-22.2593051526931,-89.0700605487915,
9.26610550828782));
#27886=CARTESIAN_POINT('Ctrl Pts',(-20.5949309072274,-91.8564938185189,
9.10812234303918));
#27887=CARTESIAN_POINT('Ctrl Pts',(-22.0190409350165,-94.7732812651581,
8.95013917779055));
#27888=CARTESIAN_POINT('Ctrl Pts',(-25.2399629504105,-95.1745153202148,
8.79215601254192));
#27889=CARTESIAN_POINT('Ctrl Pts',(-27.336189146788,-92.6964009801777,8.63417284729328));
#27890=CARTESIAN_POINT('Ctrl Pts',(-26.4063813923771,-89.5866049746754,
8.47618968204465));
#27891=CARTESIAN_POINT('Ctrl Pts',(-23.2939018778273,-88.6658515048039,
8.31820651679601));
#27892=CARTESIAN_POINT('Ctrl Pts',(-20.8218782942425,-90.7692791977077,
8.16022335154738));
#27893=CARTESIAN_POINT('Ctrl Pts',(-21.2325191657662,-93.9890152722711,
8.00224018629874));
#27894=CARTESIAN_POINT('Ctrl Pts',(-24.153359813825,-95.4046453291174,7.8442570210501));
#27895=CARTESIAN_POINT('Ctrl Pts',(-26.9350977783999,-93.7321464895926,
7.68627385580147));
#27896=CARTESIAN_POINT('Ctrl Pts',(-27.0546019246961,-90.4885313561186,
7.52829069055284));
#27897=CARTESIAN_POINT('Ctrl Pts',(-24.403477841723,-88.6158700221475,7.3703075253042));
#27898=CARTESIAN_POINT('Ctrl Pts',(-21.3863855962296,-89.8127300123325,
7.21232436005556));
#27899=CARTESIAN_POINT('Ctrl Pts',(-20.7399308175942,-92.9935185734688,
7.05434119480694));
#27900=CARTESIAN_POINT('Ctrl Pts',(-23.0504700633042,-95.2731518599606,
6.89635802955829));
#27901=CARTESIAN_POINT('Ctrl Pts',(-26.2222653697413,-94.5839246983912,
6.73837486430967));
#27902=CARTESIAN_POINT('Ctrl Pts',(-27.3783901358023,-91.550989636275,6.58039169906103));
#27903=CARTESIAN_POINT('Ctrl Pts',(-25.4701997366701,-88.9253223018084,
6.4224085338124));
#27904=CARTESIAN_POINT('Ctrl Pts',(-22.2284879954675,-89.0884925839314,
6.26442536856376));
#27905=CARTESIAN_POINT('Ctrl Pts',(-20.5935981078012,-91.8924994689134,
6.10644220331513));
#27906=CARTESIAN_POINT('Ctrl Pts',(-22.0484310041947,-94.794013004571,5.94845903806649));
#27907=CARTESIAN_POINT('Ctrl Pts',(-25.2734035910007,-95.1612613795506,
5.79047587281786));
#27908=CARTESIAN_POINT('Ctrl Pts',(-27.343355656779,-92.6611377825871,5.63249270756922));
#27909=CARTESIAN_POINT('Ctrl Pts',(-26.3807700259685,-89.561339650806,5.47450954232059));
#27910=CARTESIAN_POINT('Ctrl Pts',(-23.2587447208024,-88.6734896924145,
5.31652637707195));
#27911=CARTESIAN_POINT('Ctrl Pts',(-20.8090632545395,-90.80289812398,5.15854321182332));
#27912=CARTESIAN_POINT('Ctrl Pts',(-21.2536703298387,-94.0181188166586,
5.00056004657469));
#27913=CARTESIAN_POINT('Ctrl Pts',(-24.1892921542613,-95.4028368600861,
4.84257688132605));
#27914=CARTESIAN_POINT('Ctrl Pts',(-26.9532195334778,-93.7010657249343,
4.68459371607742));
#27915=CARTESIAN_POINT('Ctrl Pts',(-27.0384759968196,-90.4563699169912,
4.52661055082878));
#27916=CARTESIAN_POINT('Ctrl Pts',(-24.3677310199108,-88.6117992802222,
4.36862738558014));
#27917=CARTESIAN_POINT('Ctrl Pts',(-21.3634414594277,-89.8404423459467,
4.21064422033152));
#27918=CARTESIAN_POINT('Ctrl Pts',(-20.7506004806489,-93.0278779078959,
4.05266105508288));
#27919=CARTESIAN_POINT('Ctrl Pts',(-23.0850757871254,-95.2829931366425,
3.89467788983424));
#27920=CARTESIAN_POINT('Ctrl Pts',(-26.2494185580208,-94.5603215084427,
3.73669472458561));
#27921=CARTESIAN_POINT('Ctrl Pts',(-27.3734619703373,-91.5153509367788,
3.57871155933698));
#27922=CARTESIAN_POINT('Ctrl Pts',(-25.4376601278634,-88.9099734973746,
3.42072839408834));
#27923=CARTESIAN_POINT('Ctrl Pts',(-22.1978516918172,-89.1073557901304,
3.26274522883971));
#27924=CARTESIAN_POINT('Ctrl Pts',(-20.5926528478276,-91.9284646537611,
3.10476206359107));
#27925=CARTESIAN_POINT('Ctrl Pts',(-22.0780350586153,-94.8144594567856,
2.94677889834244));
#27926=CARTESIAN_POINT('Ctrl Pts',(-25.3067032590667,-95.1476415518446,
2.7887957330938));
#27927=CARTESIAN_POINT('Ctrl Pts',(-27.3501507055963,-92.6258092390124,
2.63081256784517));
#27928=CARTESIAN_POINT('Ctrl Pts',(-26.3548895523608,-89.5363385897163,
2.47282940259653));
#27929=CARTESIAN_POINT('Ctrl Pts',(-23.223678641653,-88.6815092609377,2.3148462373479));
#27930=CARTESIAN_POINT('Ctrl Pts',(-20.7965861590018,-90.8366309458652,
2.15686307209926));
#27931=CARTESIAN_POINT('Ctrl Pts',(-21.2751637872942,-94.0470361903508,
1.99887990685063));
#27932=CARTESIAN_POINT('Ctrl Pts',(-24.2251293032967,-95.4005706191734,
1.84089674160199));
#27933=CARTESIAN_POINT('Ctrl Pts',(-26.9711635487424,-93.6699555592399,
1.68291357635336));
#27934=CARTESIAN_POINT('Ctrl Pts',(-27.0217022824422,-90.4240534771338,
1.52493041110472));
#27935=CARTESIAN_POINT('Ctrl Pts',(-24.3325748270696,-88.6087741969446,
1.36694724585609));
#27936=CARTESIAN_POINT('Ctrl Pts',(-21.3394999866892,-89.8670182519309,
1.20896408060746));
#27937=CARTESIAN_POINT('Ctrl Pts',(-20.7643189008962,-93.0649591913859,
1.05098091535882));
#27938=CARTESIAN_POINT('Ctrl Pts',(-22.3308555140066,-94.5433639279422,
0.945658805193066));
#27939=CARTESIAN_POINT('Ctrl Pts',(-23.2540671456531,-94.7901775698421,
0.892997750110188));
#27940=CARTESIAN_POINT('Ctrl Pts',(-21.6639373423038,-90.0026984430693,
10.3210067496694));
#27941=CARTESIAN_POINT('Ctrl Pts',(-21.0030718657857,-90.7756529106096,
10.2683456945866));
#27942=CARTESIAN_POINT('Ctrl Pts',(-20.5204111561734,-93.0164835131759,
10.1630235844208));
#27943=CARTESIAN_POINT('Ctrl Pts',(-22.9525228428248,-95.474314673475,10.0050404191722));
#27944=CARTESIAN_POINT('Ctrl Pts',(-26.3358599455363,-94.7735796108867,
9.84705725392353));
#27945=CARTESIAN_POINT('Ctrl Pts',(-27.5999507940291,-91.5606287345722,
9.6890740886749));
#27946=CARTESIAN_POINT('Ctrl Pts',(-25.5990318095031,-88.7444872358932,
9.53109092342626));
#27947=CARTESIAN_POINT('Ctrl Pts',(-22.1476049582095,-88.8820466605266,
9.37310775817762));
#27948=CARTESIAN_POINT('Ctrl Pts',(-20.3764280027803,-91.847285042836,9.21512459292899));
#27949=CARTESIAN_POINT('Ctrl Pts',(-21.8919230124438,-94.9512424150719,
9.05714142768036));
#27950=CARTESIAN_POINT('Ctrl Pts',(-25.3195312348388,-95.3782236147545,
8.89915826243172));
#27951=CARTESIAN_POINT('Ctrl Pts',(-27.5502720327727,-92.7410889535148,
8.74117509718309));
#27952=CARTESIAN_POINT('Ctrl Pts',(-26.5607986183176,-89.4317376846897,
8.58319193193445));
#27953=CARTESIAN_POINT('Ctrl Pts',(-23.2485916399684,-88.4518995672047,
8.42520876668582));
#27954=CARTESIAN_POINT('Ctrl Pts',(-20.6179385783441,-90.6903039808948,
8.26722560143718));
#27955=CARTESIAN_POINT('Ctrl Pts',(-21.0549302288588,-94.116650160768,8.10924243618856));
#27956=CARTESIAN_POINT('Ctrl Pts',(-24.1632008959979,-95.6231210406981,
7.95125927093991));
#27957=CARTESIAN_POINT('Ctrl Pts',(-27.1234426759463,-93.8432981369136,
7.79327610569129));
#27958=CARTESIAN_POINT('Ctrl Pts',(-27.2506153900006,-90.391540581579,7.63529294044264));
#27959=CARTESIAN_POINT('Ctrl Pts',(-24.4293689698895,-88.3987107783728,
7.47730977519402));
#27960=CARTESIAN_POINT('Ctrl Pts',(-21.2186702510283,-89.672373140829,7.31932660994537));
#27961=CARTESIAN_POINT('Ctrl Pts',(-20.5307325412461,-93.057272549676,7.16134344469675));
#27962=CARTESIAN_POINT('Ctrl Pts',(-22.9895388330194,-95.4831896502703,
7.0033602794481));
#27963=CARTESIAN_POINT('Ctrl Pts',(-26.364867891015,-94.7497348585049,6.84537711419948));
#27964=CARTESIAN_POINT('Ctrl Pts',(-27.5951810545518,-91.5221766912428,
6.68739394895083));
#27965=CARTESIAN_POINT('Ctrl Pts',(-25.5645422900302,-88.7280205763547,
6.52941078370221));
#27966=CARTESIAN_POINT('Ctrl Pts',(-22.114810267437,-88.9016614773084,6.37142761845357));
#27967=CARTESIAN_POINT('Ctrl Pts',(-20.3750096777634,-91.8856011718064,
6.21344445320494));
#27968=CARTESIAN_POINT('Ctrl Pts',(-21.923199039088,-94.9733045078939,6.0554612879563));
#27969=CARTESIAN_POINT('Ctrl Pts',(-25.3551177576112,-95.3641191701941,
5.89747812270767));
#27970=CARTESIAN_POINT('Ctrl Pts',(-27.5578984169117,-92.7035629204621,
5.73949495745903));
#27971=CARTESIAN_POINT('Ctrl Pts',(-26.533543773379,-89.4048510878016,5.5815117922104));
#27972=CARTESIAN_POINT('Ctrl Pts',(-23.2111784520928,-88.4600278964635,
5.42352862696177));
#27973=CARTESIAN_POINT('Ctrl Pts',(-20.6043011989706,-90.7260802299217,
5.26554546171313));
#27974=CARTESIAN_POINT('Ctrl Pts',(-21.0774386607742,-94.1476212763577,
5.1075622964645));
#27975=CARTESIAN_POINT('Ctrl Pts',(-24.2014390107181,-95.6211965224102,
4.94957913121586));
#27976=CARTESIAN_POINT('Ctrl Pts',(-27.1427273020292,-93.8102229230488,
4.79159596596723));
#27977=CARTESIAN_POINT('Ctrl Pts',(-27.2334546631283,-90.3573153464849,
4.63361280071859));
#27978=CARTESIAN_POINT('Ctrl Pts',(-24.3913282785028,-88.3943788173915,
4.47562963546995));
#27979=CARTESIAN_POINT('Ctrl Pts',(-21.1942537915233,-89.7018637718047,
4.31764647022133));
#27980=CARTESIAN_POINT('Ctrl Pts',(-20.5420868753907,-93.0938367187666,
4.15966330497269));
#27981=CARTESIAN_POINT('Ctrl Pts',(-23.026365202284,-95.4936624405808,4.00168013972406));
#27982=CARTESIAN_POINT('Ctrl Pts',(-26.3937634963623,-94.7246170544863,
3.84369697447542));
#27983=CARTESIAN_POINT('Ctrl Pts',(-27.5899366492579,-91.4842510603691,
3.68571380922678));
#27984=CARTESIAN_POINT('Ctrl Pts',(-25.5299146181504,-88.7116868408497,
3.52773064397815));
#27985=CARTESIAN_POINT('Ctrl Pts',(-22.0822080355935,-88.9217351333484,
3.36974747872952));
#27986=CARTESIAN_POINT('Ctrl Pts',(-20.3740037605626,-91.92387423856,3.21176431348088));
#27987=CARTESIAN_POINT('Ctrl Pts',(-21.9547027823836,-94.99506300667,3.05378114823225));
#27988=CARTESIAN_POINT('Ctrl Pts',(-25.3905542616683,-95.349625359661,2.89579798298362));
#27989=CARTESIAN_POINT('Ctrl Pts',(-27.5651295032547,-92.6659673481809,
2.73781481773498));
#27990=CARTESIAN_POINT('Ctrl Pts',(-26.5060025526623,-89.3782457114063,
2.57983165248635));
#27991=CARTESIAN_POINT('Ctrl Pts',(-23.1738621865499,-88.4685620798055,
2.42184848723771));
#27992=CARTESIAN_POINT('Ctrl Pts',(-20.5910234496019,-90.7619776832305,
2.26386532198907));
#27993=CARTESIAN_POINT('Ctrl Pts',(-21.1003113510007,-94.1783942746989,
2.10588215674044));
#27994=CARTESIAN_POINT('Ctrl Pts',(-24.2395758256157,-95.6187848570707,
1.94789899149181));
#27995=CARTESIAN_POINT('Ctrl Pts',(-27.1618227827549,-93.7771164214867,
1.78991582624317));
#27996=CARTESIAN_POINT('Ctrl Pts',(-27.2156045813675,-90.3229251642809,
1.63193266099454));
#27997=CARTESIAN_POINT('Ctrl Pts',(-24.3539161166825,-88.3911596148569,
1.4739494957459));
#27998=CARTESIAN_POINT('Ctrl Pts',(-21.1687759971456,-89.7301450507159,
1.31596633049727));
#27999=CARTESIAN_POINT('Ctrl Pts',(-20.5566856051374,-93.1332975040884,
1.15798316524863));
#28000=CARTESIAN_POINT('Ctrl Pts',(-22.2237466982397,-94.7065713079336,
1.05266105508288));
#28001=CARTESIAN_POINT('Ctrl Pts',(-23.2062007174672,-94.9692229537457,
0.999999999999999));
#28002=CARTESIAN_POINT('Ctrl Pts',(-22.0865340033349,-90.364012796625,10.));
#28003=CARTESIAN_POINT('Ctrl Pts',(-22.0249229041794,-90.42191210108,10.));
#28004=CARTESIAN_POINT('Ctrl Pts',(-21.9666809070895,-90.4829619660093,
10.));
#28005=CARTESIAN_POINT('Ctrl Pts',(-21.9118056829835,-90.5467776153496,
10.));
#28006=CARTESIAN_POINT('Ctrl Pts',(-21.8554777542738,-90.612282647997,10.));
#28007=CARTESIAN_POINT('Ctrl Pts',(-21.8026967773226,-90.6807022716027,
10.));
#28008=CARTESIAN_POINT('Ctrl Pts',(-21.7534857403585,-90.751668886859,10.));
#28009=CARTESIAN_POINT('Ctrl Pts',(-21.7029132366757,-90.8245988560858,
10.));
#28010=CARTESIAN_POINT('Ctrl Pts',(-21.6561104020018,-90.9002192512322,
10.));
#28011=CARTESIAN_POINT('Ctrl Pts',(-21.6131362838788,-90.9781741250521,
10.));
#28012=CARTESIAN_POINT('Ctrl Pts',(-21.5942448480483,-91.0124431120789,
10.));
#28013=CARTESIAN_POINT('Ctrl Pts',(-21.5760937898788,-91.0471637309784,
10.));
#28014=CARTESIAN_POINT('Ctrl Pts',(-21.5586905433102,-91.0823078140376,
10.));
#28015=CARTESIAN_POINT('Ctrl Pts',(-21.5487655216201,-91.1023503839837,
10.));
#28016=CARTESIAN_POINT('Ctrl Pts',(-21.5390837455501,-91.122530701603,10.));
#28017=CARTESIAN_POINT('Ctrl Pts',(-21.5296468276344,-91.1428436902072,
10.));
#28018=CARTESIAN_POINT('Ctrl Pts',(-21.5211298019169,-91.1611766086332,
10.));
#28019=CARTESIAN_POINT('Ctrl Pts',(-21.5128098409547,-91.1796233420343,
10.));
#28020=CARTESIAN_POINT('Ctrl Pts',(-21.5047018248584,-91.1981483274791,
10.));
#28021=CARTESIAN_POINT('Ctrl Pts',(-21.468137058809,-91.281690559118,10.));
#28022=CARTESIAN_POINT('Ctrl Pts',(-21.435832611822,-91.3669162867985,10.));
#28023=CARTESIAN_POINT('Ctrl Pts',(-21.4078135856883,-91.4534267955088,
10.));
#28024=CARTESIAN_POINT('Ctrl Pts',(-21.3793318743036,-91.5413658740861,
10.));
#28025=CARTESIAN_POINT('Ctrl Pts',(-21.3552777914222,-91.6306332709131,
10.));
#28026=CARTESIAN_POINT('Ctrl Pts',(-21.3357167785958,-91.7208473131702,
10.));
#28027=CARTESIAN_POINT('Ctrl Pts',(-21.3167363466558,-91.8083837564149,
10.));
#28028=CARTESIAN_POINT('Ctrl Pts',(-21.3019860690135,-91.8968124021051,
10.));
#28029=CARTESIAN_POINT('Ctrl Pts',(-21.2915665512102,-91.9858064658359,
10.));
#28030=CARTESIAN_POINT('Ctrl Pts',(-21.2872071979573,-92.0230401045266,
10.));
#28031=CARTESIAN_POINT('Ctrl Pts',(-21.2836064360671,-92.0603729082663,
10.));
#28032=CARTESIAN_POINT('Ctrl Pts',(-21.2807739547557,-92.0977815592145,
10.));
#28033=CARTESIAN_POINT('Ctrl Pts',(-21.2790033727376,-92.1211656798516,
10.));
#28034=CARTESIAN_POINT('Ctrl Pts',(-21.2775330236673,-92.1445794431136,
10.));
#28035=CARTESIAN_POINT('Ctrl Pts',(-21.2763655645011,-92.1680171857376,
10.));
#28036=CARTESIAN_POINT('Ctrl Pts',(-21.2756812972385,-92.1817544370702,
10.));
#28037=CARTESIAN_POINT('Ctrl Pts',(-21.2751013563293,-92.1954953575252,
10.));
#28038=CARTESIAN_POINT('Ctrl Pts',(-21.2746262639777,-92.2092305726123,
10.));
#28039=CARTESIAN_POINT('Ctrl Pts',(-21.2712684324437,-92.3063075686709,
10.));
#28040=CARTESIAN_POINT('Ctrl Pts',(-21.2731377894438,-92.4032200227796,
10.));
#28041=CARTESIAN_POINT('Ctrl Pts',(-21.2802991313829,-92.4995456761415,
10.));
#28042=CARTESIAN_POINT('Ctrl Pts',(-21.2874604733219,-92.5958713295034,
10.));
#28043=CARTESIAN_POINT('Ctrl Pts',(-21.2999133653317,-92.6916112366308,
10.));
#28044=CARTESIAN_POINT('Ctrl Pts',(-21.3177754963829,-92.7863620775548,
10.));
#28045=CARTESIAN_POINT('Ctrl Pts',(-21.3348530128177,-92.8769508789951,
10.));
#28046=CARTESIAN_POINT('Ctrl Pts',(-21.3568748775386,-92.9666365695189,
10.));
#28047=CARTESIAN_POINT('Ctrl Pts',(-21.3835663946288,-93.0551798098071,
10.));
#28048=CARTESIAN_POINT('Ctrl Pts',(-21.3925012626256,-93.0848192702138,
10.));
#28049=CARTESIAN_POINT('Ctrl Pts',(-21.4019598223812,-93.1143306773249,
10.));
#28050=CARTESIAN_POINT('Ctrl Pts',(-21.4119330456339,-93.1437048746533,
10.));
#28051=CARTESIAN_POINT('Ctrl Pts',(-21.4184142793756,-93.1627940932574,
10.));
#28052=CARTESIAN_POINT('Ctrl Pts',(-21.4251128797724,-93.1818253626268,
10.));
#28053=CARTESIAN_POINT('Ctrl Pts',(-21.4320265053981,-93.2007961347298,
10.));
#28054=CARTESIAN_POINT('Ctrl Pts',(-21.4386160833976,-93.2188777302993,
10.));
#28055=CARTESIAN_POINT('Ctrl Pts',(-21.4454027538013,-93.2369085767537,
10.));
#28056=CARTESIAN_POINT('Ctrl Pts',(-21.4523736968937,-93.2548593171236,
10.));
#28057=CARTESIAN_POINT('Ctrl Pts',(-21.4862171782416,-93.3420090096165,
10.));
#28058=CARTESIAN_POINT('Ctrl Pts',(-21.5244390025882,-93.4273844054068,
10.));
#28059=CARTESIAN_POINT('Ctrl Pts',(-21.566707986091,-93.5107518898265,10.));
#28060=CARTESIAN_POINT('Ctrl Pts',(-21.6105462295651,-93.5972144393595,
10.));
#28061=CARTESIAN_POINT('Ctrl Pts',(-21.658737839251,-93.6815179448056,10.));
#28062=CARTESIAN_POINT('Ctrl Pts',(-21.7109693333793,-93.7633987878851,
10.));
#28063=CARTESIAN_POINT('Ctrl Pts',(-21.7637892526044,-93.8462020771595,
10.));
#28064=CARTESIAN_POINT('Ctrl Pts',(-21.8207410024304,-93.9265286302991,
10.));
#28065=CARTESIAN_POINT('Ctrl Pts',(-21.8815521717217,-94.0040909732374,
10.));
#28066=CARTESIAN_POINT('Ctrl Pts',(-21.9232146414969,-94.0572298752848,
10.));
#28067=CARTESIAN_POINT('Ctrl Pts',(-21.9666897223061,-94.1090710101977,
10.));
#28068=CARTESIAN_POINT('Ctrl Pts',(-22.0119020259848,-94.1595148903617,
10.));
#28069=CARTESIAN_POINT('Ctrl Pts',(-22.0240091589624,-94.1730229559845,
10.));
#28070=CARTESIAN_POINT('Ctrl Pts',(-22.0362421971848,-94.1864320425615,
10.));
#28071=CARTESIAN_POINT('Ctrl Pts',(-22.0485860744409,-94.1997257421532,
10.));
#28072=CARTESIAN_POINT('Ctrl Pts',(-22.1172469211216,-94.2736698239476,
10.));
#28073=CARTESIAN_POINT('Ctrl Pts',(-22.1894216591264,-94.3441460198121,
10.));
#28074=CARTESIAN_POINT('Ctrl Pts',(-22.2647998275067,-94.4108645190983,
10.));
#28075=CARTESIAN_POINT('Ctrl Pts',(-22.3277047217446,-94.4665427112258,
10.));
#28076=CARTESIAN_POINT('Ctrl Pts',(-22.3928416636934,-94.5196039171525,
10.));
#28077=CARTESIAN_POINT('Ctrl Pts',(-22.4600538825451,-94.5698659316683,
10.));
#28078=CARTESIAN_POINT('Ctrl Pts',(-22.4819361594785,-94.5862297318769,
10.));
#28079=CARTESIAN_POINT('Ctrl Pts',(-22.5040385610628,-94.6022967070182,
10.));
#28080=CARTESIAN_POINT('Ctrl Pts',(-22.5263561031885,-94.6180601837531,
10.));
#28081=CARTESIAN_POINT('Ctrl Pts',(-22.5491249077463,-94.6341423992097,
10.));
#28082=CARTESIAN_POINT('Ctrl Pts',(-22.5721230552632,-94.6499121464985,
10.));
#28083=CARTESIAN_POINT('Ctrl Pts',(-22.5953161167533,-94.6653431121406,
10.));
#28084=CARTESIAN_POINT('Ctrl Pts',(-22.6802614455734,-94.7218595168873,
10.));
#28085=CARTESIAN_POINT('Ctrl Pts',(-22.7678730455798,-94.7738754900138,
10.));
#28086=CARTESIAN_POINT('Ctrl Pts',(-22.8578606517821,-94.8210829659429,
10.));
#28087=CARTESIAN_POINT('Ctrl Pts',(-22.9411342809957,-94.8647682912064,
10.));
#28088=CARTESIAN_POINT('Ctrl Pts',(-23.0264434122392,-94.9043361313526,
10.));
#28089=CARTESIAN_POINT('Ctrl Pts',(-23.1135854408295,-94.9395135107766,
10.));
#28090=CARTESIAN_POINT('Ctrl Pts',(-23.1436093918511,-94.9516335398141,
10.));
#28091=CARTESIAN_POINT('Ctrl Pts',(-23.173851123563,-94.9632321026033,10.));
#28092=CARTESIAN_POINT('Ctrl Pts',(-23.2042982523172,-94.9743127795766,
10.));
#28093=CARTESIAN_POINT('Ctrl Pts',(-26.5182106813093,-92.0021944371302,
8.38741669750803));
#28094=CARTESIAN_POINT('Ctrl Pts',(-26.5197766683662,-92.1747250448626,
8.39833391417657));
#28095=CARTESIAN_POINT('Ctrl Pts',(-26.5035406983691,-92.3469627335709,
8.40925113084512));
#28096=CARTESIAN_POINT('Ctrl Pts',(-26.4684111368875,-92.5152564032994,
8.42016834751366));
#28097=CARTESIAN_POINT('Ctrl Pts',(-26.2989577103971,-93.3270495993809,
8.47282940259654));
#28098=CARTESIAN_POINT('Ctrl Pts',(-25.6898920459756,-94.0470741652581,
8.52549045767941));
#28099=CARTESIAN_POINT('Ctrl Pts',(-24.9174342801995,-94.3487964872293,
8.57815151276229));
#28100=CARTESIAN_POINT('Ctrl Pts',(-24.1449765144233,-94.6505188092004,
8.63081256784517));
#28101=CARTESIAN_POINT('Ctrl Pts',(-23.2091266472925,-94.5339388872655,
8.68347362292804));
#28102=CARTESIAN_POINT('Ctrl Pts',(-22.5343117030538,-94.0519076603904,
8.73613467801092));
#28103=CARTESIAN_POINT('Ctrl Pts',(-21.859496758815,-93.5698764335152,8.7887957330938));
#28104=CARTESIAN_POINT('Ctrl Pts',(-21.4457167374683,-92.7223939016998,
8.84145678817668));
#28105=CARTESIAN_POINT('Ctrl Pts',(-21.4806215310513,-91.8938487950316,
8.89411784325956));
#28106=CARTESIAN_POINT('Ctrl Pts',(-21.5155263246344,-91.0653036883635,
8.94677889834244));
#28107=CARTESIAN_POINT('Ctrl Pts',(-21.9991159331473,-90.2556960068425,
8.99943995342531));
#28108=CARTESIAN_POINT('Ctrl Pts',(-22.7120873058182,-89.8321130406813,
9.05210100850819));
#28109=CARTESIAN_POINT('Ctrl Pts',(-23.4250586784891,-89.4085300745201,
9.10476206359107));
#28110=CARTESIAN_POINT('Ctrl Pts',(-24.3674118153181,-89.3709718237187,
9.15742311867395));
#28111=CARTESIAN_POINT('Ctrl Pts',(-25.1117467560304,-89.7366423606423,
9.21008417375683));
#28112=CARTESIAN_POINT('Ctrl Pts',(-25.8560816967427,-90.102312897566,9.2627452288397));
#28113=CARTESIAN_POINT('Ctrl Pts',(-26.4023984413383,-90.8712122222148,
9.31540628392258));
#28114=CARTESIAN_POINT('Ctrl Pts',(-26.5029876085453,-91.6942825575571,
9.36806733900546));
#28115=CARTESIAN_POINT('Ctrl Pts',(-26.5153075025967,-91.7950900262914,
9.37451712517298));
#28116=CARTESIAN_POINT('Ctrl Pts',(-26.5209411710519,-91.8967100980969,
9.3809669113405));
#28117=CARTESIAN_POINT('Ctrl Pts',(-26.5201759878003,-91.9984131478585,
9.38741669750802));
#28118=CARTESIAN_POINT('Ctrl Pts',(-24.7937992825329,-94.9692229537457,
10.));
#28119=CARTESIAN_POINT('Ctrl Pts',(-25.7762533017603,-94.7065713079336,
9.94733894491712));
#28120=CARTESIAN_POINT('Ctrl Pts',(-27.4433142859563,-93.1332967687399,
9.84201683475136));
#28121=CARTESIAN_POINT('Ctrl Pts',(-26.8312240969782,-89.7301452717062,
9.68403366950274));
#28122=CARTESIAN_POINT('Ctrl Pts',(-23.6460838755241,-88.3911593875009,
9.52605050425409));
#28123=CARTESIAN_POINT('Ctrl Pts',(-20.7843953448966,-90.3229252160129,
9.36806733900547));
#28124=CARTESIAN_POINT('Ctrl Pts',(-20.8381771631847,-93.7771164103054,
9.21008417375682));
#28125=CARTESIAN_POINT('Ctrl Pts',(-23.7604241627304,-95.6187849549087,
9.05210100850819));
#28126=CARTESIAN_POINT('Ctrl Pts',(-26.8996887115742,-94.1783943047284,
8.89411784325956));
#28127=CARTESIAN_POINT('Ctrl Pts',(-27.4089766159342,-90.7619776656796,
8.73613467801092));
#28128=CARTESIAN_POINT('Ctrl Pts',(-24.8261378316183,-88.4685620052275,
8.57815151276229));
#28129=CARTESIAN_POINT('Ctrl Pts',(-21.493997396212,-89.3782456609066,8.42016834751366));
#28130=CARTESIAN_POINT('Ctrl Pts',(-20.4348704258473,-92.6659673604641,
8.26218518226503));
#28131=CARTESIAN_POINT('Ctrl Pts',(-22.6094457101907,-95.3496254273119,
8.10420201701638));
#28132=CARTESIAN_POINT('Ctrl Pts',(-26.0452972587431,-94.9950630663803,
7.94621885176775));
#28133=CARTESIAN_POINT('Ctrl Pts',(-27.6259963119893,-91.9238742371833,
7.78823568651911));
#28134=CARTESIAN_POINT('Ctrl Pts',(-25.9177920028682,-88.9217350716083,
7.63025252127049));
#28135=CARTESIAN_POINT('Ctrl Pts',(-22.4700853511787,-88.7116867750179,
7.47226935602185));
#28136=CARTESIAN_POINT('Ctrl Pts',(-20.4100632788413,-91.4842510500175,
7.31428619077321));
#28137=CARTESIAN_POINT('Ctrl Pts',(-21.6062364556795,-94.7246171090759,
7.15630302552459));
#28138=CARTESIAN_POINT('Ctrl Pts',(-24.9736348172233,-95.4936625105602,
6.99831986027594));
#28139=CARTESIAN_POINT('Ctrl Pts',(-27.4579131938761,-93.0938367406809,
6.84033669502731));
#28140=CARTESIAN_POINT('Ctrl Pts',(-26.8057462646821,-89.7018637257671,
6.68235352977867));
#28141=CARTESIAN_POINT('Ctrl Pts',(-23.6086717136575,-88.3943787451648,
6.52437036453005));
#28142=CARTESIAN_POINT('Ctrl Pts',(-20.7665452720997,-90.3573153135784,
6.36638719928141));
#28143=CARTESIAN_POINT('Ctrl Pts',(-20.8572726350159,-93.8102229593112,
6.20840403403277));
#28144=CARTESIAN_POINT('Ctrl Pts',(-23.7985609852469,-95.6211965949497,
6.05042086878414));
#28145=CARTESIAN_POINT('Ctrl Pts',(-26.9225613977704,-94.1476213193784,
5.8924377035355));
#28146=CARTESIAN_POINT('Ctrl Pts',(-27.3956988690517,-90.7260802044029,
5.73445453828687));
#28147=CARTESIAN_POINT('Ctrl Pts',(-24.7888215637087,-88.4600278255509,
5.57647137303823));
#28148=CARTESIAN_POINT('Ctrl Pts',(-21.4664561758692,-89.404851035816,5.41848820778961));
#28149=CARTESIAN_POINT('Ctrl Pts',(-20.4421015118168,-92.7035629345559,
5.26050504254096));
#28150=CARTESIAN_POINT('Ctrl Pts',(-22.6448822152433,-95.3641192375839,
5.10252187729233));
#28151=CARTESIAN_POINT('Ctrl Pts',(-26.0768010025144,-94.9733045674548,
4.94453871204369));
#28152=CARTESIAN_POINT('Ctrl Pts',(-27.6249903948521,-91.8856011695148,
4.78655554679506));
#28153=CARTESIAN_POINT('Ctrl Pts',(-25.8851897703268,-88.9016614152428,
4.62857238154642));
#28154=CARTESIAN_POINT('Ctrl Pts',(-22.435457678629,-88.7280205108105,4.4705892162978));
#28155=CARTESIAN_POINT('Ctrl Pts',(-20.4048188734298,-91.5221766816716,
4.31260605104916));
#28156=CARTESIAN_POINT('Ctrl Pts',(-21.6351320616123,-94.7497349135865,
4.15462288580052));
#28157=CARTESIAN_POINT('Ctrl Pts',(-25.0104611872221,-95.4831897200468,
3.99663972055189));
#28158=CARTESIAN_POINT('Ctrl Pts',(-27.46926752825,-93.0572725708519,3.83865655530325));
#28159=CARTESIAN_POINT('Ctrl Pts',(-26.7813298046868,-89.6723730942085,
3.68067339005462));
#28160=CARTESIAN_POINT('Ctrl Pts',(-23.5706310215098,-88.3987107062197,
3.52269022480598));
#28161=CARTESIAN_POINT('Ctrl Pts',(-20.7493845448822,-90.3915405493825,
3.36470705955735));
#28162=CARTESIAN_POINT('Ctrl Pts',(-20.876557261488,-93.8432981737925,3.20672389430871));
#28163=CARTESIAN_POINT('Ctrl Pts',(-23.8367991007265,-95.6231211133646,
3.04874072906008));
#28164=CARTESIAN_POINT('Ctrl Pts',(-26.9450698301516,-94.1166502029988,
2.89075756381144));
#28165=CARTESIAN_POINT('Ctrl Pts',(-27.3820614893708,-90.6903039549832,
2.73277439856281));
#28166=CARTESIAN_POINT('Ctrl Pts',(-24.7514083751606,-88.4518994955133,
2.57479123331418));
#28167=CARTESIAN_POINT('Ctrl Pts',(-21.4392013302128,-89.4317376344075,
2.41680806806554));
#28168=CARTESIAN_POINT('Ctrl Pts',(-20.4497278964894,-92.7410889661721,
2.25882490281691));
#28169=CARTESIAN_POINT('Ctrl Pts',(-22.6804687378898,-95.3782236865055,
2.10084173756827));
#28170=CARTESIAN_POINT('Ctrl Pts',(-26.1080770316232,-94.9512424666579,
1.94285857231964));
#28171=CARTESIAN_POINT('Ctrl Pts',(-27.6235720657977,-91.8472850535337,
1.78487540707101));
#28172=CARTESIAN_POINT('Ctrl Pts',(-25.852395087606,-88.8820465732967,1.62689224182237));
#28173=CARTESIAN_POINT('Ctrl Pts',(-22.4009681396119,-88.7444872144855,
1.46890907657374));
#28174=CARTESIAN_POINT('Ctrl Pts',(-20.4000491745082,-91.5606286501729,
1.3109259113251));
#28175=CARTESIAN_POINT('Ctrl Pts',(-21.6641399192573,-94.7735797938367,
1.15294274607647));
#28176=CARTESIAN_POINT('Ctrl Pts',(-25.0474773599211,-95.4743145446722,
0.994959580827833));
#28177=CARTESIAN_POINT('Ctrl Pts',(-27.4795883375449,-93.0164840574888,
0.836976415579199));
#28178=CARTESIAN_POINT('Ctrl Pts',(-26.9969281342143,-90.7756529106095,
0.731654305413442));
#28179=CARTESIAN_POINT('Ctrl Pts',(-26.3360626576961,-90.0026984430693,
0.678993250330564));
#28180=CARTESIAN_POINT('Ctrl Pts',(-24.745932854347,-94.7901775698421,10.1070022498898));
#28181=CARTESIAN_POINT('Ctrl Pts',(-25.6691444859934,-94.5433639279422,
10.0543411948069));
#28182=CARTESIAN_POINT('Ctrl Pts',(-27.2356809967647,-93.0649585003793,
9.94901908464118));
#28183=CARTESIAN_POINT('Ctrl Pts',(-26.6605001017588,-89.8670184595953,
9.79103591939254));
#28184=CARTESIAN_POINT('Ctrl Pts',(-23.6674251656069,-88.6087739832982,
9.6330527541439));
#28185=CARTESIAN_POINT('Ctrl Pts',(-20.9782976482682,-90.4240535257464,
9.47506958889527));
#28186=CARTESIAN_POINT('Ctrl Pts',(-21.028836400457,-93.6699555487327,9.31708642364663));
#28187=CARTESIAN_POINT('Ctrl Pts',(-23.7748706857521,-95.4005707111119,
9.159103258398));
#28188=CARTESIAN_POINT('Ctrl Pts',(-26.7248362715075,-94.0470362185693,
9.00112009314937));
#28189=CARTESIAN_POINT('Ctrl Pts',(-27.2034139025825,-90.8366309293727,
8.84313692790074));
#28190=CARTESIAN_POINT('Ctrl Pts',(-24.7763213754196,-88.6815091908567,
8.68515376265209));
#28191=CARTESIAN_POINT('Ctrl Pts',(-21.6451103995964,-89.5363385422618,
8.52717059740347));
#28192=CARTESIAN_POINT('Ctrl Pts',(-20.6498492277809,-92.6258092505549,
8.36918743215483));
#28193=CARTESIAN_POINT('Ctrl Pts',(-22.6932967144892,-95.147641615416,8.2112042669062));
#28194=CARTESIAN_POINT('Ctrl Pts',(-25.9219649800314,-94.8144595128954,
8.05322110165755));
#28195=CARTESIAN_POINT('Ctrl Pts',(-27.4073472203494,-91.9284646524673,
7.89523793640893));
#28196=CARTESIAN_POINT('Ctrl Pts',(-25.8021483443253,-89.1073557321131,
7.73725477116029));
#28197=CARTESIAN_POINT('Ctrl Pts',(-22.5623398433152,-88.9099734355125,
7.57927160591166));
#28198=CARTESIAN_POINT('Ctrl Pts',(-20.6265379620976,-91.5153509270514,
7.42128844066302));
#28199=CARTESIAN_POINT('Ctrl Pts',(-21.7505813969129,-94.5603215597406,
7.26330527541439));
#28200=CARTESIAN_POINT('Ctrl Pts',(-24.9149242312056,-95.2829932024021,
7.10532211016575));
#28201=CARTESIAN_POINT('Ctrl Pts',(-27.2493995844411,-93.0278779284887,
6.94733894491712));
#28202=CARTESIAN_POINT('Ctrl Pts',(-26.6365585933884,-89.8404423026853,
6.78935577966849));
#28203=CARTESIAN_POINT('Ctrl Pts',(-23.6322689727223,-88.6117992123508,
6.63137261441985));
#28204=CARTESIAN_POINT('Ctrl Pts',(-20.9615239423141,-90.4563698860691,
6.47338944917121));
#28205=CARTESIAN_POINT('Ctrl Pts',(-21.0467804073635,-93.7010657590101,
6.31540628392259));
#28206=CARTESIAN_POINT('Ctrl Pts',(-23.8107078419469,-95.4028369282512,
6.15742311867394));
#28207=CARTESIAN_POINT('Ctrl Pts',(-26.7463297251756,-94.0181188570853,
5.99943995342532));
#28208=CARTESIAN_POINT('Ctrl Pts',(-27.1909368093811,-90.8028980999997,
5.84145678817668));
#28209=CARTESIAN_POINT('Ctrl Pts',(-24.7412552940463,-88.6734896257781,
5.68347362292804));
#28210=CARTESIAN_POINT('Ctrl Pts',(-21.6192299263401,-89.5613396019551,
5.52549045767942));
#28211=CARTESIAN_POINT('Ctrl Pts',(-20.6566442762471,-92.661137795831,5.36750729243077));
#28212=CARTESIAN_POINT('Ctrl Pts',(-22.7265963834907,-95.1612614428767,
5.20952412718215));
#28213=CARTESIAN_POINT('Ctrl Pts',(-25.951569034899,-94.7940130605404,5.0515409619335));
#28214=CARTESIAN_POINT('Ctrl Pts',(-27.4064019604355,-91.8924994667599,
4.89355779668488));
#28215=CARTESIAN_POINT('Ctrl Pts',(-25.7715120400192,-89.0884925256083,
4.73557463143623));
#28216=CARTESIAN_POINT('Ctrl Pts',(-22.529800233879,-88.9253222402167,4.5775914661876));
#28217=CARTESIAN_POINT('Ctrl Pts',(-20.6216097965221,-91.5509896272809,
4.41960830093897));
#28218=CARTESIAN_POINT('Ctrl Pts',(-21.7777345857426,-94.5839247501514,
4.26162513569033));
#28219=CARTESIAN_POINT('Ctrl Pts',(-24.9495299557167,-95.2731519255295,
4.1036419704417));
#28220=CARTESIAN_POINT('Ctrl Pts',(-27.2600692477113,-92.9935185933678,
3.94565880519307));
#28221=CARTESIAN_POINT('Ctrl Pts',(-26.6136144561259,-89.8127299685233,
3.78767563994443));
#28222=CARTESIAN_POINT('Ctrl Pts',(-23.5965221501949,-88.6158699543453,
3.6296924746958));
#28223=CARTESIAN_POINT('Ctrl Pts',(-20.9453980141133,-90.4885313258635,
3.47170930944716));
#28224=CARTESIAN_POINT('Ctrl Pts',(-21.0649021628071,-93.7321465242476,
3.31372614419853));
#28225=CARTESIAN_POINT('Ctrl Pts',(-23.8466401830969,-95.4046453974022,
3.15574297894989));
#28226=CARTESIAN_POINT('Ctrl Pts',(-26.7674808896859,-93.9890153119552,
2.99775981370126));
#28227=CARTESIAN_POINT('Ctrl Pts',(-27.1781217693893,-90.7692791733585,
2.83977664845263));
#28228=CARTESIAN_POINT('Ctrl Pts',(-24.7060981363894,-88.6658514374356,
2.68179348320399));
#28229=CARTESIAN_POINT('Ctrl Pts',(-21.593618559257,-89.5866049274252,2.52381031795535));
#28230=CARTESIAN_POINT('Ctrl Pts',(-20.6638107867396,-92.6964009920719,
2.36582715270672));
#28231=CARTESIAN_POINT('Ctrl Pts',(-22.7600370239625,-95.1745153876391,
2.20784398745808));
#28232=CARTESIAN_POINT('Ctrl Pts',(-25.9809591063933,-94.7732813136335,
2.04986082220945));
#28233=CARTESIAN_POINT('Ctrl Pts',(-27.4050691572154,-91.8564938285714,
1.89187765696081));
#28234=CARTESIAN_POINT('Ctrl Pts',(-25.7406948903597,-89.0700604668216,
1.73389449171218));
#28235=CARTESIAN_POINT('Ctrl Pts',(-22.4973904284657,-88.9407959947845,
1.57591132646355));
#28236=CARTESIAN_POINT('Ctrl Pts',(-20.6171277124371,-91.587122926026,1.41792816121491));
#28237=CARTESIAN_POINT('Ctrl Pts',(-21.8049932574595,-94.606331774166,1.25994499596628));
#28238=CARTESIAN_POINT('Ctrl Pts',(-24.9843140377459,-95.2648119269358,
1.10196183071764));
#28239=CARTESIAN_POINT('Ctrl Pts',(-27.2697677078963,-92.9551896443915,
0.943978665469009));
#28240=CARTESIAN_POINT('Ctrl Pts',(-26.8162121163602,-90.8494815513232,
0.838656555303253));
#28241=CARTESIAN_POINT('Ctrl Pts',(-26.1951971040191,-90.1231365609212,
0.785995500220375));
#28242=CARTESIAN_POINT('Ctrl Pts',(-24.698066426161,-94.6111321859386,10.2140044997796));
#28243=CARTESIAN_POINT('Ctrl Pts',(-25.5620356702265,-94.3801565479507,
10.1613434446967));
#28244=CARTESIAN_POINT('Ctrl Pts',(-27.028047707573,-92.9966202320186,10.056021334531));
#28245=CARTESIAN_POINT('Ctrl Pts',(-26.4897761065395,-90.0038916474845,
9.89803816928236));
#28246=CARTESIAN_POINT('Ctrl Pts',(-23.6887664556898,-88.8263885790956,
9.74005500403371));
#28247=CARTESIAN_POINT('Ctrl Pts',(-21.1721999516397,-90.5251818354797,
9.58207183878509));
#28248=CARTESIAN_POINT('Ctrl Pts',(-21.2194956377293,-93.5627946871602,
9.42408867353644));
#28249=CARTESIAN_POINT('Ctrl Pts',(-23.7893172087738,-95.1823564673149,
9.26610550828781));
#28250=CARTESIAN_POINT('Ctrl Pts',(-26.5499838314408,-93.9156781324104,
9.10812234303918));
#28251=CARTESIAN_POINT('Ctrl Pts',(-26.9978511892308,-90.9112841930657,
8.95013917779054));
#28252=CARTESIAN_POINT('Ctrl Pts',(-24.7265049192209,-88.8944563764859,
8.79215601254191));
#28253=CARTESIAN_POINT('Ctrl Pts',(-21.7962234029808,-89.694431423617,8.63417284729327));
#28254=CARTESIAN_POINT('Ctrl Pts',(-20.8648280297145,-92.5856511406459,
8.47618968204465));
#28255=CARTESIAN_POINT('Ctrl Pts',(-22.7771477187876,-94.9456578035201,
8.318206516796));
#28256=CARTESIAN_POINT('Ctrl Pts',(-25.7986327013197,-94.6338559594106,
8.16022335154737));
#28257=CARTESIAN_POINT('Ctrl Pts',(-27.1886981287095,-91.9330550677512,
8.00224018629873));
#28258=CARTESIAN_POINT('Ctrl Pts',(-25.6865046857824,-89.2929763926183,
7.84425702105011));
#28259=CARTESIAN_POINT('Ctrl Pts',(-22.6545943354517,-89.1082600960069,
7.68627385580146));
#28260=CARTESIAN_POINT('Ctrl Pts',(-20.8430126453538,-91.5464508040853,
7.52829069055284));
#28261=CARTESIAN_POINT('Ctrl Pts',(-21.8949263381463,-94.3960260104053,
7.3703075253042));
#28262=CARTESIAN_POINT('Ctrl Pts',(-24.8562136451879,-95.0723238942441,
7.21232436005556));
#28263=CARTESIAN_POINT('Ctrl Pts',(-27.0408859750062,-92.9619191162963,
7.05434119480693));
#28264=CARTESIAN_POINT('Ctrl Pts',(-26.4673709220948,-89.9790208796034,
6.8963580295583));
#28265=CARTESIAN_POINT('Ctrl Pts',(-23.655866231787,-88.8292196795367,6.73837486430967));
#28266=CARTESIAN_POINT('Ctrl Pts',(-21.1565026125286,-90.5554244585598,
6.58039169906103));
#28267=CARTESIAN_POINT('Ctrl Pts',(-21.2362881797111,-93.5919085587089,
6.4224085338124));
#28268=CARTESIAN_POINT('Ctrl Pts',(-23.8228546986469,-95.1844772615529,
6.26442536856376));
#28269=CARTESIAN_POINT('Ctrl Pts',(-26.5700980525808,-93.8886163947921,
6.10644220331512));
#28270=CARTESIAN_POINT('Ctrl Pts',(-26.9861747497105,-90.8797159955968,
5.94845903806649));
#28271=CARTESIAN_POINT('Ctrl Pts',(-24.6936890243839,-88.8869514260051,
5.79047587281785));
#28272=CARTESIAN_POINT('Ctrl Pts',(-21.772003676811,-89.7178281680943,5.63249270756923));
#28273=CARTESIAN_POINT('Ctrl Pts',(-20.8711870406774,-92.6187126571061,
5.47450954232058));
#28274=CARTESIAN_POINT('Ctrl Pts',(-22.808310551738,-94.9584036481696,5.31652637707196));
#28275=CARTESIAN_POINT('Ctrl Pts',(-25.8263370672835,-94.6147215536259,
5.15854321182331));
#28276=CARTESIAN_POINT('Ctrl Pts',(-27.187813526019,-91.8993977640052,5.00056004657469));
#28277=CARTESIAN_POINT('Ctrl Pts',(-25.6578343097115,-89.2753236359738,
4.84257688132605));
#28278=CARTESIAN_POINT('Ctrl Pts',(-22.6241427891289,-89.1226239696228,
4.68459371607741));
#28279=CARTESIAN_POINT('Ctrl Pts',(-20.8384007196145,-91.5798025728902,
4.52661055082878));
#28280=CARTESIAN_POINT('Ctrl Pts',(-21.9203371098729,-94.4181145867162,
4.36862738558014));
#28281=CARTESIAN_POINT('Ctrl Pts',(-24.8885987242113,-95.0631141310124,
4.21064422033151));
#28282=CARTESIAN_POINT('Ctrl Pts',(-27.0508709671726,-92.9297646158834,
4.05266105508287));
#28283=CARTESIAN_POINT('Ctrl Pts',(-26.445899107565,-89.9530868428382,3.89467788983424));
#28284=CARTESIAN_POINT('Ctrl Pts',(-23.6224132788799,-88.8330292024708,
3.73669472458561));
#28285=CARTESIAN_POINT('Ctrl Pts',(-21.1414114833444,-90.5855221023446,
3.57871155933697));
#28286=CARTESIAN_POINT('Ctrl Pts',(-21.2532470641262,-93.6209948747027,
3.42072839408834));
#28287=CARTESIAN_POINT('Ctrl Pts',(-23.8564812654673,-95.18616968144,3.26274522883971));
#28288=CARTESIAN_POINT('Ctrl Pts',(-26.5898919492202,-93.8613804209116,
3.10476206359106));
#28289=CARTESIAN_POINT('Ctrl Pts',(-26.9741820494077,-90.8482543917338,
2.94677889834244));
#28290=CARTESIAN_POINT('Ctrl Pts',(-24.6607878976183,-88.8798033793578,
2.7887957330938));
#28291=CARTESIAN_POINT('Ctrl Pts',(-21.7480357883011,-89.741472220443,2.63081256784516));
#28292=CARTESIAN_POINT('Ctrl Pts',(-20.8778936769898,-92.6517130179715,
2.47282940259653));
#28293=CARTESIAN_POINT('Ctrl Pts',(-22.8396053100352,-94.9708070887728,
2.3148462373479));
#28294=CARTESIAN_POINT('Ctrl Pts',(-25.8538411811634,-94.595320160609,2.15686307209926));
#28295=CARTESIAN_POINT('Ctrl Pts',(-27.186566248633,-91.8657026036092,1.99887990685063));
#28296=CARTESIAN_POINT('Ctrl Pts',(-25.6289946931135,-89.2580743603465,
1.84089674160199));
#28297=CARTESIAN_POINT('Ctrl Pts',(-22.5938127173193,-89.1371047750836,
1.68291357635336));
#28298=CARTESIAN_POINT('Ctrl Pts',(-20.834206250366,-91.613617201879,1.52493041110472));
#28299=CARTESIAN_POINT('Ctrl Pts',(-21.9458465956616,-94.4390837544956,
1.36694724585609));
#28300=CARTESIAN_POINT('Ctrl Pts',(-24.9211507155708,-95.0553093091994,
1.20896408060745));
#28301=CARTESIAN_POINT('Ctrl Pts',(-27.0599470782477,-92.8938952312942,
1.05098091535882));
#28302=CARTESIAN_POINT('Ctrl Pts',(-26.6354960985062,-90.923310192037,0.945658805193063));
#28303=CARTESIAN_POINT('Ctrl Pts',(-26.054331550342,-90.2435746787731,0.892997750110186));
#28304=CARTESIAN_POINT('Ctrl Pts',(-24.6501999979751,-94.4320868020351,
10.3210067496694));
#28305=CARTESIAN_POINT('Ctrl Pts',(-25.4549268544596,-94.2169491679593,
10.2683456945866));
#28306=CARTESIAN_POINT('Ctrl Pts',(-26.8204144183814,-92.928281963658,10.1630235844208));
#28307=CARTESIAN_POINT('Ctrl Pts',(-26.3190521113202,-90.1407648353735,
10.0050404191722));
#28308=CARTESIAN_POINT('Ctrl Pts',(-23.7101077457725,-89.044003174893,9.84705725392353));
#28309=CARTESIAN_POINT('Ctrl Pts',(-21.3661022550113,-90.6263101452131,
9.6890740886749));
#28310=CARTESIAN_POINT('Ctrl Pts',(-21.4101548750016,-93.4556338255877,
9.53109092342626));
#28311=CARTESIAN_POINT('Ctrl Pts',(-23.8037637317956,-94.964142223518,9.37310775817762));
#28312=CARTESIAN_POINT('Ctrl Pts',(-26.375131391374,-93.7843200462514,9.21512459292899));
#28313=CARTESIAN_POINT('Ctrl Pts',(-26.7922884758791,-90.9859374567588,
9.05714142768035));
#28314=CARTESIAN_POINT('Ctrl Pts',(-24.6766884630223,-89.107403562115,8.89915826243172));
#28315=CARTESIAN_POINT('Ctrl Pts',(-21.9473364063653,-89.8525243049722,
8.74117509718308));
#28316=CARTESIAN_POINT('Ctrl Pts',(-21.0798068316481,-92.5454930307366,
8.58319193193445));
#28317=CARTESIAN_POINT('Ctrl Pts',(-22.8609987230861,-94.7436739916243,
8.42520876668582));
#28318=CARTESIAN_POINT('Ctrl Pts',(-25.6753004226081,-94.4532524059257,
8.26722560143718));
#28319=CARTESIAN_POINT('Ctrl Pts',(-26.9700490370695,-91.9376454830352,
8.10924243618854));
#28320=CARTESIAN_POINT('Ctrl Pts',(-25.5708610272396,-89.4785970531231,
7.95125927093992));
#28321=CARTESIAN_POINT('Ctrl Pts',(-22.7468488275882,-89.3065467565015,
7.79327610569128));
#28322=CARTESIAN_POINT('Ctrl Pts',(-21.0594873286101,-91.577550681119,7.63529294044264));
#28323=CARTESIAN_POINT('Ctrl Pts',(-22.0392712793796,-94.2317304610699,
7.47730977519402));
#28324=CARTESIAN_POINT('Ctrl Pts',(-24.7975030591702,-94.8616545860859,
7.31932660994537));
#28325=CARTESIAN_POINT('Ctrl Pts',(-26.8323723655712,-92.8959603041042,
7.16134344469674));
#28326=CARTESIAN_POINT('Ctrl Pts',(-26.2981832508011,-90.1175994565215,
7.00336027944811));
#28327=CARTESIAN_POINT('Ctrl Pts',(-23.6794634908517,-89.0466401467228,
6.84537711419948));
#28328=CARTESIAN_POINT('Ctrl Pts',(-21.3514812827431,-90.6544790310504,
6.68739394895084));
#28329=CARTESIAN_POINT('Ctrl Pts',(-21.4257959520587,-93.4827513584078,
6.5294107837022));
#28330=CARTESIAN_POINT('Ctrl Pts',(-23.835001555347,-94.9661175948546,6.37142761845357));
#28331=CARTESIAN_POINT('Ctrl Pts',(-26.393866379986,-93.7591139324989,6.21344445320494));
#28332=CARTESIAN_POINT('Ctrl Pts',(-26.7814126900399,-90.9565338911937,
6.0554612879563));
#28333=CARTESIAN_POINT('Ctrl Pts',(-24.6461227547216,-89.1004132262322,
5.89747812270766));
#28334=CARTESIAN_POINT('Ctrl Pts',(-21.9247774272818,-89.8743167342334,
5.73949495745903));
#28335=CARTESIAN_POINT('Ctrl Pts',(-21.0857298051078,-92.5762875183812,
5.5815117922104));
#28336=CARTESIAN_POINT('Ctrl Pts',(-22.8900247199853,-94.7555458534625,
5.42352862696176));
#28337=CARTESIAN_POINT('Ctrl Pts',(-25.7011050996681,-94.4354300467114,
5.26554546171313));
#28338=CARTESIAN_POINT('Ctrl Pts',(-26.9692250916024,-91.9062960612505,
5.1075622964645));
#28339=CARTESIAN_POINT('Ctrl Pts',(-25.5441565794039,-89.4621547463392,
4.94957913121586));
#28340=CARTESIAN_POINT('Ctrl Pts',(-22.7184853443789,-89.319925699029,4.79159596596723));
#28341=CARTESIAN_POINT('Ctrl Pts',(-21.0551916427068,-91.6086155184995,
4.63361280071859));
#28342=CARTESIAN_POINT('Ctrl Pts',(-22.0629396340032,-94.252304423281,4.47562963546995));
#28343=CARTESIAN_POINT('Ctrl Pts',(-24.8276674927059,-94.8530763364951,
4.31764647022132));
#28344=CARTESIAN_POINT('Ctrl Pts',(-26.841672686634,-92.8660106383991,4.15966330497269));
#28345=CARTESIAN_POINT('Ctrl Pts',(-26.2781837590041,-90.0934437171531,
4.00168013972405));
#28346=CARTESIAN_POINT('Ctrl Pts',(-23.648304407565,-89.0501884505964,3.84369697447542));
#28347=CARTESIAN_POINT('Ctrl Pts',(-21.3374249525755,-90.6825128788255,
3.68571380922678));
#28348=CARTESIAN_POINT('Ctrl Pts',(-21.4415919654453,-93.5098432251578,
3.52773064397815));
#28349=CARTESIAN_POINT('Ctrl Pts',(-23.8663223478376,-94.9676939654777,
3.36974747872952));
#28350=CARTESIAN_POINT('Ctrl Pts',(-26.4123030087544,-93.733745529868,3.21176431348088));
#28351=CARTESIAN_POINT('Ctrl Pts',(-26.7702423294261,-90.9272296101091,
3.05378114823225));
#28352=CARTESIAN_POINT('Ctrl Pts',(-24.6154776588472,-89.0937553212802,
2.89579798298361));
#28353=CARTESIAN_POINT('Ctrl Pts',(-21.9024530173453,-89.8963395134605,
2.73781481773497));
#28354=CARTESIAN_POINT('Ctrl Pts',(-21.09197656724,-92.6070250438713,2.57983165248634));
#28355=CARTESIAN_POINT('Ctrl Pts',(-22.9191735961078,-94.7670987899065,
2.42184848723771));
#28356=CARTESIAN_POINT('Ctrl Pts',(-25.7267232559334,-94.4173590075845,
2.26386532198907));
#28357=CARTESIAN_POINT('Ctrl Pts',(-26.9680633400506,-91.8749113786469,
2.10588215674044));
#28358=CARTESIAN_POINT('Ctrl Pts',(-25.5172944958673,-89.4460882538716,
1.94789899149181));
#28359=CARTESIAN_POINT('Ctrl Pts',(-22.6902350061731,-89.3334135553823,
1.78991582624317));
#28360=CARTESIAN_POINT('Ctrl Pts',(-21.051284788295,-91.6401114777323,1.63193266099454));
#28361=CARTESIAN_POINT('Ctrl Pts',(-22.0866999338637,-94.2718357348247,
1.4739494957459));
#28362=CARTESIAN_POINT('Ctrl Pts',(-24.8579873933956,-94.8458066914632,
1.31596633049727));
#28363=CARTESIAN_POINT('Ctrl Pts',(-26.8501264485991,-92.8326008181969,
1.15798316524863));
#28364=CARTESIAN_POINT('Ctrl Pts',(-26.4547800806521,-90.9971388327507,
1.05266105508287));
#28365=CARTESIAN_POINT('Ctrl Pts',(-25.913465996665,-90.364012796625,0.999999999999996));
#28366=CARTESIAN_POINT('Ctrl Pts',(-26.5149492652116,-91.9982505980886,
9.11258330249198));
#28367=CARTESIAN_POINT('Ctrl Pts',(-26.5168562980303,-91.7052247424894,
9.09410267755477));
#28368=CARTESIAN_POINT('Ctrl Pts',(-26.4695028989504,-91.412794780389,9.07562205261756));
#28369=CARTESIAN_POINT('Ctrl Pts',(-26.3701622929854,-91.1392455725669,
9.05714142768035));
#28370=CARTESIAN_POINT('Ctrl Pts',(-26.0870884715935,-90.3597594918776,
9.00448037259747));
#28371=CARTESIAN_POINT('Ctrl Pts',(-25.3818884673079,-89.7335815269963,
8.9518193175146));
#28372=CARTESIAN_POINT('Ctrl Pts',(-24.5743964557222,-89.5446793350319,
8.89915826243172));
#28373=CARTESIAN_POINT('Ctrl Pts',(-23.7669044441366,-89.3557771430674,
8.84649720734884));
#28374=CARTESIAN_POINT('Ctrl Pts',(-22.8571204252509,-89.6041507240198,
8.79383615226596));
#28375=CARTESIAN_POINT('Ctrl Pts',(-22.2576401533552,-90.1771656354567,
8.74117509718308));
#28376=CARTESIAN_POINT('Ctrl Pts',(-21.6581598814595,-90.7501805468937,
8.68851404210021));
#28377=CARTESIAN_POINT('Ctrl Pts',(-21.3689833565538,-91.6478367888151,
8.63585298701733));
#28378=CARTESIAN_POINT('Ctrl Pts',(-21.5212604093406,-92.4630284032571,
8.58319193193445));
#28379=CARTESIAN_POINT('Ctrl Pts',(-21.6735374621274,-93.2782200176992,
8.53053087685158));
#28380=CARTESIAN_POINT('Ctrl Pts',(-22.2672680926068,-94.0109470046617,
8.4778698217687));
#28381=CARTESIAN_POINT('Ctrl Pts',(-23.0331836911001,-94.3289069005266,
8.42520876668582));
#28382=CARTESIAN_POINT('Ctrl Pts',(-23.7990992895934,-94.6468667963914,
8.37254771160294));
#28383=CARTESIAN_POINT('Ctrl Pts',(-24.7371998561007,-94.5500596011586,
8.31988665652006));
#28384=CARTESIAN_POINT('Ctrl Pts',(-25.422041575098,-94.0823881830604,8.26722560143718));
#28385=CARTESIAN_POINT('Ctrl Pts',(-26.0924009622684,-93.6246066015112,
8.21567816845544));
#28386=CARTESIAN_POINT('Ctrl Pts',(-26.5200995637937,-92.8114802627189,
8.16413073547371));
#28387=CARTESIAN_POINT('Ctrl Pts',(-26.5215633824187,-91.9996804087644,
8.11258330249198));
#28388=CARTESIAN_POINT('Ctrl Pts',(-24.7937992825329,-94.9692229537457,
10.));
#28389=CARTESIAN_POINT('Ctrl Pts',(-24.8868523869064,-94.9351837125004,
10.));
#28390=CARTESIAN_POINT('Ctrl Pts',(-24.9778402151602,-94.896376143455,10.));
#28391=CARTESIAN_POINT('Ctrl Pts',(-25.0665542695767,-94.8531284786691,
10.));
#28392=CARTESIAN_POINT('Ctrl Pts',(-25.1572340298607,-94.8089225419499,
10.));
#28393=CARTESIAN_POINT('Ctrl Pts',(-25.2455388043612,-94.7600769477965,
10.));
#28394=CARTESIAN_POINT('Ctrl Pts',(-25.3312170072774,-94.7068966945096,
10.));
#28395=CARTESIAN_POINT('Ctrl Pts',(-25.4136695050773,-94.6557186285851,
10.));
#28396=CARTESIAN_POINT('Ctrl Pts',(-25.4936897697097,-94.6005252759114,
10.));
#28397=CARTESIAN_POINT('Ctrl Pts',(-25.5710205780852,-94.5415583960945,
10.));
#28398=CARTESIAN_POINT('Ctrl Pts',(-25.6386850354138,-94.4899623762547,
10.));
#28399=CARTESIAN_POINT('Ctrl Pts',(-25.7042900873087,-94.4354765516692,
10.));
#28400=CARTESIAN_POINT('Ctrl Pts',(-25.7676387673434,-94.3782501713689,
10.));
#28401=CARTESIAN_POINT('Ctrl Pts',(-25.7817376093299,-94.3655139045221,
10.));
#28402=CARTESIAN_POINT('Ctrl Pts',(-25.7957272919033,-94.3526391912685,
10.));
#28403=CARTESIAN_POINT('Ctrl Pts',(-25.8095861705285,-94.3396461050441,
10.));
#28404=CARTESIAN_POINT('Ctrl Pts',(-25.8820168750965,-94.2717402942496,
10.));
#28405=CARTESIAN_POINT('Ctrl Pts',(-25.9509819060194,-94.2005127260723,
10.));
#28406=CARTESIAN_POINT('Ctrl Pts',(-26.0162413172849,-94.1262540066716,
10.));
#28407=CARTESIAN_POINT('Ctrl Pts',(-26.0811410662591,-94.0524045471867,
10.));
#28408=CARTESIAN_POINT('Ctrl Pts',(-26.1423764147278,-93.9755564586353,
10.));
#28409=CARTESIAN_POINT('Ctrl Pts',(-26.1996677535222,-93.8959688011541,
10.));
#28410=CARTESIAN_POINT('Ctrl Pts',(-26.2548605589272,-93.8192963723989,
10.));
#28411=CARTESIAN_POINT('Ctrl Pts',(-26.3063931619513,-93.7400806580874,
10.));
#28412=CARTESIAN_POINT('Ctrl Pts',(-26.3539706372977,-93.6585396692493,
10.));
#28413=CARTESIAN_POINT('Ctrl Pts',(-26.3739594034205,-93.6242817826455,
10.));
#28414=CARTESIAN_POINT('Ctrl Pts',(-26.3932494781019,-93.5896133547583,
10.));
#28415=CARTESIAN_POINT('Ctrl Pts',(-26.4118163867695,-93.5545502531732,
10.));
#28416=CARTESIAN_POINT('Ctrl Pts',(-26.4248529713493,-93.5299310180799,
10.));
#28417=CARTESIAN_POINT('Ctrl Pts',(-26.4375330011256,-93.5051172053521,
10.));
#28418=CARTESIAN_POINT('Ctrl Pts',(-26.4498475176157,-93.480114301777,10.));
#28419=CARTESIAN_POINT('Ctrl Pts',(-26.4575999795916,-93.4643740119,10.));
#28420=CARTESIAN_POINT('Ctrl Pts',(-26.465208458444,-93.4485566581552,10.));
#28421=CARTESIAN_POINT('Ctrl Pts',(-26.4726610534608,-93.4326847361421,
10.));
#28422=CARTESIAN_POINT('Ctrl Pts',(-26.5147816015831,-93.3429798677795,
10.));
#28423=CARTESIAN_POINT('Ctrl Pts',(-26.5519999407493,-93.2513903181037,
10.));
#28424=CARTESIAN_POINT('Ctrl Pts',(-26.5840244250131,-93.158188555653,10.));
#28425=CARTESIAN_POINT('Ctrl Pts',(-26.6138868935444,-93.0712789687469,
10.));
#28426=CARTESIAN_POINT('Ctrl Pts',(-26.6392329460521,-92.9829667141397,
10.));
#28427=CARTESIAN_POINT('Ctrl Pts',(-26.6597755596719,-92.8934640331731,
10.));
#28428=CARTESIAN_POINT('Ctrl Pts',(-26.6612628263319,-92.8869841199622,
10.));
#28429=CARTESIAN_POINT('Ctrl Pts',(-26.6627248923853,-92.8804979658116,
10.));
#28430=CARTESIAN_POINT('Ctrl Pts',(-26.6641616381052,-92.8740056509469,
10.));
#28431=CARTESIAN_POINT('Ctrl Pts',(-26.6847472407915,-92.7809841702031,
10.));
#28432=CARTESIAN_POINT('Ctrl Pts',(-26.7001390631713,-92.6866969715701,
10.));
#28433=CARTESIAN_POINT('Ctrl Pts',(-26.7104141120204,-92.5915520773693,
10.));
#28434=CARTESIAN_POINT('Ctrl Pts',(-26.7162317525625,-92.5376818912505,
10.));
#28435=CARTESIAN_POINT('Ctrl Pts',(-26.7204081622487,-92.4835369406454,
10.));
#28436=CARTESIAN_POINT('Ctrl Pts',(-26.7229504259501,-92.429193979476,10.));
#28437=CARTESIAN_POINT('Ctrl Pts',(-26.7235977676582,-92.4153565222196,
10.));
#28438=CARTESIAN_POINT('Ctrl Pts',(-26.7241390041195,-92.401507632359,10.));
#28439=CARTESIAN_POINT('Ctrl Pts',(-26.7245740715224,-92.387660812466,10.));
#28440=CARTESIAN_POINT('Ctrl Pts',(-26.727502891379,-92.2944457364089,10.));
#28441=CARTESIAN_POINT('Ctrl Pts',(-26.7256323237373,-92.2011733961936,
10.));
#28442=CARTESIAN_POINT('Ctrl Pts',(-26.7190972361968,-92.1082190602615,
10.));
#28443=CARTESIAN_POINT('Ctrl Pts',(-26.7125517108832,-92.015116258641,10.));
#28444=CARTESIAN_POINT('Ctrl Pts',(-26.7013263747252,-91.9223314983086,
10.));
#28445=CARTESIAN_POINT('Ctrl Pts',(-26.6855058357789,-91.8302540028465,
10.));
#28446=CARTESIAN_POINT('Ctrl Pts',(-26.6699124599891,-91.7394986250815,
10.));
#28447=CARTESIAN_POINT('Ctrl Pts',(-26.6498544352219,-91.6494295035836,
10.));
#28448=CARTESIAN_POINT('Ctrl Pts',(-26.6253697912314,-91.5604445847042,
10.));
#28449=CARTESIAN_POINT('Ctrl Pts',(-26.6161277167569,-91.5268559710524,
10.));
#28450=CARTESIAN_POINT('Ctrl Pts',(-26.606254534053,-91.4934221580589,10.));
#28451=CARTESIAN_POINT('Ctrl Pts',(-26.5957508647621,-91.4601658756637,
10.));
#28452=CARTESIAN_POINT('Ctrl Pts',(-26.5880548971476,-91.4357992219538,
10.));
#28453=CARTESIAN_POINT('Ctrl Pts',(-26.5800204435636,-91.411527889357,10.));
#28454=CARTESIAN_POINT('Ctrl Pts',(-26.5716475015492,-91.3873611147699,
10.));
#28455=CARTESIAN_POINT('Ctrl Pts',(-26.5664800361945,-91.372446289109,10.));
#28456=CARTESIAN_POINT('Ctrl Pts',(-26.5611866348768,-91.3575799762243,
10.));
#28457=CARTESIAN_POINT('Ctrl Pts',(-26.5557684843854,-91.3427662651665,
10.));
#28458=CARTESIAN_POINT('Ctrl Pts',(-26.5240624592361,-91.2560791389784,
10.));
#28459=CARTESIAN_POINT('Ctrl Pts',(-26.4880796645469,-91.1711661845881,
10.));
#28460=CARTESIAN_POINT('Ctrl Pts',(-26.4478804014549,-91.0884282233226,
10.));
#28461=CARTESIAN_POINT('Ctrl Pts',(-26.417730954136,-91.0263747523735,10.));
#28462=CARTESIAN_POINT('Ctrl Pts',(-26.3852087542102,-90.9655451999197,
10.));
#28463=CARTESIAN_POINT('Ctrl Pts',(-26.3503241512938,-90.9061236582789,
10.));
#28464=CARTESIAN_POINT('Ctrl Pts',(-26.3345452493638,-90.879246279731,10.));
#28465=CARTESIAN_POINT('Ctrl Pts',(-26.3182828568508,-90.8526571659942,
10.));
#28466=CARTESIAN_POINT('Ctrl Pts',(-26.3015371511582,-90.8263744220268,
10.));
#28467=CARTESIAN_POINT('Ctrl Pts',(-26.2924151855709,-90.8120573015417,
10.));
#28468=CARTESIAN_POINT('Ctrl Pts',(-26.2831549824545,-90.7978392516847,
10.));
#28469=CARTESIAN_POINT('Ctrl Pts',(-26.2737572212358,-90.783723284612,10.));
#28470=CARTESIAN_POINT('Ctrl Pts',(-26.2261821464327,-90.7122628406009,
10.));
#28471=CARTESIAN_POINT('Ctrl Pts',(-26.175081861218,-90.6434116538366,10.));
#28472=CARTESIAN_POINT('Ctrl Pts',(-26.1204874224643,-90.577523210881,10.));
#28473=CARTESIAN_POINT('Ctrl Pts',(-26.0743569854985,-90.5218497259268,
10.));
#28474=CARTESIAN_POINT('Ctrl Pts',(-26.0257311604375,-90.4682919003903,
10.));
#28475=CARTESIAN_POINT('Ctrl Pts',(-25.9746123907308,-90.41708711057,10.));
#28476=CARTESIAN_POINT('Ctrl Pts',(-25.9557806038368,-90.3982236344852,
10.));
#28477=CARTESIAN_POINT('Ctrl Pts',(-25.9366103467742,-90.3796797449892,
10.));
#28478=CARTESIAN_POINT('Ctrl Pts',(-25.9171117712833,-90.3614597429256,
10.));
#28479=CARTESIAN_POINT('Origin',(-24.,-92.,5.));
#28480=CARTESIAN_POINT('Origin',(-24.,92.,1.));
#28481=CARTESIAN_POINT('Ctrl Pts',(-25.913465996665,93.635987203375,0.999999999999996));
#28482=CARTESIAN_POINT('Ctrl Pts',(-25.9756063047027,93.5775905725192,0.999999999999996));
#28483=CARTESIAN_POINT('Ctrl Pts',(-26.0343713138183,93.5159402490042,0.999999999999997));
#28484=CARTESIAN_POINT('Ctrl Pts',(-26.0897489850044,93.4514126613341,0.999999999999999));
#28485=CARTESIAN_POINT('Ctrl Pts',(-26.1464813764581,93.3853065162965,1.));
#28486=CARTESIAN_POINT('Ctrl Pts',(-26.1996591402971,93.3161801193224,1.));
#28487=CARTESIAN_POINT('Ctrl Pts',(-26.2492404445134,93.2443919311744,1.));
#28488=CARTESIAN_POINT('Ctrl Pts',(-26.2621841917353,93.2256508315686,1.));
#28489=CARTESIAN_POINT('Ctrl Pts',(-26.274882658945,93.2067281064287,1.));
#28490=CARTESIAN_POINT('Ctrl Pts',(-26.2873347259162,93.1876296997784,1.));
#28491=CARTESIAN_POINT('Ctrl Pts',(-26.2974956811164,93.1720452948103,1.));
#28492=CARTESIAN_POINT('Ctrl Pts',(-26.3074930000883,93.1563430141694,1.));
#28493=CARTESIAN_POINT('Ctrl Pts',(-26.3173172475083,93.1405406478853,1.));
#28494=CARTESIAN_POINT('Ctrl Pts',(-26.3647645432756,93.0642213620562,1.));
#28495=CARTESIAN_POINT('Ctrl Pts',(-26.4082282644583,92.985494853327,1.));
#28496=CARTESIAN_POINT('Ctrl Pts',(-26.4476736593442,92.9047536082207,1.));
#28497=CARTESIAN_POINT('Ctrl Pts',(-26.4795145181984,92.8395781778169,1.));
#28498=CARTESIAN_POINT('Ctrl Pts',(-26.5087365606955,92.7730888691482,1.));
#28499=CARTESIAN_POINT('Ctrl Pts',(-26.5353043305085,92.7054742951973,1.));
#28500=CARTESIAN_POINT('Ctrl Pts',(-26.546029034718,92.6781800845433,1.));
#28501=CARTESIAN_POINT('Ctrl Pts',(-26.5563210321205,92.650702354303,1.));
#28502=CARTESIAN_POINT('Ctrl Pts',(-26.5661772000867,92.6230529446547,1.));
#28503=CARTESIAN_POINT('Ctrl Pts',(-26.5713953802244,92.6084144359825,1.));
#28504=CARTESIAN_POINT('Ctrl Pts',(-26.5764908406454,92.5937291337602,0.999999999999998));
#28505=CARTESIAN_POINT('Ctrl Pts',(-26.5814593611535,92.5790106126507,0.999999999999999));
#28506=CARTESIAN_POINT('Ctrl Pts',(-26.6109734289791,92.4915794689899,1.));
#28507=CARTESIAN_POINT('Ctrl Pts',(-26.6360512213471,92.4028684426336,1.));
#28508=CARTESIAN_POINT('Ctrl Pts',(-26.6566599711623,92.3132752268106,1.));
#28509=CARTESIAN_POINT('Ctrl Pts',(-26.6775876501422,92.2222955178845,1.));
#28510=CARTESIAN_POINT('Ctrl Pts',(-26.6939073958785,92.1304052976179,1.));
#28511=CARTESIAN_POINT('Ctrl Pts',(-26.7055430518716,92.0379878724461,1.));
#28512=CARTESIAN_POINT('Ctrl Pts',(-26.7170875469971,91.9462945020825,1.00000000000001));
#28513=CARTESIAN_POINT('Ctrl Pts',(-26.7240214047279,91.854081225586,1.00000000000001));
#28514=CARTESIAN_POINT('Ctrl Pts',(-26.7262232901922,91.7617032514415,1.00000000000001));
#28515=CARTESIAN_POINT('Ctrl Pts',(-26.7273184961007,91.7157549472591,1.00000000000001));
#28516=CARTESIAN_POINT('Ctrl Pts',(-26.7272422423285,91.6697656845161,1.00000000000001));
#28517=CARTESIAN_POINT('Ctrl Pts',(-26.72597480777,91.6237784805461,1.00000000000001));
#28518=CARTESIAN_POINT('Ctrl Pts',(-26.7255580393425,91.6086565836768,1.00000000000001));
#28519=CARTESIAN_POINT('Ctrl Pts',(-26.7250123597643,91.5935330587279,1.));
#28520=CARTESIAN_POINT('Ctrl Pts',(-26.7243372523629,91.5784152587756,1.));
#28521=CARTESIAN_POINT('Ctrl Pts',(-26.7200633703958,91.4827094607578,1.));
#28522=CARTESIAN_POINT('Ctrl Pts',(-26.7106224530131,91.3875708354282,1.00000000000001));
#28523=CARTESIAN_POINT('Ctrl Pts',(-26.6959503279345,91.2933977109171,1.00000000000001));
#28524=CARTESIAN_POINT('Ctrl Pts',(-26.6917956796564,91.2667310755459,1.00000000000001));
#28525=CARTESIAN_POINT('Ctrl Pts',(-26.6872212841807,91.2401417271289,1.00000000000001));
#28526=CARTESIAN_POINT('Ctrl Pts',(-26.6822249702578,91.2136384506289,1.));
#28527=CARTESIAN_POINT('Ctrl Pts',(-26.6652600471296,91.1236468977731,1.));
#28528=CARTESIAN_POINT('Ctrl Pts',(-26.6434348327882,91.0346478147219,1.));
#28529=CARTESIAN_POINT('Ctrl Pts',(-26.6170519644759,90.9468734390352,1.));
#28530=CARTESIAN_POINT('Ctrl Pts',(-26.5900726212499,90.8571146235775,1.));
#28531=CARTESIAN_POINT('Ctrl Pts',(-26.5583270022612,90.7686358185392,1.00000000000001));
#28532=CARTESIAN_POINT('Ctrl Pts',(-26.5220844975705,90.6816890800664,1.00000000000001));
#28533=CARTESIAN_POINT('Ctrl Pts',(-26.5094176334725,90.6513009341755,1.00000000000001));
#28534=CARTESIAN_POINT('Ctrl Pts',(-26.4962010035771,90.6211000168169,1.));
#28535=CARTESIAN_POINT('Ctrl Pts',(-26.4824446757821,90.5910974447628,1.));
#28536=CARTESIAN_POINT('Ctrl Pts',(-26.4754977538534,90.5759461973644,1.));
#28537=CARTESIAN_POINT('Ctrl Pts',(-26.4684131851587,90.5608455364142,1.));
#28538=CARTESIAN_POINT('Ctrl Pts',(-26.4611921989836,90.545796919332,1.));
#28539=CARTESIAN_POINT('Ctrl Pts',(-26.455182228529,90.5332720727456,1.));
#28540=CARTESIAN_POINT('Ctrl Pts',(-26.4490796038181,90.5207872118101,1.));
#28541=CARTESIAN_POINT('Ctrl Pts',(-26.4428889235851,90.5083503619119,1.));
#28542=CARTESIAN_POINT('Ctrl Pts',(-26.3999256383549,90.4220386951104,1.));
#28543=CARTESIAN_POINT('Ctrl Pts',(-26.352675311748,90.3379337033055,1.));
#28544=CARTESIAN_POINT('Ctrl Pts',(-26.3014800112192,90.2562854651096,1.));
#28545=CARTESIAN_POINT('Ctrl Pts',(-26.2492799088519,90.1730347302195,1.));
#28546=CARTESIAN_POINT('Ctrl Pts',(-26.1929781409368,90.0923373579129,1.));
#28547=CARTESIAN_POINT('Ctrl Pts',(-26.1328823971401,90.014465764712,1.));
#28548=CARTESIAN_POINT('Ctrl Pts',(-26.0723186336165,89.935987715222,1.));
#28549=CARTESIAN_POINT('Ctrl Pts',(-26.0079011072123,89.8603787928957,1.));
#28550=CARTESIAN_POINT('Ctrl Pts',(-25.9398956031168,89.787937415356,1.));
#28551=CARTESIAN_POINT('Ctrl Pts',(-25.9029689988626,89.7486021568998,1.));
#28552=CARTESIAN_POINT('Ctrl Pts',(-25.8649836968098,89.7102012386594,0.999999999999998));
#28553=CARTESIAN_POINT('Ctrl Pts',(-25.8259770082825,89.6727861936411,0.999999999999997));
#28554=CARTESIAN_POINT('Ctrl Pts',(-25.8138450071499,89.6611492312207,0.999999999999997));
#28555=CARTESIAN_POINT('Ctrl Pts',(-25.8016141768636,89.6496076606791,1.));
#28556=CARTESIAN_POINT('Ctrl Pts',(-25.789285575206,89.6381630971647,1.));
#28557=CARTESIAN_POINT('Ctrl Pts',(-25.7779997494658,89.6276865359874,1.));
#28558=CARTESIAN_POINT('Ctrl Pts',(-25.7666377256336,89.6172966286238,1.));
#28559=CARTESIAN_POINT('Ctrl Pts',(-25.7552049288473,89.6069982204744,1.));
#28560=CARTESIAN_POINT('Ctrl Pts',(-25.679395860332,89.5387111037176,1.));
#28561=CARTESIAN_POINT('Ctrl Pts',(-25.600420502922,89.4743910090163,1.));
#28562=CARTESIAN_POINT('Ctrl Pts',(-25.5186050207122,89.4143205615864,1.));
#28563=CARTESIAN_POINT('Ctrl Pts',(-25.4367186080971,89.3541980357348,1.));
#28564=CARTESIAN_POINT('Ctrl Pts',(-25.3519865671594,89.2983316916956,1.));
#28565=CARTESIAN_POINT('Ctrl Pts',(-25.2646909477799,89.2470310937083,1.));
#28566=CARTESIAN_POINT('Ctrl Pts',(-25.1791591002471,89.1967670030634,1.));
#28567=CARTESIAN_POINT('Ctrl Pts',(-25.091165555463,89.1508853502904,1.));
#28568=CARTESIAN_POINT('Ctrl Pts',(-25.0009418604243,89.1097134462671,1.));
#28569=CARTESIAN_POINT('Ctrl Pts',(-24.9631524549254,89.0924689543891,1.));
#28570=CARTESIAN_POINT('Ctrl Pts',(-24.9249714626436,89.0760511834599,1.));
#28571=CARTESIAN_POINT('Ctrl Pts',(-24.8864145036881,89.0604865582877,1.));
#28572=CARTESIAN_POINT('Ctrl Pts',(-24.8564008056108,89.0483706660271,1.));
#28573=CARTESIAN_POINT('Ctrl Pts',(-24.8261592741353,89.0367717663531,1.));
#28574=CARTESIAN_POINT('Ctrl Pts',(-24.7957016814435,89.0256872793281,1.));
#28575=CARTESIAN_POINT('Ctrl Pts',(-23.2062007174672,89.0307770462543,0.999999999999999));
#28576=CARTESIAN_POINT('Ctrl Pts',(-23.1113643609077,89.065468609115,0.999999999999999));
#28577=CARTESIAN_POINT('Ctrl Pts',(-23.018571234946,89.1051505773298,0.999999999999999));
#28578=CARTESIAN_POINT('Ctrl Pts',(-22.9280622736109,89.1495027068318,1.));
#28579=CARTESIAN_POINT('Ctrl Pts',(-22.836281839029,89.1944778966946,1.));
#28580=CARTESIAN_POINT('Ctrl Pts',(-22.7468495274982,89.2442560843952,0.999999999999997));
#28581=CARTESIAN_POINT('Ctrl Pts',(-22.6600505960784,89.2985440193305,0.999999999999997));
#28582=CARTESIAN_POINT('Ctrl Pts',(-22.6355418278746,89.3138728994427,0.999999999999996));
#28583=CARTESIAN_POINT('Ctrl Pts',(-22.6112432552978,89.3295615450764,1.));
#28584=CARTESIAN_POINT('Ctrl Pts',(-22.5871618961201,89.3456038099341,1.));
#28585=CARTESIAN_POINT('Ctrl Pts',(-22.5678312416192,89.3584813006558,1.));
#28586=CARTESIAN_POINT('Ctrl Pts',(-22.5486384464619,89.3715882773608,0.999999999999998));
#28587=CARTESIAN_POINT('Ctrl Pts',(-22.5296064292129,89.3849077949563,0.999999999999998));
#28588=CARTESIAN_POINT('Ctrl Pts',(-22.446898789183,89.4427905644099,1.));
#28589=CARTESIAN_POINT('Ctrl Pts',(-22.3671459828654,89.5047351114195,0.999999999999997));
#28590=CARTESIAN_POINT('Ctrl Pts',(-22.2906143664206,89.5704442021524,0.999999999999998));
#28591=CARTESIAN_POINT('Ctrl Pts',(-22.2316015136182,89.6211119010635,0.999999999999999));
#28592=CARTESIAN_POINT('Ctrl Pts',(-22.1745045554968,89.6740188394976,0.999999999999999));
#28593=CARTESIAN_POINT('Ctrl Pts',(-22.1194631966057,89.7290405250296,1.));
#28594=CARTESIAN_POINT('Ctrl Pts',(-22.0901430624395,89.7583501793395,1.));
#28595=CARTESIAN_POINT('Ctrl Pts',(-22.0614065053773,89.7882600668129,1.));
#28596=CARTESIAN_POINT('Ctrl Pts',(-22.0332766723516,89.8187522038962,1.));
#28597=CARTESIAN_POINT('Ctrl Pts',(-22.0236426842444,89.8291952408583,1.));
#28598=CARTESIAN_POINT('Ctrl Pts',(-22.014080660821,89.8397057922762,1.));
#28599=CARTESIAN_POINT('Ctrl Pts',(-22.0045980888106,89.8502756076143,1.));
#28600=CARTESIAN_POINT('Ctrl Pts',(-21.9388055958393,89.9236116709296,1.));
#28601=CARTESIAN_POINT('Ctrl Pts',(-21.8767453524491,89.9998940820391,1.));
#28602=CARTESIAN_POINT('Ctrl Pts',(-21.8186611502822,90.0788444257391,1.));
#28603=CARTESIAN_POINT('Ctrl Pts',(-21.7610833540022,90.157106442539,1.));
#28604=CARTESIAN_POINT('Ctrl Pts',(-21.7074121340599,90.2379908580803,1.));
#28605=CARTESIAN_POINT('Ctrl Pts',(-21.6579307654416,90.3212488810837,1.));
#28606=CARTESIAN_POINT('Ctrl Pts',(-21.6098823874139,90.4020957346531,1.));
#28607=CARTESIAN_POINT('Ctrl Pts',(-21.5657844914906,90.4851814058657,1.));
#28608=CARTESIAN_POINT('Ctrl Pts',(-21.5259442417593,90.5702884177283,1.));
#28609=CARTESIAN_POINT('Ctrl Pts',(-21.5051329728217,90.6147455916742,1.));
#28610=CARTESIAN_POINT('Ctrl Pts',(-21.4854842990003,90.659754434822,1.));
#28611=CARTESIAN_POINT('Ctrl Pts',(-21.4670477073908,90.7052841842656,1.));
#28612=CARTESIAN_POINT('Ctrl Pts',(-21.4599070329778,90.7229183068716,1.));
#28613=CARTESIAN_POINT('Ctrl Pts',(-21.452948225379,90.7406305688681,1.));
#28614=CARTESIAN_POINT('Ctrl Pts',(-21.4461743283707,90.7584191738098,1.));
#28615=CARTESIAN_POINT('Ctrl Pts',(-21.441020443057,90.7719535440028,1.));
#28616=CARTESIAN_POINT('Ctrl Pts',(-21.4359736403243,90.7855322279792,1.));
#28617=CARTESIAN_POINT('Ctrl Pts',(-21.4310400911309,90.7991405304999,1.));
#28618=CARTESIAN_POINT('Ctrl Pts',(-21.3993682454182,90.8865015845694,1.));
#28619=CARTESIAN_POINT('Ctrl Pts',(-21.372305110326,90.975223579926,1.));
#28620=CARTESIAN_POINT('Ctrl Pts',(-21.3501019716912,91.0650831130208,1.));
#28621=CARTESIAN_POINT('Ctrl Pts',(-21.3450993725627,91.085329404743,1.));
#28622=CARTESIAN_POINT('Ctrl Pts',(-21.3403436950143,91.1056334832557,1.));
#28623=CARTESIAN_POINT('Ctrl Pts',(-21.3358381789014,91.1259928495363,1.));
#28624=CARTESIAN_POINT('Ctrl Pts',(-21.3154926547754,91.21792948176,1.));
#28625=CARTESIAN_POINT('Ctrl Pts',(-21.3002441342106,91.3109938333365,1.));
#28626=CARTESIAN_POINT('Ctrl Pts',(-21.2899827069894,91.4047941591649,1.));
#28627=CARTESIAN_POINT('Ctrl Pts',(-21.2792695744501,91.5027235505803,1.));
#28628=CARTESIAN_POINT('Ctrl Pts',(-21.2739922714095,91.6014563765819,0.999999999999999));
#28629=CARTESIAN_POINT('Ctrl Pts',(-21.2740832157028,91.7005321536462,0.999999999999999));
#28630=CARTESIAN_POINT('Ctrl Pts',(-21.2741183389869,91.7387958702903,0.999999999999999));
#28631=CARTESIAN_POINT('Ctrl Pts',(-21.2749547528149,91.7771104872721,0.999999999999999));
#28632=CARTESIAN_POINT('Ctrl Pts',(-21.2765906985084,91.8154482999678,0.999999999999999));
#28633=CARTESIAN_POINT('Ctrl Pts',(-21.277178303569,91.8292186181647,0.999999999999999));
#28634=CARTESIAN_POINT('Ctrl Pts',(-21.2778690508016,91.8429901308369,0.999999999999999));
#28635=CARTESIAN_POINT('Ctrl Pts',(-21.2786619686978,91.8567498857155,0.999999999999999));
#28636=CARTESIAN_POINT('Ctrl Pts',(-21.2840135874423,91.9496182173293,1.));
#28637=CARTESIAN_POINT('Ctrl Pts',(-21.2940209180043,92.0420994637286,1.));
#28638=CARTESIAN_POINT('Ctrl Pts',(-21.3085609026778,92.1338217237554,1.));
#28639=CARTESIAN_POINT('Ctrl Pts',(-21.3230638385398,92.2253102695935,1.));
#28640=CARTESIAN_POINT('Ctrl Pts',(-21.3420767703985,92.3160446363129,0.999999999999998));
#28641=CARTESIAN_POINT('Ctrl Pts',(-21.3655261680114,92.4056386468098,0.999999999999998));
#28642=CARTESIAN_POINT('Ctrl Pts',(-21.3885742626337,92.4936993836192,0.999999999999998));
#28643=CARTESIAN_POINT('Ctrl Pts',(-21.4159087427557,92.5806592446602,0.999999999999998));
#28644=CARTESIAN_POINT('Ctrl Pts',(-21.4475001239804,92.6661223199064,0.999999999999998));
#28645=CARTESIAN_POINT('Ctrl Pts',(-21.4633626089743,92.7090345540687,0.999999999999998));
#28646=CARTESIAN_POINT('Ctrl Pts',(-21.4802989345861,92.7515688848743,0.999999999999994));
#28647=CARTESIAN_POINT('Ctrl Pts',(-21.4983087570456,92.7936714133834,0.999999999999994));
#28648=CARTESIAN_POINT('Ctrl Pts',(-21.5036080709844,92.8060599039801,0.999999999999994));
#28649=CARTESIAN_POINT('Ctrl Pts',(-21.5090003429253,92.8184109900054,0.999999999999999));
#28650=CARTESIAN_POINT('Ctrl Pts',(-21.5144855985927,92.8307232495397,0.999999999999999));
#28651=CARTESIAN_POINT('Ctrl Pts',(-21.5200790278412,92.8432783165719,0.999999999999999));
#28652=CARTESIAN_POINT('Ctrl Pts',(-21.5257654643176,92.8557847221215,0.999999999999994));
#28653=CARTESIAN_POINT('Ctrl Pts',(-21.5315436189536,92.8682391310481,0.999999999999995));
#28654=CARTESIAN_POINT('Ctrl Pts',(-21.5690290041703,92.9490362619096,0.999999999999995));
#28655=CARTESIAN_POINT('Ctrl Pts',(-21.6103840907841,93.0276765322135,1.));
#28656=CARTESIAN_POINT('Ctrl Pts',(-21.6555390550696,93.1038122346988,1.));
#28657=CARTESIAN_POINT('Ctrl Pts',(-21.6999358276416,93.1786695515261,1.));
#28658=CARTESIAN_POINT('Ctrl Pts',(-21.7480063970068,93.251106371718,0.999999999999998));
#28659=CARTESIAN_POINT('Ctrl Pts',(-21.7997205984681,93.3207580281866,0.999999999999998));
#28660=CARTESIAN_POINT('Ctrl Pts',(-21.8498548445433,93.3882817100044,0.999999999999997));
#28661=CARTESIAN_POINT('Ctrl Pts',(-21.9034139287086,93.4531882520499,0.999999999999996));
#28662=CARTESIAN_POINT('Ctrl Pts',(-21.960398059015,93.5151051166907,0.999999999999996));
#28663=CARTESIAN_POINT('Ctrl Pts',(-21.9815871896649,93.5381284484017,0.999999999999995));
#28664=CARTESIAN_POINT('Ctrl Pts',(-22.0032501397421,93.5607379645122,0.999999999999999));
#28665=CARTESIAN_POINT('Ctrl Pts',(-22.0253877587029,93.5829128445691,0.999999999999999));
#28666=CARTESIAN_POINT('Ctrl Pts',(-22.0442145502047,93.6017713245233,0.999999999999999));
#28667=CARTESIAN_POINT('Ctrl Pts',(-22.0633846686702,93.6203154277105,0.999999999999998));
#28668=CARTESIAN_POINT('Ctrl Pts',(-22.0828883826538,93.638540237813,0.999999999999998));
#28669=CARTESIAN_POINT('Origin',(-24.,92.,12.2084234471775));
#28670=CARTESIAN_POINT('Ctrl Pts',(-27.076766805402,92.0019372679896,9.70842344717746));
#28671=CARTESIAN_POINT('Ctrl Pts',(-27.0777009893786,92.1261018275903,9.70197366100994));
#28672=CARTESIAN_POINT('Ctrl Pts',(-27.0146667615987,93.2631137100916,9.64286281975954));
#28673=CARTESIAN_POINT('Ctrl Pts',(-25.5990316467514,95.2555126958587,9.53109092342626));
#28674=CARTESIAN_POINT('Ctrl Pts',(-22.1476051047098,95.1179530605298,9.37310775817762));
#28675=CARTESIAN_POINT('Ctrl Pts',(-20.3764282219686,92.1527149914235,9.215124592929));
#28676=CARTESIAN_POINT('Ctrl Pts',(-21.8919231533181,89.0487577497888,9.05714142768035));
#28677=CARTESIAN_POINT('Ctrl Pts',(-25.3195311476576,88.6217766146216,8.89915826243172));
#28678=CARTESIAN_POINT('Ctrl Pts',(-26.9608439554881,90.5621019356809,8.78291893559742));
#28679=CARTESIAN_POINT('Ctrl Pts',(-27.0762792831289,91.7866862376245,8.719340663846));
#28680=CARTESIAN_POINT('Ctrl Pts',(-27.0743674416594,91.9973209105276,8.70842344717745));
#28681=CARTESIAN_POINT('Ctrl Pts',(-27.0702888275776,91.9968971804148,9.79157655282255));
#28682=CARTESIAN_POINT('Ctrl Pts',(-27.0652853128242,92.6903808619892,9.75572892504928));
#28683=CARTESIAN_POINT('Ctrl Pts',(-26.4922439119073,94.4123573994235,9.66722024219312));
#28684=CARTESIAN_POINT('Ctrl Pts',(-23.6460838986402,95.6088399383518,9.5260505042541));
#28685=CARTESIAN_POINT('Ctrl Pts',(-20.7843955634607,93.6770749374766,9.36806733900546));
#28686=CARTESIAN_POINT('Ctrl Pts',(-20.8381773234134,90.2228835564638,9.21008417375683));
#28687=CARTESIAN_POINT('Ctrl Pts',(-23.760424197283,88.3812153351417,9.05210100850819));
#28688=CARTESIAN_POINT('Ctrl Pts',(-26.5324622678489,89.6531111499585,8.91259846819677));
#28689=CARTESIAN_POINT('Ctrl Pts',(-27.0660796534741,91.3404823888654,8.82575698296822));
#28690=CARTESIAN_POINT('Ctrl Pts',(-27.0703857423214,92.0021357609841,8.79157655282255));
#28691=CARTESIAN_POINT('Ctrl Pts',(-22.0865340033349,93.6359872033749,10.));
#28692=CARTESIAN_POINT('Ctrl Pts',(-21.5452199193478,93.0028611672492,9.94733894491712));
#28693=CARTESIAN_POINT('Ctrl Pts',(-21.1498718103827,91.167401053521,9.84201683475137));
#28694=CARTESIAN_POINT('Ctrl Pts',(-23.1420133042203,89.1541928650905,9.68403366950274));
#28695=CARTESIAN_POINT('Ctrl Pts',(-25.9132996010903,89.7281648944129,9.52605050425409));
#28696=CARTESIAN_POINT('Ctrl Pts',(-26.9487151037096,92.3598882319117,9.36806733900546));
#28697=CARTESIAN_POINT('Ctrl Pts',(-25.3097648188374,94.6665863711807,9.21008417375683));
#28698=CARTESIAN_POINT('Ctrl Pts',(-22.4827056616583,94.5539114461962,9.05210100850819));
#28699=CARTESIAN_POINT('Ctrl Pts',(-21.0319368956584,92.1250886581775,8.89411784325956));
#28700=CARTESIAN_POINT('Ctrl Pts',(-22.2732768955518,89.5826411697067,8.73613467801092));
#28701=CARTESIAN_POINT('Ctrl Pts',(-25.0808263101441,89.2329014567464,8.57815151276229));
#28702=CARTESIAN_POINT('Ctrl Pts',(-26.9080231896089,91.3929749996272,8.42016834751365));
#28703=CARTESIAN_POINT('Ctrl Pts',(-26.0975468057329,94.1036603137053,8.26218518226502));
#28704=CARTESIAN_POINT('Ctrl Pts',(-23.3845223931579,94.9062444322857,8.10420201701639));
#28705=CARTESIAN_POINT('Ctrl Pts',(-21.2297579033362,93.0727703008244,7.94621885176775));
#28706=CARTESIAN_POINT('Ctrl Pts',(-21.5876971940873,90.2662546152948,7.78823568651912));
#28707=CARTESIAN_POINT('Ctrl Pts',(-24.1336776409024,89.0323062843058,7.63025252127048));
#28708=CARTESIAN_POINT('Ctrl Pts',(-26.5584078194921,90.4901569016087,7.47226935602185));
#28709=CARTESIAN_POINT('Ctrl Pts',(-26.6625748235914,93.3174870105019,7.31428619077321));
#28710=CARTESIAN_POINT('Ctrl Pts',(-24.3516955628713,94.9498113013859,7.15630302552459));
#28711=CARTESIAN_POINT('Ctrl Pts',(-21.7218164325105,93.9065561225942,6.99831986027594));
#28712=CARTESIAN_POINT('Ctrl Pts',(-21.1583275522511,91.1339894343907,6.84033669502731));
#28713=CARTESIAN_POINT('Ctrl Pts',(-23.1723325768719,89.1469239033541,6.68235352977868));
#28714=CARTESIAN_POINT('Ctrl Pts',(-25.9370602031581,89.7476957660557,6.52437036453004));
#28715=CARTESIAN_POINT('Ctrl Pts',(-26.9448081097383,92.3913844486005,6.36638719928141));
#28716=CARTESIAN_POINT('Ctrl Pts',(-25.2815145478907,94.6800740756701,6.20840403403277));
#28717=CARTESIAN_POINT('Ctrl Pts',(-22.4558435504054,94.5378450403174,6.05042086878414));
#28718=CARTESIAN_POINT('Ctrl Pts',(-21.0307751580051,92.0937039308721,5.8924377035355));
#28719=CARTESIAN_POINT('Ctrl Pts',(-22.2988950433351,89.5645701580226,5.73445453828688));
#28720=CARTESIAN_POINT('Ctrl Pts',(-25.1099751867048,89.244454378182,5.57647137303823));
#28721=CARTESIAN_POINT('Ctrl Pts',(-26.9142699499045,91.4237125300643,5.4184882077896));
#28722=CARTESIAN_POINT('Ctrl Pts',(-26.0752223982648,94.1256830870714,5.26050504254097));
#28723=CARTESIAN_POINT('Ctrl Pts',(-23.3538772995946,94.8995865300144,5.10252187729233));
#28724=CARTESIAN_POINT('Ctrl Pts',(-21.2185875437792,93.0434660210873,4.9445387120437));
#28725=CARTESIAN_POINT('Ctrl Pts',(-21.606133821254,90.2408862153809,4.78655554679506));
#28726=CARTESIAN_POINT('Ctrl Pts',(-24.1649984307827,89.0338826544914,4.62857238154643));
#28727=CARTESIAN_POINT('Ctrl Pts',(-26.5742038315408,90.5172487662401,4.47058921629779));
#28728=CARTESIAN_POINT('Ctrl Pts',(-26.6485184946104,93.3455208558374,4.31260605104916));
#28729=CARTESIAN_POINT('Ctrl Pts',(-24.3205364822007,94.9533596050058,4.15462288580052));
#28730=CARTESIAN_POINT('Ctrl Pts',(-21.7018169423985,93.8824003852299,3.99663972055189));
#28731=CARTESIAN_POINT('Ctrl Pts',(-21.1676278725257,91.1040397712239,3.83865655530325));
#28732=CARTESIAN_POINT('Ctrl Pts',(-23.2024970078836,89.1383456544602,3.68067339005462));
#28733=CARTESIAN_POINT('Ctrl Pts',(-25.9607285557694,89.768269726576,3.52269022480599));
#28734=CARTESIAN_POINT('Ctrl Pts',(-26.9405124242392,92.4224492832981,3.36470705955735));
#28735=CARTESIAN_POINT('Ctrl Pts',(-25.2531510669841,94.6934530172095,3.20672389430872));
#28736=CARTESIAN_POINT('Ctrl Pts',(-22.4291391049686,94.5214027346518,3.04874072906009));
#28737=CARTESIAN_POINT('Ctrl Pts',(-21.029951212319,92.0623545122335,2.89075756381144));
#28738=CARTESIAN_POINT('Ctrl Pts',(-22.3246997187609,89.5467477993204,2.73277439856282));
#28739=CARTESIAN_POINT('Ctrl Pts',(-25.1390011801809,89.2563262409203,2.57479123331418));
#28740=CARTESIAN_POINT('Ctrl Pts',(-26.9201929246498,91.4545070114807,2.41680806806554));
#28741=CARTESIAN_POINT('Ctrl Pts',(-26.0526634178927,94.1474755214498,2.25882490281691));
#28742=CARTESIAN_POINT('Ctrl Pts',(-23.3233115994341,94.892596181515,2.10084173756827));
#28743=CARTESIAN_POINT('Ctrl Pts',(-21.2077117493853,93.0140624829425,1.94285857231964));
#28744=CARTESIAN_POINT('Ctrl Pts',(-21.6248688237331,90.215680056917,1.78487540707101));
#28745=CARTESIAN_POINT('Ctrl Pts',(-24.1962362281276,89.0358581128856,1.62689224182237));
#28746=CARTESIAN_POINT('Ctrl Pts',(-26.5898449391916,90.5443661358105,1.46890907657374));
#28747=CARTESIAN_POINT('Ctrl Pts',(-26.6338974915197,93.3736900328969,1.31092591132511));
#28748=CARTESIAN_POINT('Ctrl Pts',(-24.2898922274084,94.9559960431297,1.15294274607647));
#28749=CARTESIAN_POINT('Ctrl Pts',(-21.6809482123999,93.8592359252299,0.994959580827835));
#28750=CARTESIAN_POINT('Ctrl Pts',(-21.1795852070609,91.0717155076706,0.836976415579202));
#28751=CARTESIAN_POINT('Ctrl Pts',(-22.5450731455404,89.7830508320407,0.731654305413445));
#28752=CARTESIAN_POINT('Ctrl Pts',(-23.3498000020249,89.5679131979649,0.678993250330566));
#28753=CARTESIAN_POINT('Ctrl Pts',(-21.9456684496579,93.7564253212268,10.1070022498898));
#28754=CARTESIAN_POINT('Ctrl Pts',(-21.3645039014938,93.0766898079629,10.0543411948069));
#28755=CARTESIAN_POINT('Ctrl Pts',(-20.9400510525638,91.106106778216,9.94901908464118));
#28756=CARTESIAN_POINT('Ctrl Pts',(-23.0788500334022,88.9446902147085,9.79103591939254));
#28757=CARTESIAN_POINT('Ctrl Pts',(-26.0541529050567,89.5609169210655,9.63305275414391));
#28758=CARTESIAN_POINT('Ctrl Pts',(-27.1657936336882,92.3863824863894,9.47506958889527));
#28759=CARTESIAN_POINT('Ctrl Pts',(-25.4061870948087,94.8628951460734,9.31708642364664));
#28760=CARTESIAN_POINT('Ctrl Pts',(-22.3710054760088,94.7419253176408,9.159103258398));
#28761=CARTESIAN_POINT('Ctrl Pts',(-20.8134340044285,92.134297435926,9.00112009314937));
#28762=CARTESIAN_POINT('Ctrl Pts',(-22.1461589814739,89.4046800297342,8.84313692790073));
#28763=CARTESIAN_POINT('Ctrl Pts',(-25.1603945893153,89.0291931760381,8.6851537626521));
#28764=CARTESIAN_POINT('Ctrl Pts',(-27.1221060619588,91.3482870287292,8.52717059740346));
#28765=CARTESIAN_POINT('Ctrl Pts',(-26.2519640217524,94.2585275939991,8.36918743215483));
#28766=CARTESIAN_POINT('Ctrl Pts',(-23.3392121582153,95.1201963560661,8.2112042669062));
#28767=CARTESIAN_POINT('Ctrl Pts',(-21.0258182004901,93.1517455126427,8.05322110165756));
#28768=CARTESIAN_POINT('Ctrl Pts',(-21.4101082685543,90.1386197349378,7.89523793640893));
#28769=CARTESIAN_POINT('Ctrl Pts',(-24.1435187224439,88.813830586732,7.73725477116029));
#28770=CARTESIAN_POINT('Ctrl Pts',(-26.7467527049787,90.3790052613962,7.57927160591167));
#28771=CARTESIAN_POINT('Ctrl Pts',(-26.8585882763444,93.4144777788355,7.42128844066302));
#28772=CARTESIAN_POINT('Ctrl Pts',(-24.3775866893799,95.1669705312529,7.2633052754144));
#28773=CARTESIAN_POINT('Ctrl Pts',(-21.5541010980485,94.0469129851116,7.10532211016575));
#28774=CARTESIAN_POINT('Ctrl Pts',(-20.9491292892987,91.0702354622651,6.94733894491712));
#28775=CARTESIAN_POINT('Ctrl Pts',(-23.1114013504886,88.936886126494,6.78935577966849));
#28776=CARTESIAN_POINT('Ctrl Pts',(-26.0796627153006,89.5818856165591,6.63137261441985));
#28777=CARTESIAN_POINT('Ctrl Pts',(-27.1615990146061,92.4201973917876,6.47338944917122));
#28778=CARTESIAN_POINT('Ctrl Pts',(-25.3758570952097,94.8773757884901,6.31540628392258));
#28779=CARTESIAN_POINT('Ctrl Pts',(-22.342165829654,94.7246761349771,6.15742311867395));
#28780=CARTESIAN_POINT('Ctrl Pts',(-20.8121867419641,92.1006022275374,5.99943995342532));
#28781=CARTESIAN_POINT('Ctrl Pts',(-22.1736630862473,89.3852786661803,5.84145678817668));
#28782=CARTESIAN_POINT('Ctrl Pts',(-25.1916893480828,89.0415966005281,5.68347362292805));
#28783=CARTESIAN_POINT('Ctrl Pts',(-27.1288126962993,91.381287394906,5.52549045767941));
#28784=CARTESIAN_POINT('Ctrl Pts',(-26.2279961358928,94.2821716400552,5.36750729243078));
#28785=CARTESIAN_POINT('Ctrl Pts',(-23.3063110339308,95.113048312297,5.20952412718214));
#28786=CARTESIAN_POINT('Ctrl Pts',(-21.0138255013219,93.1202839102265,5.05154096193351));
#28787=CARTESIAN_POINT('Ctrl Pts',(-21.4299021634741,90.1113837639743,4.89355779668487));
#28788=CARTESIAN_POINT('Ctrl Pts',(-24.1771452864616,88.8155230061493,4.73557463143624));
#28789=CARTESIAN_POINT('Ctrl Pts',(-26.7637115879574,90.4080915751154,4.5775914661876));
#28790=CARTESIAN_POINT('Ctrl Pts',(-26.843497148434,93.4445754200009,4.41960830093897));
#28791=CARTESIAN_POINT('Ctrl Pts',(-24.3441337392816,95.1707800539146,4.26162513569034));
#28792=CARTESIAN_POINT('Ctrl Pts',(-21.5326292853278,94.0209789504981,4.1036419704417));
#28793=CARTESIAN_POINT('Ctrl Pts',(-20.9591142806189,91.0380809645771,3.94565880519306));
#28794=CARTESIAN_POINT('Ctrl Pts',(-23.1437864268023,88.9276763640108,3.78767563994443));
#28795=CARTESIAN_POINT('Ctrl Pts',(-26.1050734848668,89.6039741910547,3.6296924746958));
#28796=CARTESIAN_POINT('Ctrl Pts',(-27.1569870893008,92.4535491577125,3.47170930944716));
#28797=CARTESIAN_POINT('Ctrl Pts',(-25.3454055513592,94.891739661045,3.31372614419853));
#28798=CARTESIAN_POINT('Ctrl Pts',(-22.3134954561587,94.7070233795333,3.1557429789499));
#28799=CARTESIAN_POINT('Ctrl Pts',(-20.8113021390385,92.0669449271691,2.99775981370126));
#28800=CARTESIAN_POINT('Ctrl Pts',(-22.2013674504565,89.3661442609453,2.83977664845263));
#28801=CARTESIAN_POINT('Ctrl Pts',(-25.2228521773581,89.0543424461441,2.68179348320399));
#28802=CARTESIAN_POINT('Ctrl Pts',(-27.1351717086426,91.4143489046793,2.52381031795536));
#28803=CARTESIAN_POINT('Ctrl Pts',(-26.2037764083394,94.3055683900266,2.36582715270672));
#28804=CARTESIAN_POINT('Ctrl Pts',(-23.2734951478333,95.1055433482707,2.20784398745809));
#28805=CARTESIAN_POINT('Ctrl Pts',(-21.0021490526171,93.0887157421965,2.04986082220945));
#28806=CARTESIAN_POINT('Ctrl Pts',(-21.4500163995022,90.084321978353,1.89187765696082));
#28807=CARTESIAN_POINT('Ctrl Pts',(-24.210682748199,88.8176438938542,1.73389449171219));
#28808=CARTESIAN_POINT('Ctrl Pts',(-26.7805041627851,90.4372052713962,1.57591132646355));
#28809=CARTESIAN_POINT('Ctrl Pts',(-26.8277997762314,93.4748183557424,1.41792816121491));
#28810=CARTESIAN_POINT('Ctrl Pts',(-24.3112335155169,95.1736105813595,1.25994499596628));
#28811=CARTESIAN_POINT('Ctrl Pts',(-21.5102242410122,93.9961091691131,1.10196183071765));
#28812=CARTESIAN_POINT('Ctrl Pts',(-20.9719518902951,91.0033770531542,0.943978665469013));
#28813=CARTESIAN_POINT('Ctrl Pts',(-22.4379643297735,89.6198434520492,0.838656555303256));
#28814=CARTESIAN_POINT('Ctrl Pts',(-23.301933573839,89.3888678140614,0.785995500220377));
#28815=CARTESIAN_POINT('Ctrl Pts',(-21.8048028959809,93.8768634390787,10.2140044997796));
#28816=CARTESIAN_POINT('Ctrl Pts',(-21.1837878836397,93.1505184486767,10.1613434446967));
#28817=CARTESIAN_POINT('Ctrl Pts',(-20.7302302947449,91.0448125029107,10.056021334531));
#28818=CARTESIAN_POINT('Ctrl Pts',(-23.0156867625841,88.7351875643265,9.89803816928235));
#28819=CARTESIAN_POINT('Ctrl Pts',(-26.1950062090231,89.3936689477181,9.74005500403371));
#28820=CARTESIAN_POINT('Ctrl Pts',(-27.3828721636666,92.4128767408671,9.58207183878509));
#28821=CARTESIAN_POINT('Ctrl Pts',(-25.5026093707801,95.059203920966,9.42408867353644));
#28822=CARTESIAN_POINT('Ctrl Pts',(-22.2593052903593,94.9299391890853,9.26610550828782));
#28823=CARTESIAN_POINT('Ctrl Pts',(-20.5949311131986,92.1435062136747,9.10812234303918));
#28824=CARTESIAN_POINT('Ctrl Pts',(-22.019041067396,89.2267188897615,8.95013917779055));
#28825=CARTESIAN_POINT('Ctrl Pts',(-25.2399628684864,88.8254848953298,8.79215601254191));
#28826=CARTESIAN_POINT('Ctrl Pts',(-27.3361889343087,91.3035990578311,8.63417284729328));
#28827=CARTESIAN_POINT('Ctrl Pts',(-26.4063812377719,94.4133948742933,8.47618968204464));
#28828=CARTESIAN_POINT('Ctrl Pts',(-23.2939019232727,95.3341482798463,8.31820651679601));
#28829=CARTESIAN_POINT('Ctrl Pts',(-20.821878497644,93.2307207244612,8.16022335154738));
#28830=CARTESIAN_POINT('Ctrl Pts',(-21.2325193430214,90.0109848545807,8.00224018629874));
#28831=CARTESIAN_POINT('Ctrl Pts',(-24.1533598039853,88.5953548891582,7.84425702105011));
#28832=CARTESIAN_POINT('Ctrl Pts',(-26.9350975904653,90.2678536211836,7.68627385580147));
#28833=CARTESIAN_POINT('Ctrl Pts',(-27.0546017290974,93.5114685471691,7.52829069055283));
#28834=CARTESIAN_POINT('Ctrl Pts',(-24.4034778158886,95.3841297611199,7.37030752530421));
#28835=CARTESIAN_POINT('Ctrl Pts',(-21.3863857635864,94.1872698476289,7.21232436005556));
#28836=CARTESIAN_POINT('Ctrl Pts',(-20.7399310263462,91.0064814901395,7.05434119480693));
#28837=CARTESIAN_POINT('Ctrl Pts',(-23.0504701241054,88.7268483496341,6.8963580295583));
#28838=CARTESIAN_POINT('Ctrl Pts',(-26.222265227443,89.4160754670625,6.73837486430966));
#28839=CARTESIAN_POINT('Ctrl Pts',(-27.378389919474,92.449010334975,6.58039169906103));
#28840=CARTESIAN_POINT('Ctrl Pts',(-25.4701996425288,95.0746775013101,6.42240853381239));
#28841=CARTESIAN_POINT('Ctrl Pts',(-22.2284881089027,94.9115072296366,6.26442536856376));
#28842=CARTESIAN_POINT('Ctrl Pts',(-20.5935983259232,92.1075005242027,6.10644220331512));
#28843=CARTESIAN_POINT('Ctrl Pts',(-22.0484311291595,89.205987174338,5.9484590380665));
#28844=CARTESIAN_POINT('Ctrl Pts',(-25.2734035094609,88.8387388228741,5.79047587281786));
#28845=CARTESIAN_POINT('Ctrl Pts',(-27.3433554426941,91.3388622597476,5.63249270756922));
#28846=CARTESIAN_POINT('Ctrl Pts',(-26.3807698735208,94.4386601930392,5.47450954232059));
#28847=CARTESIAN_POINT('Ctrl Pts',(-23.2587447682671,95.3265100945794,5.31652637707196));
#28848=CARTESIAN_POINT('Ctrl Pts',(-20.8090634588646,93.1971017993658,5.15854321182332));
#28849=CARTESIAN_POINT('Ctrl Pts',(-21.2536705056942,89.9818813125677,5.00056004657469));
#28850=CARTESIAN_POINT('Ctrl Pts',(-24.1892921421406,88.5971633578074,4.84257688132605));
#28851=CARTESIAN_POINT('Ctrl Pts',(-26.9532193443741,90.2989343839904,4.68459371607741));
#28852=CARTESIAN_POINT('Ctrl Pts',(-27.0384758022577,93.5436299841646,4.52661055082878));
#28853=CARTESIAN_POINT('Ctrl Pts',(-24.3677309963625,95.3882005028233,4.36862738558015));
#28854=CARTESIAN_POINT('Ctrl Pts',(-21.3634416282571,94.1595575157663,4.21064422033151));
#28855=CARTESIAN_POINT('Ctrl Pts',(-20.7506006887122,90.9721221579303,4.05266105508288));
#28856=CARTESIAN_POINT('Ctrl Pts',(-23.085075845721,88.7170070735612,3.89467788983424));
#28857=CARTESIAN_POINT('Ctrl Pts',(-26.2494184139641,89.4396786555336,3.73669472458561));
#28858=CARTESIAN_POINT('Ctrl Pts',(-27.3734617543622,92.4846490321267,3.57871155933697));
#28859=CARTESIAN_POINT('Ctrl Pts',(-25.4376600357343,95.0900263048807,3.42072839408834));
#28860=CARTESIAN_POINT('Ctrl Pts',(-22.1978518073487,94.8926440244144,3.26274522883971));
#28861=CARTESIAN_POINT('Ctrl Pts',(-20.592653065758,92.071535342105,3.10476206359107));
#28862=CARTESIAN_POINT('Ctrl Pts',(-22.0780351821522,89.1855407225702,2.94677889834244));
#28863=CARTESIAN_POINT('Ctrl Pts',(-25.3067031745353,88.8523586513677,2.7887957330938));
#28864=CARTESIAN_POINT('Ctrl Pts',(-27.3501504926354,91.3741907978781,2.63081256784517));
#28865=CARTESIAN_POINT('Ctrl Pts',(-26.354889398786,94.4636612586034,2.47282940259654));
#28866=CARTESIAN_POINT('Ctrl Pts',(-23.2236786962326,95.3184905150264,2.3148462373479));
#28867=CARTESIAN_POINT('Ctrl Pts',(-20.7965863558489,93.1633690014506,2.15686307209926));
#28868=CARTESIAN_POINT('Ctrl Pts',(-21.2751639752712,89.952963899789,1.99887990685063));
#28869=CARTESIAN_POINT('Ctrl Pts',(-24.2251292682703,88.5994296748227,1.840896741602));
#28870=CARTESIAN_POINT('Ctrl Pts',(-26.9711633863787,90.3300444069818,1.68291357635336));
#28871=CARTESIAN_POINT('Ctrl Pts',(-27.021702060943,93.575946678588,1.52493041110472));
#28872=CARTESIAN_POINT('Ctrl Pts',(-24.3325748036253,95.3912251195891,1.3669472458561));
#28873=CARTESIAN_POINT('Ctrl Pts',(-21.3395002696245,94.1329824129964,1.20896408060746));
#28874=CARTESIAN_POINT('Ctrl Pts',(-20.7643185735292,90.9350385986377,1.05098091535882));
#28875=CARTESIAN_POINT('Ctrl Pts',(-22.3308555140066,89.4566360720578,0.945658805193066));
#28876=CARTESIAN_POINT('Ctrl Pts',(-23.2540671456531,89.2098224301578,0.892997750110188));
#28877=CARTESIAN_POINT('Ctrl Pts',(-21.6639373423038,93.9973015569306,10.3210067496694));
#28878=CARTESIAN_POINT('Ctrl Pts',(-21.0030718657857,93.2243470893904,10.2683456945866));
#28879=CARTESIAN_POINT('Ctrl Pts',(-20.520409536926,90.9835182276056,10.1630235844208));
#28880=CARTESIAN_POINT('Ctrl Pts',(-22.9525234917661,88.5256849139446,10.0050404191722));
#28881=CARTESIAN_POINT('Ctrl Pts',(-26.3358595129894,89.2264209743707,9.84705725392353));
#28882=CARTESIAN_POINT('Ctrl Pts',(-27.5999506936452,92.4393709953448,9.68907408867489));
#28883=CARTESIAN_POINT('Ctrl Pts',(-25.5990316467514,95.2555126958587,9.53109092342626));
#28884=CARTESIAN_POINT('Ctrl Pts',(-22.1476051047098,95.1179530605298,9.37310775817762));
#28885=CARTESIAN_POINT('Ctrl Pts',(-20.3764282219686,92.1527149914235,9.215124592929));
#28886=CARTESIAN_POINT('Ctrl Pts',(-21.8919231533181,89.0487577497888,9.05714142768035));
#28887=CARTESIAN_POINT('Ctrl Pts',(-25.3195311476576,88.6217766146216,8.89915826243172));
#28888=CARTESIAN_POINT('Ctrl Pts',(-27.5502718066586,91.2589110869332,8.74117509718309));
#28889=CARTESIAN_POINT('Ctrl Pts',(-26.5607984537915,94.5682621545871,8.58319193193445));
#28890=CARTESIAN_POINT('Ctrl Pts',(-23.24859168833,95.5481002036266,8.42520876668582));
#28891=CARTESIAN_POINT('Ctrl Pts',(-20.6179387947979,93.3096959362796,8.26722560143718));
#28892=CARTESIAN_POINT('Ctrl Pts',(-21.0549304174885,89.8833499742237,8.10924243618856));
#28893=CARTESIAN_POINT('Ctrl Pts',(-24.1632008855267,88.3768791915844,7.95125927093991));
#28894=CARTESIAN_POINT('Ctrl Pts',(-27.123442475952,90.156701980971,7.79327610569129));
#28895=CARTESIAN_POINT('Ctrl Pts',(-27.2506151818504,93.6084593155026,7.63529294044264));
#28896=CARTESIAN_POINT('Ctrl Pts',(-24.4293689423972,95.6012889909869,7.47730977519402));
#28897=CARTESIAN_POINT('Ctrl Pts',(-21.2186704291245,94.3276267101463,7.31932660994538));
#28898=CARTESIAN_POINT('Ctrl Pts',(-20.5307327633938,90.9427275180138,7.16134344469674));
#28899=CARTESIAN_POINT('Ctrl Pts',(-22.9895388977221,88.5168105727741,7.00336027944811));
#28900=CARTESIAN_POINT('Ctrl Pts',(-26.3648677395855,89.2502653175659,6.84537711419947));
#28901=CARTESIAN_POINT('Ctrl Pts',(-27.5951808243418,92.4778232781622,6.68739394895084));
#28902=CARTESIAN_POINT('Ctrl Pts',(-25.5645421898479,95.27197921413,6.5294107837022));
#28903=CARTESIAN_POINT('Ctrl Pts',(-22.1148103881513,95.0983383242963,6.37142761845358));
#28904=CARTESIAN_POINT('Ctrl Pts',(-20.3750099098822,92.114398820868,6.21344445320493));
#28905=CARTESIAN_POINT('Ctrl Pts',(-21.9231991720717,89.0266956824957,6.05546128795631));
#28906=CARTESIAN_POINT('Ctrl Pts',(-25.355117670839,88.6358810452203,5.89747812270766));
#28907=CARTESIAN_POINT('Ctrl Pts',(-27.557898189089,91.2964371245891,5.73949495745904));
#28908=CARTESIAN_POINT('Ctrl Pts',(-26.5335436111487,94.5951487460233,5.5815117922104));
#28909=CARTESIAN_POINT('Ctrl Pts',(-23.2111785026033,95.5399718768618,5.42352862696177));
#28910=CARTESIAN_POINT('Ctrl Pts',(-20.6043014164074,93.2739196885051,5.26554546171313));
#28911=CARTESIAN_POINT('Ctrl Pts',(-21.0774388479142,89.8523788611612,5.1075622964645));
#28912=CARTESIAN_POINT('Ctrl Pts',(-24.2014389978196,88.3788037094653,4.94957913121586));
#28913=CARTESIAN_POINT('Ctrl Pts',(-27.1427271007907,90.1897771928657,4.79159596596723));
#28914=CARTESIAN_POINT('Ctrl Pts',(-27.2334544560815,93.6426845483281,4.63361280071859));
#28915=CARTESIAN_POINT('Ctrl Pts',(-24.3913282534434,95.6056209517321,4.47562963546996));
#28916=CARTESIAN_POINT('Ctrl Pts',(-21.1942539711864,94.2981360810344,4.31764647022132));
#28917=CARTESIAN_POINT('Ctrl Pts',(-20.5420870968054,90.9061633512837,4.15966330497269));
#28918=CARTESIAN_POINT('Ctrl Pts',(-23.0263652646397,88.5063377831116,4.00168013972405));
#28919=CARTESIAN_POINT('Ctrl Pts',(-26.3937633430615,89.2753831200125,3.84369697447542));
#28920=CARTESIAN_POINT('Ctrl Pts',(-27.5899364194237,92.5157489065408,3.68571380922678));
#28921=CARTESIAN_POINT('Ctrl Pts',(-25.5299145201095,95.2883129487163,3.52773064397815));
#28922=CARTESIAN_POINT('Ctrl Pts',(-22.0822081585386,95.0782646692958,3.36974747872952));
#28923=CARTESIAN_POINT('Ctrl Pts',(-20.3740039924776,92.0761257570406,3.21176431348088));
#28924=CARTESIAN_POINT('Ctrl Pts',(-21.9547029138477,89.0049371841951,3.05378114823225));
#28925=CARTESIAN_POINT('Ctrl Pts',(-25.3905541717125,88.6503748565914,2.89579798298361));
#28926=CARTESIAN_POINT('Ctrl Pts',(-27.5651292766281,91.3340326910768,2.73781481773498));
#28927=CARTESIAN_POINT('Ctrl Pts',(-26.5060023892327,94.6217541271801,2.57983165248635));
#28928=CARTESIAN_POINT('Ctrl Pts',(-23.1738622446318,95.5314376817822,2.42184848723771));
#28929=CARTESIAN_POINT('Ctrl Pts',(-20.5910236590807,93.2380222607045,2.26386532198907));
#28930=CARTESIAN_POINT('Ctrl Pts',(-21.1003115510402,89.8216058212251,2.10588215674044));
#28931=CARTESIAN_POINT('Ctrl Pts',(-24.2395757883417,88.3812154557912,1.94789899149181));
#28932=CARTESIAN_POINT('Ctrl Pts',(-27.1618226099723,90.2228835425675,1.78991582624317));
#28933=CARTESIAN_POINT('Ctrl Pts',(-27.2156043456547,93.6770750014334,1.63193266099454));
#28934=CARTESIAN_POINT('Ctrl Pts',(-24.3539160917338,95.6088396578189,1.4739494957459));
#28935=CARTESIAN_POINT('Ctrl Pts',(-21.1687762982368,94.2698556568795,1.31596633049727));
#28936=CARTESIAN_POINT('Ctrl Pts',(-20.5566852567634,90.8667001441213,1.15798316524863));
#28937=CARTESIAN_POINT('Ctrl Pts',(-22.2237466982397,89.2934286920664,1.05266105508288));
#28938=CARTESIAN_POINT('Ctrl Pts',(-23.2062007174672,89.0307770462543,0.999999999999999));
#28939=CARTESIAN_POINT('Ctrl Pts',(-22.0865340033349,93.6359872033749,10.));
#28940=CARTESIAN_POINT('Ctrl Pts',(-22.0249228618564,93.5780878591467,10.));
#28941=CARTESIAN_POINT('Ctrl Pts',(-21.966680820328,93.517037957369,10.));
#28942=CARTESIAN_POINT('Ctrl Pts',(-21.9118055510414,93.4532222734472,10.));
#28943=CARTESIAN_POINT('Ctrl Pts',(-21.8554775805296,93.3877172106225,10.));
#28944=CARTESIAN_POINT('Ctrl Pts',(-21.8026965604156,93.319297559701,10.));
#28945=CARTESIAN_POINT('Ctrl Pts',(-21.7534854803777,93.2483309191729,10.));
#28946=CARTESIAN_POINT('Ctrl Pts',(-21.7029129709051,93.1754009794607,10.));
#28947=CARTESIAN_POINT('Ctrl Pts',(-21.6561101248005,93.0997806200771,10.));
#28948=CARTESIAN_POINT('Ctrl Pts',(-21.6131359910424,93.0218257865766,10.));
#28949=CARTESIAN_POINT('Ctrl Pts',(-21.5942445812211,92.9875568769228,10.));
#28950=CARTESIAN_POINT('Ctrl Pts',(-21.5760935456704,92.9528363378501,10.));
#28951=CARTESIAN_POINT('Ctrl Pts',(-21.558690318408,92.917692336787,10.));
#28952=CARTESIAN_POINT('Ctrl Pts',(-21.548765297561,92.8976497930713,10.));
#28953=CARTESIAN_POINT('Ctrl Pts',(-21.5390835217549,92.877469502106,10.));
#28954=CARTESIAN_POINT('Ctrl Pts',(-21.5296466035414,92.8571565405433,10.));
#28955=CARTESIAN_POINT('Ctrl Pts',(-21.5211295714091,92.8388236332939,10.));
#28956=CARTESIAN_POINT('Ctrl Pts',(-21.5128096038615,92.8203769112349,10.));
#28957=CARTESIAN_POINT('Ctrl Pts',(-21.5047015810338,92.8018519372552,10.));
#28958=CARTESIAN_POINT('Ctrl Pts',(-21.4681367627671,92.7183097073719,10.));
#28959=CARTESIAN_POINT('Ctrl Pts',(-21.4358322656584,92.6330839819686,10.));
#28960=CARTESIAN_POINT('Ctrl Pts',(-21.4078131930248,92.5465734750324,10.));
#28961=CARTESIAN_POINT('Ctrl Pts',(-21.3793314408844,92.4586344183647,10.));
#28962=CARTESIAN_POINT('Ctrl Pts',(-21.355277318963,92.3693670435349,10.));
#28963=CARTESIAN_POINT('Ctrl Pts',(-21.3357162703818,92.2791530220287,10.));
#28964=CARTESIAN_POINT('Ctrl Pts',(-21.3167358111454,92.1916166330335,10.));
#28965=CARTESIAN_POINT('Ctrl Pts',(-21.3019855060024,92.1031880411159,10.));
#28966=CARTESIAN_POINT('Ctrl Pts',(-21.2915659618292,92.014194029087,10.));
#28967=CARTESIAN_POINT('Ctrl Pts',(-21.2872066009676,91.9769604412726,10.));
#28968=CARTESIAN_POINT('Ctrl Pts',(-21.2836058304749,91.9396276882027,10.));
#28969=CARTESIAN_POINT('Ctrl Pts',(-21.2807733396412,91.902219087546,10.));
#28970=CARTESIAN_POINT('Ctrl Pts',(-21.279002750376,91.8788349812459,10.));
#28971=CARTESIAN_POINT('Ctrl Pts',(-21.277532394138,91.8554212321296,10.));
#28972=CARTESIAN_POINT('Ctrl Pts',(-21.2763649279069,91.8319835034305,10.));
#28973=CARTESIAN_POINT('Ctrl Pts',(-21.2756806561547,91.8182462532588,10.));
#28974=CARTESIAN_POINT('Ctrl Pts',(-21.2751007108994,91.8045053338933,10.));
#28975=CARTESIAN_POINT('Ctrl Pts',(-21.2746256143519,91.790770119806,10.));
#28976=CARTESIAN_POINT('Ctrl Pts',(-21.2712677542687,91.6936931627977,10.));
#28977=CARTESIAN_POINT('Ctrl Pts',(-21.2731370867467,91.5967807433318,10.));
#28978=CARTESIAN_POINT('Ctrl Pts',(-21.2802984098211,91.5004551184403,10.));
#28979=CARTESIAN_POINT('Ctrl Pts',(-21.2874597328954,91.4041294935487,10.));
#28980=CARTESIAN_POINT('Ctrl Pts',(-21.2999126116946,91.3083896087231,10.));
#28981=CARTESIAN_POINT('Ctrl Pts',(-21.3177747368199,91.2136387821642,10.));
#28982=CARTESIAN_POINT('Ctrl Pts',(-21.3348522432755,91.1230500173404,10.));
#28983=CARTESIAN_POINT('Ctrl Pts',(-21.3568741021771,91.0333643557261,10.));
#28984=CARTESIAN_POINT('Ctrl Pts',(-21.3835656166832,90.9448211375735,10.));
#28985=CARTESIAN_POINT('Ctrl Pts',(-21.3925004778797,90.9151817042657,10.));
#28986=CARTESIAN_POINT('Ctrl Pts',(-21.4019590305019,90.8856703233236,10.));
#28987=CARTESIAN_POINT('Ctrl Pts',(-21.4119322462714,90.8562961512492,10.));
#28988=CARTESIAN_POINT('Ctrl Pts',(-21.4184134249047,90.8372070970445,10.));
#28989=CARTESIAN_POINT('Ctrl Pts',(-21.4251119666752,90.8181759907897,10.));
#28990=CARTESIAN_POINT('Ctrl Pts',(-21.432025530206,90.7992053804605,10.));
#28991=CARTESIAN_POINT('Ctrl Pts',(-21.4386151870839,90.781123560242,10.));
#28992=CARTESIAN_POINT('Ctrl Pts',(-21.4454019414903,90.7630924899962,10.));
#28993=CARTESIAN_POINT('Ctrl Pts',(-21.452372973352,90.7451415274744,10.));
#28994=CARTESIAN_POINT('Ctrl Pts',(-21.4862164573767,90.6579918593344,10.));
#28995=CARTESIAN_POINT('Ctrl Pts',(-21.5244382858088,90.5726164812308,10.));
#28996=CARTESIAN_POINT('Ctrl Pts',(-21.5667072739919,90.4892490087442,10.));
#28997=CARTESIAN_POINT('Ctrl Pts',(-21.6105455323499,90.4027864518056,10.));
#28998=CARTESIAN_POINT('Ctrl Pts',(-21.6587371595505,90.3184829337529,10.));
#28999=CARTESIAN_POINT('Ctrl Pts',(-21.7109686726983,90.2366020739748,10.));
#29000=CARTESIAN_POINT('Ctrl Pts',(-21.7637886184686,90.1537987563519,10.));
#29001=CARTESIAN_POINT('Ctrl Pts',(-21.8207403975229,90.0734721713631,10.));
#29002=CARTESIAN_POINT('Ctrl Pts',(-21.8815515974698,89.9959097942702,10.));
#29003=CARTESIAN_POINT('Ctrl Pts',(-21.9232140422193,89.9427709275303,10.));
#29004=CARTESIAN_POINT('Ctrl Pts',(-21.9666890946703,89.8909298239753,10.));
#29005=CARTESIAN_POINT('Ctrl Pts',(-22.0119013665037,89.8404859712607,10.));
#29006=CARTESIAN_POINT('Ctrl Pts',(-22.0240086331348,89.8269777543553,10.));
#29007=CARTESIAN_POINT('Ctrl Pts',(-22.0362418077641,89.8135685184895,10.));
#29008=CARTESIAN_POINT('Ctrl Pts',(-22.0485858237953,89.800274672024,10.));
#29009=CARTESIAN_POINT('Ctrl Pts',(-22.1172467098524,89.7263305621724,10.));
#29010=CARTESIAN_POINT('Ctrl Pts',(-22.1894214869168,89.6558543371947,10.));
#29011=CARTESIAN_POINT('Ctrl Pts',(-22.2647996928107,89.5891358089895,10.));
#29012=CARTESIAN_POINT('Ctrl Pts',(-22.3277046148832,89.5334575958008,10.));
#29013=CARTESIAN_POINT('Ctrl Pts',(-22.3928415833451,89.4803963686579,10.));
#29014=CARTESIAN_POINT('Ctrl Pts',(-22.460053826701,89.4301343334532,10.));
#29015=CARTESIAN_POINT('Ctrl Pts',(-22.4819361315296,89.4137705116145,10.));
#29016=CARTESIAN_POINT('Ctrl Pts',(-22.5040385611967,89.3977035154392,10.));
#29017=CARTESIAN_POINT('Ctrl Pts',(-22.5263561315554,89.3819400183082,10.));
#29018=CARTESIAN_POINT('Ctrl Pts',(-22.5491248910509,89.3658578342168,10.));
#29019=CARTESIAN_POINT('Ctrl Pts',(-22.5721229921732,89.3500881169297,10.));
#29020=CARTESIAN_POINT('Ctrl Pts',(-22.595316006075,89.33465717982,10.));
#29021=CARTESIAN_POINT('Ctrl Pts',(-22.6802613709847,89.2781407396011,10.));
#29022=CARTESIAN_POINT('Ctrl Pts',(-22.7678730042567,89.2261247336488,10.));
#29023=CARTESIAN_POINT('Ctrl Pts',(-22.8578606395619,89.1789172288512,10.));
#29024=CARTESIAN_POINT('Ctrl Pts',(-22.9411343064062,89.1352318712602,10.));
#29025=CARTESIAN_POINT('Ctrl Pts',(-23.0264434722402,89.0956640032309,10.));
#29026=CARTESIAN_POINT('Ctrl Pts',(-23.1135855312338,89.060486601523,10.));
#29027=CARTESIAN_POINT('Ctrl Pts',(-23.14360948864,89.0483665664591,10.));
#29028=CARTESIAN_POINT('Ctrl Pts',(-23.1738512261799,89.0367679981665,10.));
#29029=CARTESIAN_POINT('Ctrl Pts',(-23.2042983602307,89.0256873161863,10.));
#29030=CARTESIAN_POINT('Ctrl Pts',(-26.5182105203766,91.9978055611691,8.38741669750802));
#29031=CARTESIAN_POINT('Ctrl Pts',(-26.5197765073294,91.8252749644444,8.39833391417657));
#29032=CARTESIAN_POINT('Ctrl Pts',(-26.5035405383448,91.6530372868482,8.40925113084511));
#29033=CARTESIAN_POINT('Ctrl Pts',(-26.4684109790521,91.4847436281601,8.42016834751366));
#29034=CARTESIAN_POINT('Ctrl Pts',(-26.2989575631207,90.6729504853336,8.47282940259653));
#29035=CARTESIAN_POINT('Ctrl Pts',(-25.6898919366324,89.95292597104,8.52549045767941));
#29036=CARTESIAN_POINT('Ctrl Pts',(-24.9174342209562,89.6512036660532,8.57815151276229));
#29037=CARTESIAN_POINT('Ctrl Pts',(-24.14497650528,89.3494813610665,8.63081256784517));
#29038=CARTESIAN_POINT('Ctrl Pts',(-23.2091267004159,89.4660612653866,8.68347362292804));
#29039=CARTESIAN_POINT('Ctrl Pts',(-22.5343117980016,89.9480924656251,8.73613467801092));
#29040=CARTESIAN_POINT('Ctrl Pts',(-21.8594968955873,90.4301236658636,8.7887957330938));
#29041=CARTESIAN_POINT('Ctrl Pts',(-21.4457168956229,91.2776061620205,8.84145678817668));
#29042=CARTESIAN_POINT('Ctrl Pts',(-21.480621689974,92.1061512081021,8.89411784325956));
#29043=CARTESIAN_POINT('Ctrl Pts',(-21.5155264843251,92.9346962541837,8.94677889834244));
#29044=CARTESIAN_POINT('Ctrl Pts',(-21.9991160729917,93.7443038501899,8.99943995342531));
#29045=CARTESIAN_POINT('Ctrl Pts',(-22.7120873935215,94.1678868023571,9.05210100850819));
#29046=CARTESIAN_POINT('Ctrl Pts',(-23.4250587140513,94.5914697545244,9.10476206359107));
#29047=CARTESIAN_POINT('Ctrl Pts',(-24.3674117664444,94.6290280628526,9.15742311867395));
#29048=CARTESIAN_POINT('Ctrl Pts',(-25.1117466734529,94.2633575271385,9.21008417375683));
#29049=CARTESIAN_POINT('Ctrl Pts',(-25.8560815804615,93.8976869914244,9.26274522883971));
#29050=CARTESIAN_POINT('Ctrl Pts',(-26.4023983420856,93.1287876116681,9.31540628392258));
#29051=CARTESIAN_POINT('Ctrl Pts',(-26.502987472461,92.3057173655401,9.36806733900546));
#29052=CARTESIAN_POINT('Ctrl Pts',(-26.5153073620014,92.2049099077324,9.37451712517298));
#29053=CARTESIAN_POINT('Ctrl Pts',(-26.5209410251377,92.1032898490186,9.3809669113405));
#29054=CARTESIAN_POINT('Ctrl Pts',(-26.5201758362126,92.0015868137837,9.38741669750802));
#29055=CARTESIAN_POINT('Ctrl Pts',(-24.7937992825329,89.0307770462543,10.));
#29056=CARTESIAN_POINT('Ctrl Pts',(-25.7762533017603,89.2934286920664,9.94733894491712));
#29057=CARTESIAN_POINT('Ctrl Pts',(-27.443314608871,90.8667010511062,9.84201683475136));
#29058=CARTESIAN_POINT('Ctrl Pts',(-26.8312238178928,94.2698553838416,9.68403366950273));
#29059=CARTESIAN_POINT('Ctrl Pts',(-23.6460838986402,95.6088399383518,9.5260505042541));
#29060=CARTESIAN_POINT('Ctrl Pts',(-20.7843955634607,93.6770749374766,9.36806733900546));
#29061=CARTESIAN_POINT('Ctrl Pts',(-20.8381773234134,90.2228835564638,9.21008417375683));
#29062=CARTESIAN_POINT('Ctrl Pts',(-23.760424197283,88.3812153351417,9.05210100850819));
#29063=CARTESIAN_POINT('Ctrl Pts',(-26.8996885260907,89.8216057842524,8.89411784325956));
#29064=CARTESIAN_POINT('Ctrl Pts',(-27.4089764216848,93.2380222823145,8.73613467801092));
#29065=CARTESIAN_POINT('Ctrl Pts',(-24.8261377777637,95.5314377737091,8.57815151276229));
#29066=CARTESIAN_POINT('Ctrl Pts',(-21.493997547754,94.6217541894132,8.42016834751366));
#29067=CARTESIAN_POINT('Ctrl Pts',(-20.4348706359933,91.3340326759415,8.26218518226502));
#29068=CARTESIAN_POINT('Ctrl Pts',(-22.6094457936036,88.6503747732116,8.10420201701639));
#29069=CARTESIAN_POINT('Ctrl Pts',(-26.0452971368403,89.0049371106047,7.94621885176775));
#29070=CARTESIAN_POINT('Ctrl Pts',(-27.6259960969404,92.0761257587368,7.78823568651912));
#29071=CARTESIAN_POINT('Ctrl Pts',(-25.9177918888646,95.0782647453892,7.63025252127048));
#29072=CARTESIAN_POINT('Ctrl Pts',(-22.4700854420894,95.288313029852,7.47226935602185));
#29073=CARTESIAN_POINT('Ctrl Pts',(-20.4100634919605,92.5157489192991,7.31428619077322));
#29074=CARTESIAN_POINT('Ctrl Pts',(-21.6062365978313,89.275383052732,7.15630302552458));
#29075=CARTESIAN_POINT('Ctrl Pts',(-24.9736347594025,88.5063376968639,6.99831986027595));
#29076=CARTESIAN_POINT('Ctrl Pts',(-27.4579129885641,90.9061633242749,6.84033669502731));
#29077=CARTESIAN_POINT('Ctrl Pts',(-26.8057460980852,94.2981361377744,6.68235352977868));
#29078=CARTESIAN_POINT('Ctrl Pts',(-23.6086717368945,95.6056210407497,6.52437036453004));
#29079=CARTESIAN_POINT('Ctrl Pts',(-20.7665454640887,93.6426845888844,6.36638719928141));
#29080=CARTESIAN_POINT('Ctrl Pts',(-20.857272821619,90.1897771481731,6.20840403403277));
#29081=CARTESIAN_POINT('Ctrl Pts',(-23.7985609972073,88.3788036200625,6.05042086878414));
#29082=CARTESIAN_POINT('Ctrl Pts',(-26.9225612242403,89.8523788081389,5.89243770353549));
#29083=CARTESIAN_POINT('Ctrl Pts',(-27.3956986674284,93.2739197199569,5.73445453828688));
#29084=CARTESIAN_POINT('Ctrl Pts',(-24.7888215168716,95.5399719642594,5.57647137303822));
#29085=CARTESIAN_POINT('Ctrl Pts',(-21.4664563263011,94.5951488100945,5.41848820778961));
#29086=CARTESIAN_POINT('Ctrl Pts',(-20.4421017230708,91.2964371072188,5.26050504254096));
#29087=CARTESIAN_POINT('Ctrl Pts',(-22.6448822957049,88.6358809621643,5.10252187729233));
#29088=CARTESIAN_POINT('Ctrl Pts',(-26.0768008792021,89.0266956090883,4.9445387120437));
#29089=CARTESIAN_POINT('Ctrl Pts',(-27.6249901796144,92.1143988236926,4.78655554679506));
#29090=CARTESIAN_POINT('Ctrl Pts',(-25.8851896583917,95.0983384007904,4.62857238154643));
#29091=CARTESIAN_POINT('Ctrl Pts',(-22.4354577715254,95.2719792949115,4.47058921629779));
#29092=CARTESIAN_POINT('Ctrl Pts',(-20.4048190868974,92.4778232899584,4.31260605104916));
#29093=CARTESIAN_POINT('Ctrl Pts',(-21.6351322020288,89.2502652496793,4.15462288580052));
#29094=CARTESIAN_POINT('Ctrl Pts',(-25.010461127225,88.5168104867762,3.99663972055189));
#29095=CARTESIAN_POINT('Ctrl Pts',(-27.4692673222584,90.9427274919152,3.83865655530326));
#29096=CARTESIAN_POINT('Ctrl Pts',(-26.7813296395429,94.327626767605,3.68067339005462));
#29097=CARTESIAN_POINT('Ctrl Pts',(-23.5706310470027,95.6012890799134,3.52269022480599));
#29098=CARTESIAN_POINT('Ctrl Pts',(-20.7493847378944,93.6084593551842,3.36470705955735));
#29099=CARTESIAN_POINT('Ctrl Pts',(-20.8765574469375,90.1567019355188,3.20672389430872));
#29100=CARTESIAN_POINT('Ctrl Pts',(-23.8367991104361,88.3768791020246,3.04874072906008));
#29101=CARTESIAN_POINT('Ctrl Pts',(-26.9450696552404,89.8833499221761,2.89075756381144));
#29102=CARTESIAN_POINT('Ctrl Pts',(-27.3820612886588,93.3096959682138,2.73277439856281));
#29103=CARTESIAN_POINT('Ctrl Pts',(-24.7514083303165,95.5481002919865,2.57479123331418));
#29104=CARTESIAN_POINT('Ctrl Pts',(-21.4392014827728,94.5682622165549,2.41680806806554));
#29105=CARTESIAN_POINT('Ctrl Pts',(-20.4497281061605,91.2589110713399,2.25882490281691));
#29106=CARTESIAN_POINT('Ctrl Pts',(-22.6804688187274,88.6217765261786,2.10084173756827));
#29107=CARTESIAN_POINT('Ctrl Pts',(-26.1080769010003,89.0487576862312,1.94285857231964));
#29108=CARTESIAN_POINT('Ctrl Pts',(-27.623571862538,92.1527149782027,1.784875407071));
#29109=CARTESIAN_POINT('Ctrl Pts',(-25.8523949517842,95.1179531681003,1.62689224182237));
#29110=CARTESIAN_POINT('Ctrl Pts',(-22.40096829048,95.2555127221397,1.46890907657374));
#29111=CARTESIAN_POINT('Ctrl Pts',(-20.4000492676845,92.4393710995324,1.3109259113251));
#29112=CARTESIAN_POINT('Ctrl Pts',(-21.6641403201723,89.2264207486354,1.15294274607647));
#29113=CARTESIAN_POINT('Ctrl Pts',(-25.0474767585968,88.5256850731752,0.994959580827833));
#29114=CARTESIAN_POINT('Ctrl Pts',(-27.4795898385891,90.983517556268,0.836976415579199));
#29115=CARTESIAN_POINT('Ctrl Pts',(-26.9969281342143,93.2243470893905,0.731654305413442));
#29116=CARTESIAN_POINT('Ctrl Pts',(-26.3360626576961,93.9973015569307,0.678993250330564));
#29117=CARTESIAN_POINT('Ctrl Pts',(-24.745932854347,89.2098224301578,10.1070022498898));
#29118=CARTESIAN_POINT('Ctrl Pts',(-25.6691444859934,89.4566360720578,10.0543411948069));
#29119=CARTESIAN_POINT('Ctrl Pts',(-27.2356813002074,90.9350394509311,9.94901908464117));
#29120=CARTESIAN_POINT('Ctrl Pts',(-26.6604998395025,94.1329821564226,9.79103591939255));
#29121=CARTESIAN_POINT('Ctrl Pts',(-23.6674251873291,95.3912253832059,9.63305275414391));
#29122=CARTESIAN_POINT('Ctrl Pts',(-20.9782978536527,93.5759466184876,9.47506958889528));
#29123=CARTESIAN_POINT('Ctrl Pts',(-21.0288365510238,90.3300444200403,9.31708642364664));
#29124=CARTESIAN_POINT('Ctrl Pts',(-23.7748707182211,88.5994295614483,9.159103258398));
#29125=CARTESIAN_POINT('Ctrl Pts',(-26.7248360972087,89.9529638650458,9.00112009314937));
#29126=CARTESIAN_POINT('Ctrl Pts',(-27.2034137200465,93.1633690217573,8.84313692790073));
#29127=CARTESIAN_POINT('Ctrl Pts',(-24.7763213248124,95.3184906014102,8.6851537626521));
#29128=CARTESIAN_POINT('Ctrl Pts',(-21.6451105420004,94.4636613170838,8.52717059740347));
#29129=CARTESIAN_POINT('Ctrl Pts',(-20.649849425255,91.3741907836555,8.36918743215483));
#29130=CARTESIAN_POINT('Ctrl Pts',(-22.6932967928723,88.8523585730158,8.2112042669062));
#29131=CARTESIAN_POINT('Ctrl Pts',(-25.9219648654793,89.1855406534173,8.05322110165756));
#29132=CARTESIAN_POINT('Ctrl Pts',(-27.407347018268,92.0715353436988,7.89523793640893));
#29133=CARTESIAN_POINT('Ctrl Pts',(-25.8021482371961,94.8926440959194,7.73725477116029));
#29134=CARTESIAN_POINT('Ctrl Pts',(-22.562339928744,95.0900263811238,7.57927160591167));
#29135=CARTESIAN_POINT('Ctrl Pts',(-20.6265381623655,92.4846490441157,7.42128844066302));
#29136=CARTESIAN_POINT('Ctrl Pts',(-21.7505815304928,89.4396785923101,7.26330527541439));
#29137=CARTESIAN_POINT('Ctrl Pts',(-24.9149241768714,88.7170069925143,7.10532211016575));
#29138=CARTESIAN_POINT('Ctrl Pts',(-27.2493993915096,90.9721221325502,6.94733894491713));
#29139=CARTESIAN_POINT('Ctrl Pts',(-26.6365584368374,94.1595575690848,6.78935577966848));
#29140=CARTESIAN_POINT('Ctrl Pts',(-23.632268994558,95.3882005864732,6.63137261441985));
#29141=CARTESIAN_POINT('Ctrl Pts',(-20.9615241227262,93.5436300222751,6.47338944917122));
#29142=CARTESIAN_POINT('Ctrl Pts',(-21.0467805827144,90.2989343419931,6.31540628392258));
#29143=CARTESIAN_POINT('Ctrl Pts',(-23.8107078531861,88.5971632737953,6.15742311867395));
#29144=CARTESIAN_POINT('Ctrl Pts',(-26.7463295621094,89.9818812627429,5.99943995342531));
#29145=CARTESIAN_POINT('Ctrl Pts',(-27.1909366199158,93.1971018289209,5.84145678817668));
#29146=CARTESIAN_POINT('Ctrl Pts',(-24.7412552500335,95.3265101767069,5.68347362292804));
#29147=CARTESIAN_POINT('Ctrl Pts',(-21.6192300677009,94.4386602532469,5.52549045767941));
#29148=CARTESIAN_POINT('Ctrl Pts',(-20.6566444747624,91.3388622434247,5.36750729243077));
#29149=CARTESIAN_POINT('Ctrl Pts',(-22.7265964591003,88.8387387448265,5.20952412718214));
#29150=CARTESIAN_POINT('Ctrl Pts',(-25.9515689190225,89.2059871053571,5.05154096193351));
#29151=CARTESIAN_POINT('Ctrl Pts',(-27.4064017581768,92.107500526857,4.89355779668487));
#29152=CARTESIAN_POINT('Ctrl Pts',(-25.7715119348338,94.9115073015181,4.73557463143624));
#29153=CARTESIAN_POINT('Ctrl Pts',(-22.5298003211736,95.0746775772204,4.5775914661876));
#29154=CARTESIAN_POINT('Ctrl Pts',(-20.6216099971176,92.4490103460599,4.41960830093897));
#29155=CARTESIAN_POINT('Ctrl Pts',(-21.7777347176919,89.4160754032695,4.26162513569033));
#29156=CARTESIAN_POINT('Ctrl Pts',(-24.9495298993374,88.7268482688219,4.1036419704417));
#29157=CARTESIAN_POINT('Ctrl Pts',(-27.2600690541411,91.0064814656145,3.94565880519306));
#29158=CARTESIAN_POINT('Ctrl Pts',(-26.6136143009403,94.1872699016228,3.78767563994443));
#29159=CARTESIAN_POINT('Ctrl Pts',(-23.5965221741505,95.3841298446841,3.6296924746958));
#29160=CARTESIAN_POINT('Ctrl Pts',(-20.9453981954867,93.5114685844578,3.47170930944716));
#29161=CARTESIAN_POINT('Ctrl Pts',(-21.0649023370739,90.2678535784722,3.31372614419852));
#29162=CARTESIAN_POINT('Ctrl Pts',(-23.8466401922209,88.5953548049988,3.15574297894989));
#29163=CARTESIAN_POINT('Ctrl Pts',(-26.7674807253219,90.0109848056715,2.99775981370126));
#29164=CARTESIAN_POINT('Ctrl Pts',(-27.1781215807802,93.2307207544698,2.83977664845262));
#29165=CARTESIAN_POINT('Ctrl Pts',(-24.7060980942495,95.334148362878,2.68179348320399));
#29166=CARTESIAN_POINT('Ctrl Pts',(-21.5936187026176,94.4133949325243,2.52381031795535));
#29167=CARTESIAN_POINT('Ctrl Pts',(-20.6638109837674,91.3035990431782,2.36582715270672));
#29168=CARTESIAN_POINT('Ctrl Pts',(-22.7600370999256,88.82548481222,2.20784398745809));
#29169=CARTESIAN_POINT('Ctrl Pts',(-25.980958983647,89.2267188300363,2.04986082220945));
#29170=CARTESIAN_POINT('Ctrl Pts',(-27.4050689662123,92.1435062012512,1.89187765696082));
#29171=CARTESIAN_POINT('Ctrl Pts',(-25.740694762728,94.9299392901692,1.73389449171218));
#29172=CARTESIAN_POINT('Ctrl Pts',(-22.4973905702363,95.0592039456622,1.57591132646355));
#29173=CARTESIAN_POINT('Ctrl Pts',(-20.6171277999948,92.4128768387722,1.41792816121491));
#29174=CARTESIAN_POINT('Ctrl Pts',(-21.8049936341991,89.3936687355948,1.25994499596628));
#29175=CARTESIAN_POINT('Ctrl Pts',(-24.9843134726817,88.7351877139554,1.10196183071764));
#29176=CARTESIAN_POINT('Ctrl Pts',(-27.2697691184269,91.0448118720551,0.94397866546901));
#29177=CARTESIAN_POINT('Ctrl Pts',(-26.8162121163602,93.1505184486767,0.838656555303253));
#29178=CARTESIAN_POINT('Ctrl Pts',(-26.1951971040191,93.8768634390788,0.785995500220375));
#29179=CARTESIAN_POINT('Ctrl Pts',(-24.698066426161,89.3888678140614,10.2140044997796));
#29180=CARTESIAN_POINT('Ctrl Pts',(-25.5620356702265,89.6198434520493,10.1613434446967));
#29181=CARTESIAN_POINT('Ctrl Pts',(-27.0280479915439,91.0033778507559,10.056021334531));
#29182=CARTESIAN_POINT('Ctrl Pts',(-26.4897758611121,93.9961089290037,9.89803816928235));
#29183=CARTESIAN_POINT('Ctrl Pts',(-23.688766476018,95.1736108280599,9.74005500403372));
#29184=CARTESIAN_POINT('Ctrl Pts',(-21.1722001438448,93.4748182994988,9.58207183878508));
#29185=CARTESIAN_POINT('Ctrl Pts',(-21.2194957786343,90.4372052836167,9.42408867353644));
#29186=CARTESIAN_POINT('Ctrl Pts',(-23.7893172391594,88.817643787755,9.26610550828782));
#29187=CARTESIAN_POINT('Ctrl Pts',(-26.5499836683267,90.0843219458393,9.10812234303918));
#29188=CARTESIAN_POINT('Ctrl Pts',(-26.9978510184081,93.0887157612002,8.95013917779054));
#29189=CARTESIAN_POINT('Ctrl Pts',(-24.7265048718612,95.1055434291113,8.79215601254191));
#29190=CARTESIAN_POINT('Ctrl Pts',(-21.7962235362467,94.3055684447543,8.63417284729327));
#29191=CARTESIAN_POINT('Ctrl Pts',(-20.8648282145167,91.4143488913694,8.47618968204464));
#29192=CARTESIAN_POINT('Ctrl Pts',(-22.7771477921409,89.0543423728199,8.318206516796));
#29193=CARTESIAN_POINT('Ctrl Pts',(-25.7986325941185,89.36614419623,8.16022335154738));
#29194=CARTESIAN_POINT('Ctrl Pts',(-27.1886979395956,92.0669449286608,8.00224018629874));
#29195=CARTESIAN_POINT('Ctrl Pts',(-25.6865045855277,94.7070234464497,7.84425702105011));
#29196=CARTESIAN_POINT('Ctrl Pts',(-22.6545944153985,94.8917397323956,7.68627385580146));
#29197=CARTESIAN_POINT('Ctrl Pts',(-20.8430128327706,92.4535491689321,7.52829069055284));
#29198=CARTESIAN_POINT('Ctrl Pts',(-21.8949264631544,89.6039741318884,7.3703075253042));
#29199=CARTESIAN_POINT('Ctrl Pts',(-24.8562135943403,88.9276762881646,7.21232436005557));
#29200=CARTESIAN_POINT('Ctrl Pts',(-27.040885794455,91.0380809408257,7.05434119480693));
#29201=CARTESIAN_POINT('Ctrl Pts',(-26.4673707755896,94.0209790003952,6.8963580295583));
#29202=CARTESIAN_POINT('Ctrl Pts',(-23.6558662522216,95.1707801321966,6.73837486430966));
#29203=CARTESIAN_POINT('Ctrl Pts',(-21.1565027813636,93.444575455666,6.58039169906103));
#29204=CARTESIAN_POINT('Ctrl Pts',(-21.2362883438098,90.4080915358129,6.42240853381239));
#29205=CARTESIAN_POINT('Ctrl Pts',(-23.822854709165,88.8155229275284,6.26442536856376));
#29206=CARTESIAN_POINT('Ctrl Pts',(-26.5700978999786,90.1113837173467,6.10644220331512));
#29207=CARTESIAN_POINT('Ctrl Pts',(-26.9861745724031,93.120283937885,5.94845903806649));
#29208=CARTESIAN_POINT('Ctrl Pts',(-24.6936889831954,95.1130483891543,5.79047587281785));
#29209=CARTESIAN_POINT('Ctrl Pts',(-21.7720038091006,94.2821716963994,5.63249270756922));
#29210=CARTESIAN_POINT('Ctrl Pts',(-20.8711872264541,91.3812873796306,5.47450954232059));
#29211=CARTESIAN_POINT('Ctrl Pts',(-22.8083106224958,89.0415965274887,5.31652637707195));
#29212=CARTESIAN_POINT('Ctrl Pts',(-25.8263369588428,89.3852786016259,5.15854321182332));
#29213=CARTESIAN_POINT('Ctrl Pts',(-27.1878133367392,92.1006022300214,5.00056004657468));
#29214=CARTESIAN_POINT('Ctrl Pts',(-25.6578342112759,94.7246762022458,4.84257688132605));
#29215=CARTESIAN_POINT('Ctrl Pts',(-22.6241428708219,94.8773758595294,4.68459371607741));
#29216=CARTESIAN_POINT('Ctrl Pts',(-20.8384009073378,92.4201974021612,4.52661055082878));
#29217=CARTESIAN_POINT('Ctrl Pts',(-21.9203372333551,89.5818855568597,4.36862738558014));
#29218=CARTESIAN_POINT('Ctrl Pts',(-24.8885986714499,88.9368860508676,4.21064422033151));
#29219=CARTESIAN_POINT('Ctrl Pts',(-27.0508707860238,91.0702354393139,4.05266105508288));
#29220=CARTESIAN_POINT('Ctrl Pts',(-26.4458989623376,94.0469130356406,3.89467788983424));
#29221=CARTESIAN_POINT('Ctrl Pts',(-23.6224133012983,95.1669706094549,3.73669472458561));
#29222=CARTESIAN_POINT('Ctrl Pts',(-21.1414116530791,93.4144778137314,3.57871155933697));
#29223=CARTESIAN_POINT('Ctrl Pts',(-21.2532472272103,90.3790052214256,3.42072839408834));
#29224=CARTESIAN_POINT('Ctrl Pts',(-23.8564812740058,88.8138305079731,3.2627452288397));
#29225=CARTESIAN_POINT('Ctrl Pts',(-26.5898917954034,90.1386196891669,3.10476206359107));
#29226=CARTESIAN_POINT('Ctrl Pts',(-26.9741818729016,93.1517455407258,2.94677889834244));
#29227=CARTESIAN_POINT('Ctrl Pts',(-24.6607878581825,95.1201964337696,2.7887957330938));
#29228=CARTESIAN_POINT('Ctrl Pts',(-21.7480359224623,94.2585276484937,2.63081256784516));
#29229=CARTESIAN_POINT('Ctrl Pts',(-20.8778938613744,91.3482870150165,2.47282940259653));
#29230=CARTESIAN_POINT('Ctrl Pts',(-22.8396053811238,89.0291930982614,2.31484623734789));
#29231=CARTESIAN_POINT('Ctrl Pts',(-25.8538410662937,89.4046799738415,2.15686307209927));
#29232=CARTESIAN_POINT('Ctrl Pts',(-27.1865660698866,92.1342974242998,1.99887990685063));
#29233=CARTESIAN_POINT('Ctrl Pts',(-25.6289945736719,94.7419254122381,1.84089674160199));
#29234=CARTESIAN_POINT('Ctrl Pts',(-22.5938128499926,94.8628951691849,1.68291357635336));
#29235=CARTESIAN_POINT('Ctrl Pts',(-20.8342063323051,92.3863825780119,1.52493041110472));
#29236=CARTESIAN_POINT('Ctrl Pts',(-21.9458469482259,89.5609167225542,1.36694724585609));
#29237=CARTESIAN_POINT('Ctrl Pts',(-24.9211501867667,88.9446903547357,1.20896408060745));
#29238=CARTESIAN_POINT('Ctrl Pts',(-27.0599483982647,91.1061061878422,1.05098091535882));
#29239=CARTESIAN_POINT('Ctrl Pts',(-26.6354960985062,93.076689807963,0.945658805193063));
#29240=CARTESIAN_POINT('Ctrl Pts',(-26.054331550342,93.7564253212269,0.892997750110186));
#29241=CARTESIAN_POINT('Ctrl Pts',(-24.6501999979751,89.5679131979649,10.3210067496694));
#29242=CARTESIAN_POINT('Ctrl Pts',(-25.4549268544596,89.7830508320407,10.2683456945866));
#29243=CARTESIAN_POINT('Ctrl Pts',(-26.8204146828804,91.0717162505807,10.1630235844208));
#29244=CARTESIAN_POINT('Ctrl Pts',(-26.3190518827217,93.859235701585,10.0050404191722));
#29245=CARTESIAN_POINT('Ctrl Pts',(-23.7101077647069,94.9559962729138,9.84705725392353));
#29246=CARTESIAN_POINT('Ctrl Pts',(-21.3661024340368,93.3736899805099,9.68907408867489));
#29247=CARTESIAN_POINT('Ctrl Pts',(-21.4101550062448,90.544366147193,9.53109092342626));
#29248=CARTESIAN_POINT('Ctrl Pts',(-23.8037637600975,89.0358580140619,9.37310775817763));
#29249=CARTESIAN_POINT('Ctrl Pts',(-26.3751312394447,90.2156800266326,9.21512459292898));
#29250=CARTESIAN_POINT('Ctrl Pts',(-26.7922883167697,93.0140625006431,9.05714142768037));
#29251=CARTESIAN_POINT('Ctrl Pts',(-24.67668841891,94.8925962568123,8.89915826243172));
#29252=CARTESIAN_POINT('Ctrl Pts',(-21.9473365304931,94.1474755724248,8.74117509718309));
#29253=CARTESIAN_POINT('Ctrl Pts',(-21.0798070037785,91.4545069990835,8.58319193193445));
#29254=CARTESIAN_POINT('Ctrl Pts',(-22.8609987914095,89.256326172624,8.42520876668581));
#29255=CARTESIAN_POINT('Ctrl Pts',(-25.6753003227576,89.5467477390427,8.26722560143719));
#29256=CARTESIAN_POINT('Ctrl Pts',(-26.9700488609232,92.0623545136228,8.10924243618855));
#29257=CARTESIAN_POINT('Ctrl Pts',(-25.5708609338593,94.5214027969798,7.95125927093991));
#29258=CARTESIAN_POINT('Ctrl Pts',(-22.746848902053,94.6934530836676,7.79327610569128));
#29259=CARTESIAN_POINT('Ctrl Pts',(-21.0594875031757,92.4224492937484,7.63529294044265));
#29260=CARTESIAN_POINT('Ctrl Pts',(-22.0392713958159,89.7682696714667,7.47730977519401));
#29261=CARTESIAN_POINT('Ctrl Pts',(-24.7975030118093,89.1383455838149,7.31932660994537));
#29262=CARTESIAN_POINT('Ctrl Pts',(-26.8323721974004,91.104039749101,7.16134344469675));
#29263=CARTESIAN_POINT('Ctrl Pts',(-26.2981831143418,93.8824004317056,7.0033602794481));
#29264=CARTESIAN_POINT('Ctrl Pts',(-23.6794635098851,94.95335967792,6.84537711419948));
#29265=CARTESIAN_POINT('Ctrl Pts',(-21.3514814400011,93.345520889057,6.68739394895083));
#29266=CARTESIAN_POINT('Ctrl Pts',(-21.4257961049051,90.5172487296326,6.5294107837022));
#29267=CARTESIAN_POINT('Ctrl Pts',(-23.8350015651438,89.0338825812615,6.37142761845357));
#29268=CARTESIAN_POINT('Ctrl Pts',(-26.3938662378477,90.2408861719505,6.21344445320493));
#29269=CARTESIAN_POINT('Ctrl Pts',(-26.7814125248905,93.0434660468493,6.0554612879563));
#29270=CARTESIAN_POINT('Ctrl Pts',(-24.6461227163573,94.8995866016016,5.89747812270766));
#29271=CARTESIAN_POINT('Ctrl Pts',(-21.9247775505004,94.125683139552,5.73949495745904));
#29272=CARTESIAN_POINT('Ctrl Pts',(-21.0857299781457,91.4237125158365,5.5815117922104));
#29273=CARTESIAN_POINT('Ctrl Pts',(-22.8900247858913,89.2444543101509,5.42352862696176));
#29274=CARTESIAN_POINT('Ctrl Pts',(-25.7011049986632,89.5645700978948,5.26554546171313));
#29275=CARTESIAN_POINT('Ctrl Pts',(-26.9692249153015,92.0937039331857,5.10756229646449));
#29276=CARTESIAN_POINT('Ctrl Pts',(-25.544156487718,94.5378451029737,4.94957913121586));
#29277=CARTESIAN_POINT('Ctrl Pts',(-22.7184854204702,94.6800741418382,4.79159596596723));
#29278=CARTESIAN_POINT('Ctrl Pts',(-21.055191817558,92.3913844582627,4.63361280071859));
#29279=CARTESIAN_POINT('Ctrl Pts',(-22.0629397490182,89.7476957104498,4.47562963546996));
#29280=CARTESIAN_POINT('Ctrl Pts',(-24.8276674435624,89.1469238329133,4.31764647022132));
#29281=CARTESIAN_POINT('Ctrl Pts',(-26.8416725179065,91.1339894130133,4.15966330497269));
#29282=CARTESIAN_POINT('Ctrl Pts',(-26.2781836237349,93.9065561696585,4.00168013972405));
#29283=CARTESIAN_POINT('Ctrl Pts',(-23.6483044284461,94.9498113742255,3.84369697447542));
#29284=CARTESIAN_POINT('Ctrl Pts',(-21.3374251106716,93.3174870430051,3.68571380922678));
#29285=CARTESIAN_POINT('Ctrl Pts',(-21.4415921173467,90.4901568643789,3.52773064397815));
#29286=CARTESIAN_POINT('Ctrl Pts',(-23.8663223557907,89.0323062109474,3.36974747872951));
#29287=CARTESIAN_POINT('Ctrl Pts',(-26.4123028654849,90.2662545726625,3.21176431348088));
#29288=CARTESIAN_POINT('Ctrl Pts',(-26.7702421650231,93.0727703269818,3.05378114823224));
#29289=CARTESIAN_POINT('Ctrl Pts',(-24.6154776221154,94.9062445046611,2.89579798298361));
#29290=CARTESIAN_POINT('Ctrl Pts',(-21.902453142307,94.103660364463,2.73781481773497));
#29291=CARTESIAN_POINT('Ctrl Pts',(-21.0919767389813,91.3929749868548,2.57983165248634));
#29292=CARTESIAN_POINT('Ctrl Pts',(-22.9191736623219,89.2329013843028,2.4218484872377));
#29293=CARTESIAN_POINT('Ctrl Pts',(-25.7267231489403,89.5826411176466,2.26386532198907));
#29294=CARTESIAN_POINT('Ctrl Pts',(-26.9680631735609,92.1250886473484,2.10588215674044));
#29295=CARTESIAN_POINT('Ctrl Pts',(-25.5172943846158,94.553911534307,1.9478989914918));
#29296=CARTESIAN_POINT('Ctrl Pts',(-22.690235129749,94.6665863927075,1.78991582624317));
#29297=CARTESIAN_POINT('Ctrl Pts',(-21.0512848646155,92.3598883172517,1.63193266099453));
#29298=CARTESIAN_POINT('Ctrl Pts',(-22.0867002622527,89.7281647095134,1.4739494957459));
#29299=CARTESIAN_POINT('Ctrl Pts',(-24.8579869008516,89.1541929955161,1.31596633049727));
#29300=CARTESIAN_POINT('Ctrl Pts',(-26.8501276781025,91.1674005036292,1.15798316524863));
#29301=CARTESIAN_POINT('Ctrl Pts',(-26.4547800806521,93.0028611672493,1.05266105508287));
#29302=CARTESIAN_POINT('Ctrl Pts',(-25.913465996665,93.635987203375,0.999999999999996));
#29303=CARTESIAN_POINT('Ctrl Pts',(-26.5149491154365,92.0017493991467,9.11258330249198));
#29304=CARTESIAN_POINT('Ctrl Pts',(-26.5168561491793,92.2947752403159,9.09410267755477));
#29305=CARTESIAN_POINT('Ctrl Pts',(-26.4695027538977,92.5872051880346,9.07562205261757));
#29306=CARTESIAN_POINT('Ctrl Pts',(-26.3701621542389,92.8607543810029,9.05714142768036));
#29307=CARTESIAN_POINT('Ctrl Pts',(-26.0870883508165,93.6402404193662,9.00448037259748));
#29308=CARTESIAN_POINT('Ctrl Pts',(-25.3818883848633,94.2664183380893,8.95181931751459));
#29309=CARTESIAN_POINT('Ctrl Pts',(-24.5743964204838,94.4553205167195,8.89915826243172));
#29310=CARTESIAN_POINT('Ctrl Pts',(-23.7669044561044,94.6442226953498,8.84649720734884));
#29311=CARTESIAN_POINT('Ctrl Pts',(-22.8571204932987,94.3958491338873,8.79383615226596));
#29312=CARTESIAN_POINT('Ctrl Pts',(-22.2576402574435,93.8228342575992,8.74117509718308));
#29313=CARTESIAN_POINT('Ctrl Pts',(-21.6581600215882,93.249819381311,8.68851404210021));
#29314=CARTESIAN_POINT('Ctrl Pts',(-21.3689835126833,92.3521631901972,8.63585298701733));
#29315=CARTESIAN_POINT('Ctrl Pts',(-21.5212605561694,91.5369716235638,8.58319193193445));
#29316=CARTESIAN_POINT('Ctrl Pts',(-21.6735375996555,90.7217800569303,8.53053087685157));
#29317=CARTESIAN_POINT('Ctrl Pts',(-22.2672681955325,89.9890531147772,8.47786982176869));
#29318=CARTESIAN_POINT('Ctrl Pts',(-23.0331837486957,89.6710932381037,8.42520876668581));
#29319=CARTESIAN_POINT('Ctrl Pts',(-23.7990993018589,89.3531333614303,8.37254771160294));
#29320=CARTESIAN_POINT('Ctrl Pts',(-24.7371998123082,89.4499405502364,8.31988665652006));
#29321=CARTESIAN_POINT('Ctrl Pts',(-25.4220414905605,89.9176119404029,8.26722560143718));
#29322=CARTESIAN_POINT('Ctrl Pts',(-26.0924008378476,90.375393494611,8.21567816845545));
#29323=CARTESIAN_POINT('Ctrl Pts',(-26.5200994141618,91.1885197854572,8.16413073547372));
#29324=CARTESIAN_POINT('Ctrl Pts',(-26.5215632327497,92.0003195913041,8.11258330249199));
#29325=CARTESIAN_POINT('Ctrl Pts',(-24.7937992825329,89.0307770462543,10.));
#29326=CARTESIAN_POINT('Ctrl Pts',(-24.8868524293128,89.0648163030121,10.));
#29327=CARTESIAN_POINT('Ctrl Pts',(-24.9778402996117,89.1036238816563,10.));
#29328=CARTESIAN_POINT('Ctrl Pts',(-25.0665543950931,89.146871551718,10.));
#29329=CARTESIAN_POINT('Ctrl Pts',(-25.1572341761829,89.19107748351,10.));
#29330=CARTESIAN_POINT('Ctrl Pts',(-25.2455389715748,89.2399230660525,10.));
#29331=CARTESIAN_POINT('Ctrl Pts',(-25.3312171949433,89.2931033029458,10.));
#29332=CARTESIAN_POINT('Ctrl Pts',(-25.413669686943,89.3442813372769,10.));
#29333=CARTESIAN_POINT('Ctrl Pts',(-25.4936899468709,89.3994746514444,10.));
#29334=CARTESIAN_POINT('Ctrl Pts',(-25.5710207513823,89.4584414877532,10.));
#29335=CARTESIAN_POINT('Ctrl Pts',(-25.6386852053297,89.5100374695235,10.));
#29336=CARTESIAN_POINT('Ctrl Pts',(-25.7042902544872,89.5645232522079,10.));
#29337=CARTESIAN_POINT('Ctrl Pts',(-25.7676389322598,89.6217495880626,10.));
#29338=CARTESIAN_POINT('Ctrl Pts',(-25.78173773919,89.6344858138041,10.));
#29339=CARTESIAN_POINT('Ctrl Pts',(-25.7957273872409,89.6473604851229,10.));
#29340=CARTESIAN_POINT('Ctrl Pts',(-25.8095862319979,89.6603535287235,10.));
#29341=CARTESIAN_POINT('Ctrl Pts',(-25.8820169439212,89.7282592895964,10.));
#29342=CARTESIAN_POINT('Ctrl Pts',(-25.950981982325,89.7994868058506,10.));
#29343=CARTESIAN_POINT('Ctrl Pts',(-26.0162414008611,89.8737454733438,10.));
#29344=CARTESIAN_POINT('Ctrl Pts',(-26.0811411487042,89.9475948716925,10.));
#29345=CARTESIAN_POINT('Ctrl Pts',(-26.1423764967775,90.0244428983472,10.));
#29346=CARTESIAN_POINT('Ctrl Pts',(-26.1996678356882,90.1040304952653,10.));
#29347=CARTESIAN_POINT('Ctrl Pts',(-26.2548606489779,90.1807028764735,10.));
#29348=CARTESIAN_POINT('Ctrl Pts',(-26.3063932593322,90.2599185451886,10.));
#29349=CARTESIAN_POINT('Ctrl Pts',(-26.3539707411373,90.341459492214,10.));
#29350=CARTESIAN_POINT('Ctrl Pts',(-26.3739595056633,90.3757173538636,10.));
#29351=CARTESIAN_POINT('Ctrl Pts',(-26.393249578895,90.4103857572883,10.));
#29352=CARTESIAN_POINT('Ctrl Pts',(-26.4118164862517,90.4454488350539,10.));
#29353=CARTESIAN_POINT('Ctrl Pts',(-26.4248530614507,90.4700680374454,10.));
#29354=CARTESIAN_POINT('Ctrl Pts',(-26.4375330823773,90.4948818175359,10.));
#29355=CARTESIAN_POINT('Ctrl Pts',(-26.4498475905638,90.5198846886023,10.));
#29356=CARTESIAN_POINT('Ctrl Pts',(-26.457600065583,90.5356249951102,10.));
#29357=CARTESIAN_POINT('Ctrl Pts',(-26.4652085570304,90.5514423659275,10.));
#29358=CARTESIAN_POINT('Ctrl Pts',(-26.4726611641404,90.5673143053848,10.));
#29359=CARTESIAN_POINT('Ctrl Pts',(-26.514781719135,90.6570191414131,10.));
#29360=CARTESIAN_POINT('Ctrl Pts',(-26.5520000635457,90.7486086651382,10.));
#29361=CARTESIAN_POINT('Ctrl Pts',(-26.5840245510355,90.8418104101182,10.));
#29362=CARTESIAN_POINT('Ctrl Pts',(-26.6138870174205,90.9287199657321,10.));
#29363=CARTESIAN_POINT('Ctrl Pts',(-26.6392330675846,91.0170321959346,10.));
#29364=CARTESIAN_POINT('Ctrl Pts',(-26.6597756784745,91.1065348612826,10.));
#29365=CARTESIAN_POINT('Ctrl Pts',(-26.6612629487393,91.11301478993,10.));
#29366=CARTESIAN_POINT('Ctrl Pts',(-26.6627250182667,91.1195009595951,10.));
#29367=CARTESIAN_POINT('Ctrl Pts',(-26.6641617673287,91.1259932900523,10.));
#29368=CARTESIAN_POINT('Ctrl Pts',(-26.6847473682253,91.2190147697362,10.));
#29369=CARTESIAN_POINT('Ctrl Pts',(-26.7001391868307,91.313301977244,10.));
#29370=CARTESIAN_POINT('Ctrl Pts',(-26.710414230246,91.4084468885593,10.));
#29371=CARTESIAN_POINT('Ctrl Pts',(-26.7162318667374,91.4623170753475,10.));
#29372=CARTESIAN_POINT('Ctrl Pts',(-26.7204082723903,91.5164620291722,10.));
#29373=CARTESIAN_POINT('Ctrl Pts',(-26.7229505321309,91.5708049958447,10.));
#29374=CARTESIAN_POINT('Ctrl Pts',(-26.7235978728721,91.5846424553929,10.));
#29375=CARTESIAN_POINT('Ctrl Pts',(-26.7241391083581,91.5984913477053,10.));
#29376=CARTESIAN_POINT('Ctrl Pts',(-26.7245741747786,91.6123381701919,10.));
#29377=CARTESIAN_POINT('Ctrl Pts',(-26.727502988299,91.7055532725557,10.));
#29378=CARTESIAN_POINT('Ctrl Pts',(-26.7256324130775,91.7988256455911,10.));
#29379=CARTESIAN_POINT('Ctrl Pts',(-26.7190973170402,91.8917800191792,10.));
#29380=CARTESIAN_POINT('Ctrl Pts',(-26.7125517832716,91.9848828577297,10.));
#29381=CARTESIAN_POINT('Ctrl Pts',(-26.701326437817,92.0776676598524,10.));
#29382=CARTESIAN_POINT('Ctrl Pts',(-26.6855058890497,92.169745200331,10.));
#29383=CARTESIAN_POINT('Ctrl Pts',(-26.6699125051892,92.2605006131003,10.));
#29384=CARTESIAN_POINT('Ctrl Pts',(-26.6498544727619,92.350569772881,10.));
#29385=CARTESIAN_POINT('Ctrl Pts',(-26.625369821818,92.4395547318735,10.));
#29386=CARTESIAN_POINT('Ctrl Pts',(-26.6161277488857,92.4731433455226,10.));
#29387=CARTESIAN_POINT('Ctrl Pts',(-26.606254568394,92.5065771589137,10.));
#29388=CARTESIAN_POINT('Ctrl Pts',(-26.5957509020014,92.5398334420584,10.));
#29389=CARTESIAN_POINT('Ctrl Pts',(-26.5880549567592,92.5642000322064,10.));
#29390=CARTESIAN_POINT('Ctrl Pts',(-26.5800205276971,92.5884713019318,10.));
#29391=CARTESIAN_POINT('Ctrl Pts',(-26.5716476123613,92.6126380143925,10.));
#29392=CARTESIAN_POINT('Ctrl Pts',(-26.5664801186219,92.627552931161,10.));
#29393=CARTESIAN_POINT('Ctrl Pts',(-26.5611866874407,92.6424193349119,10.));
#29394=CARTESIAN_POINT('Ctrl Pts',(-26.5557685057611,92.6572331361345,10.));
#29395=CARTESIAN_POINT('Ctrl Pts',(-26.5240624701884,92.7439203194567,10.));
#29396=CARTESIAN_POINT('Ctrl Pts',(-26.4880796645806,92.8288333308672,10.));
#29397=CARTESIAN_POINT('Ctrl Pts',(-26.4478803904145,92.9115713473252,10.));
#29398=CARTESIAN_POINT('Ctrl Pts',(-26.4177309347899,92.9736248596687,10.));
#29399=CARTESIAN_POINT('Ctrl Pts',(-26.3852087264707,93.034454452489,10.));
#29400=CARTESIAN_POINT('Ctrl Pts',(-26.3503241152161,93.0938760327216,10.));
#29401=CARTESIAN_POINT('Ctrl Pts',(-26.3345452312659,93.1207533916747,10.));
#29402=CARTESIAN_POINT('Ctrl Pts',(-26.3182828580768,93.1473424862479,10.));
#29403=CARTESIAN_POINT('Ctrl Pts',(-26.3015371730653,93.1736252114869,10.));
#29404=CARTESIAN_POINT('Ctrl Pts',(-26.2924151850266,93.1879423746897,10.));
#29405=CARTESIAN_POINT('Ctrl Pts',(-26.2831549587563,93.2021604667855,10.));
#29406=CARTESIAN_POINT('Ctrl Pts',(-26.2737571737911,93.2162764754243,10.));
#29407=CARTESIAN_POINT('Ctrl Pts',(-26.22618210498,93.2877369402902,10.));
#29408=CARTESIAN_POINT('Ctrl Pts',(-26.1750818283943,93.3565881459249,10.));
#29409=CARTESIAN_POINT('Ctrl Pts',(-26.1204874011636,93.422476604652,10.));
#29410=CARTESIAN_POINT('Ctrl Pts',(-26.0743569378935,93.4781501464292,10.));
#29411=CARTESIAN_POINT('Ctrl Pts',(-26.0257310846976,93.5317080232741,10.));
#29412=CARTESIAN_POINT('Ctrl Pts',(-25.974612285206,93.5829128576333,10.));
#29413=CARTESIAN_POINT('Ctrl Pts',(-25.9557804971257,93.6017763403232,10.));
#29414=CARTESIAN_POINT('Ctrl Pts',(-25.9366102390046,93.6203202358367,10.));
#29415=CARTESIAN_POINT('Ctrl Pts',(-25.9171116625783,93.6385402433575,10.));
#29416=CARTESIAN_POINT('Origin',(-24.,92.,5.));
#29417=CARTESIAN_POINT('Origin',(92.,24.,1.));
#29418=CARTESIAN_POINT('Ctrl Pts',(90.0865340033349,25.6359872033749,1.));
#29419=CARTESIAN_POINT('Ctrl Pts',(90.0243936537204,25.5775905334472,1.));
#29420=CARTESIAN_POINT('Ctrl Pts',(89.9656286004716,25.515940174112,1.));
#29421=CARTESIAN_POINT('Ctrl Pts',(89.9102508840482,25.4514125531291,1.));
#29422=CARTESIAN_POINT('Ctrl Pts',(89.8535184531324,25.385306381983,1.));
#29423=CARTESIAN_POINT('Ctrl Pts',(89.8003406478074,25.3161799622637,1.00000000000001));
#29424=CARTESIAN_POINT('Ctrl Pts',(89.750759301611,25.2443917537902,1.00000000000001));
#29425=CARTESIAN_POINT('Ctrl Pts',(89.7378154616087,25.2256505304105,1.00000000000001));
#29426=CARTESIAN_POINT('Ctrl Pts',(89.7251169046858,25.2067276793656,1.));
#29427=CARTESIAN_POINT('Ctrl Pts',(89.7126647511175,25.1876291447746,1.));
#29428=CARTESIAN_POINT('Ctrl Pts',(89.7025039315658,25.1720449518382,1.));
#29429=CARTESIAN_POINT('Ctrl Pts',(89.6925067437675,25.1563428868077,1.));
#29430=CARTESIAN_POINT('Ctrl Pts',(89.6826826227138,25.1405407390384,1.));
#29431=CARTESIAN_POINT('Ctrl Pts',(89.6352352786345,25.0642214491697,1.));
#29432=CARTESIAN_POINT('Ctrl Pts',(89.5917715087151,24.985494938699,1.));
#29433=CARTESIAN_POINT('Ctrl Pts',(89.5523260662542,24.9047536930622,1.));
#29434=CARTESIAN_POINT('Ctrl Pts',(89.5204851860134,24.8395782970616,1.));
#29435=CARTESIAN_POINT('Ctrl Pts',(89.4912631200874,24.7730890249891,1.));
#29436=CARTESIAN_POINT('Ctrl Pts',(89.4646953255791,24.7054744889604,1.));
#29437=CARTESIAN_POINT('Ctrl Pts',(89.4539704661986,24.6781799240781,1.));
#29438=CARTESIAN_POINT('Ctrl Pts',(89.4436783251344,24.6507018348571,1.));
#29439=CARTESIAN_POINT('Ctrl Pts',(89.433822025196,24.6230520618988,1.));
#29440=CARTESIAN_POINT('Ctrl Pts',(89.4286038515389,24.6084135750653,1.));
#29441=CARTESIAN_POINT('Ctrl Pts',(89.4235083975283,24.5937282955295,1.));
#29442=CARTESIAN_POINT('Ctrl Pts',(89.4185398830814,24.5790097971537,1.));
#29443=CARTESIAN_POINT('Ctrl Pts',(89.389025801749,24.4915786418671,1.));
#29444=CARTESIAN_POINT('Ctrl Pts',(89.3639479999348,24.4028676051837,1.));
#29445=CARTESIAN_POINT('Ctrl Pts',(89.3433392465014,24.3132743791318,1.));
#29446=CARTESIAN_POINT('Ctrl Pts',(89.3224115745818,24.2222947064846,1.));
#29447=CARTESIAN_POINT('Ctrl Pts',(89.3060918371883,24.1304045235307,1.));
#29448=CARTESIAN_POINT('Ctrl Pts',(89.2944561926122,24.0379871349153,1.00000000000001));
#29449=CARTESIAN_POINT('Ctrl Pts',(89.2829117117522,23.9462938241557,1.00000000000001));
#29450=CARTESIAN_POINT('Ctrl Pts',(89.2759778689656,23.8540806067861,1.00000000000001));
#29451=CARTESIAN_POINT('Ctrl Pts',(89.273776000804,23.7617026893423,1.00000000000001));
#29452=CARTESIAN_POINT('Ctrl Pts',(89.2726808058124,23.715754510296,1.00000000000001));
#29453=CARTESIAN_POINT('Ctrl Pts',(89.2727570661434,23.6697653722625,1.));
#29454=CARTESIAN_POINT('Ctrl Pts',(89.2740245029826,23.6237782920667,1.));
#29455=CARTESIAN_POINT('Ctrl Pts',(89.2744412788452,23.6086561933353,1.));
#29456=CARTESIAN_POINT('Ctrl Pts',(89.2749869695608,23.5935324657531,1.));
#29457=CARTESIAN_POINT('Ctrl Pts',(89.275662091735,23.5784144647086,1.));
#29458=CARTESIAN_POINT('Ctrl Pts',(89.2799360088404,23.4827087010319,1.));
#29459=CARTESIAN_POINT('Ctrl Pts',(89.2893769673482,23.3875701065554,1.));
#29460=CARTESIAN_POINT('Ctrl Pts',(89.3040491413972,23.2933970076216,1.));
#29461=CARTESIAN_POINT('Ctrl Pts',(89.3082037215585,23.266730905703,1.));
#29462=CARTESIAN_POINT('Ctrl Pts',(89.3127780329822,23.2401420872658,1.));
#29463=CARTESIAN_POINT('Ctrl Pts',(89.3177742468288,23.2136393367139,1.));
#29464=CARTESIAN_POINT('Ctrl Pts',(89.3347391581862,23.1236478296161,1.));
#29465=CARTESIAN_POINT('Ctrl Pts',(89.356564364113,23.034648784227,1.));
#29466=CARTESIAN_POINT('Ctrl Pts',(89.3829472265017,22.9468744390315,1.));
#29467=CARTESIAN_POINT('Ctrl Pts',(89.4099265677864,22.8571156410599,1.));
#29468=CARTESIAN_POINT('Ctrl Pts',(89.4416721888927,22.7686368463988,1.));
#29469=CARTESIAN_POINT('Ctrl Pts',(89.4779146987112,22.6816901122092,1.));
#29470=CARTESIAN_POINT('Ctrl Pts',(89.4905815187872,22.6513020777246,1.));
#29471=CARTESIAN_POINT('Ctrl Pts',(89.5037981010522,22.6211012696727,1.00000000000001));
#29472=CARTESIAN_POINT('Ctrl Pts',(89.5175543776716,22.5910988047463,1.00000000000001));
#29473=CARTESIAN_POINT('Ctrl Pts',(89.5245011977754,22.5759477771625,1.00000000000001));
#29474=CARTESIAN_POINT('Ctrl Pts',(89.5315856607301,22.5608473343647,1.));
#29475=CARTESIAN_POINT('Ctrl Pts',(89.5388065372973,22.5457989337137,1.));
#29476=CARTESIAN_POINT('Ctrl Pts',(89.5448162869273,22.5332745373471,1.));
#29477=CARTESIAN_POINT('Ctrl Pts',(89.5509186846871,22.5207901225854,1.00000000000001));
#29478=CARTESIAN_POINT('Ctrl Pts',(89.5571091315649,22.5083537155743,1.00000000000001));
#29479=CARTESIAN_POINT('Ctrl Pts',(89.6000723368599,22.4220420295041,1.00000000000001));
#29480=CARTESIAN_POINT('Ctrl Pts',(89.6473225868892,22.337937009213,1.00000000000001));
#29481=CARTESIAN_POINT('Ctrl Pts',(89.6985178128694,22.2562887342086,1.00000000000001));
#29482=CARTESIAN_POINT('Ctrl Pts',(89.7507178517981,22.1730379417357,1.00000000000001));
#29483=CARTESIAN_POINT('Ctrl Pts',(89.8070195603585,22.0923405044241,1.));
#29484=CARTESIAN_POINT('Ctrl Pts',(89.8671152472941,22.0144688397376,1.));
#29485=CARTESIAN_POINT('Ctrl Pts',(89.9276789696687,21.9359906972714,1.));
#29486=CARTESIAN_POINT('Ctrl Pts',(89.9920964595121,21.8603816769157,1.));
#29487=CARTESIAN_POINT('Ctrl Pts',(90.0601019298659,21.7879401973074,1.));
#29488=CARTESIAN_POINT('Ctrl Pts',(90.0970286042451,21.7486047892127,1.));
#29489=CARTESIAN_POINT('Ctrl Pts',(90.1350139823262,21.7102037246147,1.));
#29490=CARTESIAN_POINT('Ctrl Pts',(90.1740207522492,21.6727885370382,1.));
#29491=CARTESIAN_POINT('Ctrl Pts',(90.186150608565,21.6611536118642,1.));
#29492=CARTESIAN_POINT('Ctrl Pts',(90.1983792592015,21.6496140448139,1.));
#29493=CARTESIAN_POINT('Ctrl Pts',(90.2107056469257,21.6381714501822,1.));
#29494=CARTESIAN_POINT('Ctrl Pts',(90.2219939257138,21.627692532826,1.));
#29495=CARTESIAN_POINT('Ctrl Pts',(90.2333584433832,21.6173003008198,1.));
#29496=CARTESIAN_POINT('Ctrl Pts',(90.2447937623118,21.6069996110817,1.));
#29497=CARTESIAN_POINT('Ctrl Pts',(90.3206028376455,21.5387124238838,1.));
#29498=CARTESIAN_POINT('Ctrl Pts',(90.3995782020434,21.4743922574611,0.999999999999998));
#29499=CARTESIAN_POINT('Ctrl Pts',(90.4813936898827,21.4143217382276,0.999999999999999));
#29500=CARTESIAN_POINT('Ctrl Pts',(90.5632801177989,21.3541991334127,1.));
#29501=CARTESIAN_POINT('Ctrl Pts',(90.6480121733501,21.2983327113302,1.));
#29502=CARTESIAN_POINT('Ctrl Pts',(90.7353078050742,21.2470320374408,1.));
#29503=CARTESIAN_POINT('Ctrl Pts',(90.8208396632406,21.1967678732862,1.));
#29504=CARTESIAN_POINT('Ctrl Pts',(90.9088332163986,21.1508861489069,1.));
#29505=CARTESIAN_POINT('Ctrl Pts',(90.9990569161034,21.1097141762738,1.));
#29506=CARTESIAN_POINT('Ctrl Pts',(91.0368467525653,21.0924694598887,1.00000000000001));
#29507=CARTESIAN_POINT('Ctrl Pts',(91.0750281840494,21.0760514837458,1.));
#29508=CARTESIAN_POINT('Ctrl Pts',(91.1135855898122,21.0604866736419,1.));
#29509=CARTESIAN_POINT('Ctrl Pts',(91.1435992944683,21.0483707751719,1.));
#29510=CARTESIAN_POINT('Ctrl Pts',(91.1738408319515,21.0367718698255,1.));
#29511=CARTESIAN_POINT('Ctrl Pts',(91.2042984301044,21.0256873776386,1.));
#29512=CARTESIAN_POINT('Ctrl Pts',(92.7937992825329,21.0307770462543,1.));
#29513=CARTESIAN_POINT('Ctrl Pts',(92.8886355471641,21.0654685754872,1.));
#29514=CARTESIAN_POINT('Ctrl Pts',(92.981428580578,21.1051505313063,1.00000000000001));
#29515=CARTESIAN_POINT('Ctrl Pts',(93.0719374504447,21.1495026644839,1.));
#29516=CARTESIAN_POINT('Ctrl Pts',(93.1637178577445,21.1944778901568,1.));
#29517=CARTESIAN_POINT('Ctrl Pts',(93.2531501397529,21.2442561370497,1.));
#29518=CARTESIAN_POINT('Ctrl Pts',(93.3399490406757,21.2985441485801,0.999999999999999));
#29519=CARTESIAN_POINT('Ctrl Pts',(93.3644577825898,21.3138730392628,0.999999999999999));
#29520=CARTESIAN_POINT('Ctrl Pts',(93.3887563291026,21.3295616963359,1.));
#29521=CARTESIAN_POINT('Ctrl Pts',(93.4128376624865,21.3456039733805,1.));
#29522=CARTESIAN_POINT('Ctrl Pts',(93.4321684182458,21.3584815551335,1.));
#29523=CARTESIAN_POINT('Ctrl Pts',(93.4513613131721,21.3715886263023,1.));
#29524=CARTESIAN_POINT('Ctrl Pts',(93.4703934284029,21.3849082414666,1.));
#29525=CARTESIAN_POINT('Ctrl Pts',(93.5531010557067,21.4427911280235,1.));
#29526=CARTESIAN_POINT('Ctrl Pts',(93.6328538471322,21.5047358078477,1.));
#29527=CARTESIAN_POINT('Ctrl Pts',(93.7093854474969,21.5704450409762,1.));
#29528=CARTESIAN_POINT('Ctrl Pts',(93.7683982885621,21.6211128502557,1.));
#29529=CARTESIAN_POINT('Ctrl Pts',(93.8254952341963,21.6740199048097,1.));
#29530=CARTESIAN_POINT('Ctrl Pts',(93.8805365802951,21.7290417093972,1.));
#29531=CARTESIAN_POINT('Ctrl Pts',(93.9098566848023,21.7583514042907,1.));
#29532=CARTESIAN_POINT('Ctrl Pts',(93.9385932130282,21.7882613322448,1.));
#29533=CARTESIAN_POINT('Ctrl Pts',(93.966723018163,21.8187535093172,1.));
#29534=CARTESIAN_POINT('Ctrl Pts',(93.9763569992674,21.8291965627383,1.));
#29535=CARTESIAN_POINT('Ctrl Pts',(93.9859190158138,21.8397071306493,1.));
#29536=CARTESIAN_POINT('Ctrl Pts',(93.9954015810245,21.8502769624256,1.));
#29537=CARTESIAN_POINT('Ctrl Pts',(94.0611940655502,21.9236131829668,1.));
#29538=CARTESIAN_POINT('Ctrl Pts',(94.1232543001003,21.9998957526439,1.));
#29539=CARTESIAN_POINT('Ctrl Pts',(94.1813384939113,22.0788462503669,1.));
#29540=CARTESIAN_POINT('Ctrl Pts',(94.2389162823979,22.1571084205125,1.));
#29541=CARTESIAN_POINT('Ctrl Pts',(94.2925874949548,22.2379929849892,1.));
#29542=CARTESIAN_POINT('Ctrl Pts',(94.3420688574455,22.3212511467048,0.999999999999999));
#29543=CARTESIAN_POINT('Ctrl Pts',(94.390117240581,22.4020981535756,0.999999999999999));
#29544=CARTESIAN_POINT('Ctrl Pts',(94.4342151409803,22.4851839694888,1.));
#29545=CARTESIAN_POINT('Ctrl Pts',(94.4740553951334,22.57029111177,1.));
#29546=CARTESIAN_POINT('Ctrl Pts',(94.4948666592991,22.6147483387141,1.));
#29547=CARTESIAN_POINT('Ctrl Pts',(94.5145153291242,22.6597572305835,1.));
#29548=CARTESIAN_POINT('Ctrl Pts',(94.532951917645,22.7052870236586,1.));
#29549=CARTESIAN_POINT('Ctrl Pts',(94.5400925813619,22.7229211397036,1.));
#29550=CARTESIAN_POINT('Ctrl Pts',(94.5470513788846,22.7406333941673,0.999999999999999));
#29551=CARTESIAN_POINT('Ctrl Pts',(94.5538252664571,22.7584219905631,0.999999999999999));
#29552=CARTESIAN_POINT('Ctrl Pts',(94.5589791553681,22.7719563825541,0.999999999999999));
#29553=CARTESIAN_POINT('Ctrl Pts',(94.5640259616331,22.7855350879592,0.999999999999999));
#29554=CARTESIAN_POINT('Ctrl Pts',(94.5689595142746,22.7991434114529,1.));
#29555=CARTESIAN_POINT('Ctrl Pts',(94.6006313710319,22.8865045695715,1.));
#29556=CARTESIAN_POINT('Ctrl Pts',(94.6276945170064,22.9752266495777,1.));
#29557=CARTESIAN_POINT('Ctrl Pts',(94.6498976668917,23.0650862424225,1.));
#29558=CARTESIAN_POINT('Ctrl Pts',(94.6549002608062,23.0853325162461,1.));
#29559=CARTESIAN_POINT('Ctrl Pts',(94.659655933924,23.1056365754165,1.));
#29560=CARTESIAN_POINT('Ctrl Pts',(94.6641614464107,23.1259959208575,1.));
#29561=CARTESIAN_POINT('Ctrl Pts',(94.684506977676,23.2179325652312,1.));
#29562=CARTESIAN_POINT('Ctrl Pts',(94.6997555099893,23.3109969010515,0.999999999999998));
#29563=CARTESIAN_POINT('Ctrl Pts',(94.7100169526532,23.4047971880022,0.999999999999998));
#29564=CARTESIAN_POINT('Ctrl Pts',(94.7207301009448,23.5027265354449,0.999999999999998));
#29565=CARTESIAN_POINT('Ctrl Pts',(94.7260074241417,23.6014592922061,0.999999999999998));
#29566=CARTESIAN_POINT('Ctrl Pts',(94.7259165033721,23.7005349801267,0.999999999999998));
#29567=CARTESIAN_POINT('Ctrl Pts',(94.72588138918,23.7387986546096,0.999999999999998));
#29568=CARTESIAN_POINT('Ctrl Pts',(94.7250449852703,23.7771132264404,0.999999999999997));
#29569=CARTESIAN_POINT('Ctrl Pts',(94.7234090502602,23.8154509913219,0.999999999999997));
#29570=CARTESIAN_POINT('Ctrl Pts',(94.7228214486292,23.8292213019001,0.999999999999996));
#29571=CARTESIAN_POINT('Ctrl Pts',(94.7221307047809,23.8429928066208,0.999999999999999));
#29572=CARTESIAN_POINT('Ctrl Pts',(94.7213377902191,23.8567525532216,0.999999999999999));
#29573=CARTESIAN_POINT('Ctrl Pts',(94.7159861969755,23.9496207769742,1.));
#29574=CARTESIAN_POINT('Ctrl Pts',(94.7059788948869,24.042101901153,0.999999999999996));
#29575=CARTESIAN_POINT('Ctrl Pts',(94.6914389407265,24.1338240294237,0.999999999999997));
#29576=CARTESIAN_POINT('Ctrl Pts',(94.6769360336291,24.2253124543804,0.999999999999997));
#29577=CARTESIAN_POINT('Ctrl Pts',(94.6579231315279,24.3160466905483,1.));
#29578=CARTESIAN_POINT('Ctrl Pts',(94.634473763784,24.4056405654129,1.));
#29579=CARTESIAN_POINT('Ctrl Pts',(94.6114256905903,24.4937011992063,1.));
#29580=CARTESIAN_POINT('Ctrl Pts',(94.5840912290588,24.5806609515592,0.999999999999999));
#29581=CARTESIAN_POINT('Ctrl Pts',(94.5524998627482,24.6661239164516,0.999999999999999));
#29582=CARTESIAN_POINT('Ctrl Pts',(94.5366373928654,24.7090360745829,0.999999999999999));
#29583=CARTESIAN_POINT('Ctrl Pts',(94.5197010824682,24.7515703293015,1.));
#29584=CARTESIAN_POINT('Ctrl Pts',(94.5016912752121,24.7936727822635,1.));
#29585=CARTESIAN_POINT('Ctrl Pts',(94.4963919593661,24.8060612655474,1.));
#29586=CARTESIAN_POINT('Ctrl Pts',(94.4909996852932,24.8184123442166,1.));
#29587=CARTESIAN_POINT('Ctrl Pts',(94.4855144272657,24.830724596362,1.));
#29588=CARTESIAN_POINT('Ctrl Pts',(94.4799210126452,24.8432796176239,1.));
#29589=CARTESIAN_POINT('Ctrl Pts',(94.4742345911846,24.855785977545,0.999999999999998));
#29590=CARTESIAN_POINT('Ctrl Pts',(94.4684564518667,24.8682403411912,0.999999999999998));
#29591=CARTESIAN_POINT('Ctrl Pts',(94.4309710840811,24.9490373549233,0.999999999999997));
#29592=CARTESIAN_POINT('Ctrl Pts',(94.3896160117749,25.0276775108318,1.));
#29593=CARTESIAN_POINT('Ctrl Pts',(94.3444610578896,25.1038131056636,1.));
#29594=CARTESIAN_POINT('Ctrl Pts',(94.3000642811839,25.1786703408565,0.999999999999999));
#29595=CARTESIAN_POINT('Ctrl Pts',(94.2519937015338,25.2511070843615,0.999999999999999));
#29596=CARTESIAN_POINT('Ctrl Pts',(94.2002794828524,25.3207586726253,0.999999999999999));
#29597=CARTESIAN_POINT('Ctrl Pts',(94.1501451979328,25.3882823181555,1.));
#29598=CARTESIAN_POINT('Ctrl Pts',(94.0965860653805,25.4531888295719,0.999999999999999));
#29599=CARTESIAN_POINT('Ctrl Pts',(94.0396018763204,25.5151056720679,0.999999999999999));
#29600=CARTESIAN_POINT('Ctrl Pts',(94.0184128643754,25.5381288428261,0.999999999999999));
#29601=CARTESIAN_POINT('Ctrl Pts',(93.9967500378537,25.5607382046462,0.999999999999998));
#29602=CARTESIAN_POINT('Ctrl Pts',(93.9746125472696,25.5829129376406,0.999999999999998));
#29603=CARTESIAN_POINT('Ctrl Pts',(93.9557857592068,25.6017713984427,0.999999999999998));
#29604=CARTESIAN_POINT('Ctrl Pts',(93.936615643811,25.6203154841753,0.999999999999998));
#29605=CARTESIAN_POINT('Ctrl Pts',(93.9171119325403,25.6385402784441,0.999999999999998));
#29606=CARTESIAN_POINT('Origin',(92.,24.,12.2084234471775));
#29607=CARTESIAN_POINT('Ctrl Pts',(88.9232326966468,24.0019373937314,9.70842344717745));
#29608=CARTESIAN_POINT('Ctrl Pts',(88.9222985312732,24.1261020010043,9.70197366100993));
#29609=CARTESIAN_POINT('Ctrl Pts',(88.9853329189178,25.263114277285,9.64286281975953));
#29610=CARTESIAN_POINT('Ctrl Pts',(90.4009679157595,27.2555128800837,9.53109092342627));
#29611=CARTESIAN_POINT('Ctrl Pts',(93.8523952892238,27.1179538105414,9.37310775817762));
#29612=CARTESIAN_POINT('Ctrl Pts',(95.6235723677572,24.1527148994824,9.215124592929));
#29613=CARTESIAN_POINT('Ctrl Pts',(94.1080772256066,21.0487573061686,9.05714142768035));
#29614=CARTESIAN_POINT('Ctrl Pts',(90.6804686178369,20.6217759976464,8.89915826243173));
#29615=CARTESIAN_POINT('Ctrl Pts',(89.0391555349924,22.5621016925695,8.78291893559742));
#29616=CARTESIAN_POINT('Ctrl Pts',(88.9237201879855,23.7866862070449,8.719340663846));
#29617=CARTESIAN_POINT('Ctrl Pts',(88.925632029797,23.9973209161002,8.70842344717745));
#29618=CARTESIAN_POINT('Ctrl Pts',(88.929711085108,23.9968960951897,9.79157655282255));
#29619=CARTESIAN_POINT('Ctrl Pts',(88.9347146766408,24.6903800819212,9.75572892504928));
#29620=CARTESIAN_POINT('Ctrl Pts',(89.5077563627456,26.4123579721077,9.66722024219312));
#29621=CARTESIAN_POINT('Ctrl Pts',(92.3539160756187,27.6088391884301,9.5260505042541));
#29622=CARTESIAN_POINT('Ctrl Pts',(95.2156041936735,25.6770751085581,9.36806733900546));
#29623=CARTESIAN_POINT('Ctrl Pts',(95.1618224985938,22.2228835192268,9.21008417375683));
#29624=CARTESIAN_POINT('Ctrl Pts',(92.2395757642924,20.3812156575975,9.05210100850819));
#29625=CARTESIAN_POINT('Ctrl Pts',(89.4675379096604,21.6531112748897,8.91259846819677));
#29626=CARTESIAN_POINT('Ctrl Pts',(88.9339205520176,23.3404824212939,8.82575698296822));
#29627=CARTESIAN_POINT('Ctrl Pts',(88.9296144608475,24.002135757227,8.79157655282255));
#29628=CARTESIAN_POINT('Ctrl Pts',(93.9134659966651,25.6359872033749,10.));
#29629=CARTESIAN_POINT('Ctrl Pts',(94.4547800806522,25.0028611672492,9.94733894491712));
#29630=CARTESIAN_POINT('Ctrl Pts',(94.850124624194,23.1673972202025,9.84201683475137));
#29631=CARTESIAN_POINT('Ctrl Pts',(92.8579881232768,21.154193771773,9.68403366950273));
#29632=CARTESIAN_POINT('Ctrl Pts',(90.0866994468077,21.7281636060897,9.5260505042541));
#29633=CARTESIAN_POINT('Ctrl Pts',(89.0512846745644,24.3598888261915,9.36806733900546));
#29634=CARTESIAN_POINT('Ctrl Pts',(90.6902348228159,26.6665865220793,9.21008417375683));
#29635=CARTESIAN_POINT('Ctrl Pts',(93.5172946610121,26.5539120605297,9.0521010085082));
#29636=CARTESIAN_POINT('Ctrl Pts',(94.9680635873854,24.1250885828687,8.89411784325955));
#29637=CARTESIAN_POINT('Ctrl Pts',(93.726723414825,21.5826408063378,8.73613467801094));
#29638=CARTESIAN_POINT('Ctrl Pts',(90.9191734977728,21.2329009513827,8.57815151276228));
#29639=CARTESIAN_POINT('Ctrl Pts',(89.0919763121477,23.3929749104686,8.42016834751366));
#29640=CARTESIAN_POINT('Ctrl Pts',(89.9024528317436,26.1036606678714,8.26218518226502));
#29641=CARTESIAN_POINT('Ctrl Pts',(92.6154777134031,26.906244937241,8.10420201701639));
#29642=CARTESIAN_POINT('Ctrl Pts',(94.7702425736134,25.0727704833333,7.94621885176775));
#29643=CARTESIAN_POINT('Ctrl Pts',(94.4123032215513,22.2662543178418,7.78823568651912));
#29644=CARTESIAN_POINT('Ctrl Pts',(91.866322336025,21.0323057724808,7.63025252127049));
#29645=CARTESIAN_POINT('Ctrl Pts',(89.441591739827,22.4901566418531,7.47226935602184));
#29646=CARTESIAN_POINT('Ctrl Pts',(89.3374247177566,25.3174872372792,7.31428619077322));
#29647=CARTESIAN_POINT('Ctrl Pts',(91.6483043765505,26.9498118095941,7.15630302552458));
#29648=CARTESIAN_POINT('Ctrl Pts',(94.2781839599183,25.906556450965,6.99831986027594));
#29649=CARTESIAN_POINT('Ctrl Pts',(94.8416729372438,23.1339892852383,6.84033669502732));
#29650=CARTESIAN_POINT('Ctrl Pts',(92.8276675656984,21.1469234118836,6.68235352977867));
#29651=CARTESIAN_POINT('Ctrl Pts',(90.0629394631723,21.7476953780895,6.52437036453004));
#29652=CARTESIAN_POINT('Ctrl Pts',(89.0551913830017,24.3913845160155,6.36638719928141));
#29653=CARTESIAN_POINT('Ctrl Pts',(90.7184852313611,26.6800745373299,6.20840403403277));
#29654=CARTESIAN_POINT('Ctrl Pts',(93.5441567155844,26.537845477475,6.05042086878414));
#29655=CARTESIAN_POINT('Ctrl Pts',(94.9692253534609,24.0937039470136,5.8924377035355));
#29656=CARTESIAN_POINT('Ctrl Pts',(93.70110524969,21.5645697385057,5.73445453828687));
#29657=CARTESIAN_POINT('Ctrl Pts',(90.8900246220956,21.2444539035236,5.57647137303823));
#29658=CARTESIAN_POINT('Ctrl Pts',(89.0857295480959,23.4237124307955,5.4184882077896));
#29659=CARTESIAN_POINT('Ctrl Pts',(89.9247772442662,26.1256834532325,5.26050504254097));
#29660=CARTESIAN_POINT('Ctrl Pts',(92.6461228117038,26.8995870294848,5.10252187729233));
#29661=CARTESIAN_POINT('Ctrl Pts',(94.781412935335,25.0434662008304,4.9445387120437));
#29662=CARTESIAN_POINT('Ctrl Pts',(94.393866591103,22.2408859123632,4.78655554679506));
#29663=CARTESIAN_POINT('Ctrl Pts',(91.8350015407957,21.0338821435613,4.62857238154643));
#29664=CARTESIAN_POINT('Ctrl Pts',(89.4257957250371,22.5172485108266,4.4705892162978));
#29665=CARTESIAN_POINT('Ctrl Pts',(89.3514810491689,25.3455210876135,4.31260605104916));
#29666=CARTESIAN_POINT('Ctrl Pts',(91.6794634625817,26.953360113734,4.15462288580053));
#29667=CARTESIAN_POINT('Ctrl Pts',(94.2981834534832,25.8824007094939,3.99663972055189));
#29668=CARTESIAN_POINT('Ctrl Pts',(94.8323726153541,23.1040396168705,3.83865655530326));
#29669=CARTESIAN_POINT('Ctrl Pts',(92.797503129515,21.1383451615613,3.68067339005462));
#29670=CARTESIAN_POINT('Ctrl Pts',(90.0392711064376,21.7682693420746,3.52269022480599));
#29671=CARTESIAN_POINT('Ctrl Pts',(89.0594870693288,24.4224493562101,3.36470705955735));
#29672=CARTESIAN_POINT('Ctrl Pts',(90.7468487169863,26.6934534808945,3.20672389430872));
#29673=CARTESIAN_POINT('Ctrl Pts',(93.5708611659363,26.521403169517,3.04874072906008));
#29674=CARTESIAN_POINT('Ctrl Pts',(94.9700492986991,24.0623545219302,2.89075756381145));
#29675=CARTESIAN_POINT('Ctrl Pts',(93.6753005709137,21.5467473787504,2.73277439856282));
#29676=CARTESIAN_POINT('Ctrl Pts',(90.8609986216085,21.2563257644251,2.57479123331418));
#29677=CARTESIAN_POINT('Ctrl Pts',(89.0798065759794,23.4545069249601,2.41680806806555));
#29678=CARTESIAN_POINT('Ctrl Pts',(89.947336222007,26.1474758771512,2.25882490281691));
#29679=CARTESIAN_POINT('Ctrl Pts',(92.6766885285289,26.8925967067901,2.10084173756828));
#29680=CARTESIAN_POINT('Ctrl Pts',(94.7922887122239,25.0140626065851,1.94285857231964));
#29681=CARTESIAN_POINT('Ctrl Pts',(94.3751316170022,22.215679845363,1.78487540707101));
#29682=CARTESIAN_POINT('Ctrl Pts',(91.8037636898017,21.0358574238383,1.62689224182237));
#29683=CARTESIAN_POINT('Ctrl Pts',(89.410154680019,22.5443662144373,1.46890907657374));
#29684=CARTESIAN_POINT('Ctrl Pts',(89.3661019891307,25.3736896687445,1.3109259113251));
#29685=CARTESIAN_POINT('Ctrl Pts',(91.7101077177225,26.9559976441494,1.15294274607647));
#29686=CARTESIAN_POINT('Ctrl Pts',(94.3190524504204,25.8592343694376,0.994959580827835));
#29687=CARTESIAN_POINT('Ctrl Pts',(94.8204140260176,23.0717206863195,0.836976415579202));
#29688=CARTESIAN_POINT('Ctrl Pts',(93.4549268544596,21.7830508320407,0.731654305413445));
#29689=CARTESIAN_POINT('Ctrl Pts',(92.6501999979751,21.5679131979649,0.678993250330566));
#29690=CARTESIAN_POINT('Ctrl Pts',(94.0543315503421,25.7564253212268,10.1070022498898));
#29691=CARTESIAN_POINT('Ctrl Pts',(94.6354960985062,25.0766898079629,10.0543411948069));
#29692=CARTESIAN_POINT('Ctrl Pts',(95.0599451195336,23.1061026626961,9.94901908464117));
#29693=CARTESIAN_POINT('Ctrl Pts',(92.9211514991843,20.9446911881392,9.79103591939255));
#29694=CARTESIAN_POINT('Ctrl Pts',(89.9458460727495,21.5609155378985,9.63305275414391));
#29695=CARTESIAN_POINT('Ctrl Pts',(88.834206128263,24.3863831244189,9.47506958889527));
#29696=CARTESIAN_POINT('Ctrl Pts',(90.5938125204637,26.8628953080808,9.31708642364664));
#29697=CARTESIAN_POINT('Ctrl Pts',(93.628994870416,26.7419259772002,9.159103258398));
#29698=CARTESIAN_POINT('Ctrl Pts',(95.1865665141759,24.1342973550732,9.00112009314937));
#29699=CARTESIAN_POINT('Ctrl Pts',(93.8538413517522,21.4046796396148,8.84313692790074));
#29700=CARTESIAN_POINT('Ctrl Pts',(90.8396052044608,21.0291926334706,8.6851537626521));
#29701=CARTESIAN_POINT('Ctrl Pts',(88.8778934031181,23.348286933007,8.52717059740347));
#29702=CARTESIAN_POINT('Ctrl Pts',(89.7480355890358,26.2585279742383,8.36918743215483));
#29703=CARTESIAN_POINT('Ctrl Pts',(92.6607879561905,27.1201968981952,8.2112042669062));
#29704=CARTESIAN_POINT('Ctrl Pts',(94.9741823115716,25.1517457085876,8.05322110165757));
#29705=CARTESIAN_POINT('Ctrl Pts',(94.5898921776827,22.1386194155869,7.89523793640892));
#29706=CARTESIAN_POINT('Ctrl Pts',(91.8564812527851,20.8138300372275,7.7372547711603));
#29707=CARTESIAN_POINT('Ctrl Pts',(89.2532468218983,22.3790049825178,7.57927160591166));
#29708=CARTESIAN_POINT('Ctrl Pts',(89.1414112312387,25.4144780223077,7.42128844066303));
#29709=CARTESIAN_POINT('Ctrl Pts',(91.6224132455821,27.1669710768744,7.26330527541439));
#29710=CARTESIAN_POINT('Ctrl Pts',(94.4458993232702,26.0469133376563,7.10532211016575));
#29711=CARTESIAN_POINT('Ctrl Pts',(95.0508712362317,23.0702353021324,6.94733894491713));
#29712=CARTESIAN_POINT('Ctrl Pts',(92.8885988025775,20.9368855988426,6.78935577966848));
#29713=CARTESIAN_POINT('Ctrl Pts',(89.9203369264657,21.5818852000316,6.63137261441985));
#29714=CARTESIAN_POINT('Ctrl Pts',(88.8384004407904,24.4201974641658,6.47338944917122));
#29715=CARTESIAN_POINT('Ctrl Pts',(90.624142667791,26.8773762841363,6.31540628392259));
#29716=CARTESIAN_POINT('Ctrl Pts',(93.6578344559174,26.7246766043172,6.15742311867394));
#29717=CARTESIAN_POINT('Ctrl Pts',(95.1878138071549,24.1006022448672,5.99943995342532));
#29718=CARTESIAN_POINT('Ctrl Pts',(93.8263372283497,21.3852782157794,5.84145678817669));
#29719=CARTESIAN_POINT('Ctrl Pts',(90.8083104466419,21.0415960909264,5.68347362292804));
#29720=CARTESIAN_POINT('Ctrl Pts',(88.8711867647448,23.3812872883291,5.52549045767941));
#29721=CARTESIAN_POINT('Ctrl Pts',(89.7720034803222,26.2821720331725,5.36750729243078));
#29722=CARTESIAN_POINT('Ctrl Pts',(92.693689085561,27.1130488485372,5.20952412718214));
#29723=CARTESIAN_POINT('Ctrl Pts',(94.9861750130637,25.120284103202,5.05154096193351));
#29724=CARTESIAN_POINT('Ctrl Pts',(94.5700982792398,22.1113834386491,4.89355779668487));
#29725=CARTESIAN_POINT('Ctrl Pts',(91.8228546830244,20.8155224576056,4.73557463143624));
#29726=CARTESIAN_POINT('Ctrl Pts',(89.2362879359766,22.4080913008987,4.57759146618761));
#29727=CARTESIAN_POINT('Ctrl Pts',(89.1565023617591,25.4445756688399,4.41960830093897));
#29728=CARTESIAN_POINT('Ctrl Pts',(91.6558662014358,27.1707806000943,4.26162513569034));
#29729=CARTESIAN_POINT('Ctrl Pts',(94.4673711396979,26.0209792986337,4.1036419704417));
#29730=CARTESIAN_POINT('Ctrl Pts',(95.0408862431775,23.0380807988606,3.94565880519307));
#29731=CARTESIAN_POINT('Ctrl Pts',(92.8562137207113,20.9276758348255,3.78767563994443));
#29732=CARTESIAN_POINT('Ctrl Pts',(89.8949261524727,21.6039737782472,3.6296924746958));
#29733=CARTESIAN_POINT('Ctrl Pts',(88.8430123669848,24.4535492359919,3.47170930944716));
#29734=CARTESIAN_POINT('Ctrl Pts',(90.6545942167075,26.8917401588657,3.31372614419853));
#29735=CARTESIAN_POINT('Ctrl Pts',(93.6865048346898,26.7070238464122,3.15574297894989));
#29736=CARTESIAN_POINT('Ctrl Pts',(95.1886984095997,24.0669449375797,2.99775981370126));
#29737=CARTESIAN_POINT('Ctrl Pts',(93.7986328605434,21.3661438094138,2.83977664845263));
#29738=CARTESIAN_POINT('Ctrl Pts',(90.7771476098394,21.0543419345702,2.68179348320399));
#29739=CARTESIAN_POINT('Ctrl Pts',(88.864827755224,23.4143488117893,2.52381031795536));
#29740=CARTESIAN_POINT('Ctrl Pts',(89.7962232050506,26.305568771914,2.36582715270672));
#29741=CARTESIAN_POINT('Ctrl Pts',(92.72650498955,27.1055439122155,2.20784398745809));
#29742=CARTESIAN_POINT('Ctrl Pts',(94.9978514429748,25.0887158749415,2.04986082220945));
#29743=CARTESIAN_POINT('Ctrl Pts',(94.5499840736793,22.0843217512249,1.89187765696082));
#29744=CARTESIAN_POINT('Ctrl Pts',(91.7893171636885,20.8176431540805,1.73389449171218));
#29745=CARTESIAN_POINT('Ctrl Pts',(89.2194954283924,22.4372053558113,1.57591132646355));
#29746=CARTESIAN_POINT('Ctrl Pts',(89.1721996661856,25.4748179647818,1.41792816121491));
#29747=CARTESIAN_POINT('Ctrl Pts',(91.6887664255746,27.173612300243,1.25994499596628));
#29748=CARTESIAN_POINT('Ctrl Pts',(94.4897764706037,25.9961074987865,1.10196183071765));
#29749=CARTESIAN_POINT('Ctrl Pts',(95.0280472863242,23.0033826130449,0.943978665469013));
#29750=CARTESIAN_POINT('Ctrl Pts',(93.5620356702265,21.6198434520492,0.838656555303256));
#29751=CARTESIAN_POINT('Ctrl Pts',(92.698066426161,21.3888678140614,0.785995500220377));
#29752=CARTESIAN_POINT('Ctrl Pts',(94.1951971040191,25.8768634390787,10.2140044997796));
#29753=CARTESIAN_POINT('Ctrl Pts',(94.8162121163602,25.1505184486767,10.1613434446967));
#29754=CARTESIAN_POINT('Ctrl Pts',(95.2697656148731,23.0448081051897,10.056021334531));
#29755=CARTESIAN_POINT('Ctrl Pts',(92.9843148750919,20.7351886045054,9.89803816928235));
#29756=CARTESIAN_POINT('Ctrl Pts',(89.8049926986913,21.3936674697073,9.74005500403372));
#29757=CARTESIAN_POINT('Ctrl Pts',(88.6171275819614,24.4128774226463,9.58207183878508));
#29758=CARTESIAN_POINT('Ctrl Pts',(90.4973902181116,27.0592040940823,9.42408867353646));
#29759=CARTESIAN_POINT('Ctrl Pts',(93.7406950798199,26.9299398938708,9.26610550828781));
#29760=CARTESIAN_POINT('Ctrl Pts',(95.4050694409666,24.1435061272778,9.10812234303919));
#29761=CARTESIAN_POINT('Ctrl Pts',(93.9809592886795,21.2267184728917,8.95013917779054));
#29762=CARTESIAN_POINT('Ctrl Pts',(90.7600369111488,20.8254843155585,8.79215601254192));
#29763=CARTESIAN_POINT('Ctrl Pts',(88.6638104940886,23.3035989555453,8.63417284729328));
#29764=CARTESIAN_POINT('Ctrl Pts',(89.5936183463281,26.4133952806053,8.47618968204464));
#29765=CARTESIAN_POINT('Ctrl Pts',(92.7060981989779,27.3341488591493,8.31820651679601));
#29766=CARTESIAN_POINT('Ctrl Pts',(95.1781220495298,25.2307209338419,8.16022335154737));
#29767=CARTESIAN_POINT('Ctrl Pts',(94.7674811338141,22.010984513332,8.00224018629874));
#29768=CARTESIAN_POINT('Ctrl Pts',(91.8466401695451,20.5953543019742,7.84425702105011));
#29769=CARTESIAN_POINT('Ctrl Pts',(89.0649019039696,22.2678533231826,7.68627385580147));
#29770=CARTESIAN_POINT('Ctrl Pts',(88.9453977447207,25.5114688073361,7.52829069055284));
#29771=CARTESIAN_POINT('Ctrl Pts',(91.5965221146138,27.3841303441547,7.3703075253042));
#29772=CARTESIAN_POINT('Ctrl Pts',(94.613614686622,26.1872702243476,7.21232436005557));
#29773=CARTESIAN_POINT('Ctrl Pts',(95.2600695352199,23.0064813190265,7.05434119480693));
#29774=CARTESIAN_POINT('Ctrl Pts',(92.9495300394564,20.7268477858015,6.8963580295583));
#29775=CARTESIAN_POINT('Ctrl Pts',(89.7777343897591,21.4160750219737,6.73837486430966));
#29776=CARTESIAN_POINT('Ctrl Pts',(88.621609498579,24.449010412316,6.58039169906103));
#29777=CARTESIAN_POINT('Ctrl Pts',(90.529800104221,27.0746780309427,6.42240853381239));
#29778=CARTESIAN_POINT('Ctrl Pts',(93.7715121962504,26.9115077311595,6.26442536856376));
#29779=CARTESIAN_POINT('Ctrl Pts',(95.406402260849,24.1075005427208,6.10644220331512));
#29780=CARTESIAN_POINT('Ctrl Pts',(93.9515692070094,21.205986693053,5.94845903806649));
#29781=CARTESIAN_POINT('Ctrl Pts',(90.7265962711881,20.8387382783291,5.79047587281786));
#29782=CARTESIAN_POINT('Ctrl Pts',(88.6566439813937,23.3388621458627,5.63249270756922));
#29783=CARTESIAN_POINT('Ctrl Pts',(89.6192297163781,26.4386606131126,5.47450954232059));
#29784=CARTESIAN_POINT('Ctrl Pts',(92.7412553594183,27.3265106675896,5.31652637707196));
#29785=CARTESIAN_POINT('Ctrl Pts',(95.1909370907925,25.1971020055736,5.15854321182332));
#29786=CARTESIAN_POINT('Ctrl Pts',(94.7463299673765,21.9818809649349,5.00056004657469));
#29787=CARTESIAN_POINT('Ctrl Pts',(91.8107078252533,20.59716277165,4.84257688132604));
#29788=CARTESIAN_POINT('Ctrl Pts',(89.046780146916,22.2989340909708,4.68459371607742));
#29789=CARTESIAN_POINT('Ctrl Pts',(88.9615236743494,25.5436302500664,4.52661055082878));
#29790=CARTESIAN_POINT('Ctrl Pts',(91.6322689402898,27.3882010864546,4.36862738558015));
#29791=CARTESIAN_POINT('Ctrl Pts',(94.6365588259127,26.1595578877736,4.21064422033151));
#29792=CARTESIAN_POINT('Ctrl Pts',(95.249399871001,22.9721219808507,4.05266105508288));
#29793=CARTESIAN_POINT('Ctrl Pts',(92.9149243119076,20.7170065080898,3.89467788983424));
#29794=CARTESIAN_POINT('Ctrl Pts',(89.7505811985077,21.4396782144198,3.73669472458561));
#29795=CARTESIAN_POINT('Ctrl Pts',(88.6265376646408,24.4846491157739,3.57871155933697));
#29796=CARTESIAN_POINT('Ctrl Pts',(90.5623397164288,27.0900268368369,3.42072839408834));
#29797=CARTESIAN_POINT('Ctrl Pts',(93.8021485034431,26.8926445233075,3.2627452288397));
#29798=CARTESIAN_POINT('Ctrl Pts',(95.4073475205004,24.0715353532293,3.10476206359107));
#29799=CARTESIAN_POINT('Ctrl Pts',(93.9219651501729,21.1855402400771,2.94677889834244));
#29800=CARTESIAN_POINT('Ctrl Pts',(90.6932965980705,20.8523581047152,2.7887957330938));
#29801=CARTESIAN_POINT('Ctrl Pts',(88.6498489344685,23.3741906986185,2.63081256784517));
#29802=CARTESIAN_POINT('Ctrl Pts',(89.645110188094,26.4636616666768,2.47282940259653));
#29803=CARTESIAN_POINT('Ctrl Pts',(92.776321450571,27.3184911176409,2.3148462373479));
#29804=CARTESIAN_POINT('Ctrl Pts',(95.2034141737259,25.1633691432978,2.15686307209926));
#29805=CARTESIAN_POINT('Ctrl Pts',(94.7248365303563,21.9529636570868,1.99887990685063));
#29806=CARTESIAN_POINT('Ctrl Pts',(91.7748706375752,20.5994288843227,1.84089674160199));
#29807=CARTESIAN_POINT('Ctrl Pts',(89.0288361767659,22.3300444971853,1.68291357635336));
#29808=CARTESIAN_POINT('Ctrl Pts',(88.9782973432405,25.5759462608191,1.52493041110473));
#29809=CARTESIAN_POINT('Ctrl Pts',(91.6674251334267,27.3912269563367,1.36694724585609));
#29810=CARTESIAN_POINT('Ctrl Pts',(94.660500490787,26.1329806281354,1.20896408060746));
#29811=CARTESIAN_POINT('Ctrl Pts',(95.2356805466308,22.9350445397703,1.05098091535882));
#29812=CARTESIAN_POINT('Ctrl Pts',(93.6691444859934,21.4566360720578,0.945658805193066));
#29813=CARTESIAN_POINT('Ctrl Pts',(92.7459328543469,21.2098224301578,0.892997750110188));
#29814=CARTESIAN_POINT('Ctrl Pts',(94.3360626576961,25.9973015569306,10.3210067496694));
#29815=CARTESIAN_POINT('Ctrl Pts',(94.9969281342143,25.2243470893904,10.2683456945866));
#29816=CARTESIAN_POINT('Ctrl Pts',(95.4795861102126,22.9835135476832,10.1630235844208));
#29817=CARTESIAN_POINT('Ctrl Pts',(93.0474782509995,20.5256860208715,10.0050404191722));
#29818=CARTESIAN_POINT('Ctrl Pts',(89.664139324633,21.2264194015161,9.84705725392353));
#29819=CARTESIAN_POINT('Ctrl Pts',(88.4000490356599,24.4393717208737,9.68907408867489));
#29820=CARTESIAN_POINT('Ctrl Pts',(90.4009679157595,27.2555128800837,9.53109092342627));
#29821=CARTESIAN_POINT('Ctrl Pts',(93.8523952892238,27.1179538105414,9.37310775817762));
#29822=CARTESIAN_POINT('Ctrl Pts',(95.6235723677572,24.1527148994824,9.215124592929));
#29823=CARTESIAN_POINT('Ctrl Pts',(94.1080772256066,21.0487573061686,9.05714142768035));
#29824=CARTESIAN_POINT('Ctrl Pts',(90.6804686178369,20.6217759976464,8.89915826243173));
#29825=CARTESIAN_POINT('Ctrl Pts',(88.4497275850589,23.2589109780836,8.74117509718308));
#29826=CARTESIAN_POINT('Ctrl Pts',(89.4392011036202,26.5682625869723,8.58319193193445));
#29827=CARTESIAN_POINT('Ctrl Pts',(92.7514084417654,27.5481008201034,8.42520876668582));
#29828=CARTESIAN_POINT('Ctrl Pts',(95.382061787488,25.3096961590962,8.26722560143718));
#29829=CARTESIAN_POINT('Ctrl Pts',(94.9450700899456,21.8833496110771,8.10924243618856));
#29830=CARTESIAN_POINT('Ctrl Pts',(91.8367990863051,20.3768785667209,7.95125927093992));
#29831=CARTESIAN_POINT('Ctrl Pts',(88.876556986041,22.1567016638473,7.79327610569128));
#29832=CARTESIAN_POINT('Ctrl Pts',(88.7493842582027,25.6084595923645,7.63529294044265));
#29833=CARTESIAN_POINT('Ctrl Pts',(91.5706309836454,27.601289611435,7.47730977519401));
#29834=CARTESIAN_POINT('Ctrl Pts',(94.781330049974,26.327627111039,7.31932660994538));
#29835=CARTESIAN_POINT('Ctrl Pts',(95.4692678342078,22.9427273359205,7.16134344469674));
#29836=CARTESIAN_POINT('Ctrl Pts',(93.0104612763355,20.5168099727604,7.00336027944811));
#29837=CARTESIAN_POINT('Ctrl Pts',(89.6351318530524,21.2502648439158,6.84537711419948));
#29838=CARTESIAN_POINT('Ctrl Pts',(88.4048185563678,24.4778233604662,6.68739394895084));
#29839=CARTESIAN_POINT('Ctrl Pts',(90.4354575406507,27.2719797777491,6.5294107837022));
#29840=CARTESIAN_POINT('Ctrl Pts',(93.8851899365835,27.0983388580017,6.37142761845357));
#29841=CARTESIAN_POINT('Ctrl Pts',(95.624990714543,24.1143988405745,6.21344445320494));
#29842=CARTESIAN_POINT('Ctrl Pts',(94.0768011856692,21.0266951703267,6.0554612879563));
#29843=CARTESIAN_POINT('Ctrl Pts',(90.6448820957342,20.6358804657318,5.89747812270767));
#29844=CARTESIAN_POINT('Ctrl Pts',(88.4421011980427,23.2964370033963,5.73949495745903));
#29845=CARTESIAN_POINT('Ctrl Pts',(89.4664559524339,26.5951491930526,5.5815117922104));
#29846=CARTESIAN_POINT('Ctrl Pts',(92.7888216332755,27.5399724866421,5.42352862696176));
#29847=CARTESIAN_POINT('Ctrl Pts',(95.3956991685213,25.2739199079453,5.26554546171313));
#29848=CARTESIAN_POINT('Ctrl Pts',(94.9225616555133,21.8523784912208,5.1075622964645));
#29849=CARTESIAN_POINT('Ctrl Pts',(91.798560967482,20.3788030856943,4.94957913121586));
#29850=CARTESIAN_POINT('Ctrl Pts',(88.8572723578556,22.189776881043,4.79159596596723));
#29851=CARTESIAN_POINT('Ctrl Pts',(88.7665449869396,25.642684831293,4.63361280071859));
#29852=CARTESIAN_POINT('Ctrl Pts',(91.608671679144,27.6056215728149,4.47562963546996));
#29853=CARTESIAN_POINT('Ctrl Pts',(94.8057465121273,26.2981364769134,4.31764647022132));
#29854=CARTESIAN_POINT('Ctrl Pts',(95.4579134988245,22.9061631628408,4.15966330497269));
#29855=CARTESIAN_POINT('Ctrl Pts',(92.973634903104,20.506337181354,4.00168013972405));
#29856=CARTESIAN_POINT('Ctrl Pts',(89.6062362445426,21.2753826505923,3.84369697447542));
#29857=CARTESIAN_POINT('Ctrl Pts',(88.4100629622968,24.5157489955558,3.68571380922678));
#29858=CARTESIAN_POINT('Ctrl Pts',(90.47008521615,27.2883135148081,3.52773064397815));
#29859=CARTESIAN_POINT('Ctrl Pts',(93.9177921721967,27.0782652002028,3.36974747872952));
#29860=CARTESIAN_POINT('Ctrl Pts',(95.6259966314009,24.0761257688788,3.21176431348088));
#29861=CARTESIAN_POINT('Ctrl Pts',(94.0452974398027,21.0049366707405,3.05378114823225));
#29862=CARTESIAN_POINT('Ctrl Pts',(90.6094455863014,20.6503742748602,2.89579798298361));
#29863=CARTESIAN_POINT('Ctrl Pts',(88.434870113713,23.3340325854478,2.73781481773498));
#29864=CARTESIAN_POINT('Ctrl Pts',(89.4939971711376,26.6217545614397,2.57983165248634));
#29865=CARTESIAN_POINT('Ctrl Pts',(92.8261379115921,27.5314383230663,2.42184848723771));
#29866=CARTESIAN_POINT('Ctrl Pts',(95.4089769044768,25.2380224116542,2.26386532198907));
#29867=CARTESIAN_POINT('Ctrl Pts',(94.8996889870333,21.8216055629487,2.10588215674044));
#29868=CARTESIAN_POINT('Ctrl Pts',(91.760424111462,20.3812146145649,1.94789899149181));
#29869=CARTESIAN_POINT('Ctrl Pts',(88.8381769251393,22.2228836385593,1.78991582624317));
#29870=CARTESIAN_POINT('Ctrl Pts',(88.7843950202953,25.6770745568565,1.63193266099454));
#29871=CARTESIAN_POINT('Ctrl Pts',(91.6460838412789,27.6088416124303,1.47394949574591));
#29872=CARTESIAN_POINT('Ctrl Pts',(94.8312245109702,26.2698537574842,1.31596633049727));
#29873=CARTESIAN_POINT('Ctrl Pts',(95.4433138069375,22.8667064664957,1.15798316524863));
#29874=CARTESIAN_POINT('Ctrl Pts',(93.7762533017603,21.2934286920664,1.05266105508288));
#29875=CARTESIAN_POINT('Ctrl Pts',(92.7937992825328,21.0307770462543,0.999999999999999));
#29876=CARTESIAN_POINT('Ctrl Pts',(93.9134659966651,25.6359872033749,10.));
#29877=CARTESIAN_POINT('Ctrl Pts',(93.9750770243691,25.5780879660668,10.));
#29878=CARTESIAN_POINT('Ctrl Pts',(94.0333189464364,25.5170381633454,10.));
#29879=CARTESIAN_POINT('Ctrl Pts',(94.088194094267,25.4532225723848,10.));
#29880=CARTESIAN_POINT('Ctrl Pts',(94.1445219524055,25.3877175906808,10.));
#29881=CARTESIAN_POINT('Ctrl Pts',(94.1973028564882,25.3192980131866,10.));
#29882=CARTESIAN_POINT('Ctrl Pts',(94.2465138207336,25.2483314405892,10.));
#29883=CARTESIAN_POINT('Ctrl Pts',(94.2970863146417,25.1754014215296,10.));
#29884=CARTESIAN_POINT('Ctrl Pts',(94.3438891300174,25.0997809660001,10.));
#29885=CARTESIAN_POINT('Ctrl Pts',(94.3868632217433,25.0218260241029,10.));
#29886=CARTESIAN_POINT('Ctrl Pts',(94.4057547014815,24.9875569064508,10.));
#29887=CARTESIAN_POINT('Ctrl Pts',(94.4239057978348,24.9528361527832,10.));
#29888=CARTESIAN_POINT('Ctrl Pts',(94.4413090769948,24.9176919312935,10.));
#29889=CARTESIAN_POINT('Ctrl Pts',(94.4512341001083,24.8976493170607,10.));
#29890=CARTESIAN_POINT('Ctrl Pts',(94.4609158766235,24.8774689544396,10.));
#29891=CARTESIAN_POINT('Ctrl Pts',(94.4703527940363,24.8571559201793,10.));
#29892=CARTESIAN_POINT('Ctrl Pts',(94.4788698089046,24.8388229829234,10.));
#29893=CARTESIAN_POINT('Ctrl Pts',(94.48718975873,24.8203762304135,10.));
#29894=CARTESIAN_POINT('Ctrl Pts',(94.4952977634445,24.8018512256524,10.));
#29895=CARTESIAN_POINT('Ctrl Pts',(94.5318624413391,24.7183089910421,10.));
#29896=CARTESIAN_POINT('Ctrl Pts',(94.5641668037087,24.6330832595078,10.));
#29897=CARTESIAN_POINT('Ctrl Pts',(94.5921857513385,24.5465727477908,10.));
#29898=CARTESIAN_POINT('Ctrl Pts',(94.6206673939169,24.4586336322127,10.));
#29899=CARTESIAN_POINT('Ctrl Pts',(94.6447214108873,24.3693661982349,10.));
#29900=CARTESIAN_POINT('Ctrl Pts',(94.6642823633474,24.279152120929,10.));
#29901=CARTESIAN_POINT('Ctrl Pts',(94.683262749204,24.1916155860673,10.));
#29902=CARTESIAN_POINT('Ctrl Pts',(94.6980129804155,24.1031868495632,10.));
#29903=CARTESIAN_POINT('Ctrl Pts',(94.7084324536937,24.0141926985119,10.));
#29904=CARTESIAN_POINT('Ctrl Pts',(94.7127917941012,23.976958973894,10.));
#29905=CARTESIAN_POINT('Ctrl Pts',(94.7163925414667,23.9396260845753,10.));
#29906=CARTESIAN_POINT('Ctrl Pts',(94.7192250066991,23.9022173486862,10.));
#29907=CARTESIAN_POINT('Ctrl Pts',(94.7209955764803,23.8788332038215,10.));
#29908=CARTESIAN_POINT('Ctrl Pts',(94.7224659134476,23.8554194166543,10.));
#29909=CARTESIAN_POINT('Ctrl Pts',(94.7236333606835,23.8319816504978,10.));
#29910=CARTESIAN_POINT('Ctrl Pts',(94.724317620347,23.818244397549,10.));
#29911=CARTESIAN_POINT('Ctrl Pts',(94.7248975539046,23.8045034755981,10.));
#29912=CARTESIAN_POINT('Ctrl Pts',(94.7253726391635,23.7907682591662,10.));
#29913=CARTESIAN_POINT('Ctrl Pts',(94.7287304225261,23.6936911969805,10.));
#29914=CARTESIAN_POINT('Ctrl Pts',(94.7268610241325,23.596778684182,10.));
#29915=CARTESIAN_POINT('Ctrl Pts',(94.7196996503297,23.5004529825499,10.));
#29916=CARTESIAN_POINT('Ctrl Pts',(94.7125382765269,23.4041272809177,10.));
#29917=CARTESIAN_POINT('Ctrl Pts',(94.7000853621774,23.3083873359331,10.));
#29918=CARTESIAN_POINT('Ctrl Pts',(94.6822232210626,23.2136364705516,10.));
#29919=CARTESIAN_POINT('Ctrl Pts',(94.6651456877563,23.12304760727,10.));
#29920=CARTESIAN_POINT('Ctrl Pts',(94.6431238131852,23.0333618679134,10.));
#29921=CARTESIAN_POINT('Ctrl Pts',(94.6164322917056,22.9448185902262,10.));
#29922=CARTESIAN_POINT('Ctrl Pts',(94.6074974122224,22.9151790840711,10.));
#29923=CARTESIAN_POINT('Ctrl Pts',(94.5980388404184,22.885667632781,10.));
#29924=CARTESIAN_POINT('Ctrl Pts',(94.588065604527,22.8562933928181,10.));
#29925=CARTESIAN_POINT('Ctrl Pts',(94.5815842777681,22.8372038967343,10.));
#29926=CARTESIAN_POINT('Ctrl Pts',(94.5748855784168,22.8181723520541,10.));
#29927=CARTESIAN_POINT('Ctrl Pts',(94.5679718479818,22.7992013069027,10.));
#29928=CARTESIAN_POINT('Ctrl Pts',(94.5613824030787,22.7811200904081,10.));
#29929=CARTESIAN_POINT('Ctrl Pts',(94.5545958744184,22.7630896215814,10.));
#29930=CARTESIAN_POINT('Ctrl Pts',(94.5476250811124,22.7451392560728,10.));
#29931=CARTESIAN_POINT('Ctrl Pts',(94.5137816042513,22.6579895224528,10.));
#29932=CARTESIAN_POINT('Ctrl Pts',(94.4755597867714,22.5726140967881,10.));
#29933=CARTESIAN_POINT('Ctrl Pts',(94.4332908111416,22.4892465922063,10.));
#29934=CARTESIAN_POINT('Ctrl Pts',(94.3894525927547,22.4027840551381,10.));
#29935=CARTESIAN_POINT('Ctrl Pts',(94.3412610125979,22.3184805709375,10.));
#29936=CARTESIAN_POINT('Ctrl Pts',(94.2890295505398,22.2365997560127,10.));
#29937=CARTESIAN_POINT('Ctrl Pts',(94.2362096760877,22.1537965145573,10.));
#29938=CARTESIAN_POINT('Ctrl Pts',(94.1792579755655,22.0734700151482,10.));
#29939=CARTESIAN_POINT('Ctrl Pts',(94.1184468579888,21.9959077298342,10.));
#29940=CARTESIAN_POINT('Ctrl Pts',(94.0767843459049,21.9427687681127,10.));
#29941=CARTESIAN_POINT('Ctrl Pts',(94.0333092171587,21.8909275801965,10.));
#29942=CARTESIAN_POINT('Ctrl Pts',(93.9880968596546,21.8404836536314,10.));
#29943=CARTESIAN_POINT('Ctrl Pts',(93.9759899524546,21.8269758435669,10.));
#29944=CARTESIAN_POINT('Ctrl Pts',(93.9637571446612,21.8135670091799,10.));
#29945=CARTESIAN_POINT('Ctrl Pts',(93.951413501835,21.8002735576985,10.));
#29946=CARTESIAN_POINT('Ctrl Pts',(93.882752721598,21.7263295232182,10.));
#29947=CARTESIAN_POINT('Ctrl Pts',(93.810578049503,21.6558533764537,10.));
#29948=CARTESIAN_POINT('Ctrl Pts',(93.7351999444248,21.5891349259443,10.));
#29949=CARTESIAN_POINT('Ctrl Pts',(93.6722950971385,21.5334567693214,10.));
#29950=CARTESIAN_POINT('Ctrl Pts',(93.6071581999104,21.4803955991654,10.));
#29951=CARTESIAN_POINT('Ctrl Pts',(93.5399460223894,21.4301336195356,10.));
#29952=CARTESIAN_POINT('Ctrl Pts',(93.5180637926007,21.4137698558775,10.));
#29953=CARTESIAN_POINT('Ctrl Pts',(93.4959614384794,21.3977029162792,10.));
#29954=CARTESIAN_POINT('Ctrl Pts',(93.4736439440714,21.3819394740093,10.));
#29955=CARTESIAN_POINT('Ctrl Pts',(93.4508750631855,21.3658572054161,10.));
#29956=CARTESIAN_POINT('Ctrl Pts',(93.4278768370864,21.3500874072995,10.));
#29957=CARTESIAN_POINT('Ctrl Pts',(93.4046836949952,21.3346563933178,10.));
#29958=CARTESIAN_POINT('Ctrl Pts',(93.3197384270806,21.2781400484554,10.));
#29959=CARTESIAN_POINT('Ctrl Pts',(93.2321268832175,21.226124130751,10.));
#29960=CARTESIAN_POINT('Ctrl Pts',(93.1421393261376,21.1789167035699,10.));
#29961=CARTESIAN_POINT('Ctrl Pts',(93.0588657605654,21.1352314329567,10.));
#29962=CARTESIAN_POINT('Ctrl Pts',(92.9735566878419,21.0956636399515,10.));
#29963=CARTESIAN_POINT('Ctrl Pts',(92.8864147107142,21.0604862982088,10.));
#29964=CARTESIAN_POINT('Ctrl Pts',(92.856390770472,21.048366279348,10.));
#29965=CARTESIAN_POINT('Ctrl Pts',(92.8261490486008,21.0367677258533,10.));
#29966=CARTESIAN_POINT('Ctrl Pts',(92.7957019287907,21.0256870573369,10.));
#29967=CARTESIAN_POINT('Ctrl Pts',(89.481789046694,23.9978055657336,8.38741669750803));
#29968=CARTESIAN_POINT('Ctrl Pts',(89.480223059461,23.8252749393967,8.39833391417657));
#29969=CARTESIAN_POINT('Ctrl Pts',(89.4964590311695,23.6530372319079,8.40925113084511));
#29970=CARTESIAN_POINT('Ctrl Pts',(89.5315885963512,23.4847435435215,8.42016834751366));
#29971=CARTESIAN_POINT('Ctrl Pts',(89.7010420406894,22.67295025744,8.47282940259653));
#29972=CARTESIAN_POINT('Ctrl Pts',(90.3101077692311,21.9529256044114,8.52549045767941));
#29973=CARTESIAN_POINT('Ctrl Pts',(91.0825656196773,21.6512032537229,8.57815151276229));
#29974=CARTESIAN_POINT('Ctrl Pts',(91.8550234701235,21.3494809030344,8.63081256784517));
#29975=CARTESIAN_POINT('Ctrl Pts',(92.7908734424743,21.4660608546861,8.68347362292805));
#29976=CARTESIAN_POINT('Ctrl Pts',(93.4656884574097,21.9480921266005,8.73613467801093));
#29977=CARTESIAN_POINT('Ctrl Pts',(94.1405034723451,22.4301233985148,8.78879573309381));
#29978=CARTESIAN_POINT('Ctrl Pts',(94.5542835298652,23.2776059906917,8.84145678817668));
#29979=CARTESIAN_POINT('Ctrl Pts',(94.5193787375631,24.1061511997237,8.89411784325956));
#29980=CARTESIAN_POINT('Ctrl Pts',(94.4844739452609,24.9346964087557,8.94677889834243));
#29981=CARTESIAN_POINT('Ctrl Pts',(94.0008843031365,25.7443042346427,8.99943995342532));
#29982=CARTESIAN_POINT('Ctrl Pts',(93.2879128423749,26.1678872245111,9.0521010085082));
#29983=CARTESIAN_POINT('Ctrl Pts',(92.5749413816133,26.5914702143796,9.10476206359107));
#29984=CARTESIAN_POINT('Ctrl Pts',(91.6325881022146,26.6290283682294,9.15742311867395));
#29985=CARTESIAN_POINT('Ctrl Pts',(90.8882531044733,26.2633578291731,9.21008417375683));
#29986=CARTESIAN_POINT('Ctrl Pts',(90.1439181067321,25.8976872901167,9.2627452288397));
#29987=CARTESIAN_POINT('Ctrl Pts',(89.5976013906482,25.1287880581541,9.31540628392258));
#29988=CARTESIAN_POINT('Ctrl Pts',(89.4970121613135,24.3057175721558,9.36806733900546));
#29989=CARTESIAN_POINT('Ctrl Pts',(89.484692259653,24.2049100849695,9.37451712517298));
#29990=CARTESIAN_POINT('Ctrl Pts',(89.4790585822288,24.1032899910618,9.3809669113405));
#29991=CARTESIAN_POINT('Ctrl Pts',(89.4798237559162,24.0015869167785,9.38741669750802));
#29992=CARTESIAN_POINT('Ctrl Pts',(91.2062007174671,21.0307770462543,10.));
#29993=CARTESIAN_POINT('Ctrl Pts',(90.2237466982397,21.2934286920664,9.94733894491712));
#29994=CARTESIAN_POINT('Ctrl Pts',(88.5566850319539,22.8666986268703,9.84201683475137));
#29995=CARTESIAN_POINT('Ctrl Pts',(89.1687764925373,26.2698561140492,9.68403366950273));
#29996=CARTESIAN_POINT('Ctrl Pts',(92.3539160756187,27.6088391884301,9.5260505042541));
#29997=CARTESIAN_POINT('Ctrl Pts',(95.2156041936735,25.6770751085581,9.36806733900546));
#29998=CARTESIAN_POINT('Ctrl Pts',(95.1618224985938,22.2228835192268,9.21008417375683));
#29999=CARTESIAN_POINT('Ctrl Pts',(92.2395757642924,20.3812156575975,9.05210100850819));
#30000=CARTESIAN_POINT('Ctrl Pts',(89.1003116800245,21.8216058830164,8.89411784325956));
#30001=CARTESIAN_POINT('Ctrl Pts',(88.5910237941293,25.238022224588,8.73613467801092));
#30002=CARTESIAN_POINT('Ctrl Pts',(91.1738622820844,27.531437528054,8.57815151276229));
#30003=CARTESIAN_POINT('Ctrl Pts',(94.5060022838614,26.6217540231211,8.42016834751365));
#30004=CARTESIAN_POINT('Ctrl Pts',(95.5651291305171,23.3340327163824,8.26218518226502));
#30005=CARTESIAN_POINT('Ctrl Pts',(93.3905541137143,20.6503749960184,8.10420201701639));
#30006=CARTESIAN_POINT('Ctrl Pts',(89.9547029986071,21.0049373072501,7.94621885176775));
#30007=CARTESIAN_POINT('Ctrl Pts',(88.3740041419999,24.0761257542051,7.78823568651913));
#30008=CARTESIAN_POINT('Ctrl Pts',(90.0822082378052,27.0782645420543,7.63025252127047));
#30009=CARTESIAN_POINT('Ctrl Pts',(93.5299144568995,27.2883128130434,7.47226935602186));
#30010=CARTESIAN_POINT('Ctrl Pts',(95.5899362712428,24.5157488852068,7.31428619077321));
#30011=CARTESIAN_POINT('Ctrl Pts',(94.3937632442239,21.2753832325168,7.15630302552458));
#30012=CARTESIAN_POINT('Ctrl Pts',(91.0263653048422,20.5063379273329,6.99831986027594));
#30013=CARTESIAN_POINT('Ctrl Pts',(88.542087239558,22.9061633964473,6.84033669502731));
#30014=CARTESIAN_POINT('Ctrl Pts',(89.1942540870206,26.2981359861554,6.68235352977868));
#30015=CARTESIAN_POINT('Ctrl Pts',(92.3913282372869,27.6056208028793,6.52437036453004));
#30016=CARTESIAN_POINT('Ctrl Pts',(95.2334543225921,25.6426844805108,6.36638719928141));
#30017=CARTESIAN_POINT('Ctrl Pts',(95.1427269710462,22.1897772675992,6.20840403403277));
#30018=CARTESIAN_POINT('Ctrl Pts',(92.2014389895034,20.3788038589624,6.05042086878414));
#30019=CARTESIAN_POINT('Ctrl Pts',(89.0774389685691,21.8523789498236,5.89243770353551));
#30020=CARTESIAN_POINT('Ctrl Pts',(88.6043015565952,25.2739196359127,5.73445453828687));
#30021=CARTESIAN_POINT('Ctrl Pts',(91.2111785351691,27.5399717307178,5.57647137303823));
#30022=CARTESIAN_POINT('Ctrl Pts',(94.533543506554,26.5951486388853,5.41848820778961));
#30023=CARTESIAN_POINT('Ctrl Pts',(95.5578980422049,23.2964371536349,5.26050504254096));
#30024=CARTESIAN_POINT('Ctrl Pts',(93.3551176148942,20.6358811841045,5.10252187729233));
#30025=CARTESIAN_POINT('Ctrl Pts',(89.9231992578103,21.0266958052455,4.9445387120437));
#30026=CARTESIAN_POINT('Ctrl Pts',(88.3750100595362,24.1143988161452,4.78655554679507));
#30027=CARTESIAN_POINT('Ctrl Pts',(90.1148104659794,27.0983381963848,4.62857238154643));
#30028=CARTESIAN_POINT('Ctrl Pts',(93.5645421252575,27.2719790790494,4.4705892162978));
#30029=CARTESIAN_POINT('Ctrl Pts',(95.5951806759186,24.4778232584366,4.31260605104916));
#30030=CARTESIAN_POINT('Ctrl Pts',(94.3648676419543,21.2502654310841,4.15462288580052));
#30031=CARTESIAN_POINT('Ctrl Pts',(90.9895389394379,20.5168107165773,3.99663972055189));
#30032=CARTESIAN_POINT('Ctrl Pts',(88.530732906619,22.9427275616555,3.83865655530326));
#30033=CARTESIAN_POINT('Ctrl Pts',(89.2186705439483,26.3276266140658,3.68067339005462));
#30034=CARTESIAN_POINT('Ctrl Pts',(92.4293689246723,27.6012888422859,3.52269022480599));
#30035=CARTESIAN_POINT('Ctrl Pts',(95.2506150476497,25.6084592491483,3.36470705955735));
#30036=CARTESIAN_POINT('Ctrl Pts',(95.1234423470095,22.1567020569745,3.20672389430872));
#30037=CARTESIAN_POINT('Ctrl Pts',(92.1632008787758,20.3768793413443,3.04874072906008));
#30038=CARTESIAN_POINT('Ctrl Pts',(89.0549305391036,21.8833500612562,2.89075756381145));
#30039=CARTESIAN_POINT('Ctrl Pts',(88.617938934352,25.309695882881,2.73277439856282));
#30040=CARTESIAN_POINT('Ctrl Pts',(91.2485917195107,27.5481000558719,2.57479123331418));
#30041=CARTESIAN_POINT('Ctrl Pts',(94.5607983477153,26.5682620509694,2.41680806806555));
#30042=CARTESIAN_POINT('Ctrl Pts',(95.5502716608786,23.2589111130017,2.25882490281691));
#30043=CARTESIAN_POINT('Ctrl Pts',(93.3195310914442,20.621776762524,2.10084173756828));
#30044=CARTESIAN_POINT('Ctrl Pts',(89.8919232441541,21.0487578560498,1.94285857231964));
#30045=CARTESIAN_POINT('Ctrl Pts',(88.3764283632659,24.1527150135632,1.78487540707101));
#30046=CARTESIAN_POINT('Ctrl Pts',(90.1476051992024,27.1179528805983,1.62689224182238));
#30047=CARTESIAN_POINT('Ctrl Pts',(93.5990315417431,27.2555126520044,1.46890907657374));
#30048=CARTESIAN_POINT('Ctrl Pts',(95.5999506290772,24.4393708209746,1.3109259113251));
#30049=CARTESIAN_POINT('Ctrl Pts',(94.3358592338276,21.2264213520667,1.15294274607647));
#30050=CARTESIAN_POINT('Ctrl Pts',(90.9525239108494,20.5256846472501,0.994959580827838));
#30051=CARTESIAN_POINT('Ctrl Pts',(88.5204084922262,22.9835193506337,0.836976415579203));
#30052=CARTESIAN_POINT('Ctrl Pts',(89.0030718657857,25.2243470893904,0.731654305413447));
#30053=CARTESIAN_POINT('Ctrl Pts',(89.6639373423039,25.9973015569306,0.678993250330568));
#30054=CARTESIAN_POINT('Ctrl Pts',(91.254067145653,21.2098224301579,10.1070022498898));
#30055=CARTESIAN_POINT('Ctrl Pts',(90.3308555140066,21.4566360720578,10.0543411948069));
#30056=CARTESIAN_POINT('Ctrl Pts',(88.7643183622759,22.9350371728776,9.94901908464117));
#30057=CARTESIAN_POINT('Ctrl Pts',(89.3395004522086,26.1329828425985,9.79103591939254));
#30058=CARTESIAN_POINT('Ctrl Pts',(92.3325747884819,27.3912246785047,9.6330527541439));
#30059=CARTESIAN_POINT('Ctrl Pts',(95.0217019181265,25.575946779253,9.47506958889527));
#30060=CARTESIAN_POINT('Ctrl Pts',(94.9711632817164,22.3300443850486,9.31708642364663));
#30061=CARTESIAN_POINT('Ctrl Pts',(92.2251292456713,20.59942986446,9.15910325839801));
#30062=CARTESIAN_POINT('Ctrl Pts',(89.2751640964777,21.9529639578543,9.00112009314937));
#30063=CARTESIAN_POINT('Ctrl Pts',(88.7965864827541,25.1633689675118,8.84313692790073));
#30064=CARTESIAN_POINT('Ctrl Pts',(91.2236787314268,27.3184903705682,8.6851537626521));
#30065=CARTESIAN_POINT('Ctrl Pts',(94.3548892997688,26.4636611608191,8.52717059740346));
#30066=CARTESIAN_POINT('Ctrl Pts',(95.3501503553349,23.3741908216578,8.36918743215484));
#30067=CARTESIAN_POINT('Ctrl Pts',(93.3067031200343,20.8523587823872,8.21120426690619));
#30068=CARTESIAN_POINT('Ctrl Pts',(90.0780352618006,21.1855408382049,8.05322110165756));
#30069=CARTESIAN_POINT('Ctrl Pts',(88.5926532062641,24.0715353394404,7.89523793640892));
#30070=CARTESIAN_POINT('Ctrl Pts',(90.1978518818355,26.8926439048457,7.73725477116029));
#30071=CARTESIAN_POINT('Ctrl Pts',(93.4376599763359,27.0900261773889,7.57927160591167));
#30072=CARTESIAN_POINT('Ctrl Pts',(95.3734616151168,24.484649012079,7.42128844066302));
#30073=CARTESIAN_POINT('Ctrl Pts',(94.2494183210864,21.439678761254,7.26330527541439));
#30074=CARTESIAN_POINT('Ctrl Pts',(91.0850758834994,20.7170072090858,7.10532211016575));
#30075=CARTESIAN_POINT('Ctrl Pts',(88.7506008228567,22.9721222003706,6.94733894491712));
#30076=CARTESIAN_POINT('Ctrl Pts',(89.3634417371065,26.1595574266085,6.78935577966849));
#30077=CARTESIAN_POINT('Ctrl Pts',(92.3677309811802,27.3882003629464,6.63137261441985));
#30078=CARTESIAN_POINT('Ctrl Pts',(95.038475676818,25.5436299204366,6.47338944917122));
#30079=CARTESIAN_POINT('Ctrl Pts',(94.9532192224532,22.2989344542176,6.31540628392258));
#30080=CARTESIAN_POINT('Ctrl Pts',(92.1892921343259,20.5971634982897,6.15742311867395));
#30081=CARTESIAN_POINT('Ctrl Pts',(89.2536706190735,21.9818813958838,5.99943995342532));
#30082=CARTESIAN_POINT('Ctrl Pts',(88.8090635905991,25.1971017499447,5.84145678817668));
#30083=CARTESIAN_POINT('Ctrl Pts',(91.258744798869,27.3265099572479,5.68347362292805));
#30084=CARTESIAN_POINT('Ctrl Pts',(94.3807697752332,26.4386600923617,5.52549045767941));
#30085=CARTESIAN_POINT('Ctrl Pts',(95.3433553046672,23.3388622870419,5.36750729243078));
#30086=CARTESIAN_POINT('Ctrl Pts',(93.2734034568898,20.8387389533836,5.20952412718214));
#30087=CARTESIAN_POINT('Ctrl Pts',(90.048431209728,21.2059872896859,5.05154096193352));
#30088=CARTESIAN_POINT('Ctrl Pts',(88.5935984665529,24.1075005197647,4.89355779668487));
#30089=CARTESIAN_POINT('Ctrl Pts',(90.2284881820376,26.9115071094383,4.73557463143624));
#30090=CARTESIAN_POINT('Ctrl Pts',(93.4701995818332,27.0746773743749,4.5775914661876));
#30091=CARTESIAN_POINT('Ctrl Pts',(95.3783897800006,24.4490103164388,4.41960830093897));
#30092=CARTESIAN_POINT('Ctrl Pts',(94.2222651356991,21.4160755737355,4.26162513569033));
#30093=CARTESIAN_POINT('Ctrl Pts',(91.0504701633057,20.7268484847659,4.10364197044171));
#30094=CARTESIAN_POINT('Ctrl Pts',(88.7399311609349,23.0064815311496,3.94565880519306));
#30095=CARTESIAN_POINT('Ctrl Pts',(89.3863858714864,26.1872697573421,3.78767563994444));
#30096=CARTESIAN_POINT('Ctrl Pts',(92.4034777992323,27.3841296213857,3.6296924746958));
#30097=CARTESIAN_POINT('Ctrl Pts',(95.0546016029891,25.5114684848159,3.47170930944717));
#30098=CARTESIAN_POINT('Ctrl Pts',(94.9350974692982,22.2678536926041,3.31372614419853));
#30099=CARTESIAN_POINT('Ctrl Pts',(92.1533597976414,20.5953550298875,3.1557429789499));
#30100=CARTESIAN_POINT('Ctrl Pts',(89.2325194573032,22.0109849363651,2.99775981370126));
#30101=CARTESIAN_POINT('Ctrl Pts',(88.8218786287828,25.2307206742826,2.83977664845263));
#30102=CARTESIAN_POINT('Ctrl Pts',(91.2939019525732,27.3341481410013,2.68179348320399));
#30103=CARTESIAN_POINT('Ctrl Pts',(94.4063811380922,26.4133947769236,2.52381031795536));
#30104=CARTESIAN_POINT('Ctrl Pts',(95.3361887973194,23.3035990823278,2.36582715270672));
#30105=CARTESIAN_POINT('Ctrl Pts',(93.2399628156628,20.8254850343137,2.20784398745809));
#30106=CARTESIAN_POINT('Ctrl Pts',(90.0190411527545,21.2267189896148,2.04986082220946));
#30107=CARTESIAN_POINT('Ctrl Pts',(88.5949312459757,24.1435062344795,1.89187765696082));
#30108=CARTESIAN_POINT('Ctrl Pts',(90.2593053791538,26.9299390200037,1.73389449171219));
#30109=CARTESIAN_POINT('Ctrl Pts',(93.5026092721039,27.0592038797562,1.57591132646355));
#30110=CARTESIAN_POINT('Ctrl Pts',(95.382872102992,24.4128765770115,1.41792816121492));
#30111=CARTESIAN_POINT('Ctrl Pts',(94.1950059466948,21.3936693026389,1.25994499596628));
#30112=CARTESIAN_POINT('Ctrl Pts',(91.0156871563966,20.7351873137138,1.10196183071765));
#30113=CARTESIAN_POINT('Ctrl Pts',(88.7302293130409,23.0448135582198,0.943978665469014));
#30114=CARTESIAN_POINT('Ctrl Pts',(89.1837878836397,25.1505184486767,0.838656555303258));
#30115=CARTESIAN_POINT('Ctrl Pts',(89.8048028959809,25.8768634390787,0.785995500220379));
#30116=CARTESIAN_POINT('Ctrl Pts',(91.301933573839,21.3888678140614,10.2140044997796));
#30117=CARTESIAN_POINT('Ctrl Pts',(90.4379643297735,21.6198434520493,10.1613434446967));
#30118=CARTESIAN_POINT('Ctrl Pts',(88.9719516925979,23.0033757188848,10.056021334531));
#30119=CARTESIAN_POINT('Ctrl Pts',(89.5102244118798,25.9961095711478,9.89803816928235));
#30120=CARTESIAN_POINT('Ctrl Pts',(92.3112335013454,27.1736101685792,9.74005500403371));
#30121=CARTESIAN_POINT('Ctrl Pts',(94.8277996425791,25.4748184499478,9.58207183878508));
#30122=CARTESIAN_POINT('Ctrl Pts',(94.7805040648391,22.4372052508704,9.42408867353645));
#30123=CARTESIAN_POINT('Ctrl Pts',(92.2106827270499,20.8176440713226,9.26610550828781));
#30124=CARTESIAN_POINT('Ctrl Pts',(89.4500165129309,22.0843220326922,9.10812234303918));
#30125=CARTESIAN_POINT('Ctrl Pts',(89.0021491713788,25.0887157104356,8.95013917779055));
#30126=CARTESIAN_POINT('Ctrl Pts',(91.273495180769,27.1055432130824,8.79215601254192));
#30127=CARTESIAN_POINT('Ctrl Pts',(94.2037763156761,26.3055682985171,8.63417284729327));
#30128=CARTESIAN_POINT('Ctrl Pts',(95.1351715801526,23.4143489269332,8.47618968204465));
#30129=CARTESIAN_POINT('Ctrl Pts',(93.2228521263546,21.0543425687561,8.31820651679601));
#30130=CARTESIAN_POINT('Ctrl Pts',(90.2013675249939,21.3661443691598,8.16022335154737));
#30131=CARTESIAN_POINT('Ctrl Pts',(88.8113022705282,24.0669449246757,8.00224018629874));
#30132=CARTESIAN_POINT('Ctrl Pts',(90.3134955258656,26.707023267637,7.84425702105011));
#30133=CARTESIAN_POINT('Ctrl Pts',(93.3454054957724,26.8917395417344,7.68627385580147));
#30134=CARTESIAN_POINT('Ctrl Pts',(95.1569869589906,24.4535491389512,7.52829069055285));
#30135=CARTESIAN_POINT('Ctrl Pts',(94.105073397949,21.6039742899911,7.37030752530419));
#30136=CARTESIAN_POINT('Ctrl Pts',(91.1437864621564,20.9276764908387,7.21232436005558));
#30137=CARTESIAN_POINT('Ctrl Pts',(88.9591144061554,23.038081004294,7.05434119480692));
#30138=CARTESIAN_POINT('Ctrl Pts',(89.5326293871924,26.0209788670616,6.89635802955831));
#30139=CARTESIAN_POINT('Ctrl Pts',(92.3441337250735,27.1707799230136,6.73837486430966));
#30140=CARTESIAN_POINT('Ctrl Pts',(94.8434970310438,25.4445753603624,6.58039169906103));
#30141=CARTESIAN_POINT('Ctrl Pts',(94.7637114738601,22.408091640836,6.4224085338124));
#30142=CARTESIAN_POINT('Ctrl Pts',(92.1771452791484,20.8155231376169,6.26442536856376));
#30143=CARTESIAN_POINT('Ctrl Pts',(89.4299022695779,22.111383841944,6.10644220331513));
#30144=CARTESIAN_POINT('Ctrl Pts',(89.013825624603,25.1202838639768,5.94845903806649));
#30145=CARTESIAN_POINT('Ctrl Pts',(91.3063110625691,27.113048183778,5.79047587281786));
#30146=CARTESIAN_POINT('Ctrl Pts',(94.2279960439123,26.2821715458382,5.63249270756923));
#30147=CARTESIAN_POINT('Ctrl Pts',(95.1288125671295,23.3812874204489,5.47450954232059));
#30148=CARTESIAN_POINT('Ctrl Pts',(93.1916892988852,21.0415967226627,5.31652637707195));
#30149=CARTESIAN_POINT('Ctrl Pts',(90.1736631616457,21.3852787741264,5.15854321182332));
#30150=CARTESIAN_POINT('Ctrl Pts',(88.8121868735697,24.1006022233841,5.00056004657469));
#30151=CARTESIAN_POINT('Ctrl Pts',(90.3421658980959,26.7246760224918,4.84257688132605));
#30152=CARTESIAN_POINT('Ctrl Pts',(93.375857038409,26.8773756697003,4.68459371607742));
#30153=CARTESIAN_POINT('Ctrl Pts',(95.1615988840827,24.420197374441,4.52661055082878));
#30154=CARTESIAN_POINT('Ctrl Pts',(94.0796626294438,21.5818857163869,4.36862738558015));
#30155=CARTESIAN_POINT('Ctrl Pts',(91.1114013871734,20.9368862529545,4.21064422033151));
#30156=CARTESIAN_POINT('Ctrl Pts',(88.9491294152508,23.0702355006436,4.05266105508288));
#30157=CARTESIAN_POINT('Ctrl Pts',(89.5541011990245,26.0469129006185,3.89467788983424));
#30158=CARTESIAN_POINT('Ctrl Pts',(92.3775866737925,27.1669704004854,3.73669472458561));
#30159=CARTESIAN_POINT('Ctrl Pts',(94.8585881583285,25.4144777204836,3.57871155933698));
#30160=CARTESIAN_POINT('Ctrl Pts',(94.746752591587,22.3790053282336,3.42072839408834));
#30161=CARTESIAN_POINT('Ctrl Pts',(92.1435187165069,20.8138307184307,3.26274522883971));
#30162=CARTESIAN_POINT('Ctrl Pts',(89.4101083755027,22.138619811474,3.10476206359107));
#30163=CARTESIAN_POINT('Ctrl Pts',(89.0258183232137,25.1517454656841,2.94677889834244));
#30164=CARTESIAN_POINT('Ctrl Pts',(91.3392121856356,27.1201962261306,2.7887957330938));
#30165=CARTESIAN_POINT('Ctrl Pts',(94.2519639284692,26.2585275028778,2.63081256784517));
#30166=CARTESIAN_POINT('Ctrl Pts',(95.12210593376,23.3482870516539,2.47282940259653));
#30167=CARTESIAN_POINT('Ctrl Pts',(93.1603945398814,21.0291933061033,2.3148462373479));
#30168=CARTESIAN_POINT('Ctrl Pts',(90.146159061355,21.4046801231798,2.15686307209927));
#30169=CARTESIAN_POINT('Ctrl Pts',(88.8134341286852,24.1342974553958,1.99887990685063));
#30170=CARTESIAN_POINT('Ctrl Pts',(90.3710055591055,26.7419251594091,1.840896741602));
#30171=CARTESIAN_POINT('Ctrl Pts',(93.4061870024645,26.862895107508,1.68291357635336));
#30172=CARTESIAN_POINT('Ctrl Pts',(95.1657935769071,24.3863823330484,1.52493041110473));
#30173=CARTESIAN_POINT('Ctrl Pts',(94.054152659562,21.560917253211,1.36694724585609));
#30174=CARTESIAN_POINT('Ctrl Pts',(91.0788504019437,20.9446899801776,1.20896408060746));
#30175=CARTESIAN_POINT('Ctrl Pts',(88.9400501338556,23.1061077658059,1.05098091535882));
#30176=CARTESIAN_POINT('Ctrl Pts',(89.3645039014938,25.0766898079629,0.945658805193069));
#30177=CARTESIAN_POINT('Ctrl Pts',(89.9456684496579,25.7564253212268,0.89299775011019));
#30178=CARTESIAN_POINT('Ctrl Pts',(91.3498000020249,21.5679131979649,10.3210067496694));
#30179=CARTESIAN_POINT('Ctrl Pts',(90.5450731455404,21.7830508320407,10.2683456945866));
#30180=CARTESIAN_POINT('Ctrl Pts',(89.1795850229198,23.0717142648921,10.1630235844208));
#30181=CARTESIAN_POINT('Ctrl Pts',(89.6809483715512,25.8592362996971,10.0050404191722));
#30182=CARTESIAN_POINT('Ctrl Pts',(92.2898922142085,26.9559956586539,9.84705725392353));
#30183=CARTESIAN_POINT('Ctrl Pts',(94.6338973670321,25.3736901206426,9.68907408867489));
#30184=CARTESIAN_POINT('Ctrl Pts',(94.5898448479616,22.5443661166922,9.53109092342627));
#30185=CARTESIAN_POINT('Ctrl Pts',(92.1962362084289,21.035858278185,9.37310775817761));
#30186=CARTESIAN_POINT('Ctrl Pts',(89.624868929384,22.2156801075302,9.21512459292901));
#30187=CARTESIAN_POINT('Ctrl Pts',(89.2077118600035,25.0140624533594,9.05714142768035));
#30188=CARTESIAN_POINT('Ctrl Pts',(91.3233116301113,26.8925960555965,8.89915826243173));
#30189=CARTESIAN_POINT('Ctrl Pts',(94.0526633315834,26.1474754362151,8.74117509718308));
#30190=CARTESIAN_POINT('Ctrl Pts',(94.9201928049705,23.4545070322085,8.58319193193445));
#30191=CARTESIAN_POINT('Ctrl Pts',(93.1390011326746,21.2563263551249,8.42520876668582));
#30192=CARTESIAN_POINT('Ctrl Pts',(90.3246997881873,21.5467479001146,8.26722560143718));
#30193=CARTESIAN_POINT('Ctrl Pts',(89.0299513347925,24.0623545099109,8.10924243618856));
#30194=CARTESIAN_POINT('Ctrl Pts',(90.4291391698957,26.5214026304284,7.9512592709399));
#30195=CARTESIAN_POINT('Ctrl Pts',(93.2531510152089,26.6934529060799,7.79327610569129));
#30196=CARTESIAN_POINT('Ctrl Pts',(94.9405123028644,24.4224492658234,7.63529294044264));
#30197=CARTESIAN_POINT('Ctrl Pts',(93.9607284748116,21.7682698187282,7.47730977519402));
#30198=CARTESIAN_POINT('Ctrl Pts',(91.2024970408135,21.1383457725917,7.31932660994538));
#30199=CARTESIAN_POINT('Ctrl Pts',(89.1676279894541,23.1040398082173,7.16134344469674));
#30200=CARTESIAN_POINT('Ctrl Pts',(89.7018170372782,25.8824003075147,7.00336027944811));
#30201=CARTESIAN_POINT('Ctrl Pts',(92.3205364689669,26.9533594830807,6.84537711419947));
#30202=CARTESIAN_POINT('Ctrl Pts',(94.6485183852694,25.3455208002882,6.68739394895084));
#30203=CARTESIAN_POINT('Ctrl Pts',(94.5742037252673,22.5172488274544,6.5294107837022));
#30204=CARTESIAN_POINT('Ctrl Pts',(92.1649984239708,21.0338827769442,6.37142761845357));
#30205=CARTESIAN_POINT('Ctrl Pts',(89.6061339200824,22.2408862880042,6.21344445320493));
#30206=CARTESIAN_POINT('Ctrl Pts',(89.2185876586068,25.0434659780088,6.05546128795631));
#30207=CARTESIAN_POINT('Ctrl Pts',(91.3538773262692,26.8995864103081,5.89747812270766));
#30208=CARTESIAN_POINT('Ctrl Pts',(94.0752223125914,26.1256829993147,5.73949495745904));
#30209=CARTESIAN_POINT('Ctrl Pts',(94.914269829592,23.4237125538558,5.5815117922104));
#30210=CARTESIAN_POINT('Ctrl Pts',(93.1099751408806,21.2444544919418,5.42352862696176));
#30211=CARTESIAN_POINT('Ctrl Pts',(90.2988951135634,21.5645702585669,5.26554546171313));
#30212=CARTESIAN_POINT('Ctrl Pts',(89.0307752805864,24.0937039270036,5.10756229646449));
#30213=CARTESIAN_POINT('Ctrl Pts',(90.4558436141542,26.5378449355454,4.94957913121586));
#30214=CARTESIAN_POINT('Ctrl Pts',(93.2815144949848,26.6800739650258,4.79159596596723));
#30215=CARTESIAN_POINT('Ctrl Pts',(94.9448079881648,24.3913844324432,4.63361280071859));
#30216=CARTESIAN_POINT('Ctrl Pts',(93.9370601231887,21.7476958590383,4.47562963546996));
#30217=CARTESIAN_POINT('Ctrl Pts',(91.1723326110411,21.1469240211431,4.31764647022133));
#30218=CARTESIAN_POINT('Ctrl Pts',(89.1583276695668,23.1339894701376,4.15966330497269));
#30219=CARTESIAN_POINT('Ctrl Pts',(89.7218165265625,25.9065560438948,4.00168013972405));
#30220=CARTESIAN_POINT('Ctrl Pts',(92.3516955483528,26.9498111795851,3.84369697447543));
#30221=CARTESIAN_POINT('Ctrl Pts',(94.6625747136678,25.3174869561513,3.68571380922678));
#30222=CARTESIAN_POINT('Ctrl Pts',(94.5584077138757,22.4901569638631,3.52773064397815));
#30223=CARTESIAN_POINT('Ctrl Pts',(92.1336776353725,21.0323064069739,3.36974747872952));
#30224=CARTESIAN_POINT('Ctrl Pts',(89.5876972937022,22.2662546865829,3.21176431348088));
#30225=CARTESIAN_POINT('Ctrl Pts',(89.2297580176446,25.0727702570857,3.05378114823225));
#30226=CARTESIAN_POINT('Ctrl Pts',(91.3845224186981,26.90624431126,2.89579798298361));
#30227=CARTESIAN_POINT('Ctrl Pts',(94.097546718846,26.103660228832,2.73781481773498));
#30228=CARTESIAN_POINT('Ctrl Pts',(94.9080230702007,23.39297502098,2.57983165248635));
#30229=CARTESIAN_POINT('Ctrl Pts',(93.0808262640999,21.232901577893,2.42184848723771));
#30230=CARTESIAN_POINT('Ctrl Pts',(90.2732769699554,21.5826412567448,2.26386532198908));
#30231=CARTESIAN_POINT('Ctrl Pts',(89.0319370113948,24.1250886763121,2.10588215674044));
#30232=CARTESIAN_POINT('Ctrl Pts',(90.4827057390571,26.5539112988144,1.94789899149181));
#30233=CARTESIAN_POINT('Ctrl Pts',(93.3097647328252,26.6665863352599,1.78991582624318));
#30234=CARTESIAN_POINT('Ctrl Pts',(94.9487150508221,24.3598880890852,1.63193266099454));
#30235=CARTESIAN_POINT('Ctrl Pts',(93.9132993724291,21.7281652037832,1.47394949574591));
#30236=CARTESIAN_POINT('Ctrl Pts',(91.1420136474909,21.1541926466413,1.31596633049727));
#30237=CARTESIAN_POINT('Ctrl Pts',(89.1498709546703,23.167401973392,1.15798316524864));
#30238=CARTESIAN_POINT('Ctrl Pts',(89.5452199193478,25.0028611672492,1.05266105508288));
#30239=CARTESIAN_POINT('Ctrl Pts',(90.0865340033349,25.6359872033749,1.));
#30240=CARTESIAN_POINT('Ctrl Pts',(89.4850510509789,24.0017493960693,9.11258330249199));
#30241=CARTESIAN_POINT('Ctrl Pts',(89.4831440162074,24.294775221213,9.09410267755477));
#30242=CARTESIAN_POINT('Ctrl Pts',(89.5304974072669,24.5872051529597,9.07562205261756));
#30243=CARTESIAN_POINT('Ctrl Pts',(89.6298379999183,24.8607543294274,9.05714142768035));
#30244=CARTESIAN_POINT('Ctrl Pts',(89.9129117833728,25.6402403207718,9.00448037259747));
#30245=CARTESIAN_POINT('Ctrl Pts',(90.6181117067421,26.2664181881842,8.9518193175146));
#30246=CARTESIAN_POINT('Ctrl Pts',(91.425603618672,26.4553203519934,8.89915826243172));
#30247=CARTESIAN_POINT('Ctrl Pts',(92.233095530602,26.6442225158027,8.84649720734885));
#30248=CARTESIAN_POINT('Ctrl Pts',(93.1428794310927,26.3958489760089,8.79383615226596));
#30249=CARTESIAN_POINT('Ctrl Pts',(93.7423596269025,25.8228341387776,8.74117509718308));
#30250=CARTESIAN_POINT('Ctrl Pts',(94.3418398227124,25.2498193015463,8.6885140421002));
#30251=CARTESIAN_POINT('Ctrl Pts',(94.6310163138415,24.3521631668774,8.63585298701733));
#30252=CARTESIAN_POINT('Ctrl Pts',(94.47873928069,23.5369716533623,8.58319193193445));
#30253=CARTESIAN_POINT('Ctrl Pts',(94.3264622475385,22.7217801398473,8.53053087685158));
#30254=CARTESIAN_POINT('Ctrl Pts',(93.7327316901066,21.9890532474861,8.4778698217687));
#30255=CARTESIAN_POINT('Ctrl Pts',(92.9668161873094,21.6710933921371,8.42520876668582));
#30256=CARTESIAN_POINT('Ctrl Pts',(92.2009006845122,21.3531335367881,8.37254771160294));
#30257=CARTESIAN_POINT('Ctrl Pts',(91.2628002363497,21.4499407184514,8.31988665652006));
#30258=CARTESIAN_POINT('Ctrl Pts',(90.5779586033694,21.9176120775824,8.26722560143718));
#30259=CARTESIAN_POINT('Ctrl Pts',(89.9075993003969,22.3753936014113,8.21567816845545));
#30260=CARTESIAN_POINT('Ctrl Pts',(89.4799007520942,23.1885198389857,8.16413073547372));
#30261=CARTESIAN_POINT('Ctrl Pts',(89.4784369335473,24.0003195913806,8.11258330249199));
#30262=CARTESIAN_POINT('Ctrl Pts',(91.2062007174671,21.0307770462543,10.));
#30263=CARTESIAN_POINT('Ctrl Pts',(91.1131475235304,21.0648163202623,10.));
#30264=CARTESIAN_POINT('Ctrl Pts',(91.0221596064764,21.1036239095812,10.));
#30265=CARTESIAN_POINT('Ctrl Pts',(90.9334454653294,21.1468715855109,10.));
#30266=CARTESIAN_POINT('Ctrl Pts',(90.8427656611035,21.1910775118246,10.));
#30267=CARTESIAN_POINT('Ctrl Pts',(90.7544608424801,21.2399230814569,10.));
#30268=CARTESIAN_POINT('Ctrl Pts',(90.6687825963679,21.2931033001222,10.));
#30269=CARTESIAN_POINT('Ctrl Pts',(90.5863301108167,21.3442812993236,10.));
#30270=CARTESIAN_POINT('Ctrl Pts',(90.5063098561185,21.399474570675,10.));
#30271=CARTESIAN_POINT('Ctrl Pts',(90.4289790559023,21.4584413586066,10.));
#30272=CARTESIAN_POINT('Ctrl Pts',(90.3613146057131,21.5100372980466,10.));
#30273=CARTESIAN_POINT('Ctrl Pts',(90.295709559598,21.5645230341409,10.));
#30274=CARTESIAN_POINT('Ctrl Pts',(90.2323608843392,21.6217493205763,10.));
#30275=CARTESIAN_POINT('Ctrl Pts',(90.2182621164007,21.6344855006012,10.));
#30276=CARTESIAN_POINT('Ctrl Pts',(90.2042725067479,21.6473601252806,10.));
#30277=CARTESIAN_POINT('Ctrl Pts',(90.1904136996612,21.6603531214757,10.));
#30278=CARTESIAN_POINT('Ctrl Pts',(90.1179829795585,21.7282588268378,10.));
#30279=CARTESIAN_POINT('Ctrl Pts',(90.0490179328352,21.7994862853565,10.));
#30280=CARTESIAN_POINT('Ctrl Pts',(89.9837585062133,21.8737448951322,10.));
#30281=CARTESIAN_POINT('Ctrl Pts',(89.9188587596277,21.9475942255005,10.));
#30282=CARTESIAN_POINT('Ctrl Pts',(89.8576234119932,22.0244421833297,10.));
#30283=CARTESIAN_POINT('Ctrl Pts',(89.8003320729523,22.1040297129063,10.));
#30284=CARTESIAN_POINT('Ctrl Pts',(89.7451392508881,22.1807020412544,10.));
#30285=CARTESIAN_POINT('Ctrl Pts',(89.6936066323768,22.25991765928,10.));
#30286=CARTESIAN_POINT('Ctrl Pts',(89.6460291433843,22.3414585598246,10.));
#30287=CARTESIAN_POINT('Ctrl Pts',(89.6260403806384,22.37571639372,10.));
#30288=CARTESIAN_POINT('Ctrl Pts',(89.6067503090227,22.4103847699375,10.));
#30289=CARTESIAN_POINT('Ctrl Pts',(89.5881834031273,22.4454478212108,10.));
#30290=CARTESIAN_POINT('Ctrl Pts',(89.575146838384,22.4700669871933,10.));
#30291=CARTESIAN_POINT('Ctrl Pts',(89.5624668273212,22.4948807309457,10.));
#30292=CARTESIAN_POINT('Ctrl Pts',(89.55015232839,22.5198835658164,10.));
#30293=CARTESIAN_POINT('Ctrl Pts',(89.54239983886,22.5356238908298,10.));
#30294=CARTESIAN_POINT('Ctrl Pts',(89.5347913334004,22.5514412806442,10.));
#30295=CARTESIAN_POINT('Ctrl Pts',(89.5273387128366,22.5673132395119,10.));
#30296=CARTESIAN_POINT('Ctrl Pts',(89.4852181501773,22.6570180396273,10.));
#30297=CARTESIAN_POINT('Ctrl Pts',(89.4479997999157,22.7486075345407,10.));
#30298=CARTESIAN_POINT('Ctrl Pts',(89.4159753088237,22.8418092601417,10.));
#30299=CARTESIAN_POINT('Ctrl Pts',(89.3861128448231,22.9287187809694,10.));
#30300=CARTESIAN_POINT('Ctrl Pts',(89.3607667972627,23.0170309840461,10.));
#30301=CARTESIAN_POINT('Ctrl Pts',(89.340224189406,23.1065336320398,10.));
#30302=CARTESIAN_POINT('Ctrl Pts',(89.3387369151237,23.1130135778911,10.));
#30303=CARTESIAN_POINT('Ctrl Pts',(89.3372748417248,23.119499764847,10.));
#30304=CARTESIAN_POINT('Ctrl Pts',(89.3358380889382,23.125992112682,10.));
#30305=CARTESIAN_POINT('Ctrl Pts',(89.3152524900327,23.2190135912048,10.));
#30306=CARTESIAN_POINT('Ctrl Pts',(89.2998606756261,23.3133008086003,10.));
#30307=CARTESIAN_POINT('Ctrl Pts',(89.2895856382548,23.4084457389669,10.));
#30308=CARTESIAN_POINT('Ctrl Pts',(89.2837680062693,23.4623159265052,10.));
#30309=CARTESIAN_POINT('Ctrl Pts',(89.2795916051027,23.5164608839161,10.));
#30310=CARTESIAN_POINT('Ctrl Pts',(89.2770493497674,23.5708038567141,10.));
#30311=CARTESIAN_POINT('Ctrl Pts',(89.2764020101009,23.5846413188308,10.));
#30312=CARTESIAN_POINT('Ctrl Pts',(89.275860775699,23.5984902138897,10.));
#30313=CARTESIAN_POINT('Ctrl Pts',(89.275425710371,23.6123370392804,10.));
#30314=CARTESIAN_POINT('Ctrl Pts',(89.2724969038993,23.7055521709181,10.));
#30315=CARTESIAN_POINT('Ctrl Pts',(89.274367487553,23.7988245804704,10.));
#30316=CARTESIAN_POINT('Ctrl Pts',(89.2809025930419,23.891778995953,10.));
#30317=CARTESIAN_POINT('Ctrl Pts',(89.2874481362156,23.9848818755864,10.));
#30318=CARTESIAN_POINT('Ctrl Pts',(89.2986734920106,24.0776667241966,10.));
#30319=CARTESIAN_POINT('Ctrl Pts',(89.3144940517011,24.1697443147494,10.));
#30320=CARTESIAN_POINT('Ctrl Pts',(89.3300874445373,24.2604997664527,10.));
#30321=CARTESIAN_POINT('Ctrl Pts',(89.3501454854825,24.3505689688124,10.));
#30322=CARTESIAN_POINT('Ctrl Pts',(89.3746301441576,24.4395539724182,10.));
#30323=CARTESIAN_POINT('Ctrl Pts',(89.3838722153721,24.4731425860586,10.));
#30324=CARTESIAN_POINT('Ctrl Pts',(89.3937453934005,24.5065763998858,10.));
#30325=CARTESIAN_POINT('Ctrl Pts',(89.4042490565665,24.5398326838582,10.));
#30326=CARTESIAN_POINT('Ctrl Pts',(89.4119449769147,24.5641992032794,10.));
#30327=CARTESIAN_POINT('Ctrl Pts',(89.4199793786913,24.5884704030463,10.));
#30328=CARTESIAN_POINT('Ctrl Pts',(89.4283522643419,24.6126370463772,10.));
#30329=CARTESIAN_POINT('Ctrl Pts',(89.433519789665,24.6275520645202,10.));
#30330=CARTESIAN_POINT('Ctrl Pts',(89.4388132540751,24.642418569377,10.));
#30331=CARTESIAN_POINT('Ctrl Pts',(89.4442314704579,24.657232470925,10.));
#30332=CARTESIAN_POINT('Ctrl Pts',(89.4759375176245,24.7439197178007,10.));
#30333=CARTESIAN_POINT('Ctrl Pts',(89.511920335377,24.828832792636,10.));
#30334=CARTESIAN_POINT('Ctrl Pts',(89.5521196218609,24.9115708704841,10.));
#30335=CARTESIAN_POINT('Ctrl Pts',(89.5822690867238,24.9736244288701,10.));
#30336=CARTESIAN_POINT('Ctrl Pts',(89.6147913043791,25.0344540665882,10.));
#30337=CARTESIAN_POINT('Ctrl Pts',(89.6496759249085,25.0938756897438,10.));
#30338=CARTESIAN_POINT('Ctrl Pts',(89.6654547888551,25.1207530268921,10.));
#30339=CARTESIAN_POINT('Ctrl Pts',(89.6817171405451,25.1473421001399,10.));
#30340=CARTESIAN_POINT('Ctrl Pts',(89.6984628025478,25.1736248045378,10.));
#30341=CARTESIAN_POINT('Ctrl Pts',(89.7075848155659,25.1879420152656,10.));
#30342=CARTESIAN_POINT('Ctrl Pts',(89.7168450675973,25.2021601543536,10.));
#30343=CARTESIAN_POINT('Ctrl Pts',(89.726242878983,25.2162762092358,10.));
#30344=CARTESIAN_POINT('Ctrl Pts',(89.7738179411261,25.2877366972872,10.));
#30345=CARTESIAN_POINT('Ctrl Pts',(89.82491820811,25.3565879238984,10.));
#30346=CARTESIAN_POINT('Ctrl Pts',(89.8795126225196,25.4224764001538,10.));
#30347=CARTESIAN_POINT('Ctrl Pts',(89.9256431150503,25.4781500051302,10.));
#30348=CARTESIAN_POINT('Ctrl Pts',(89.9742689995433,25.5317079390387,10.));
#30349=CARTESIAN_POINT('Ctrl Pts',(90.0253878321675,25.58291282293,10.));
#30350=CARTESIAN_POINT('Ctrl Pts',(90.0442196215672,25.6017763129624,10.));
#30351=CARTESIAN_POINT('Ctrl Pts',(90.0633898808657,25.6203202151646,10.));
#30352=CARTESIAN_POINT('Ctrl Pts',(90.0828884583321,25.6385402287509,10.));
#30353=CARTESIAN_POINT('Origin',(92.,24.,5.));
#30354=CARTESIAN_POINT('Origin',(-92.,-24.,1.));
#30355=CARTESIAN_POINT('Ctrl Pts',(-93.913465996665,-22.364012796625,0.999999999999999));
#30356=CARTESIAN_POINT('Ctrl Pts',(-93.9756062673219,-22.422409392352,0.999999999999999));
#30357=CARTESIAN_POINT('Ctrl Pts',(-94.0343712367569,-22.4840596836639,
0.999999999999998));
#30358=CARTESIAN_POINT('Ctrl Pts',(-94.0897488672685,-22.548587241387,0.999999999999999));
#30359=CARTESIAN_POINT('Ctrl Pts',(-94.1464812232377,-22.6146933629517,
1.));
#30360=CARTESIAN_POINT('Ctrl Pts',(-94.1996589497715,-22.6838197394786,
1.));
#30361=CARTESIAN_POINT('Ctrl Pts',(-94.2492402162377,-22.7556079093562,
1.));
#30362=CARTESIAN_POINT('Ctrl Pts',(-94.2621838800318,-22.7743488976672,
0.999999999999999));
#30363=CARTESIAN_POINT('Ctrl Pts',(-94.2748822665715,-22.793271509596,0.999999999999998));
#30364=CARTESIAN_POINT('Ctrl Pts',(-94.2873342556749,-22.8123698012048,
0.999999999999998));
#30365=CARTESIAN_POINT('Ctrl Pts',(-94.2974953331826,-22.8279543973438,
0.999999999999998));
#30366=CARTESIAN_POINT('Ctrl Pts',(-94.307492770427,-22.8436568723813,1.));
#30367=CARTESIAN_POINT('Ctrl Pts',(-94.3173171317856,-22.8594594356799,
1.));
#30368=CARTESIAN_POINT('Ctrl Pts',(-94.3647643840587,-22.9357787179241,
1.));
#30369=CARTESIAN_POINT('Ctrl Pts',(-94.4082280613636,-23.0145052251332,
1.));
#30370=CARTESIAN_POINT('Ctrl Pts',(-94.4476734134146,-23.0952464698073,
1.));
#30371=CARTESIAN_POINT('Ctrl Pts',(-94.4795142529548,-23.1604219311045,
1.));
#30372=CARTESIAN_POINT('Ctrl Pts',(-94.5087362743067,-23.2269112726343,
0.999999999999997));
#30373=CARTESIAN_POINT('Ctrl Pts',(-94.5353040218407,-23.2945258806355,
0.999999999999997));
#30374=CARTESIAN_POINT('Ctrl Pts',(-94.5460285882024,-23.3218197771016,
0.999999999999996));
#30375=CARTESIAN_POINT('Ctrl Pts',(-94.5563204579687,-23.3492971889389,
0.999999999999999));
#30376=CARTESIAN_POINT('Ctrl Pts',(-94.566176508671,-23.3769462763436,0.999999999999998));
#30377=CARTESIAN_POINT('Ctrl Pts',(-94.5713946946775,-23.3915848050349,
0.999999999999998));
#30378=CARTESIAN_POINT('Ctrl Pts',(-94.5764901608952,-23.4062701280322,
1.));
#30379=CARTESIAN_POINT('Ctrl Pts',(-94.5814586868804,-23.4209886699613,
1.));
#30380=CARTESIAN_POINT('Ctrl Pts',(-94.6109727420549,-23.5084198034374,
1.));
#30381=CARTESIAN_POINT('Ctrl Pts',(-94.6360505254107,-23.5971308207555,
1.));
#30382=CARTESIAN_POINT('Ctrl Pts',(-94.6566592714401,-23.6867240276082,
1.));
#30383=CARTESIAN_POINT('Ctrl Pts',(-94.6775869561989,-23.7777037692606,
1.));
#30384=CARTESIAN_POINT('Ctrl Pts',(-94.6939067088653,-23.8695940231595,
0.999999999999999));
#30385=CARTESIAN_POINT('Ctrl Pts',(-94.705542374548,-23.9620114812617,0.999999999999998));
#30386=CARTESIAN_POINT('Ctrl Pts',(-94.7170868819221,-24.0537049052259,
0.999999999999998));
#30387=CARTESIAN_POINT('Ctrl Pts',(-94.7240207525125,-24.1459182348717,
0.999999999999998));
#30388=CARTESIAN_POINT('Ctrl Pts',(-94.7262226529554,-24.2382962599632,
0.999999999999998));
#30389=CARTESIAN_POINT('Ctrl Pts',(-94.7273178683594,-24.2842446752959,
0.999999999999998));
#30390=CARTESIAN_POINT('Ctrl Pts',(-94.7272416202326,-24.3302340487982,
0.999999999999996));
#30391=CARTESIAN_POINT('Ctrl Pts',(-94.7259741875425,-24.3762213626827,
0.999999999999996));
#30392=CARTESIAN_POINT('Ctrl Pts',(-94.7255574256381,-24.3913430813046,
0.999999999999996));
#30393=CARTESIAN_POINT('Ctrl Pts',(-94.7250117558556,-24.4064664273217,
0.999999999999996));
#30394=CARTESIAN_POINT('Ctrl Pts',(-94.7243366614637,-24.4215840497042,
0.999999999999996));
#30395=CARTESIAN_POINT('Ctrl Pts',(-94.7200628102785,-24.5172898785549,
0.999999999999996));
#30396=CARTESIAN_POINT('Ctrl Pts',(-94.7106219290546,-24.6124285315491,
0.999999999999999));
#30397=CARTESIAN_POINT('Ctrl Pts',(-94.6959498471788,-24.7066016789508,
0.999999999999998));
#30398=CARTESIAN_POINT('Ctrl Pts',(-94.6917951385598,-24.7332687866252,
0.999999999999998));
#30399=CARTESIAN_POINT('Ctrl Pts',(-94.6872206686445,-24.7598586042627,
1.));
#30400=CARTESIAN_POINT('Ctrl Pts',(-94.682224266105,-24.7863623464053,1.));
#30401=CARTESIAN_POINT('Ctrl Pts',(-94.665259332382,-24.8763539404189,1.));
#30402=CARTESIAN_POINT('Ctrl Pts',(-94.6434341104636,-24.9653530573486,
0.999999999999997));
#30403=CARTESIAN_POINT('Ctrl Pts',(-94.617051236814,-25.0531274604659,0.999999999999997));
#30404=CARTESIAN_POINT('Ctrl Pts',(-94.5900718918312,-25.1428862916612,
0.999999999999996));
#30405=CARTESIAN_POINT('Ctrl Pts',(-94.5583262747353,-25.2313651060452,
0.999999999999996));
#30406=CARTESIAN_POINT('Ctrl Pts',(-94.522083774644,-25.3183118483838,0.999999999999997));
#30407=CARTESIAN_POINT('Ctrl Pts',(-94.5094168709612,-25.3487000944476,
0.999999999999997));
#30408=CARTESIAN_POINT('Ctrl Pts',(-94.4962001982363,-25.3789011100916,
0.999999999999999));
#30409=CARTESIAN_POINT('Ctrl Pts',(-94.4824438244244,-25.4089037784715,
0.999999999999999));
#30410=CARTESIAN_POINT('Ctrl Pts',(-94.4754968108625,-25.4240552236835,
0.999999999999999));
#30411=CARTESIAN_POINT('Ctrl Pts',(-94.4684121470112,-25.4391560809515,
0.999999999999999));
#30412=CARTESIAN_POINT('Ctrl Pts',(-94.4611910621987,-25.4542048928028,
0.999999999999999));
#30413=CARTESIAN_POINT('Ctrl Pts',(-94.455180892849,-25.4667301449065,0.999999999999998));
#30414=CARTESIAN_POINT('Ctrl Pts',(-94.449078063724,-25.4792154077161,0.999999999999999));
#30415=CARTESIAN_POINT('Ctrl Pts',(-94.4428871733088,-25.4916526565279,
0.999999999999999));
#30416=CARTESIAN_POINT('Ctrl Pts',(-94.3999238161019,-25.577964305988,0.999999999999999));
#30417=CARTESIAN_POINT('Ctrl Pts',(-94.3526734205402,-25.6620692721598,
1.));
#30418=CARTESIAN_POINT('Ctrl Pts',(-94.3014780528836,-25.7437174772354,
1.));
#30419=CARTESIAN_POINT('Ctrl Pts',(-94.2492778933731,-25.8269681603301,
1.));
#30420=CARTESIAN_POINT('Ctrl Pts',(-94.1929760719894,-25.907665474163,0.999999999999999));
#30421=CARTESIAN_POINT('Ctrl Pts',(-94.1328802769678,-25.9855370030581,
1.));
#30422=CARTESIAN_POINT('Ctrl Pts',(-94.0723164763602,-26.0640149689011,
1.));
#30423=CARTESIAN_POINT('Ctrl Pts',(-94.0078989170008,-26.1396238030331,
1.));
#30424=CARTESIAN_POINT('Ctrl Pts',(-93.9398933824888,-26.2120650887426,
1.));
#30425=CARTESIAN_POINT('Ctrl Pts',(-93.9029668413288,-26.2514002125325,
1.));
#30426=CARTESIAN_POINT('Ctrl Pts',(-93.8649816076841,-26.2898009990597,
0.999999999999999));
#30427=CARTESIAN_POINT('Ctrl Pts',(-93.8259749923962,-26.3272159157843,
0.999999999999999));
#30428=CARTESIAN_POINT('Ctrl Pts',(-93.8138410590721,-26.3388547134989,
0.999999999999999));
#30429=CARTESIAN_POINT('Ctrl Pts',(-93.8016082652093,-26.3503980889207,
0.999999999999998));
#30430=CARTESIAN_POINT('Ctrl Pts',(-93.7892776690852,-26.3618444261323,
0.999999999999998));
#30431=CARTESIAN_POINT('Ctrl Pts',(-93.7779940519145,-26.372318865957,0.999999999999998));
#30432=CARTESIAN_POINT('Ctrl Pts',(-93.7666342733719,-26.3827066803521,
0.999999999999997));
#30433=CARTESIAN_POINT('Ctrl Pts',(-93.7552037473516,-26.3930030342907,
0.999999999999997));
#30434=CARTESIAN_POINT('Ctrl Pts',(-93.6793946848277,-26.4612900875824,
0.999999999999996));
#30435=CARTESIAN_POINT('Ctrl Pts',(-93.6004193335679,-26.5256101176591,
0.999999999999996));
#30436=CARTESIAN_POINT('Ctrl Pts',(-93.5186038562927,-26.5856805003819,
0.999999999999995));
#30437=CARTESIAN_POINT('Ctrl Pts',(-93.4367174573237,-26.6458029550773,
0.999999999999995));
#30438=CARTESIAN_POINT('Ctrl Pts',(-93.351985429421,-26.7016692287801,0.999999999999997));
#30439=CARTESIAN_POINT('Ctrl Pts',(-93.2646898210428,-26.752969758348,0.999999999999996));
#30440=CARTESIAN_POINT('Ctrl Pts',(-93.1791579830026,-26.8032337827119,
0.999999999999996));
#30441=CARTESIAN_POINT('Ctrl Pts',(-93.0911644456872,-26.8491153709103,
0.999999999999998));
#30442=CARTESIAN_POINT('Ctrl Pts',(-93.0009407547904,-26.8902872130475,
0.999999999999999));
#30443=CARTESIAN_POINT('Ctrl Pts',(-92.963151738466,-26.9075315022044,0.999999999999999));
#30444=CARTESIAN_POINT('Ctrl Pts',(-92.9249711428035,-26.9239490878333,
1.));
#30445=CARTESIAN_POINT('Ctrl Pts',(-92.8864145873394,-26.9395135460181,
1.));
#30446=CARTESIAN_POINT('Ctrl Pts',(-92.8564008951788,-26.9516294326938,
1.));
#30447=CARTESIAN_POINT('Ctrl Pts',(-92.8261593691066,-26.9632283272652,
0.999999999999999));
#30448=CARTESIAN_POINT('Ctrl Pts',(-92.7957017813268,-26.9743128096466,
0.999999999999999));
#30449=CARTESIAN_POINT('Ctrl Pts',(-91.2062007174671,-26.9692229537457,
1.));
#30450=CARTESIAN_POINT('Ctrl Pts',(-91.1113643951071,-26.9345314033953,
1.));
#30451=CARTESIAN_POINT('Ctrl Pts',(-91.0185713035755,-26.8948494397933,
1.));
#30452=CARTESIAN_POINT('Ctrl Pts',(-90.9280623762692,-26.8504973089265,
1.));
#30453=CARTESIAN_POINT('Ctrl Pts',(-90.8362819518266,-26.805522105739,1.));
#30454=CARTESIAN_POINT('Ctrl Pts',(-90.7468496512692,-26.755743896015,0.999999999999998));
#30455=CARTESIAN_POINT('Ctrl Pts',(-90.6600507311862,-26.7014559325823,
0.999999999999998));
#30456=CARTESIAN_POINT('Ctrl Pts',(-90.6355419727628,-26.6861270485386,
0.999999999999997));
#30457=CARTESIAN_POINT('Ctrl Pts',(-90.6112434098825,-26.6704383986501,
0.999999999999998));
#30458=CARTESIAN_POINT('Ctrl Pts',(-90.5871620603007,-26.6543961292597,
0.999999999999998));
#30459=CARTESIAN_POINT('Ctrl Pts',(-90.5678313682138,-26.6415186047294,
0.999999999999998));
#30460=CARTESIAN_POINT('Ctrl Pts',(-90.5486385360232,-26.6284115929408,
0.999999999999998));
#30461=CARTESIAN_POINT('Ctrl Pts',(-90.5296064824045,-26.6150920391085,
0.999999999999998));
#30462=CARTESIAN_POINT('Ctrl Pts',(-90.4468988471007,-26.5572092261004,
0.999999999999999));
#30463=CARTESIAN_POINT('Ctrl Pts',(-90.3671460463151,-26.4952646296917,
1.));
#30464=CARTESIAN_POINT('Ctrl Pts',(-90.2906144358446,-26.4295554859959,
1.));
#30465=CARTESIAN_POINT('Ctrl Pts',(-90.2316015873974,-26.3788877460298,
1.));
#30466=CARTESIAN_POINT('Ctrl Pts',(-90.1745046339107,-26.3259807644008,
0.999999999999999));
#30467=CARTESIAN_POINT('Ctrl Pts',(-90.1194632797683,-26.2709590345817,
0.999999999999998));
#30468=CARTESIAN_POINT('Ctrl Pts',(-90.0901431566793,-26.241649365225,0.999999999999998));
#30469=CARTESIAN_POINT('Ctrl Pts',(-90.0614066103864,-26.211739462745,1.));
#30470=CARTESIAN_POINT('Ctrl Pts',(-90.0332767877765,-26.18124731084,1.));
#30471=CARTESIAN_POINT('Ctrl Pts',(-90.0236428023317,-26.1708042678209,
1.));
#30472=CARTESIAN_POINT('Ctrl Pts',(-90.0140807815228,-26.1602937103339,
1.));
#30473=CARTESIAN_POINT('Ctrl Pts',(-90.0045982120972,-26.1497238889479,
1.));
#30474=CARTESIAN_POINT('Ctrl Pts',(-89.938805722262,-26.0763877671762,1.));
#30475=CARTESIAN_POINT('Ctrl Pts',(-89.876745482153,-26.0001052971121,1.));
#30476=CARTESIAN_POINT('Ctrl Pts',(-89.8186612830851,-25.9211548961491,
1.));
#30477=CARTESIAN_POINT('Ctrl Pts',(-89.7610834896514,-25.8428928222785,
1.));
#30478=CARTESIAN_POINT('Ctrl Pts',(-89.7074122724075,-25.762008351304,1.));
#30479=CARTESIAN_POINT('Ctrl Pts',(-89.6579309060241,-25.678750276668,1.));
#30480=CARTESIAN_POINT('Ctrl Pts',(-89.6098825260779,-25.5979033660816,
1.));
#30481=CARTESIAN_POINT('Ctrl Pts',(-89.5657846284712,-25.5148176410515,
1.));
#30482=CARTESIAN_POINT('Ctrl Pts',(-89.5259443770766,-25.4297105806844,
1.));
#30483=CARTESIAN_POINT('Ctrl Pts',(-89.5051331098887,-25.3852533869951,
1.));
#30484=CARTESIAN_POINT('Ctrl Pts',(-89.4854844375302,-25.340244525694,1.));
#30485=CARTESIAN_POINT('Ctrl Pts',(-89.4670478470478,-25.2947147599898,
1.));
#30486=CARTESIAN_POINT('Ctrl Pts',(-89.4599071766988,-25.277080640044,1.));
#30487=CARTESIAN_POINT('Ctrl Pts',(-89.4529483729289,-25.2593683810712,
1.));
#30488=CARTESIAN_POINT('Ctrl Pts',(-89.4461744795067,-25.2415797795319,
1.));
#30489=CARTESIAN_POINT('Ctrl Pts',(-89.4410205926902,-25.2280454008159,
1.));
#30490=CARTESIAN_POINT('Ctrl Pts',(-89.4359737884854,-25.2144667084508,
1.));
#30491=CARTESIAN_POINT('Ctrl Pts',(-89.4310402378581,-25.2008583977092,
1.));
#30492=CARTESIAN_POINT('Ctrl Pts',(-89.3993683880461,-25.1134973049451,
1.));
#30493=CARTESIAN_POINT('Ctrl Pts',(-89.3723052489148,-25.0247752781117,
1.));
#30494=CARTESIAN_POINT('Ctrl Pts',(-89.3501021061037,-24.9349157228039,
1.));
#30495=CARTESIAN_POINT('Ctrl Pts',(-89.3450995089376,-24.9146694378273,
1.));
#30496=CARTESIAN_POINT('Ctrl Pts',(-89.3403438330582,-24.8943653665978,
1.));
#30497=CARTESIAN_POINT('Ctrl Pts',(-89.3358383183128,-24.8740060081578,
1.));
#30498=CARTESIAN_POINT('Ctrl Pts',(-89.3154927915306,-24.7820693714308,
1.));
#30499=CARTESIAN_POINT('Ctrl Pts',(-89.3002442665944,-24.6890050257332,
1.));
#30500=CARTESIAN_POINT('Ctrl Pts',(-89.2899828336273,-24.5952047143853,
1.));
#30501=CARTESIAN_POINT('Ctrl Pts',(-89.2792696952268,-24.4972753393461,
1.));
#30502=CARTESIAN_POINT('Ctrl Pts',(-89.2739923846863,-24.3985425391207,
1.));
#30503=CARTESIAN_POINT('Ctrl Pts',(-89.2740833202269,-24.2994667952368,
1.));
#30504=CARTESIAN_POINT('Ctrl Pts',(-89.2741184401281,-24.2612030942728,
1.));
#30505=CARTESIAN_POINT('Ctrl Pts',(-89.2749548502661,-24.2228884940833,
1.));
#30506=CARTESIAN_POINT('Ctrl Pts',(-89.2765907919855,-24.1845506991706,
1.));
#30507=CARTESIAN_POINT('Ctrl Pts',(-89.2771783957763,-24.170780383667,1.));
#30508=CARTESIAN_POINT('Ctrl Pts',(-89.2778691417581,-24.1570088738121,
0.999999999999999));
#30509=CARTESIAN_POINT('Ctrl Pts',(-89.2786620584242,-24.1432491218723,
0.999999999999999));
#30510=CARTESIAN_POINT('Ctrl Pts',(-89.2840136676959,-24.0503808304004,
0.999999999999999));
#30511=CARTESIAN_POINT('Ctrl Pts',(-89.2940209876791,-23.9578996294849,
1.));
#30512=CARTESIAN_POINT('Ctrl Pts',(-89.308560961015,-23.8661774184892,1.));
#30513=CARTESIAN_POINT('Ctrl Pts',(-89.3230638861899,-23.7746889176356,
1.));
#30514=CARTESIAN_POINT('Ctrl Pts',(-89.3420768069923,-23.683954599498,1.));
#30515=CARTESIAN_POINT('Ctrl Pts',(-89.3655261935074,-23.5943606394727,
1.));
#30516=CARTESIAN_POINT('Ctrl Pts',(-89.3885742801647,-23.5062999410276,
0.999999999999999));
#30517=CARTESIAN_POINT('Ctrl Pts',(-89.415908753375,-23.41934012046,0.999999999999997));
#30518=CARTESIAN_POINT('Ctrl Pts',(-89.4475001290534,-23.3338770863052,
0.999999999999997));
#30519=CARTESIAN_POINT('Ctrl Pts',(-89.4633626084254,-23.2909648804505,
0.999999999999997));
#30520=CARTESIAN_POINT('Ctrl Pts',(-89.4802989283759,-23.2484305779728,
0.999999999999998));
#30521=CARTESIAN_POINT('Ctrl Pts',(-89.4983087451776,-23.2063280775901,
0.999999999999998));
#30522=CARTESIAN_POINT('Ctrl Pts',(-89.5036080599323,-23.1939395894702,
0.999999999999997));
#30523=CARTESIAN_POINT('Ctrl Pts',(-89.5090003327764,-23.1815885059394,
0.999999999999996));
#30524=CARTESIAN_POINT('Ctrl Pts',(-89.5144855894355,-23.1692762489132,
0.999999999999995));
#30525=CARTESIAN_POINT('Ctrl Pts',(-89.5200790131214,-23.1567211991945,
0.999999999999995));
#30526=CARTESIAN_POINT('Ctrl Pts',(-89.5257654438863,-23.1442148109042,
0.999999999999999));
#30527=CARTESIAN_POINT('Ctrl Pts',(-89.5315435926943,-23.1317604191048,
0.999999999999999));
#30528=CARTESIAN_POINT('Ctrl Pts',(-89.5690289714347,-23.0509633318206,
0.999999999999999));
#30529=CARTESIAN_POINT('Ctrl Pts',(-89.6103840527349,-22.9723231040759,
0.999999999999997));
#30530=CARTESIAN_POINT('Ctrl Pts',(-89.6555390131612,-22.8961874416404,
0.999999999999998));
#30531=CARTESIAN_POINT('Ctrl Pts',(-89.69993578728,-22.8213301551846,0.999999999999999));
#30532=CARTESIAN_POINT('Ctrl Pts',(-89.748006360481,-22.7488933635223,1.));
#30533=CARTESIAN_POINT('Ctrl Pts',(-89.7997205683589,-22.6792417324263,
1.));
#30534=CARTESIAN_POINT('Ctrl Pts',(-89.8498548288956,-22.6117180641064,
1.));
#30535=CARTESIAN_POINT('Ctrl Pts',(-89.9034139310733,-22.5468115334525,
1.));
#30536=CARTESIAN_POINT('Ctrl Pts',(-89.9603980832495,-22.4848946770453,
1.));
#30537=CARTESIAN_POINT('Ctrl Pts',(-89.9815871696769,-22.4618714052826,
1.));
#30538=CARTESIAN_POINT('Ctrl Pts',(-90.0032500737241,-22.439261946639,0.999999999999998));
#30539=CARTESIAN_POINT('Ctrl Pts',(-90.0253876448586,-22.417087121357,0.999999999999998));
#30540=CARTESIAN_POINT('Ctrl Pts',(-90.0442144350809,-22.3982286485253,
0.999999999999998));
#30541=CARTESIAN_POINT('Ctrl Pts',(-90.0633845524044,-22.3796845518288,
0.999999999999999));
#30542=CARTESIAN_POINT('Ctrl Pts',(-90.0828882653787,-22.3614597476137,
0.999999999999999));
#30543=CARTESIAN_POINT('Origin',(-92.,-24.,12.2084234471775));
#30544=CARTESIAN_POINT('Ctrl Pts',(-95.0767669904684,-23.998062685181,9.70842344717746));
#30545=CARTESIAN_POINT('Ctrl Pts',(-95.0777011675186,-23.8738981078454,
9.70197366100994));
#30546=CARTESIAN_POINT('Ctrl Pts',(-95.0146668802256,-22.7368860788636,
9.64286281975954));
#30547=CARTESIAN_POINT('Ctrl Pts',(-93.5990318095031,-20.7444872358932,
9.53109092342626));
#30548=CARTESIAN_POINT('Ctrl Pts',(-90.1476049582096,-20.8820466605266,
9.37310775817762));
#30549=CARTESIAN_POINT('Ctrl Pts',(-88.3764280027803,-23.8472850428361,
9.21512459292899));
#30550=CARTESIAN_POINT('Ctrl Pts',(-89.8919230124438,-26.9512424150719,
9.05714142768036));
#30551=CARTESIAN_POINT('Ctrl Pts',(-93.3195312348388,-27.3782236147545,
8.89915826243172));
#30552=CARTESIAN_POINT('Ctrl Pts',(-94.9608441448919,-25.4378981546874,
8.78291893559742));
#30553=CARTESIAN_POINT('Ctrl Pts',(-95.0762794797313,-24.2133137737379,
8.719340663846));
#30554=CARTESIAN_POINT('Ctrl Pts',(-95.0743676381347,-24.0026790873961,
8.70842344717746));
#30555=CARTESIAN_POINT('Ctrl Pts',(-95.0702887490763,-24.0031018432153,
9.79157655282255));
#30556=CARTESIAN_POINT('Ctrl Pts',(-95.0652853033504,-23.3096184359042,
9.75572892504928));
#30557=CARTESIAN_POINT('Ctrl Pts',(-94.4922441588307,-21.5876431146109,
9.66722024219312));
#30558=CARTESIAN_POINT('Ctrl Pts',(-91.6460838755241,-20.3911593875009,
9.5260505042541));
#30559=CARTESIAN_POINT('Ctrl Pts',(-88.7843953448966,-22.3229252160129,
9.36806733900546));
#30560=CARTESIAN_POINT('Ctrl Pts',(-88.8381771631846,-25.7771164103053,
9.21008417375683));
#30561=CARTESIAN_POINT('Ctrl Pts',(-91.7604241627304,-27.6187849549088,
9.05210100850819));
#30562=CARTESIAN_POINT('Ctrl Pts',(-94.5324624275929,-26.346888962543,8.91259846819677));
#30563=CARTESIAN_POINT('Ctrl Pts',(-95.0660798384141,-24.6595176403422,
8.82575698296822));
#30564=CARTESIAN_POINT('Ctrl Pts',(-95.0703859251749,-23.9978642356407,
8.79157655282255));
#30565=CARTESIAN_POINT('Ctrl Pts',(-90.0865340033349,-22.3640127966251,
10.));
#30566=CARTESIAN_POINT('Ctrl Pts',(-89.5452199193478,-22.9971388327508,
9.94733894491712));
#30567=CARTESIAN_POINT('Ctrl Pts',(-89.1498731367062,-24.8326003723509,
9.84201683475137));
#30568=CARTESIAN_POINT('Ctrl Pts',(-91.1420127726733,-26.8458067969655,
9.68403366950273));
#30569=CARTESIAN_POINT('Ctrl Pts',(-93.9132999553889,-26.2718355849706,
9.5260505042541));
#30570=CARTESIAN_POINT('Ctrl Pts',(-94.948715185934,-23.6401115468636,9.36806733900547));
#30571=CARTESIAN_POINT('Ctrl Pts',(-93.309764952147,-21.3334135729172,9.21008417375683));
#30572=CARTESIAN_POINT('Ctrl Pts',(-90.4827055416602,-21.4460883253215,
9.05210100850819));
#30573=CARTESIAN_POINT('Ctrl Pts',(-89.0319367161215,-23.8749113698845,
8.89411784325956));
#30574=CARTESIAN_POINT('Ctrl Pts',(-90.2732767801618,-26.4173589653305,
8.73613467801093));
#30575=CARTESIAN_POINT('Ctrl Pts',(-93.0808263815541,-26.7670987311353,
8.57815151276229));
#30576=CARTESIAN_POINT('Ctrl Pts',(-94.9080233748186,-24.6070250335036,
8.42016834751366));
#30577=CARTESIAN_POINT('Ctrl Pts',(-94.0975469404961,-21.8963395546466,
8.26218518226502));
#30578=CARTESIAN_POINT('Ctrl Pts',(-91.3845223535449,-21.0937553800026,
8.10420201701639));
#30579=CARTESIAN_POINT('Ctrl Pts',(-89.2297577260391,-22.9272296313332,
7.94621885176776));
#30580=CARTESIAN_POINT('Ctrl Pts',(-89.587697039581,-25.733745495277,7.78823568651912));
#30581=CARTESIAN_POINT('Ctrl Pts',(-92.1336776494793,-26.9676939059565,
7.63025252127048));
#30582=CARTESIAN_POINT('Ctrl Pts',(-94.5584079833073,-25.5098431949504,
7.47226935602185));
#30583=CARTESIAN_POINT('Ctrl Pts',(-94.662574994087,-22.6825129051978,7.31428619077321));
#30584=CARTESIAN_POINT('Ctrl Pts',(-92.3516955853902,-21.0501885096968,
7.15630302552458));
#30585=CARTESIAN_POINT('Ctrl Pts',(-89.7218162866321,-22.0934437553399,
6.99831986027595));
#30586=CARTESIAN_POINT('Ctrl Pts',(-89.1583273702903,-24.866010621054,6.84033669502731));
#30587=CARTESIAN_POINT('Ctrl Pts',(-91.1723325238739,-26.8530762793412,
6.68235352977868));
#30588=CARTESIAN_POINT('Ctrl Pts',(-93.9370603271938,-26.2523043781637,
6.52437036453004));
#30589=CARTESIAN_POINT('Ctrl Pts',(-94.944808298303,-23.6086155263393,6.36638719928141));
#30590=CARTESIAN_POINT('Ctrl Pts',(-93.2815146299498,-21.3199257527161,
6.20840403403277));
#30591=CARTESIAN_POINT('Ctrl Pts',(-90.4558434515285,-21.4621547971772,
6.05042086878414));
#30592=CARTESIAN_POINT('Ctrl Pts',(-89.0307749678768,-23.9062960631276,
5.8924377035355));
#30593=CARTESIAN_POINT('Ctrl Pts',(-90.2988949344083,-26.4354299979252,
5.73445453828687));
#30594=CARTESIAN_POINT('Ctrl Pts',(-93.1099752577798,-26.7555457982637,
5.57647137303824));
#30595=CARTESIAN_POINT('Ctrl Pts',(-94.9142701365137,-24.576287506837,5.4184882077896));
#30596=CARTESIAN_POINT('Ctrl Pts',(-94.0752225311475,-21.8743167768149,
5.26050504254097));
#30597=CARTESIAN_POINT('Ctrl Pts',(-91.3538772582215,-21.1004132843165,
5.10252187729234));
#30598=CARTESIAN_POINT('Ctrl Pts',(-89.218587365677,-22.9565339120964,4.94453871204369));
#30599=CARTESIAN_POINT('Ctrl Pts',(-89.6061336679679,-25.7591138972605,
4.78655554679507));
#30600=CARTESIAN_POINT('Ctrl Pts',(-92.1649984413478,-26.9661175354377,
4.62857238154642));
#30601=CARTESIAN_POINT('Ctrl Pts',(-94.574203996375,-25.4827513287052,4.4705892162978));
#30602=CARTESIAN_POINT('Ctrl Pts',(-94.6485186642022,-22.6544790580041,
4.31260605104916));
#30603=CARTESIAN_POINT('Ctrl Pts',(-92.3205365027268,-21.0466402058836,
4.15462288580052));
#30604=CARTESIAN_POINT('Ctrl Pts',(-89.7018167952366,-22.1175994942308,
3.99663972055189));
#30605=CARTESIAN_POINT('Ctrl Pts',(-89.1676276911652,-24.8959602861542,
3.83865655530326));
#30606=CARTESIAN_POINT('Ctrl Pts',(-91.2024969568081,-26.861654528766,3.68067339005462));
#30607=CARTESIAN_POINT('Ctrl Pts',(-93.960728681338,-26.2317304163556,3.52269022480599));
#30608=CARTESIAN_POINT('Ctrl Pts',(-94.9405126124961,-23.577550689598,3.36470705955735));
#30609=CARTESIAN_POINT('Ctrl Pts',(-93.2531511472893,-21.3065468104243,
3.20672389430872));
#30610=CARTESIAN_POINT('Ctrl Pts',(-90.4291390042645,-21.4785971036944,
3.04874072906008));
#30611=CARTESIAN_POINT('Ctrl Pts',(-89.0299510223576,-23.9376454841629,
2.89075756381145));
#30612=CARTESIAN_POINT('Ctrl Pts',(-90.3246996110788,-26.453252357017,2.73277439856282));
#30613=CARTESIAN_POINT('Ctrl Pts',(-93.1390012538637,-26.7436739362116,
2.57479123331418));
#30614=CARTESIAN_POINT('Ctrl Pts',(-94.9201931102794,-24.5454930206753,
2.41680806806555));
#30615=CARTESIAN_POINT('Ctrl Pts',(-94.0526635517577,-21.8525243463366,
2.25882490281691));
#30616=CARTESIAN_POINT('Ctrl Pts',(-91.3233115518592,-21.1074036232017,
2.10084173756828));
#30617=CARTESIAN_POINT('Ctrl Pts',(-89.2077115778014,-22.9859374711348,
1.94285857231964));
#30618=CARTESIAN_POINT('Ctrl Pts',(-89.624868659881,-25.7843200216543,1.78487540707101));
#30619=CARTESIAN_POINT('Ctrl Pts',(-92.1962362586587,-26.964142143379,1.62689224182237));
#30620=CARTESIAN_POINT('Ctrl Pts',(-94.5898450807176,-25.4556338347462,
1.46890907657374));
#30621=CARTESIAN_POINT('Ctrl Pts',(-94.6338976845917,-22.6263101028395,
1.3109259113251));
#30622=CARTESIAN_POINT('Ctrl Pts',(-92.2898922478439,-21.04400336112,1.15294274607647));
#30623=CARTESIAN_POINT('Ctrl Pts',(-89.6809479657765,-22.1407646543606,
0.994959580827837));
#30624=CARTESIAN_POINT('Ctrl Pts',(-89.1795854924137,-24.928282565981,0.836976415579201));
#30625=CARTESIAN_POINT('Ctrl Pts',(-90.5450731455404,-26.2169491679593,
0.731654305413445));
#30626=CARTESIAN_POINT('Ctrl Pts',(-91.3498000020249,-26.4320868020351,
0.678993250330566));
#30627=CARTESIAN_POINT('Ctrl Pts',(-89.9456684496579,-22.2435746787732,
10.1070022498898));
#30628=CARTESIAN_POINT('Ctrl Pts',(-89.3645039014938,-22.9233101920371,
10.0543411948069));
#30629=CARTESIAN_POINT('Ctrl Pts',(-88.9400524765287,-24.8938947526259,
9.94901908464118));
#30630=CARTESIAN_POINT('Ctrl Pts',(-91.0788494627237,-27.0553094224687,
9.79103591939254));
#30631=CARTESIAN_POINT('Ctrl Pts',(-94.0541532854381,-26.4390835936093,
9.63305275414391));
#30632=CARTESIAN_POINT('Ctrl Pts',(-95.1657937219657,-23.6136172760998,
9.47506958889528));
#30633=CARTESIAN_POINT('Ctrl Pts',(-93.4061872379324,-21.1371047939092,
9.31708642364664));
#30634=CARTESIAN_POINT('Ctrl Pts',(-90.3710053471766,-21.2580744370565,
9.159103258398));
#30635=CARTESIAN_POINT('Ctrl Pts',(-88.8134338116745,-23.8657025942017,
9.00112009314937));
#30636=CARTESIAN_POINT('Ctrl Pts',(-90.1461588575891,-26.5953201152443,
8.84313692790073));
#30637=CARTESIAN_POINT('Ctrl Pts',(-93.1603946659823,-26.970807025675,8.68515376265211));
#30638=CARTESIAN_POINT('Ctrl Pts',(-95.1221062608034,-24.6517130068407,
8.52717059740346));
#30639=CARTESIAN_POINT('Ctrl Pts',(-94.2519641664366,-21.741472264661,8.36918743215484));
#30640=CARTESIAN_POINT('Ctrl Pts',(-91.3392121156861,-20.8798034424033,
8.21120426690619));
#30641=CARTESIAN_POINT('Ctrl Pts',(-89.0258180101408,-22.8482544145205,
8.05322110165756));
#30642=CARTESIAN_POINT('Ctrl Pts',(-89.4101081026736,-25.861380383774,7.89523793640894));
#30643=CARTESIAN_POINT('Ctrl Pts',(-92.1435187316521,-27.186169617537,7.73725477116029));
#30644=CARTESIAN_POINT('Ctrl Pts',(-94.7467528808537,-25.6209948422715,
7.57927160591167));
#30645=CARTESIAN_POINT('Ctrl Pts',(-94.8585884593915,-22.5855221306583,
7.42128844066302));
#30646=CARTESIAN_POINT('Ctrl Pts',(-92.3775867135567,-20.8330292659221,
7.26330527541439));
#30647=CARTESIAN_POINT('Ctrl Pts',(-89.5541009414307,-21.9530868838363,
7.10532211016575));
#30648=CARTESIAN_POINT('Ctrl Pts',(-88.9491290939423,-24.9297645972614,
6.94733894491712));
#30649=CARTESIAN_POINT('Ctrl Pts',(-91.111401293589,-27.0631140696509,6.78935577966849));
#30650=CARTESIAN_POINT('Ctrl Pts',(-94.0796628484676,-26.4181145382775,
6.63137261441986));
#30651=CARTESIAN_POINT('Ctrl Pts',(-95.1615992170526,-23.5798025813071,
6.47338944917121));
#30652=CARTESIAN_POINT('Ctrl Pts',(-93.37585718331,-21.1226240272623,6.31540628392259));
#30653=CARTESIAN_POINT('Ctrl Pts',(-90.342165723498,-21.2753236905543,6.15742311867395));
#30654=CARTESIAN_POINT('Ctrl Pts',(-88.812186537839,-23.8993977660205,5.99943995342531));
#30655=CARTESIAN_POINT('Ctrl Pts',(-90.1736629693015,-26.6147215012481,
5.84145678817668));
#30656=CARTESIAN_POINT('Ctrl Pts',(-93.1916894243903,-26.9584035889072,
5.68347362292805));
#30657=CARTESIAN_POINT('Ctrl Pts',(-95.1288128966464,-24.618712644712,5.52549045767941));
#30658=CARTESIAN_POINT('Ctrl Pts',(-94.227996278558,-21.7178282138105,5.36750729243077));
#30659=CARTESIAN_POINT('Ctrl Pts',(-91.306310989512,-20.8869514883654,5.20952412718215));
#30660=CARTESIAN_POINT('Ctrl Pts',(-89.0138253101082,-22.8797160180383,
5.05154096193351));
#30661=CARTESIAN_POINT('Ctrl Pts',(-89.4299019989034,-25.8886163569595,
4.89355779668488));
#30662=CARTESIAN_POINT('Ctrl Pts',(-92.1771452978045,-27.1844771977619,
4.73557463143624));
#30663=CARTESIAN_POINT('Ctrl Pts',(-94.7637117649265,-25.5919085268197,
4.5775914661876));
#30664=CARTESIAN_POINT('Ctrl Pts',(-94.8434973305108,-22.5554244874977,
4.41960830093897));
#30665=CARTESIAN_POINT('Ctrl Pts',(-92.3441337613189,-20.8292197430529,
4.26162513569033));
#30666=CARTESIAN_POINT('Ctrl Pts',(-89.5326291273321,-21.9790209200887,
4.10364197044171));
#30667=CARTESIAN_POINT('Ctrl Pts',(-88.9591140859071,-24.961919097025,3.94565880519306));
#30668=CARTESIAN_POINT('Ctrl Pts',(-91.1437863719667,-27.0723238327043,
3.78767563994443));
#30669=CARTESIAN_POINT('Ctrl Pts',(-94.1050736196794,-26.3960259623991,
3.6296924746958));
#30670=CARTESIAN_POINT('Ctrl Pts',(-95.1569872914167,-23.5464508131884,
3.47170930944716));
#30671=CARTESIAN_POINT('Ctrl Pts',(-93.3454056375763,-21.1082601538994,
3.31372614419853));
#30672=CARTESIAN_POINT('Ctrl Pts',(-90.3134953480409,-21.2929764469124,
3.15574297894989));
#30673=CARTESIAN_POINT('Ctrl Pts',(-88.8113019350925,-23.933055068962,2.99775981370126));
#30674=CARTESIAN_POINT('Ctrl Pts',(-90.2013673348471,-26.6338559069013,
2.83977664845262));
#30675=CARTESIAN_POINT('Ctrl Pts',(-93.2228522564652,-26.9456577440281,
2.68179348320399));
#30676=CARTESIAN_POINT('Ctrl Pts',(-95.1351719079378,-24.5856511298438,
2.52381031795535));
#30677=CARTESIAN_POINT('Ctrl Pts',(-94.2037765520592,-21.6944314680265,
2.36582715270672));
#30678=CARTESIAN_POINT('Ctrl Pts',(-91.2734950967561,-20.8944564420696,
2.20784398745809));
#30679=CARTESIAN_POINT('Ctrl Pts',(-89.0021488684016,-22.9112842085,2.04986082220945));
#30680=CARTESIAN_POINT('Ctrl Pts',(-89.4500162235876,-25.9156781060025,
1.89187765696082));
#30681=CARTESIAN_POINT('Ctrl Pts',(-92.2106827809777,-27.1823563812762,
1.73389449171218));
#30682=CARTESIAN_POINT('Ctrl Pts',(-94.78050431473,-25.562794696993,1.57591132646355));
#30683=CARTESIAN_POINT('Ctrl Pts',(-94.8277999835169,-22.5251817899866,
1.41792816121491));
#30684=CARTESIAN_POINT('Ctrl Pts',(-92.3112335374568,-20.8263887790323,
1.25994499596628));
#30685=CARTESIAN_POINT('Ctrl Pts',(-89.5102239762328,-22.0038914531457,
1.10196183071765));
#30686=CARTESIAN_POINT('Ctrl Pts',(-88.971952196655,-24.9966208786834,0.943978665469012));
#30687=CARTESIAN_POINT('Ctrl Pts',(-90.4379643297735,-26.3801565479508,
0.838656555303256));
#30688=CARTESIAN_POINT('Ctrl Pts',(-91.301933573839,-26.6111321859386,0.785995500220377));
#30689=CARTESIAN_POINT('Ctrl Pts',(-89.8048028959809,-22.1231365609213,
10.2140044997796));
#30690=CARTESIAN_POINT('Ctrl Pts',(-89.1837878836397,-22.8494815513233,
10.1613434446967));
#30691=CARTESIAN_POINT('Ctrl Pts',(-88.7302318163511,-24.9551891329009,
10.056021334531));
#30692=CARTESIAN_POINT('Ctrl Pts',(-91.0156861527742,-27.2648120479719,
9.89803816928236));
#30693=CARTESIAN_POINT('Ctrl Pts',(-94.1950066154872,-26.606331602248,9.74005500403371));
#30694=CARTESIAN_POINT('Ctrl Pts',(-95.3828722579974,-23.587123005336,9.58207183878509));
#30695=CARTESIAN_POINT('Ctrl Pts',(-93.5026095237177,-20.9407960149012,
9.42408867353644));
#30696=CARTESIAN_POINT('Ctrl Pts',(-90.2593051526931,-21.0700605487915,
9.26610550828782));
#30697=CARTESIAN_POINT('Ctrl Pts',(-88.5949309072274,-23.8564938185189,
9.10812234303918));
#30698=CARTESIAN_POINT('Ctrl Pts',(-90.0190409350164,-26.7732812651581,
8.95013917779055));
#30699=CARTESIAN_POINT('Ctrl Pts',(-93.2399629504105,-27.1745153202148,
8.79215601254192));
#30700=CARTESIAN_POINT('Ctrl Pts',(-95.336189146788,-24.6964009801777,8.63417284729328));
#30701=CARTESIAN_POINT('Ctrl Pts',(-94.4063813923771,-21.5866049746754,
8.47618968204465));
#30702=CARTESIAN_POINT('Ctrl Pts',(-91.2939018778273,-20.665851504804,8.31820651679601));
#30703=CARTESIAN_POINT('Ctrl Pts',(-88.8218782942424,-22.7692791977076,
8.16022335154738));
#30704=CARTESIAN_POINT('Ctrl Pts',(-89.2325191657663,-25.9890152722711,
8.00224018629874));
#30705=CARTESIAN_POINT('Ctrl Pts',(-92.1533598138249,-27.4046453291175,
7.8442570210501));
#30706=CARTESIAN_POINT('Ctrl Pts',(-94.9350977784,-25.7321464895925,7.68627385580147));
#30707=CARTESIAN_POINT('Ctrl Pts',(-95.0546019246959,-22.4885313561187,
7.52829069055284));
#30708=CARTESIAN_POINT('Ctrl Pts',(-92.4034778417231,-20.6158700221474,
7.3703075253042));
#30709=CARTESIAN_POINT('Ctrl Pts',(-89.3863855962295,-21.8127300123327,
7.21232436005556));
#30710=CARTESIAN_POINT('Ctrl Pts',(-88.7399308175942,-24.9935185734687,
7.05434119480694));
#30711=CARTESIAN_POINT('Ctrl Pts',(-91.0504700633043,-27.2731518599606,
6.89635802955829));
#30712=CARTESIAN_POINT('Ctrl Pts',(-94.2222653697412,-26.5839246983912,
6.73837486430967));
#30713=CARTESIAN_POINT('Ctrl Pts',(-95.3783901358023,-23.5509896362749,
6.58039169906103));
#30714=CARTESIAN_POINT('Ctrl Pts',(-93.47019973667,-20.9253223018085,6.4224085338124));
#30715=CARTESIAN_POINT('Ctrl Pts',(-90.2284879954676,-21.0884925839313,
6.26442536856376));
#30716=CARTESIAN_POINT('Ctrl Pts',(-88.5935981078011,-23.8924994689134,
6.10644220331513));
#30717=CARTESIAN_POINT('Ctrl Pts',(-90.0484310041948,-26.794013004571,5.94845903806649));
#30718=CARTESIAN_POINT('Ctrl Pts',(-93.2734035910007,-27.1612613795506,
5.79047587281786));
#30719=CARTESIAN_POINT('Ctrl Pts',(-95.343355656779,-24.6611377825871,5.63249270756922));
#30720=CARTESIAN_POINT('Ctrl Pts',(-94.3807700259685,-21.561339650806,5.47450954232059));
#30721=CARTESIAN_POINT('Ctrl Pts',(-91.2587447208024,-20.6734896924144,
5.31652637707195));
#30722=CARTESIAN_POINT('Ctrl Pts',(-88.8090632545394,-22.8028981239801,
5.15854321182332));
#30723=CARTESIAN_POINT('Ctrl Pts',(-89.2536703298387,-26.0181188166585,
5.00056004657469));
#30724=CARTESIAN_POINT('Ctrl Pts',(-92.1892921542613,-27.4028368600861,
4.84257688132605));
#30725=CARTESIAN_POINT('Ctrl Pts',(-94.9532195334778,-25.7010657249343,
4.68459371607742));
#30726=CARTESIAN_POINT('Ctrl Pts',(-95.0384759968196,-22.4563699169912,
4.52661055082878));
#30727=CARTESIAN_POINT('Ctrl Pts',(-92.3677310199108,-20.6117992802222,
4.36862738558014));
#30728=CARTESIAN_POINT('Ctrl Pts',(-89.3634414594277,-21.8404423459467,
4.21064422033152));
#30729=CARTESIAN_POINT('Ctrl Pts',(-88.7506004806488,-25.0278779078958,
4.05266105508288));
#30730=CARTESIAN_POINT('Ctrl Pts',(-91.0850757871254,-27.2829931366426,
3.89467788983424));
#30731=CARTESIAN_POINT('Ctrl Pts',(-94.2494185580209,-26.5603215084426,
3.73669472458561));
#30732=CARTESIAN_POINT('Ctrl Pts',(-95.3734619703373,-23.5153509367788,
3.57871155933698));
#30733=CARTESIAN_POINT('Ctrl Pts',(-93.4376601278633,-20.9099734973745,
3.42072839408834));
#30734=CARTESIAN_POINT('Ctrl Pts',(-90.1978516918172,-21.1073557901305,
3.26274522883971));
#30735=CARTESIAN_POINT('Ctrl Pts',(-88.5926528478276,-23.9284646537609,
3.10476206359107));
#30736=CARTESIAN_POINT('Ctrl Pts',(-90.0780350586153,-26.8144594567857,
2.94677889834244));
#30737=CARTESIAN_POINT('Ctrl Pts',(-93.3067032590667,-27.1476415518445,
2.7887957330938));
#30738=CARTESIAN_POINT('Ctrl Pts',(-95.3501507055962,-24.6258092390124,
2.63081256784517));
#30739=CARTESIAN_POINT('Ctrl Pts',(-94.3548895523608,-21.5363385897164,
2.47282940259653));
#30740=CARTESIAN_POINT('Ctrl Pts',(-91.2236786416529,-20.6815092609376,
2.3148462373479));
#30741=CARTESIAN_POINT('Ctrl Pts',(-88.7965861590017,-22.8366309458653,
2.15686307209926));
#30742=CARTESIAN_POINT('Ctrl Pts',(-89.2751637872942,-26.0470361903507,
1.99887990685063));
#30743=CARTESIAN_POINT('Ctrl Pts',(-92.2251293032968,-27.4005706191735,
1.84089674160199));
#30744=CARTESIAN_POINT('Ctrl Pts',(-94.9711635487424,-25.6699555592398,
1.68291357635336));
#30745=CARTESIAN_POINT('Ctrl Pts',(-95.0217022824422,-22.4240534771338,
1.52493041110472));
#30746=CARTESIAN_POINT('Ctrl Pts',(-92.3325748270696,-20.6087741969446,
1.36694724585609));
#30747=CARTESIAN_POINT('Ctrl Pts',(-89.3394999866892,-21.8670182519308,
1.20896408060746));
#30748=CARTESIAN_POINT('Ctrl Pts',(-88.7643189008962,-25.0649591913859,
1.05098091535882));
#30749=CARTESIAN_POINT('Ctrl Pts',(-90.3308555140066,-26.5433639279422,
0.945658805193066));
#30750=CARTESIAN_POINT('Ctrl Pts',(-91.2540671456531,-26.7901775698422,
0.892997750110188));
#30751=CARTESIAN_POINT('Ctrl Pts',(-89.6639373423038,-22.0026984430694,
10.3210067496694));
#30752=CARTESIAN_POINT('Ctrl Pts',(-89.0030718657857,-22.7756529106096,
10.2683456945866));
#30753=CARTESIAN_POINT('Ctrl Pts',(-88.5204111561735,-25.0164835131759,
10.1630235844208));
#30754=CARTESIAN_POINT('Ctrl Pts',(-90.9525228428247,-27.4743146734751,
10.0050404191722));
#30755=CARTESIAN_POINT('Ctrl Pts',(-94.3358599455364,-26.7735796108866,
9.84705725392353));
#30756=CARTESIAN_POINT('Ctrl Pts',(-95.599950794029,-23.5606287345722,9.6890740886749));
#30757=CARTESIAN_POINT('Ctrl Pts',(-93.5990318095031,-20.7444872358932,
9.53109092342626));
#30758=CARTESIAN_POINT('Ctrl Pts',(-90.1476049582096,-20.8820466605266,
9.37310775817762));
#30759=CARTESIAN_POINT('Ctrl Pts',(-88.3764280027803,-23.8472850428361,
9.21512459292899));
#30760=CARTESIAN_POINT('Ctrl Pts',(-89.8919230124438,-26.9512424150719,
9.05714142768036));
#30761=CARTESIAN_POINT('Ctrl Pts',(-93.3195312348388,-27.3782236147545,
8.89915826243172));
#30762=CARTESIAN_POINT('Ctrl Pts',(-95.5502720327727,-24.7410889535148,
8.74117509718309));
#30763=CARTESIAN_POINT('Ctrl Pts',(-94.5607986183176,-21.4317376846898,
8.58319193193445));
#30764=CARTESIAN_POINT('Ctrl Pts',(-91.2485916399685,-20.4518995672047,
8.42520876668582));
#30765=CARTESIAN_POINT('Ctrl Pts',(-88.6179385783441,-22.6903039808949,
8.26722560143718));
#30766=CARTESIAN_POINT('Ctrl Pts',(-89.0549302288588,-26.1166501607681,
8.10924243618856));
#30767=CARTESIAN_POINT('Ctrl Pts',(-92.1632008959979,-27.623121040698,7.95125927093991));
#30768=CARTESIAN_POINT('Ctrl Pts',(-95.1234426759463,-25.8432981369136,
7.79327610569129));
#30769=CARTESIAN_POINT('Ctrl Pts',(-95.2506153900005,-22.3915405815791,
7.63529294044264));
#30770=CARTESIAN_POINT('Ctrl Pts',(-92.4293689698895,-20.3987107783727,
7.47730977519402));
#30771=CARTESIAN_POINT('Ctrl Pts',(-89.2186702510282,-21.6723731408291,
7.31932660994537));
#30772=CARTESIAN_POINT('Ctrl Pts',(-88.5307325412461,-25.0572725496761,
7.16134344469675));
#30773=CARTESIAN_POINT('Ctrl Pts',(-90.9895388330194,-27.4831896502702,
7.0033602794481));
#30774=CARTESIAN_POINT('Ctrl Pts',(-94.364867891015,-26.749734858505,6.84537711419948));
#30775=CARTESIAN_POINT('Ctrl Pts',(-95.5951810545519,-23.5221766912428,
6.68739394895083));
#30776=CARTESIAN_POINT('Ctrl Pts',(-93.5645422900301,-20.7280205763547,
6.52941078370221));
#30777=CARTESIAN_POINT('Ctrl Pts',(-90.1148102674372,-20.9016614773084,
6.37142761845357));
#30778=CARTESIAN_POINT('Ctrl Pts',(-88.3750096777633,-23.8856011718064,
6.21344445320494));
#30779=CARTESIAN_POINT('Ctrl Pts',(-89.9231990390881,-26.973304507894,6.0554612879563));
#30780=CARTESIAN_POINT('Ctrl Pts',(-93.3551177576112,-27.364119170194,5.89747812270767));
#30781=CARTESIAN_POINT('Ctrl Pts',(-95.5578984169116,-24.7035629204622,
5.73949495745903));
#30782=CARTESIAN_POINT('Ctrl Pts',(-94.5335437733791,-21.4048510878016,
5.5815117922104));
#30783=CARTESIAN_POINT('Ctrl Pts',(-91.2111784520928,-20.4600278964634,
5.42352862696177));
#30784=CARTESIAN_POINT('Ctrl Pts',(-88.6043011989707,-22.7260802299219,
5.26554546171313));
#30785=CARTESIAN_POINT('Ctrl Pts',(-89.0774386607742,-26.1476212763575,
5.1075622964645));
#30786=CARTESIAN_POINT('Ctrl Pts',(-92.201439010718,-27.6211965224103,4.94957913121586));
#30787=CARTESIAN_POINT('Ctrl Pts',(-95.1427273020293,-25.8102229230488,
4.79159596596723));
#30788=CARTESIAN_POINT('Ctrl Pts',(-95.2334546631283,-22.3573153464848,
4.63361280071859));
#30789=CARTESIAN_POINT('Ctrl Pts',(-92.3913282785029,-20.3943788173916,
4.47562963546995));
#30790=CARTESIAN_POINT('Ctrl Pts',(-89.1942537915232,-21.7018637718047,
4.31764647022133));
#30791=CARTESIAN_POINT('Ctrl Pts',(-88.5420868753907,-25.0938367187666,
4.15966330497269));
#30792=CARTESIAN_POINT('Ctrl Pts',(-91.0263652022841,-27.4936624405808,
4.00168013972406));
#30793=CARTESIAN_POINT('Ctrl Pts',(-94.3937634963622,-26.7246170544862,
3.84369697447542));
#30794=CARTESIAN_POINT('Ctrl Pts',(-95.589936649258,-23.4842510603692,3.68571380922678));
#30795=CARTESIAN_POINT('Ctrl Pts',(-93.5299146181504,-20.7116868408496,
3.52773064397815));
#30796=CARTESIAN_POINT('Ctrl Pts',(-90.0822080355936,-20.9217351333484,
3.36974747872952));
#30797=CARTESIAN_POINT('Ctrl Pts',(-88.3740037605625,-23.92387423856,3.21176431348088));
#30798=CARTESIAN_POINT('Ctrl Pts',(-89.9547027823836,-26.99506300667,3.05378114823225));
#30799=CARTESIAN_POINT('Ctrl Pts',(-93.3905542616683,-27.349625359661,2.89579798298362));
#30800=CARTESIAN_POINT('Ctrl Pts',(-95.5651295032547,-24.6659673481809,
2.73781481773498));
#30801=CARTESIAN_POINT('Ctrl Pts',(-94.5060025526623,-21.3782457114063,
2.57983165248635));
#30802=CARTESIAN_POINT('Ctrl Pts',(-91.1738621865499,-20.4685620798055,
2.42184848723771));
#30803=CARTESIAN_POINT('Ctrl Pts',(-88.5910234496018,-22.7619776832305,
2.26386532198907));
#30804=CARTESIAN_POINT('Ctrl Pts',(-89.1003113510008,-26.1783942746989,
2.10588215674044));
#30805=CARTESIAN_POINT('Ctrl Pts',(-92.2395758256157,-27.6187848570707,
1.94789899149181));
#30806=CARTESIAN_POINT('Ctrl Pts',(-95.1618227827549,-25.7771164214866,
1.78991582624317));
#30807=CARTESIAN_POINT('Ctrl Pts',(-95.2156045813675,-22.3229251642809,
1.63193266099454));
#30808=CARTESIAN_POINT('Ctrl Pts',(-92.3539161166825,-20.3911596148569,
1.4739494957459));
#30809=CARTESIAN_POINT('Ctrl Pts',(-89.1687759971456,-21.7301450507159,
1.31596633049727));
#30810=CARTESIAN_POINT('Ctrl Pts',(-88.5566856051374,-25.1332975040883,
1.15798316524863));
#30811=CARTESIAN_POINT('Ctrl Pts',(-90.2237466982397,-26.7065713079336,
1.05266105508288));
#30812=CARTESIAN_POINT('Ctrl Pts',(-91.2062007174672,-26.9692229537457,
0.999999999999999));
#30813=CARTESIAN_POINT('Ctrl Pts',(-90.0865340033349,-22.3640127966251,
10.));
#30814=CARTESIAN_POINT('Ctrl Pts',(-90.0249229041799,-22.4219121010796,
10.));
#30815=CARTESIAN_POINT('Ctrl Pts',(-89.9666809070904,-22.4829619660083,
10.));
#30816=CARTESIAN_POINT('Ctrl Pts',(-89.9118056829848,-22.546777615348,10.));
#30817=CARTESIAN_POINT('Ctrl Pts',(-89.8554777542744,-22.6122826479962,
10.));
#30818=CARTESIAN_POINT('Ctrl Pts',(-89.8026967773227,-22.6807022716026,
10.));
#30819=CARTESIAN_POINT('Ctrl Pts',(-89.753485740358,-22.7516688868598,10.));
#30820=CARTESIAN_POINT('Ctrl Pts',(-89.7029132366753,-22.8245988560865,
10.));
#30821=CARTESIAN_POINT('Ctrl Pts',(-89.6561104020014,-22.9002192512329,
10.));
#30822=CARTESIAN_POINT('Ctrl Pts',(-89.6131362838785,-22.9781741250528,
10.));
#30823=CARTESIAN_POINT('Ctrl Pts',(-89.5942448480481,-23.0124431120793,
10.));
#30824=CARTESIAN_POINT('Ctrl Pts',(-89.5760937898788,-23.0471637309785,
10.));
#30825=CARTESIAN_POINT('Ctrl Pts',(-89.5586905433103,-23.0823078140373,
10.));
#30826=CARTESIAN_POINT('Ctrl Pts',(-89.5487655216206,-23.1023503839827,
10.));
#30827=CARTESIAN_POINT('Ctrl Pts',(-89.539083745551,-23.1225307016013,10.));
#30828=CARTESIAN_POINT('Ctrl Pts',(-89.5296468276356,-23.1428436902047,
10.));
#30829=CARTESIAN_POINT('Ctrl Pts',(-89.521129801935,-23.1611766085942,10.));
#30830=CARTESIAN_POINT('Ctrl Pts',(-89.512809840989,-23.1796233419582,10.));
#30831=CARTESIAN_POINT('Ctrl Pts',(-89.504701824908,-23.1981483273657,10.));
#30832=CARTESIAN_POINT('Ctrl Pts',(-89.4681370588538,-23.2816905590052,
10.));
#30833=CARTESIAN_POINT('Ctrl Pts',(-89.4358326118623,-23.3669162866866,
10.));
#30834=CARTESIAN_POINT('Ctrl Pts',(-89.4078135857242,-23.4534267953981,
10.));
#30835=CARTESIAN_POINT('Ctrl Pts',(-89.3793318743352,-23.5413658739758,
10.));
#30836=CARTESIAN_POINT('Ctrl Pts',(-89.3552777914497,-23.6306332708035,
10.));
#30837=CARTESIAN_POINT('Ctrl Pts',(-89.3357167786194,-23.7208473130613,
10.));
#30838=CARTESIAN_POINT('Ctrl Pts',(-89.316736346674,-23.8083837563144,10.));
#30839=CARTESIAN_POINT('Ctrl Pts',(-89.301986069027,-23.8968124020132,10.));
#30840=CARTESIAN_POINT('Ctrl Pts',(-89.2915665512199,-23.9858064657529,
10.));
#30841=CARTESIAN_POINT('Ctrl Pts',(-89.2872071979636,-24.0230401044627,
10.));
#30842=CARTESIAN_POINT('Ctrl Pts',(-89.2836064360708,-24.0603729082217,
10.));
#30843=CARTESIAN_POINT('Ctrl Pts',(-89.2807739547576,-24.0977815591893,
10.));
#30844=CARTESIAN_POINT('Ctrl Pts',(-89.2790033727378,-24.1211656798468,
10.));
#30845=CARTESIAN_POINT('Ctrl Pts',(-89.2775330236662,-24.1445794431293,
10.));
#30846=CARTESIAN_POINT('Ctrl Pts',(-89.2763655644993,-24.1680171857739,
10.));
#30847=CARTESIAN_POINT('Ctrl Pts',(-89.275681297243,-24.181754436983,10.));
#30848=CARTESIAN_POINT('Ctrl Pts',(-89.2751013563383,-24.1954953573145,
10.));
#30849=CARTESIAN_POINT('Ctrl Pts',(-89.2746262639892,-24.2092305722781,
10.));
#30850=CARTESIAN_POINT('Ctrl Pts',(-89.2712684324413,-24.3063075683927,
10.));
#30851=CARTESIAN_POINT('Ctrl Pts',(-89.2731377894335,-24.4032200225579,
10.));
#30852=CARTESIAN_POINT('Ctrl Pts',(-89.2802991313706,-24.4995456759757,
10.));
#30853=CARTESIAN_POINT('Ctrl Pts',(-89.2874604733076,-24.5958713293936,
10.));
#30854=CARTESIAN_POINT('Ctrl Pts',(-89.2999133653215,-24.6916112365764,
10.));
#30855=CARTESIAN_POINT('Ctrl Pts',(-89.3177754963829,-24.7863620775548,
10.));
#30856=CARTESIAN_POINT('Ctrl Pts',(-89.3348530128177,-24.8769508789953,
10.));
#30857=CARTESIAN_POINT('Ctrl Pts',(-89.3568748775387,-24.9666365695192,
10.));
#30858=CARTESIAN_POINT('Ctrl Pts',(-89.383566394629,-25.0551798098077,10.));
#30859=CARTESIAN_POINT('Ctrl Pts',(-89.3925012626259,-25.0848192702146,
10.));
#30860=CARTESIAN_POINT('Ctrl Pts',(-89.4019598223816,-25.1143306773261,
10.));
#30861=CARTESIAN_POINT('Ctrl Pts',(-89.4119330456345,-25.1437048746548,
10.));
#30862=CARTESIAN_POINT('Ctrl Pts',(-89.4184142793766,-25.1627940932605,
10.));
#30863=CARTESIAN_POINT('Ctrl Pts',(-89.425112879774,-25.1818253626315,10.));
#30864=CARTESIAN_POINT('Ctrl Pts',(-89.4320265054004,-25.2007961347361,
10.));
#30865=CARTESIAN_POINT('Ctrl Pts',(-89.4386160834063,-25.218877730323,10.));
#30866=CARTESIAN_POINT('Ctrl Pts',(-89.4454027538168,-25.2369085767948,
10.));
#30867=CARTESIAN_POINT('Ctrl Pts',(-89.4523736969164,-25.254859317182,10.));
#30868=CARTESIAN_POINT('Ctrl Pts',(-89.4862171782651,-25.342009009671,10.));
#30869=CARTESIAN_POINT('Ctrl Pts',(-89.524439002612,-25.4273844054574,10.));
#30870=CARTESIAN_POINT('Ctrl Pts',(-89.5667079861147,-25.5107518898734,
10.));
#30871=CARTESIAN_POINT('Ctrl Pts',(-89.6105462295904,-25.5972144394055,
10.));
#30872=CARTESIAN_POINT('Ctrl Pts',(-89.6587378392776,-25.6815179448506,
10.));
#30873=CARTESIAN_POINT('Ctrl Pts',(-89.7109693334073,-25.763398787929,10.));
#30874=CARTESIAN_POINT('Ctrl Pts',(-89.7637892526335,-25.846202077202,10.));
#30875=CARTESIAN_POINT('Ctrl Pts',(-89.8207410024605,-25.9265286303401,
10.));
#30876=CARTESIAN_POINT('Ctrl Pts',(-89.8815521717527,-26.004090973277,10.));
#30877=CARTESIAN_POINT('Ctrl Pts',(-89.923214641541,-26.0572298753393,10.));
#30878=CARTESIAN_POINT('Ctrl Pts',(-89.9666897223643,-26.1090710102662,
10.));
#30879=CARTESIAN_POINT('Ctrl Pts',(-90.011902026058,-26.1595148904434,10.));
#30880=CARTESIAN_POINT('Ctrl Pts',(-90.0240091589916,-26.1730229560162,
10.));
#30881=CARTESIAN_POINT('Ctrl Pts',(-90.0362421971691,-26.1864320425439,
10.));
#30882=CARTESIAN_POINT('Ctrl Pts',(-90.0485860743795,-26.1997257420871,
10.));
#30883=CARTESIAN_POINT('Ctrl Pts',(-90.1172469210647,-26.2736698238907,
10.));
#30884=CARTESIAN_POINT('Ctrl Pts',(-90.1894216590749,-26.3441460197638,
10.));
#30885=CARTESIAN_POINT('Ctrl Pts',(-90.2647998274612,-26.410864519058,10.));
#30886=CARTESIAN_POINT('Ctrl Pts',(-90.3277047217017,-26.4665427111901,
10.));
#30887=CARTESIAN_POINT('Ctrl Pts',(-90.3928416636536,-26.5196039171212,
10.));
#30888=CARTESIAN_POINT('Ctrl Pts',(-90.4600538825085,-26.569865931641,10.));
#30889=CARTESIAN_POINT('Ctrl Pts',(-90.4819361594316,-26.5862297318424,
10.));
#30890=CARTESIAN_POINT('Ctrl Pts',(-90.5040385610053,-26.6022967069767,
10.));
#30891=CARTESIAN_POINT('Ctrl Pts',(-90.5263561031203,-26.6180601837049,
10.));
#30892=CARTESIAN_POINT('Ctrl Pts',(-90.5491249077408,-26.6341423992068,
10.));
#30893=CARTESIAN_POINT('Ctrl Pts',(-90.5721230553218,-26.6499121465391,
10.));
#30894=CARTESIAN_POINT('Ctrl Pts',(-90.5953161168769,-26.6653431122229,
10.));
#30895=CARTESIAN_POINT('Ctrl Pts',(-90.680261445699,-26.7218595169649,10.));
#30896=CARTESIAN_POINT('Ctrl Pts',(-90.7678730457073,-26.7738754900865,
10.));
#30897=CARTESIAN_POINT('Ctrl Pts',(-90.8578606519112,-26.8210829660107,
10.));
#30898=CARTESIAN_POINT('Ctrl Pts',(-90.9411342810838,-26.8647682912474,
10.));
#30899=CARTESIAN_POINT('Ctrl Pts',(-91.0264434122842,-26.9043361313708,
10.));
#30900=CARTESIAN_POINT('Ctrl Pts',(-91.1135854408295,-26.9395135107767,
10.));
#30901=CARTESIAN_POINT('Ctrl Pts',(-91.1436093918511,-26.9516335398141,
10.));
#30902=CARTESIAN_POINT('Ctrl Pts',(-91.173851123563,-26.9632321026033,10.));
#30903=CARTESIAN_POINT('Ctrl Pts',(-91.2042982523172,-26.9743127795766,
10.));
#30904=CARTESIAN_POINT('Ctrl Pts',(-94.5182106813093,-24.0021944371302,
8.38741669750803));
#30905=CARTESIAN_POINT('Ctrl Pts',(-94.5197766683662,-24.1747250448626,
8.39833391417657));
#30906=CARTESIAN_POINT('Ctrl Pts',(-94.5035406983691,-24.3469627335709,
8.40925113084511));
#30907=CARTESIAN_POINT('Ctrl Pts',(-94.4684111368875,-24.5152564032994,
8.42016834751366));
#30908=CARTESIAN_POINT('Ctrl Pts',(-94.2989577103971,-25.3270495993809,
8.47282940259654));
#30909=CARTESIAN_POINT('Ctrl Pts',(-93.6898920459757,-26.0470741652581,
8.52549045767941));
#30910=CARTESIAN_POINT('Ctrl Pts',(-92.9174342801995,-26.3487964872292,
8.57815151276229));
#30911=CARTESIAN_POINT('Ctrl Pts',(-92.1449765144234,-26.6505188092004,
8.63081256784517));
#30912=CARTESIAN_POINT('Ctrl Pts',(-91.2091266472926,-26.5339388872655,
8.68347362292805));
#30913=CARTESIAN_POINT('Ctrl Pts',(-90.5343117030538,-26.0519076603903,
8.73613467801093));
#30914=CARTESIAN_POINT('Ctrl Pts',(-89.859496758815,-25.5698764335152,8.7887957330938));
#30915=CARTESIAN_POINT('Ctrl Pts',(-89.4457167374682,-24.7223939016998,
8.84145678817668));
#30916=CARTESIAN_POINT('Ctrl Pts',(-89.4806215310513,-23.8938487950316,
8.89411784325956));
#30917=CARTESIAN_POINT('Ctrl Pts',(-89.5155263246344,-23.0653036883635,
8.94677889834244));
#30918=CARTESIAN_POINT('Ctrl Pts',(-89.9991159331473,-22.2556960068425,
8.99943995342531));
#30919=CARTESIAN_POINT('Ctrl Pts',(-90.7120873058182,-21.8321130406813,
9.05210100850819));
#30920=CARTESIAN_POINT('Ctrl Pts',(-91.4250586784891,-21.4085300745201,
9.10476206359107));
#30921=CARTESIAN_POINT('Ctrl Pts',(-92.3674118153181,-21.3709718237187,
9.15742311867395));
#30922=CARTESIAN_POINT('Ctrl Pts',(-93.1117467560304,-21.7366423606423,
9.21008417375683));
#30923=CARTESIAN_POINT('Ctrl Pts',(-93.8560816967427,-22.102312897566,9.26274522883971));
#30924=CARTESIAN_POINT('Ctrl Pts',(-94.4023984413383,-22.8712122222148,
9.31540628392259));
#30925=CARTESIAN_POINT('Ctrl Pts',(-94.5029876085453,-23.6942825575571,
9.36806733900547));
#30926=CARTESIAN_POINT('Ctrl Pts',(-94.5153075025967,-23.7950900262915,
9.37451712517299));
#30927=CARTESIAN_POINT('Ctrl Pts',(-94.520941171052,-23.8967100980969,9.38096691134051));
#30928=CARTESIAN_POINT('Ctrl Pts',(-94.5201759878003,-23.9984131478585,
9.38741669750803));
#30929=CARTESIAN_POINT('Ctrl Pts',(-92.7937992825329,-26.9692229537457,
10.));
#30930=CARTESIAN_POINT('Ctrl Pts',(-93.7762533017603,-26.7065713079336,
9.94733894491712));
#30931=CARTESIAN_POINT('Ctrl Pts',(-95.4433142859563,-25.1332967687399,
9.84201683475136));
#30932=CARTESIAN_POINT('Ctrl Pts',(-94.8312240969781,-21.7301452717063,
9.68403366950273));
#30933=CARTESIAN_POINT('Ctrl Pts',(-91.6460838755241,-20.3911593875009,
9.5260505042541));
#30934=CARTESIAN_POINT('Ctrl Pts',(-88.7843953448966,-22.3229252160129,
9.36806733900546));
#30935=CARTESIAN_POINT('Ctrl Pts',(-88.8381771631846,-25.7771164103053,
9.21008417375683));
#30936=CARTESIAN_POINT('Ctrl Pts',(-91.7604241627304,-27.6187849549088,
9.05210100850819));
#30937=CARTESIAN_POINT('Ctrl Pts',(-94.8996887115742,-26.1783943047283,
8.89411784325956));
#30938=CARTESIAN_POINT('Ctrl Pts',(-95.4089766159342,-22.7619776656796,
8.73613467801093));
#30939=CARTESIAN_POINT('Ctrl Pts',(-92.8261378316182,-20.4685620052276,
8.57815151276229));
#30940=CARTESIAN_POINT('Ctrl Pts',(-89.493997396212,-21.3782456609066,8.42016834751365));
#30941=CARTESIAN_POINT('Ctrl Pts',(-88.4348704258472,-24.6659673604642,
8.26218518226502));
#30942=CARTESIAN_POINT('Ctrl Pts',(-90.6094457101907,-27.3496254273118,
8.10420201701639));
#30943=CARTESIAN_POINT('Ctrl Pts',(-94.045297258743,-26.9950630663804,7.94621885176775));
#30944=CARTESIAN_POINT('Ctrl Pts',(-95.6259963119894,-23.9238742371833,
7.78823568651911));
#30945=CARTESIAN_POINT('Ctrl Pts',(-93.9177920028682,-20.9217350716083,
7.63025252127049));
#30946=CARTESIAN_POINT('Ctrl Pts',(-90.4700853511787,-20.7116867750179,
7.47226935602185));
#30947=CARTESIAN_POINT('Ctrl Pts',(-88.4100632788413,-23.4842510500175,
7.31428619077322));
#30948=CARTESIAN_POINT('Ctrl Pts',(-89.6062364556796,-26.7246171090759,
7.15630302552458));
#30949=CARTESIAN_POINT('Ctrl Pts',(-92.9736348172232,-27.4936625105602,
6.99831986027594));
#30950=CARTESIAN_POINT('Ctrl Pts',(-95.4579131938762,-25.0938367406809,
6.84033669502731));
#30951=CARTESIAN_POINT('Ctrl Pts',(-94.805746264682,-21.7018637257672,6.68235352977868));
#30952=CARTESIAN_POINT('Ctrl Pts',(-91.6086717136577,-20.3943787451648,
6.52437036453004));
#30953=CARTESIAN_POINT('Ctrl Pts',(-88.7665452720996,-22.3573153135784,
6.36638719928141));
#30954=CARTESIAN_POINT('Ctrl Pts',(-88.8572726350159,-25.8102229593112,
6.20840403403277));
#30955=CARTESIAN_POINT('Ctrl Pts',(-91.7985609852469,-27.6211965949497,
6.05042086878414));
#30956=CARTESIAN_POINT('Ctrl Pts',(-94.9225613977702,-26.1476213193785,
5.8924377035355));
#30957=CARTESIAN_POINT('Ctrl Pts',(-95.3956988690517,-22.7260802044028,
5.73445453828687));
#30958=CARTESIAN_POINT('Ctrl Pts',(-92.7888215637087,-20.460027825551,5.57647137303824));
#30959=CARTESIAN_POINT('Ctrl Pts',(-89.4664561758693,-21.4048510358159,
5.4184882077896));
#30960=CARTESIAN_POINT('Ctrl Pts',(-88.4421015118167,-24.7035629345559,
5.26050504254097));
#30961=CARTESIAN_POINT('Ctrl Pts',(-90.6448822152433,-27.3641192375838,
5.10252187729233));
#30962=CARTESIAN_POINT('Ctrl Pts',(-94.0768010025145,-26.9733045674549,
4.9445387120437));
#30963=CARTESIAN_POINT('Ctrl Pts',(-95.6249903948519,-23.8856011695146,
4.78655554679506));
#30964=CARTESIAN_POINT('Ctrl Pts',(-93.885189770327,-20.9016614152429,4.62857238154643));
#30965=CARTESIAN_POINT('Ctrl Pts',(-90.435457678629,-20.7280205108105,4.47058921629779));
#30966=CARTESIAN_POINT('Ctrl Pts',(-88.4048188734298,-23.5221766816715,
4.31260605104916));
#30967=CARTESIAN_POINT('Ctrl Pts',(-89.6351320616122,-26.7497349135866,
4.15462288580052));
#30968=CARTESIAN_POINT('Ctrl Pts',(-93.0104611872221,-27.4831897200468,
3.99663972055189));
#30969=CARTESIAN_POINT('Ctrl Pts',(-95.4692675282499,-25.0572725708519,
3.83865655530325));
#30970=CARTESIAN_POINT('Ctrl Pts',(-94.7813298046868,-21.6723730942086,
3.68067339005462));
#30971=CARTESIAN_POINT('Ctrl Pts',(-91.5706310215098,-20.3987107062197,
3.52269022480599));
#30972=CARTESIAN_POINT('Ctrl Pts',(-88.7493845448822,-22.3915405493825,
3.36470705955735));
#30973=CARTESIAN_POINT('Ctrl Pts',(-88.8765572614881,-25.8432981737925,
3.20672389430872));
#30974=CARTESIAN_POINT('Ctrl Pts',(-91.8367991007263,-27.6231211133645,
3.04874072906008));
#30975=CARTESIAN_POINT('Ctrl Pts',(-94.9450698301517,-26.1166502029989,
2.89075756381145));
#30976=CARTESIAN_POINT('Ctrl Pts',(-95.3820614893708,-22.6903039549832,
2.73277439856281));
#30977=CARTESIAN_POINT('Ctrl Pts',(-92.7514083751607,-20.4518994955132,
2.57479123331418));
#30978=CARTESIAN_POINT('Ctrl Pts',(-89.4392013302128,-21.4317376344076,
2.41680806806554));
#30979=CARTESIAN_POINT('Ctrl Pts',(-88.4497278964895,-24.7410889661721,
2.25882490281691));
#30980=CARTESIAN_POINT('Ctrl Pts',(-90.6804687378896,-27.3782236865054,
2.10084173756828));
#30981=CARTESIAN_POINT('Ctrl Pts',(-94.1080770316232,-26.9512424666579,
1.94285857231964));
#30982=CARTESIAN_POINT('Ctrl Pts',(-95.6235720657977,-23.8472850535338,
1.78487540707101));
#30983=CARTESIAN_POINT('Ctrl Pts',(-93.8523950876059,-20.8820465732966,
1.62689224182237));
#30984=CARTESIAN_POINT('Ctrl Pts',(-90.400968139612,-20.7444872144857,1.46890907657374));
#30985=CARTESIAN_POINT('Ctrl Pts',(-88.4000491745082,-23.5606286501727,
1.31092591132511));
#30986=CARTESIAN_POINT('Ctrl Pts',(-89.6641399192572,-26.7735797938367,
1.15294274607647));
#30987=CARTESIAN_POINT('Ctrl Pts',(-93.0474773599211,-27.4743145446721,
0.994959580827837));
#30988=CARTESIAN_POINT('Ctrl Pts',(-95.4795883375448,-25.0164840574889,
0.8369764155792));
#30989=CARTESIAN_POINT('Ctrl Pts',(-94.9969281342143,-22.7756529106095,
0.731654305413444));
#30990=CARTESIAN_POINT('Ctrl Pts',(-94.3360626576961,-22.0026984430693,
0.678993250330566));
#30991=CARTESIAN_POINT('Ctrl Pts',(-92.7459328543469,-26.7901775698421,
10.1070022498898));
#30992=CARTESIAN_POINT('Ctrl Pts',(-93.6691444859934,-26.5433639279422,
10.0543411948069));
#30993=CARTESIAN_POINT('Ctrl Pts',(-95.2356809967647,-25.0649585003793,
9.94901908464118));
#30994=CARTESIAN_POINT('Ctrl Pts',(-94.6605001017588,-21.8670184595954,
9.79103591939254));
#30995=CARTESIAN_POINT('Ctrl Pts',(-91.667425165607,-20.6087739832983,9.63305275414391));
#30996=CARTESIAN_POINT('Ctrl Pts',(-88.9782976482681,-22.4240535257463,
9.47506958889527));
#30997=CARTESIAN_POINT('Ctrl Pts',(-89.0288364004571,-25.6699555487328,
9.31708642364664));
#30998=CARTESIAN_POINT('Ctrl Pts',(-91.774870685752,-27.4005707111119,9.159103258398));
#30999=CARTESIAN_POINT('Ctrl Pts',(-94.7248362715076,-26.0470362185693,
9.00112009314937));
#31000=CARTESIAN_POINT('Ctrl Pts',(-95.2034139025824,-22.8366309293727,
8.84313692790074));
#31001=CARTESIAN_POINT('Ctrl Pts',(-92.7763213754197,-20.6815091908568,
8.6851537626521));
#31002=CARTESIAN_POINT('Ctrl Pts',(-89.6451103995963,-21.5363385422618,
8.52717059740347));
#31003=CARTESIAN_POINT('Ctrl Pts',(-88.6498492277809,-24.625809250555,8.36918743215482));
#31004=CARTESIAN_POINT('Ctrl Pts',(-90.6932967144891,-27.147641615416,8.21120426690621));
#31005=CARTESIAN_POINT('Ctrl Pts',(-93.9219649800314,-26.8144595128955,
8.05322110165755));
#31006=CARTESIAN_POINT('Ctrl Pts',(-95.4073472203493,-23.9284646524673,
7.89523793640893));
#31007=CARTESIAN_POINT('Ctrl Pts',(-93.8021483443254,-21.1073557321132,
7.73725477116029));
#31008=CARTESIAN_POINT('Ctrl Pts',(-90.5623398433152,-20.9099734355125,
7.57927160591166));
#31009=CARTESIAN_POINT('Ctrl Pts',(-88.6265379620975,-23.5153509270513,
7.42128844066302));
#31010=CARTESIAN_POINT('Ctrl Pts',(-89.7505813969129,-26.5603215597406,
7.26330527541439));
#31011=CARTESIAN_POINT('Ctrl Pts',(-92.9149242312055,-27.2829932024021,
7.10532211016575));
#31012=CARTESIAN_POINT('Ctrl Pts',(-95.2493995844411,-25.0278779284887,
6.94733894491713));
#31013=CARTESIAN_POINT('Ctrl Pts',(-94.6365585933884,-21.8404423026853,
6.78935577966848));
#31014=CARTESIAN_POINT('Ctrl Pts',(-91.6322689727223,-20.6117992123508,
6.63137261441986));
#31015=CARTESIAN_POINT('Ctrl Pts',(-88.9615239423142,-22.4563698860691,
6.47338944917121));
#31016=CARTESIAN_POINT('Ctrl Pts',(-89.0467804073635,-25.7010657590101,
6.31540628392258));
#31017=CARTESIAN_POINT('Ctrl Pts',(-91.8107078419469,-27.4028369282513,
6.15742311867395));
#31018=CARTESIAN_POINT('Ctrl Pts',(-94.7463297251755,-26.0181188570852,
5.99943995342532));
#31019=CARTESIAN_POINT('Ctrl Pts',(-95.190936809381,-22.8028980999998,5.84145678817668));
#31020=CARTESIAN_POINT('Ctrl Pts',(-92.7412552940464,-20.6734896257781,
5.68347362292805));
#31021=CARTESIAN_POINT('Ctrl Pts',(-89.6192299263401,-21.561339601955,5.52549045767941));
#31022=CARTESIAN_POINT('Ctrl Pts',(-88.6566442762471,-24.661137795831,5.36750729243077));
#31023=CARTESIAN_POINT('Ctrl Pts',(-90.7265963834906,-27.1612614428767,
5.20952412718214));
#31024=CARTESIAN_POINT('Ctrl Pts',(-93.951569034899,-26.7940130605404,5.05154096193351));
#31025=CARTESIAN_POINT('Ctrl Pts',(-95.4064019604354,-23.8924994667599,
4.89355779668487));
#31026=CARTESIAN_POINT('Ctrl Pts',(-93.7715120400194,-21.0884925256084,
4.73557463143624));
#31027=CARTESIAN_POINT('Ctrl Pts',(-90.5298002338789,-20.9253222402166,
4.5775914661876));
#31028=CARTESIAN_POINT('Ctrl Pts',(-88.6216097965222,-23.5509896272809,
4.41960830093897));
#31029=CARTESIAN_POINT('Ctrl Pts',(-89.7777345857426,-26.5839247501514,
4.26162513569034));
#31030=CARTESIAN_POINT('Ctrl Pts',(-92.9495299557167,-27.2731519255296,
4.1036419704417));
#31031=CARTESIAN_POINT('Ctrl Pts',(-95.2600692477113,-24.9935185933677,
3.94565880519306));
#31032=CARTESIAN_POINT('Ctrl Pts',(-94.6136144561259,-21.8127299685234,
3.78767563994443));
#31033=CARTESIAN_POINT('Ctrl Pts',(-91.5965221501949,-20.6158699543453,
3.6296924746958));
#31034=CARTESIAN_POINT('Ctrl Pts',(-88.9453980141133,-22.4885313258635,
3.47170930944716));
#31035=CARTESIAN_POINT('Ctrl Pts',(-89.0649021628072,-25.7321465242476,
3.31372614419853));
#31036=CARTESIAN_POINT('Ctrl Pts',(-91.8466401830968,-27.4046453974022,
3.1557429789499));
#31037=CARTESIAN_POINT('Ctrl Pts',(-94.7674808896859,-25.9890153119553,
2.99775981370126));
#31038=CARTESIAN_POINT('Ctrl Pts',(-95.1781217693893,-22.7692791733585,
2.83977664845263));
#31039=CARTESIAN_POINT('Ctrl Pts',(-92.7060981363895,-20.6658514374356,
2.68179348320399));
#31040=CARTESIAN_POINT('Ctrl Pts',(-89.5936185592569,-21.5866049274252,
2.52381031795536));
#31041=CARTESIAN_POINT('Ctrl Pts',(-88.6638107867397,-24.6964009920718,
2.36582715270672));
#31042=CARTESIAN_POINT('Ctrl Pts',(-90.7600370239624,-27.1745153876391,
2.20784398745809));
#31043=CARTESIAN_POINT('Ctrl Pts',(-93.9809591063932,-26.7732813136335,
2.04986082220945));
#31044=CARTESIAN_POINT('Ctrl Pts',(-95.4050691572154,-23.8564938285714,
1.89187765696082));
#31045=CARTESIAN_POINT('Ctrl Pts',(-93.7406948903597,-21.0700604668217,
1.73389449171218));
#31046=CARTESIAN_POINT('Ctrl Pts',(-90.4973904284657,-20.9407959947845,
1.57591132646355));
#31047=CARTESIAN_POINT('Ctrl Pts',(-88.6171277124372,-23.5871229260259,
1.41792816121492));
#31048=CARTESIAN_POINT('Ctrl Pts',(-89.8049932574594,-26.6063317741661,
1.25994499596628));
#31049=CARTESIAN_POINT('Ctrl Pts',(-92.9843140377459,-27.2648119269358,
1.10196183071765));
#31050=CARTESIAN_POINT('Ctrl Pts',(-95.2697677078962,-24.9551896443915,
0.943978665469012));
#31051=CARTESIAN_POINT('Ctrl Pts',(-94.8162121163602,-22.8494815513233,
0.838656555303255));
#31052=CARTESIAN_POINT('Ctrl Pts',(-94.1951971040191,-22.1231365609212,
0.785995500220377));
#31053=CARTESIAN_POINT('Ctrl Pts',(-92.698066426161,-26.6111321859386,10.2140044997796));
#31054=CARTESIAN_POINT('Ctrl Pts',(-93.5620356702265,-26.3801565479507,
10.1613434446967));
#31055=CARTESIAN_POINT('Ctrl Pts',(-95.028047707573,-24.9966202320186,10.056021334531));
#31056=CARTESIAN_POINT('Ctrl Pts',(-94.4897761065395,-22.0038916474845,
9.89803816928235));
#31057=CARTESIAN_POINT('Ctrl Pts',(-91.6887664556897,-20.8263885790956,
9.74005500403372));
#31058=CARTESIAN_POINT('Ctrl Pts',(-89.1721999516398,-22.5251818354798,
9.58207183878508));
#31059=CARTESIAN_POINT('Ctrl Pts',(-89.2194956377292,-25.5627946871602,
9.42408867353645));
#31060=CARTESIAN_POINT('Ctrl Pts',(-91.7893172087739,-27.182356467315,9.26610550828781));
#31061=CARTESIAN_POINT('Ctrl Pts',(-94.5499838314406,-25.9156781324103,
9.10812234303918));
#31062=CARTESIAN_POINT('Ctrl Pts',(-94.9978511892309,-22.9112841930658,
8.95013917779054));
#31063=CARTESIAN_POINT('Ctrl Pts',(-92.7265049192209,-20.8944563764859,
8.79215601254192));
#31064=CARTESIAN_POINT('Ctrl Pts',(-89.7962234029809,-21.694431423617,8.63417284729327));
#31065=CARTESIAN_POINT('Ctrl Pts',(-88.8648280297145,-24.5856511406457,
8.47618968204465));
#31066=CARTESIAN_POINT('Ctrl Pts',(-90.7771477187876,-26.9456578035202,
8.318206516796));
#31067=CARTESIAN_POINT('Ctrl Pts',(-93.7986327013197,-26.6338559594106,
8.16022335154738));
#31068=CARTESIAN_POINT('Ctrl Pts',(-95.1886981287094,-23.9330550677513,
8.00224018629873));
#31069=CARTESIAN_POINT('Ctrl Pts',(-93.6865046857825,-21.2929763926182,
7.84425702105011));
#31070=CARTESIAN_POINT('Ctrl Pts',(-90.6545943354517,-21.108260096007,7.68627385580146));
#31071=CARTESIAN_POINT('Ctrl Pts',(-88.8430126453538,-23.5464508040852,
7.52829069055284));
#31072=CARTESIAN_POINT('Ctrl Pts',(-89.8949263381463,-26.3960260104052,
7.3703075253042));
#31073=CARTESIAN_POINT('Ctrl Pts',(-92.8562136451878,-27.0723238942441,
7.21232436005557));
#31074=CARTESIAN_POINT('Ctrl Pts',(-95.0408859750062,-24.9619191162964,
7.05434119480693));
#31075=CARTESIAN_POINT('Ctrl Pts',(-94.4673709220947,-21.9790208796034,
6.8963580295583));
#31076=CARTESIAN_POINT('Ctrl Pts',(-91.6558662317871,-20.8292196795368,
6.73837486430966));
#31077=CARTESIAN_POINT('Ctrl Pts',(-89.1565026125286,-22.5554244585598,
6.58039169906103));
#31078=CARTESIAN_POINT('Ctrl Pts',(-89.2362881797111,-25.5919085587089,
6.42240853381239));
#31079=CARTESIAN_POINT('Ctrl Pts',(-91.822854698647,-27.184477261553,6.26442536856376));
#31080=CARTESIAN_POINT('Ctrl Pts',(-94.5700980525807,-25.8886163947921,
6.10644220331513));
#31081=CARTESIAN_POINT('Ctrl Pts',(-94.9861747497105,-22.8797159955968,
5.94845903806648));
#31082=CARTESIAN_POINT('Ctrl Pts',(-92.6936890243839,-20.8869514260051,
5.79047587281786));
#31083=CARTESIAN_POINT('Ctrl Pts',(-89.7720036768111,-21.7178281680942,
5.63249270756922));
#31084=CARTESIAN_POINT('Ctrl Pts',(-88.8711870406774,-24.6187126571061,
5.47450954232059));
#31085=CARTESIAN_POINT('Ctrl Pts',(-90.808310551738,-26.9584036481696,5.31652637707195));
#31086=CARTESIAN_POINT('Ctrl Pts',(-93.8263370672836,-26.614721553626,5.15854321182333));
#31087=CARTESIAN_POINT('Ctrl Pts',(-95.1878135260188,-23.8993977640051,
5.00056004657468));
#31088=CARTESIAN_POINT('Ctrl Pts',(-93.6578343097117,-21.2753236359739,
4.84257688132605));
#31089=CARTESIAN_POINT('Ctrl Pts',(-90.6241427891289,-21.1226239696228,
4.68459371607742));
#31090=CARTESIAN_POINT('Ctrl Pts',(-88.8384007196145,-23.5798025728902,
4.52661055082878));
#31091=CARTESIAN_POINT('Ctrl Pts',(-89.9203371098729,-26.4181145867162,
4.36862738558015));
#31092=CARTESIAN_POINT('Ctrl Pts',(-92.8885987242112,-27.0631141310124,
4.21064422033151));
#31093=CARTESIAN_POINT('Ctrl Pts',(-95.0508709671726,-24.9297646158834,
4.05266105508288));
#31094=CARTESIAN_POINT('Ctrl Pts',(-94.445899107565,-21.9530868428383,3.89467788983425));
#31095=CARTESIAN_POINT('Ctrl Pts',(-91.62241327888,-20.8330292024708,3.7366947245856));
#31096=CARTESIAN_POINT('Ctrl Pts',(-89.1414114833444,-22.5855221023445,
3.57871155933698));
#31097=CARTESIAN_POINT('Ctrl Pts',(-89.2532470641262,-25.6209948747027,
3.42072839408834));
#31098=CARTESIAN_POINT('Ctrl Pts',(-91.8564812654672,-27.1861696814399,
3.26274522883971));
#31099=CARTESIAN_POINT('Ctrl Pts',(-94.58989194922,-25.8613804209117,3.10476206359107));
#31100=CARTESIAN_POINT('Ctrl Pts',(-94.9741820494077,-22.8482543917338,
2.94677889834244));
#31101=CARTESIAN_POINT('Ctrl Pts',(-92.6607878976182,-20.8798033793579,
2.7887957330938));
#31102=CARTESIAN_POINT('Ctrl Pts',(-89.7480357883012,-21.7414722204429,
2.63081256784517));
#31103=CARTESIAN_POINT('Ctrl Pts',(-88.8778936769897,-24.6517130179715,
2.47282940259654));
#31104=CARTESIAN_POINT('Ctrl Pts',(-90.8396053100351,-26.9708070887728,
2.3148462373479));
#31105=CARTESIAN_POINT('Ctrl Pts',(-93.8538411811633,-26.595320160609,2.15686307209927));
#31106=CARTESIAN_POINT('Ctrl Pts',(-95.186566248633,-23.8657026036092,1.99887990685063));
#31107=CARTESIAN_POINT('Ctrl Pts',(-93.6289946931135,-21.2580743603466,
1.840896741602));
#31108=CARTESIAN_POINT('Ctrl Pts',(-90.5938127173193,-21.1371047750834,
1.68291357635336));
#31109=CARTESIAN_POINT('Ctrl Pts',(-88.8342062503661,-23.6136172018791,
1.52493041110473));
#31110=CARTESIAN_POINT('Ctrl Pts',(-89.9458465956615,-26.4390837544954,
1.36694724585609));
#31111=CARTESIAN_POINT('Ctrl Pts',(-92.9211507155708,-27.0553093091995,
1.20896408060746));
#31112=CARTESIAN_POINT('Ctrl Pts',(-95.0599470782476,-24.8938952312942,
1.05098091535882));
#31113=CARTESIAN_POINT('Ctrl Pts',(-94.6354960985062,-22.923310192037,0.945658805193066));
#31114=CARTESIAN_POINT('Ctrl Pts',(-94.054331550342,-22.2435746787731,0.892997750110188));
#31115=CARTESIAN_POINT('Ctrl Pts',(-92.6501999979751,-26.4320868020351,
10.3210067496694));
#31116=CARTESIAN_POINT('Ctrl Pts',(-93.4549268544596,-26.2169491679593,
10.2683456945866));
#31117=CARTESIAN_POINT('Ctrl Pts',(-94.8204144183814,-24.928281963658,10.1630235844208));
#31118=CARTESIAN_POINT('Ctrl Pts',(-94.3190521113201,-22.1407648353735,
10.0050404191722));
#31119=CARTESIAN_POINT('Ctrl Pts',(-91.7101077457726,-21.044003174893,9.84705725392354));
#31120=CARTESIAN_POINT('Ctrl Pts',(-89.3661022550113,-22.6263101452131,
9.68907408867489));
#31121=CARTESIAN_POINT('Ctrl Pts',(-89.4101548750016,-25.4556338255876,
9.53109092342626));
#31122=CARTESIAN_POINT('Ctrl Pts',(-91.8037637317956,-26.9641422235181,
9.37310775817763));
#31123=CARTESIAN_POINT('Ctrl Pts',(-94.3751313913739,-25.7843200462513,
9.21512459292899));
#31124=CARTESIAN_POINT('Ctrl Pts',(-94.7922884758791,-22.9859374567589,
9.05714142768036));
#31125=CARTESIAN_POINT('Ctrl Pts',(-92.6766884630223,-21.107403562115,8.89915826243172));
#31126=CARTESIAN_POINT('Ctrl Pts',(-89.9473364063652,-21.8525243049723,
8.7411750971831));
#31127=CARTESIAN_POINT('Ctrl Pts',(-89.0798068316481,-24.5454930307365,
8.58319193193445));
#31128=CARTESIAN_POINT('Ctrl Pts',(-90.8609987230861,-26.7436739916243,
8.42520876668582));
#31129=CARTESIAN_POINT('Ctrl Pts',(-93.675300422608,-26.4532524059257,8.26722560143718));
#31130=CARTESIAN_POINT('Ctrl Pts',(-94.9700490370695,-23.9376454830353,
8.10924243618854));
#31131=CARTESIAN_POINT('Ctrl Pts',(-93.5708610272395,-21.4785970531231,
7.95125927093992));
#31132=CARTESIAN_POINT('Ctrl Pts',(-90.7468488275882,-21.3065467565016,
7.79327610569128));
#31133=CARTESIAN_POINT('Ctrl Pts',(-89.05948732861,-23.577550681119,7.63529294044265));
#31134=CARTESIAN_POINT('Ctrl Pts',(-90.0392712793796,-26.2317304610699,
7.47730977519401));
#31135=CARTESIAN_POINT('Ctrl Pts',(-92.7975030591701,-26.861654586086,7.31932660994538));
#31136=CARTESIAN_POINT('Ctrl Pts',(-94.8323723655712,-24.8959603041042,
7.16134344469674));
#31137=CARTESIAN_POINT('Ctrl Pts',(-94.298183250801,-22.1175994565215,7.00336027944811));
#31138=CARTESIAN_POINT('Ctrl Pts',(-91.6794634908518,-21.0466401467228,
6.84537711419947));
#31139=CARTESIAN_POINT('Ctrl Pts',(-89.3514812827431,-22.6544790310505,
6.68739394895084));
#31140=CARTESIAN_POINT('Ctrl Pts',(-89.4257959520587,-25.4827513584077,
6.52941078370221));
#31141=CARTESIAN_POINT('Ctrl Pts',(-91.8350015553469,-26.9661175948547,
6.37142761845357));
#31142=CARTESIAN_POINT('Ctrl Pts',(-94.393866379986,-25.7591139324989,6.21344445320494));
#31143=CARTESIAN_POINT('Ctrl Pts',(-94.7814126900398,-22.9565338911938,
6.0554612879563));
#31144=CARTESIAN_POINT('Ctrl Pts',(-92.6461227547216,-21.1004132262322,
5.89747812270767));
#31145=CARTESIAN_POINT('Ctrl Pts',(-89.9247774272819,-21.8743167342334,
5.73949495745903));
#31146=CARTESIAN_POINT('Ctrl Pts',(-89.0857298051077,-24.5762875183812,
5.5815117922104));
#31147=CARTESIAN_POINT('Ctrl Pts',(-90.8900247199854,-26.7555458534626,
5.42352862696176));
#31148=CARTESIAN_POINT('Ctrl Pts',(-93.7011050996681,-26.4354300467115,
5.26554546171314));
#31149=CARTESIAN_POINT('Ctrl Pts',(-94.9692250916023,-23.9062960612504,
5.10756229646449));
#31150=CARTESIAN_POINT('Ctrl Pts',(-93.5441565794039,-21.4621547463393,
4.94957913121586));
#31151=CARTESIAN_POINT('Ctrl Pts',(-90.718485344379,-21.3199256990289,4.79159596596723));
#31152=CARTESIAN_POINT('Ctrl Pts',(-89.0551916427067,-23.6086155184995,
4.63361280071859));
#31153=CARTESIAN_POINT('Ctrl Pts',(-90.0629396340034,-26.252304423281,4.47562963546996));
#31154=CARTESIAN_POINT('Ctrl Pts',(-92.8276674927058,-26.8530763364952,
4.31764647022132));
#31155=CARTESIAN_POINT('Ctrl Pts',(-94.841672686634,-24.8660106383991,4.15966330497269));
#31156=CARTESIAN_POINT('Ctrl Pts',(-94.278183759004,-22.0934437171531,4.00168013972405));
#31157=CARTESIAN_POINT('Ctrl Pts',(-91.648304407565,-21.0501884505964,3.84369697447542));
#31158=CARTESIAN_POINT('Ctrl Pts',(-89.3374249525755,-22.6825128788256,
3.68571380922679));
#31159=CARTESIAN_POINT('Ctrl Pts',(-89.4415919654453,-25.5098432251578,
3.52773064397815));
#31160=CARTESIAN_POINT('Ctrl Pts',(-91.8663223478376,-26.9676939654775,
3.36974747872951));
#31161=CARTESIAN_POINT('Ctrl Pts',(-94.4123030087544,-25.7337455298681,
3.21176431348088));
#31162=CARTESIAN_POINT('Ctrl Pts',(-94.770242329426,-22.9272296101091,3.05378114823225));
#31163=CARTESIAN_POINT('Ctrl Pts',(-92.6154776588472,-21.0937553212802,
2.89579798298361));
#31164=CARTESIAN_POINT('Ctrl Pts',(-89.9024530173452,-21.8963395134606,
2.73781481773498));
#31165=CARTESIAN_POINT('Ctrl Pts',(-89.0919765672402,-24.6070250438712,
2.57983165248634));
#31166=CARTESIAN_POINT('Ctrl Pts',(-90.9191735961077,-26.7670987899064,
2.42184848723771));
#31167=CARTESIAN_POINT('Ctrl Pts',(-93.7267232559334,-26.4173590075846,
2.26386532198908));
#31168=CARTESIAN_POINT('Ctrl Pts',(-94.9680633400506,-23.8749113786469,
2.10588215674044));
#31169=CARTESIAN_POINT('Ctrl Pts',(-93.5172944958673,-21.4460882538716,
1.94789899149181));
#31170=CARTESIAN_POINT('Ctrl Pts',(-90.6902350061731,-21.3334135553823,
1.78991582624317));
#31171=CARTESIAN_POINT('Ctrl Pts',(-89.051284788295,-23.6401114777322,1.63193266099454));
#31172=CARTESIAN_POINT('Ctrl Pts',(-90.0866999338637,-26.2718357348248,
1.4739494957459));
#31173=CARTESIAN_POINT('Ctrl Pts',(-92.8579873933955,-26.8458066914632,
1.31596633049727));
#31174=CARTESIAN_POINT('Ctrl Pts',(-94.8501264485991,-24.8326008181969,
1.15798316524863));
#31175=CARTESIAN_POINT('Ctrl Pts',(-94.4547800806522,-22.9971388327508,
1.05266105508288));
#31176=CARTESIAN_POINT('Ctrl Pts',(-93.913465996665,-22.364012796625,0.999999999999999));
#31177=CARTESIAN_POINT('Ctrl Pts',(-94.5149492652116,-23.9982505980887,
9.11258330249199));
#31178=CARTESIAN_POINT('Ctrl Pts',(-94.5168562980303,-23.7052247424895,
9.09410267755478));
#31179=CARTESIAN_POINT('Ctrl Pts',(-94.4695028989504,-23.4127947803891,
9.07562205261757));
#31180=CARTESIAN_POINT('Ctrl Pts',(-94.3701622929854,-23.139245572567,9.05714142768036));
#31181=CARTESIAN_POINT('Ctrl Pts',(-94.0870884715935,-22.3597594918776,
9.00448037259748));
#31182=CARTESIAN_POINT('Ctrl Pts',(-93.3818884673079,-21.7335815269963,
8.9518193175146));
#31183=CARTESIAN_POINT('Ctrl Pts',(-92.5743964557222,-21.5446793350319,
8.89915826243172));
#31184=CARTESIAN_POINT('Ctrl Pts',(-91.7669044441366,-21.3557771430674,
8.84649720734885));
#31185=CARTESIAN_POINT('Ctrl Pts',(-90.8571204252509,-21.6041507240199,
8.79383615226597));
#31186=CARTESIAN_POINT('Ctrl Pts',(-90.2576401533552,-22.1771656354568,
8.74117509718309));
#31187=CARTESIAN_POINT('Ctrl Pts',(-89.6581598814595,-22.7501805468937,
8.68851404210021));
#31188=CARTESIAN_POINT('Ctrl Pts',(-89.3689833565538,-23.6478367888151,
8.63585298701733));
#31189=CARTESIAN_POINT('Ctrl Pts',(-89.5212604093406,-24.4630284032571,
8.58319193193445));
#31190=CARTESIAN_POINT('Ctrl Pts',(-89.6735374621274,-25.2782200176991,
8.53053087685158));
#31191=CARTESIAN_POINT('Ctrl Pts',(-90.2672680926067,-26.0109470046617,
8.4778698217687));
#31192=CARTESIAN_POINT('Ctrl Pts',(-91.0331836911001,-26.3289069005266,
8.42520876668582));
#31193=CARTESIAN_POINT('Ctrl Pts',(-91.7990992895934,-26.6468667963914,
8.37254771160294));
#31194=CARTESIAN_POINT('Ctrl Pts',(-92.7371998561007,-26.5500596011586,
8.31988665652006));
#31195=CARTESIAN_POINT('Ctrl Pts',(-93.422041575098,-26.0823881830604,8.26722560143718));
#31196=CARTESIAN_POINT('Ctrl Pts',(-94.0924009622684,-25.6246066015112,
8.21567816845545));
#31197=CARTESIAN_POINT('Ctrl Pts',(-94.5200995637937,-24.811480262719,8.16413073547371));
#31198=CARTESIAN_POINT('Ctrl Pts',(-94.5215633824187,-23.9996804087645,
8.11258330249198));
#31199=CARTESIAN_POINT('Ctrl Pts',(-92.7937992825329,-26.9692229537457,
10.));
#31200=CARTESIAN_POINT('Ctrl Pts',(-92.886852386908,-26.9351837124997,10.));
#31201=CARTESIAN_POINT('Ctrl Pts',(-92.9778402151635,-26.8963761434536,
10.));
#31202=CARTESIAN_POINT('Ctrl Pts',(-93.0665542695815,-26.8531284786668,
10.));
#31203=CARTESIAN_POINT('Ctrl Pts',(-93.1572340298667,-26.8089225419468,
10.));
#31204=CARTESIAN_POINT('Ctrl Pts',(-93.2455388043682,-26.7600769477925,
10.));
#31205=CARTESIAN_POINT('Ctrl Pts',(-93.3312170072855,-26.7068966945046,
10.));
#31206=CARTESIAN_POINT('Ctrl Pts',(-93.4136695050849,-26.65571862858,10.));
#31207=CARTESIAN_POINT('Ctrl Pts',(-93.4936897697168,-26.6005252759063,
10.));
#31208=CARTESIAN_POINT('Ctrl Pts',(-93.5710205780919,-26.5415583960894,
10.));
#31209=CARTESIAN_POINT('Ctrl Pts',(-93.63868503542,-26.4899623762497,10.));
#31210=CARTESIAN_POINT('Ctrl Pts',(-93.7042900873145,-26.4354765516642,
10.));
#31211=CARTESIAN_POINT('Ctrl Pts',(-93.7676387673489,-26.378250171364,10.));
#31212=CARTESIAN_POINT('Ctrl Pts',(-93.781737609333,-26.3655139045193,10.));
#31213=CARTESIAN_POINT('Ctrl Pts',(-93.795727291904,-26.3526391912679,10.));
#31214=CARTESIAN_POINT('Ctrl Pts',(-93.8095861705268,-26.3396461050457,
10.));
#31215=CARTESIAN_POINT('Ctrl Pts',(-93.882016875094,-26.271740294252,10.));
#31216=CARTESIAN_POINT('Ctrl Pts',(-93.9509819060163,-26.2005127260756,
10.));
#31217=CARTESIAN_POINT('Ctrl Pts',(-94.0162413172811,-26.1262540066759,
10.));
#31218=CARTESIAN_POINT('Ctrl Pts',(-94.0811410662549,-26.0524045471918,
10.));
#31219=CARTESIAN_POINT('Ctrl Pts',(-94.1423764147232,-25.9755564586413,
10.));
#31220=CARTESIAN_POINT('Ctrl Pts',(-94.1996677535172,-25.895968801161,10.));
#31221=CARTESIAN_POINT('Ctrl Pts',(-94.2548605589228,-25.8192963724053,
10.));
#31222=CARTESIAN_POINT('Ctrl Pts',(-94.3063931619475,-25.7400806580935,
10.));
#31223=CARTESIAN_POINT('Ctrl Pts',(-94.3539706372945,-25.6585396692548,
10.));
#31224=CARTESIAN_POINT('Ctrl Pts',(-94.3739594034168,-25.6242817826521,
10.));
#31225=CARTESIAN_POINT('Ctrl Pts',(-94.3932494780977,-25.589613354766,10.));
#31226=CARTESIAN_POINT('Ctrl Pts',(-94.4118163867649,-25.554550253182,10.));
#31227=CARTESIAN_POINT('Ctrl Pts',(-94.424852971342,-25.5299310180939,10.));
#31228=CARTESIAN_POINT('Ctrl Pts',(-94.4375330011157,-25.5051172053715,
10.));
#31229=CARTESIAN_POINT('Ctrl Pts',(-94.4498475176035,-25.4801143018019,
10.));
#31230=CARTESIAN_POINT('Ctrl Pts',(-94.4575999796004,-25.4643740118823,
10.));
#31231=CARTESIAN_POINT('Ctrl Pts',(-94.4652084584732,-25.4485566580947,
10.));
#31232=CARTESIAN_POINT('Ctrl Pts',(-94.4726610535095,-25.4326847360384,
10.));
#31233=CARTESIAN_POINT('Ctrl Pts',(-94.5147816016199,-25.3429798676917,
10.));
#31234=CARTESIAN_POINT('Ctrl Pts',(-94.551999940776,-25.2513903180325,10.));
#31235=CARTESIAN_POINT('Ctrl Pts',(-94.5840244250316,-25.1581885555992,
10.));
#31236=CARTESIAN_POINT('Ctrl Pts',(-94.6138868935619,-25.0712789686901,
10.));
#31237=CARTESIAN_POINT('Ctrl Pts',(-94.6392329460682,-24.9829667140799,
10.));
#31238=CARTESIAN_POINT('Ctrl Pts',(-94.6597755596864,-24.8934640331103,
10.));
#31239=CARTESIAN_POINT('Ctrl Pts',(-94.6612628263414,-24.8869841199203,
10.));
#31240=CARTESIAN_POINT('Ctrl Pts',(-94.6627248923899,-24.8804979657906,
10.));
#31241=CARTESIAN_POINT('Ctrl Pts',(-94.6641616381052,-24.874005650947,10.));
#31242=CARTESIAN_POINT('Ctrl Pts',(-94.6847472407902,-24.7809841702089,
10.));
#31243=CARTESIAN_POINT('Ctrl Pts',(-94.7001390631694,-24.6866969715819,
10.));
#31244=CARTESIAN_POINT('Ctrl Pts',(-94.7104141120184,-24.5915520773872,
10.));
#31245=CARTESIAN_POINT('Ctrl Pts',(-94.7162317525601,-24.5376818912762,
10.));
#31246=CARTESIAN_POINT('Ctrl Pts',(-94.7204081622463,-24.483536940679,10.));
#31247=CARTESIAN_POINT('Ctrl Pts',(-94.7229504259482,-24.4291939795176,
10.));
#31248=CARTESIAN_POINT('Ctrl Pts',(-94.7235977676587,-24.4153565222132,
10.));
#31249=CARTESIAN_POINT('Ctrl Pts',(-94.7241390041218,-24.4015076323046,
10.));
#31250=CARTESIAN_POINT('Ctrl Pts',(-94.7245740715257,-24.3876608123636,
10.));
#31251=CARTESIAN_POINT('Ctrl Pts',(-94.7275028913787,-24.2944457363059,
10.));
#31252=CARTESIAN_POINT('Ctrl Pts',(-94.7256323237335,-24.20117339609,10.));
#31253=CARTESIAN_POINT('Ctrl Pts',(-94.7190972361895,-24.1082190601576,
10.));
#31254=CARTESIAN_POINT('Ctrl Pts',(-94.7125517108725,-24.0151162585377,
10.));
#31255=CARTESIAN_POINT('Ctrl Pts',(-94.7013263747111,-23.922331498206,10.));
#31256=CARTESIAN_POINT('Ctrl Pts',(-94.6855058357614,-23.8302540027448,
10.));
#31257=CARTESIAN_POINT('Ctrl Pts',(-94.669912459968,-23.7394986249788,10.));
#31258=CARTESIAN_POINT('Ctrl Pts',(-94.6498544351971,-23.6494295034801,
10.));
#31259=CARTESIAN_POINT('Ctrl Pts',(-94.6253697912028,-23.5604445846,10.));
#31260=CARTESIAN_POINT('Ctrl Pts',(-94.6161277167171,-23.5268559709129,
10.));
#31261=CARTESIAN_POINT('Ctrl Pts',(-94.6062545340008,-23.4934221578844,
10.));
#31262=CARTESIAN_POINT('Ctrl Pts',(-94.5957508646961,-23.4601658754547,
10.));
#31263=CARTESIAN_POINT('Ctrl Pts',(-94.5880548970241,-23.4357992215696,
10.));
#31264=CARTESIAN_POINT('Ctrl Pts',(-94.5800204433778,-23.4115278887989,
10.));
#31265=CARTESIAN_POINT('Ctrl Pts',(-94.5716475012962,-23.3873611140396,
10.));
#31266=CARTESIAN_POINT('Ctrl Pts',(-94.5664800360046,-23.3724462885743,
10.));
#31267=CARTESIAN_POINT('Ctrl Pts',(-94.5611866347534,-23.3575799758845,
10.));
#31268=CARTESIAN_POINT('Ctrl Pts',(-94.5557684843318,-23.3427662650201,
10.));
#31269=CARTESIAN_POINT('Ctrl Pts',(-94.5240624591822,-23.2560791388461,
10.));
#31270=CARTESIAN_POINT('Ctrl Pts',(-94.4880796644939,-23.1711661844698,
10.));
#31271=CARTESIAN_POINT('Ctrl Pts',(-94.447880401404,-23.0884282232178,10.));
#31272=CARTESIAN_POINT('Ctrl Pts',(-94.4177309540866,-23.0263747522788,
10.));
#31273=CARTESIAN_POINT('Ctrl Pts',(-94.3852087541631,-22.9655451998349,
10.));
#31274=CARTESIAN_POINT('Ctrl Pts',(-94.3503241512496,-22.9061236582037,
10.));
#31275=CARTESIAN_POINT('Ctrl Pts',(-94.334545249284,-22.8792462795972,10.));
#31276=CARTESIAN_POINT('Ctrl Pts',(-94.3182828567332,-22.8526571658029,
10.));
#31277=CARTESIAN_POINT('Ctrl Pts',(-94.3015371510007,-22.8263744217796,
10.));
#31278=CARTESIAN_POINT('Ctrl Pts',(-94.2924151854529,-22.8120573013602,
10.));
#31279=CARTESIAN_POINT('Ctrl Pts',(-94.2831549823775,-22.7978392515682,
10.));
#31280=CARTESIAN_POINT('Ctrl Pts',(-94.2737572212008,-22.7837232845595,
10.));
#31281=CARTESIAN_POINT('Ctrl Pts',(-94.2261821463953,-22.7122628405486,
10.));
#31282=CARTESIAN_POINT('Ctrl Pts',(-94.175081861178,-22.6434116537846,10.));
#31283=CARTESIAN_POINT('Ctrl Pts',(-94.1204874224216,-22.5775232108296,
10.));
#31284=CARTESIAN_POINT('Ctrl Pts',(-94.0743569854685,-22.5218497258939,
10.));
#31285=CARTESIAN_POINT('Ctrl Pts',(-94.0257311604217,-22.4682919003745,
10.));
#31286=CARTESIAN_POINT('Ctrl Pts',(-93.9746123907307,-22.41708711057,10.));
#31287=CARTESIAN_POINT('Ctrl Pts',(-93.9557806038367,-22.3982236344852,
10.));
#31288=CARTESIAN_POINT('Ctrl Pts',(-93.9366103467742,-22.3796797449892,
10.));
#31289=CARTESIAN_POINT('Ctrl Pts',(-93.9171117712832,-22.3614597429256,
10.));
#31290=CARTESIAN_POINT('Origin',(-92.,-24.,5.));
#31291=CARTESIAN_POINT('Origin',(-30.,-108.,40.));
#31292=CARTESIAN_POINT('',(-30.,-95.3939201416946,10.));
#31293=CARTESIAN_POINT('',(-30.,-95.3939201416946,40.));
#31294=CARTESIAN_POINT('',(-30.,-95.3939201416946,0.));
#31295=CARTESIAN_POINT('',(-30.,-88.,10.));
#31296=CARTESIAN_POINT('',(-30.,-88.,10.));
#31297=CARTESIAN_POINT('',(-30.,-88.,40.));
#31298=CARTESIAN_POINT('',(-30.,-88.,40.));
#31299=CARTESIAN_POINT('',(-30.,-54.,40.));
#31300=CARTESIAN_POINT('Origin',(-30.,-88.,40.));
#31301=CARTESIAN_POINT('',(-12.,-88.,40.));
#31302=CARTESIAN_POINT('',(-12.,-88.,28.));
#31303=CARTESIAN_POINT('',(-12.,-88.,40.));
#31304=CARTESIAN_POINT('',(-15.,-88.,40.));
#31305=CARTESIAN_POINT('',(30.,-88.,10.));
#31306=CARTESIAN_POINT('',(30.,-88.,10.));
#31307=CARTESIAN_POINT('',(30.,-88.,40.));
#31308=CARTESIAN_POINT('',(30.,-88.,40.));
#31309=CARTESIAN_POINT('',(12.,-88.,40.));
#31310=CARTESIAN_POINT('',(-15.,-88.,40.));
#31311=CARTESIAN_POINT('',(12.,-88.,28.));
#31312=CARTESIAN_POINT('',(12.,-88.,40.));
#31313=CARTESIAN_POINT('',(18.,-88.,28.));
#31314=CARTESIAN_POINT('',(-15.,-88.,28.));
#31315=CARTESIAN_POINT('',(18.,-88.,12.));
#31316=CARTESIAN_POINT('',(18.,-88.,34.));
#31317=CARTESIAN_POINT('',(-18.,-88.,12.));
#31318=CARTESIAN_POINT('',(-15.,-88.,12.));
#31319=CARTESIAN_POINT('',(-18.,-88.,28.));
#31320=CARTESIAN_POINT('',(-18.,-88.,34.));
#31321=CARTESIAN_POINT('',(-15.,-88.,28.));
#31322=CARTESIAN_POINT('Origin',(30.,-88.,40.));
#31323=CARTESIAN_POINT('',(30.,-95.3939201416946,40.));
#31324=CARTESIAN_POINT('',(30.,-95.3939201416946,10.));
#31325=CARTESIAN_POINT('',(30.,-95.3939201416946,0.));
#31326=CARTESIAN_POINT('',(30.,-44.,40.));
#31327=CARTESIAN_POINT('',(30.,-108.,10.));
#31328=CARTESIAN_POINT('Origin',(0.,-98.,10.));
#31329=CARTESIAN_POINT('Origin',(0.,0.,10.));
#31330=CARTESIAN_POINT('Origin',(30.,88.,40.));
#31331=CARTESIAN_POINT('',(12.,88.,40.));
#31332=CARTESIAN_POINT('',(12.,88.,28.));
#31333=CARTESIAN_POINT('',(12.,88.,40.));
#31334=CARTESIAN_POINT('',(30.,88.,40.));
#31335=CARTESIAN_POINT('',(15.,88.,40.));
#31336=CARTESIAN_POINT('',(30.,88.,10.));
#31337=CARTESIAN_POINT('',(30.,88.,40.));
#31338=CARTESIAN_POINT('',(-30.,88.,10.));
#31339=CARTESIAN_POINT('',(-30.,88.,10.));
#31340=CARTESIAN_POINT('',(-30.,88.,40.));
#31341=CARTESIAN_POINT('',(-30.,88.,40.));
#31342=CARTESIAN_POINT('',(-12.,88.,40.));
#31343=CARTESIAN_POINT('',(15.,88.,40.));
#31344=CARTESIAN_POINT('',(-12.,88.,28.));
#31345=CARTESIAN_POINT('',(-12.,88.,40.));
#31346=CARTESIAN_POINT('',(-18.,88.,28.));
#31347=CARTESIAN_POINT('',(15.,88.,28.));
#31348=CARTESIAN_POINT('',(-18.,88.,12.));
#31349=CARTESIAN_POINT('',(-18.,88.,34.));
#31350=CARTESIAN_POINT('',(18.,88.,12.));
#31351=CARTESIAN_POINT('',(15.,88.,12.));
#31352=CARTESIAN_POINT('',(18.,88.,28.));
#31353=CARTESIAN_POINT('',(18.,88.,34.));
#31354=CARTESIAN_POINT('',(15.,88.,28.));
#31355=CARTESIAN_POINT('Origin',(30.,108.,40.));
#31356=CARTESIAN_POINT('',(30.,95.3939201416946,10.));
#31357=CARTESIAN_POINT('',(30.,95.3939201416946,40.));
#31358=CARTESIAN_POINT('',(30.,95.3939201416946,0.));
#31359=CARTESIAN_POINT('',(30.,88.,10.));
#31360=CARTESIAN_POINT('',(30.,54.,40.));
#31361=CARTESIAN_POINT('Origin',(-30.,88.,40.));
#31362=CARTESIAN_POINT('',(-30.,95.3939201416946,40.));
#31363=CARTESIAN_POINT('',(-30.,95.3939201416946,10.));
#31364=CARTESIAN_POINT('',(-30.,95.3939201416946,0.));
#31365=CARTESIAN_POINT('',(-30.,44.,40.));
#31366=CARTESIAN_POINT('',(-30.,108.,10.));
#31367=CARTESIAN_POINT('Origin',(0.,98.,10.));
#31368=CARTESIAN_POINT('Origin',(0.,0.,10.));
#31369=CARTESIAN_POINT('Origin',(0.,-54.,12.));
#31370=CARTESIAN_POINT('',(18.,-18.,12.));
#31371=CARTESIAN_POINT('',(18.,-90.,12.));
#31372=CARTESIAN_POINT('',(8.71779788708135,-18.,12.));
#31373=CARTESIAN_POINT('',(18.,-18.,12.));
#31374=CARTESIAN_POINT('',(-8.71779788708135,-18.,12.));
#31375=CARTESIAN_POINT('Origin',(0.,0.,12.));
#31376=CARTESIAN_POINT('',(-18.,-18.,12.));
#31377=CARTESIAN_POINT('',(18.,-18.,12.));
#31378=CARTESIAN_POINT('',(-18.,-18.,12.));
#31379=CARTESIAN_POINT('Origin',(18.,-18.,28.));
#31380=CARTESIAN_POINT('',(18.,-18.,28.));
#31381=CARTESIAN_POINT('',(18.,-90.,28.));
#31382=CARTESIAN_POINT('',(18.,-18.,28.));
#31383=CARTESIAN_POINT('Origin',(0.,0.,40.));
#31384=CARTESIAN_POINT('',(95.3939201416946,-30.,40.));
#31385=CARTESIAN_POINT('Origin',(0.,0.,40.));
#31386=CARTESIAN_POINT('',(88.,-30.,40.));
#31387=CARTESIAN_POINT('',(54.,-30.,40.));
#31388=CARTESIAN_POINT('',(88.,-12.,40.));
#31389=CARTESIAN_POINT('',(88.,-15.,40.));
#31390=CARTESIAN_POINT('',(18.,-12.,40.));
#31391=CARTESIAN_POINT('',(45.,-12.,40.));
#31392=CARTESIAN_POINT('',(18.,-8.71779788708135,40.));
#31393=CARTESIAN_POINT('',(18.,-6.,40.));
#31394=CARTESIAN_POINT('',(8.71779788708135,-18.,40.));
#31395=CARTESIAN_POINT('Origin',(0.,0.,40.));
#31396=CARTESIAN_POINT('',(12.,-18.,40.));
#31397=CARTESIAN_POINT('',(-6.,-18.,40.));
#31398=CARTESIAN_POINT('',(12.,-9.,40.));
#31399=CARTESIAN_POINT('Origin',(0.,0.,40.));
#31400=CARTESIAN_POINT('',(-12.,-18.,40.));
#31401=CARTESIAN_POINT('',(-12.,-45.,40.));
#31402=CARTESIAN_POINT('',(-8.71779788708135,-18.,40.));
#31403=CARTESIAN_POINT('',(-6.,-18.,40.));
#31404=CARTESIAN_POINT('',(-18.,-8.71779788708135,40.));
#31405=CARTESIAN_POINT('Origin',(0.,0.,40.));
#31406=CARTESIAN_POINT('',(-18.,-12.,40.));
#31407=CARTESIAN_POINT('',(-18.,6.,40.));
#31408=CARTESIAN_POINT('',(-88.,-12.,40.));
#31409=CARTESIAN_POINT('',(-9.,-12.,40.));
#31410=CARTESIAN_POINT('',(-88.,-30.,40.));
#31411=CARTESIAN_POINT('',(-88.,15.,40.));
#31412=CARTESIAN_POINT('',(-95.3939201416946,-30.,40.));
#31413=CARTESIAN_POINT('',(-44.,-30.,40.));
#31414=CARTESIAN_POINT('Origin',(0.,0.,40.));
#31415=CARTESIAN_POINT('Origin',(0.,-54.,28.));
#31416=CARTESIAN_POINT('',(12.,-18.,28.));
#31417=CARTESIAN_POINT('',(12.,-90.,28.));
#31418=CARTESIAN_POINT('',(18.,-18.,28.));
#31419=CARTESIAN_POINT('Origin',(12.,-18.,40.));
#31420=CARTESIAN_POINT('',(12.,-18.,40.));
#31421=CARTESIAN_POINT('Origin',(0.,54.,12.));
#31422=CARTESIAN_POINT('',(-18.,18.,12.));
#31423=CARTESIAN_POINT('',(-18.,90.,12.));
#31424=CARTESIAN_POINT('',(-8.71779788708135,18.,12.));
#31425=CARTESIAN_POINT('',(-18.,18.,12.));
#31426=CARTESIAN_POINT('',(8.71779788708135,18.,12.));
#31427=CARTESIAN_POINT('Origin',(0.,0.,12.));
#31428=CARTESIAN_POINT('',(18.,18.,12.));
#31429=CARTESIAN_POINT('',(-18.,18.,12.));
#31430=CARTESIAN_POINT('',(18.,18.,12.));
#31431=CARTESIAN_POINT('Origin',(-18.,18.,28.));
#31432=CARTESIAN_POINT('',(-18.,18.,28.));
#31433=CARTESIAN_POINT('',(-18.,90.,28.));
#31434=CARTESIAN_POINT('',(-18.,18.,28.));
#31435=CARTESIAN_POINT('Origin',(0.,54.,28.));
#31436=CARTESIAN_POINT('',(-12.,18.,28.));
#31437=CARTESIAN_POINT('',(-12.,90.,28.));
#31438=CARTESIAN_POINT('',(-18.,18.,28.));
#31439=CARTESIAN_POINT('Origin',(-12.,18.,40.));
#31440=CARTESIAN_POINT('',(-12.,18.,40.));
#31441=CARTESIAN_POINT('',(-12.,9.,40.));
#31442=CARTESIAN_POINT('',(-12.,18.,40.));
#31443=CARTESIAN_POINT('Origin',(0.,0.,40.));
#31444=CARTESIAN_POINT('',(-95.3939201416946,30.,40.));
#31445=CARTESIAN_POINT('Origin',(0.,0.,40.));
#31446=CARTESIAN_POINT('',(-88.,30.,40.));
#31447=CARTESIAN_POINT('',(-54.,30.,40.));
#31448=CARTESIAN_POINT('',(-88.,12.,40.));
#31449=CARTESIAN_POINT('',(-88.,15.,40.));
#31450=CARTESIAN_POINT('',(-18.,12.,40.));
#31451=CARTESIAN_POINT('',(-45.,12.,40.));
#31452=CARTESIAN_POINT('',(-18.,8.71779788708135,40.));
#31453=CARTESIAN_POINT('',(-18.,6.,40.));
#31454=CARTESIAN_POINT('',(-8.71779788708135,18.,40.));
#31455=CARTESIAN_POINT('Origin',(0.,0.,40.));
#31456=CARTESIAN_POINT('',(6.,18.,40.));
#31457=CARTESIAN_POINT('Origin',(-18.,-90.,28.));
#31458=CARTESIAN_POINT('',(-18.,-18.,28.));
#31459=CARTESIAN_POINT('',(-18.,-18.,28.));
#31460=CARTESIAN_POINT('',(-18.,-18.,28.));
#31461=CARTESIAN_POINT('Origin',(0.,-54.,28.));
#31462=CARTESIAN_POINT('',(-12.,-18.,28.));
#31463=CARTESIAN_POINT('',(18.,-18.,28.));
#31464=CARTESIAN_POINT('',(-12.,-18.,28.));
#31465=CARTESIAN_POINT('Origin',(0.,54.,28.));
#31466=CARTESIAN_POINT('',(18.,18.,28.));
#31467=CARTESIAN_POINT('',(18.,18.,28.));
#31468=CARTESIAN_POINT('',(12.,18.,28.));
#31469=CARTESIAN_POINT('',(-18.,18.,28.));
#31470=CARTESIAN_POINT('',(12.,18.,28.));
#31471=CARTESIAN_POINT('Origin',(18.,90.,28.));
#31472=CARTESIAN_POINT('',(18.,18.,28.));
#31473=CARTESIAN_POINT('Origin',(0.,0.,0.));
#31474=CARTESIAN_POINT('',(-8.71779788708135,-18.,0.));
#31475=CARTESIAN_POINT('',(8.71779788708135,-18.,0.));
#31476=CARTESIAN_POINT('',(18.,-8.71779788708135,12.));
#31477=CARTESIAN_POINT('',(18.,-8.71779788708135,0.));
#31478=CARTESIAN_POINT('',(18.,8.71779788708135,12.));
#31479=CARTESIAN_POINT('Origin',(0.,0.,12.));
#31480=CARTESIAN_POINT('',(18.,8.71779788708135,40.));
#31481=CARTESIAN_POINT('',(18.,8.71779788708135,0.));
#31482=CARTESIAN_POINT('',(8.71779788708135,18.,40.));
#31483=CARTESIAN_POINT('Origin',(0.,0.,40.));
#31484=CARTESIAN_POINT('',(8.71779788708135,18.,0.));
#31485=CARTESIAN_POINT('',(-8.71779788708135,18.,0.));
#31486=CARTESIAN_POINT('',(-18.,8.71779788708135,12.));
#31487=CARTESIAN_POINT('',(-18.,8.71779788708135,0.));
#31488=CARTESIAN_POINT('',(-20.,-2.44929359829471E-15,12.));
#31489=CARTESIAN_POINT('Origin',(0.,0.,12.));
#31490=CARTESIAN_POINT('',(-20.,2.44929359829471E-15,4.));
#31491=CARTESIAN_POINT('',(-20.,-2.44929359829471E-15,0.));
#31492=CARTESIAN_POINT('Origin',(0.,0.,4.));
#31493=CARTESIAN_POINT('',(-18.,-8.71779788708135,12.));
#31494=CARTESIAN_POINT('Origin',(0.,0.,12.));
#31495=CARTESIAN_POINT('',(-18.,-8.71779788708135,0.));
#31496=CARTESIAN_POINT('Origin',(-12.,-18.,40.));
#31497=CARTESIAN_POINT('',(-12.,-18.,40.));
#31498=CARTESIAN_POINT('',(-18.,-18.,28.));
#31499=CARTESIAN_POINT('Origin',(-12.,-18.,40.));
#31500=CARTESIAN_POINT('',(18.,-18.,28.));
#31501=CARTESIAN_POINT('Origin',(-12.,-90.,40.));
#31502=CARTESIAN_POINT('Origin',(12.,18.,40.));
#31503=CARTESIAN_POINT('',(-18.,18.,28.));
#31504=CARTESIAN_POINT('Origin',(12.,18.,40.));
#31505=CARTESIAN_POINT('',(12.,18.,40.));
#31506=CARTESIAN_POINT('',(6.,18.,40.));
#31507=CARTESIAN_POINT('',(12.,18.,40.));
#31508=CARTESIAN_POINT('',(18.,18.,28.));
#31509=CARTESIAN_POINT('Origin',(12.,90.,40.));
#31510=CARTESIAN_POINT('',(12.,45.,40.));
#31511=CARTESIAN_POINT('Origin',(-88.,-30.,40.));
#31512=CARTESIAN_POINT('',(-95.3939201416946,-30.,10.));
#31513=CARTESIAN_POINT('',(-95.3939201416946,-30.,0.));
#31514=CARTESIAN_POINT('',(-88.,-30.,10.));
#31515=CARTESIAN_POINT('',(-88.,-30.,40.));
#31516=CARTESIAN_POINT('',(-108.,-30.,10.));
#31517=CARTESIAN_POINT('Origin',(-98.,0.,10.));
#31518=CARTESIAN_POINT('',(-100.,-1.22464679914735E-14,10.));
#31519=CARTESIAN_POINT('Origin',(0.,0.,10.));
#31520=CARTESIAN_POINT('',(-88.,30.,10.));
#31521=CARTESIAN_POINT('',(-88.,-30.,10.));
#31522=CARTESIAN_POINT('',(-95.3939201416946,30.,10.));
#31523=CARTESIAN_POINT('',(-88.,30.,10.));
#31524=CARTESIAN_POINT('Origin',(0.,0.,10.));
#31525=CARTESIAN_POINT('Origin',(-88.,30.,40.));
#31526=CARTESIAN_POINT('',(-88.,-12.,28.));
#31527=CARTESIAN_POINT('',(-88.,-12.,40.));
#31528=CARTESIAN_POINT('',(-88.,-18.,28.));
#31529=CARTESIAN_POINT('',(-88.,15.,28.));
#31530=CARTESIAN_POINT('',(-88.,-18.,12.));
#31531=CARTESIAN_POINT('',(-88.,-18.,34.));
#31532=CARTESIAN_POINT('',(-88.,18.,12.));
#31533=CARTESIAN_POINT('',(-88.,15.,12.));
#31534=CARTESIAN_POINT('',(-88.,18.,28.));
#31535=CARTESIAN_POINT('',(-88.,18.,34.));
#31536=CARTESIAN_POINT('',(-88.,12.,28.));
#31537=CARTESIAN_POINT('',(-88.,15.,28.));
#31538=CARTESIAN_POINT('',(-88.,12.,40.));
#31539=CARTESIAN_POINT('',(-88.,30.,40.));
#31540=CARTESIAN_POINT('Origin',(-108.,30.,40.));
#31541=CARTESIAN_POINT('',(-95.3939201416946,30.,0.));
#31542=CARTESIAN_POINT('Origin',(108.,-30.,40.));
#31543=CARTESIAN_POINT('',(95.3939201416946,-30.,10.));
#31544=CARTESIAN_POINT('',(95.3939201416946,-30.,0.));
#31545=CARTESIAN_POINT('',(88.,-30.,10.));
#31546=CARTESIAN_POINT('',(88.,-30.,10.));
#31547=CARTESIAN_POINT('',(88.,-30.,40.));
#31548=CARTESIAN_POINT('Origin',(88.,-30.,40.));
#31549=CARTESIAN_POINT('',(88.,-12.,28.));
#31550=CARTESIAN_POINT('',(88.,-12.,40.));
#31551=CARTESIAN_POINT('',(88.,30.,10.));
#31552=CARTESIAN_POINT('',(88.,30.,10.));
#31553=CARTESIAN_POINT('',(88.,30.,40.));
#31554=CARTESIAN_POINT('',(88.,30.,40.));
#31555=CARTESIAN_POINT('',(88.,12.,40.));
#31556=CARTESIAN_POINT('',(88.,-15.,40.));
#31557=CARTESIAN_POINT('',(88.,12.,28.));
#31558=CARTESIAN_POINT('',(88.,12.,40.));
#31559=CARTESIAN_POINT('',(88.,18.,28.));
#31560=CARTESIAN_POINT('',(88.,-15.,28.));
#31561=CARTESIAN_POINT('',(88.,18.,12.));
#31562=CARTESIAN_POINT('',(88.,18.,34.));
#31563=CARTESIAN_POINT('',(88.,-18.,12.));
#31564=CARTESIAN_POINT('',(88.,-15.,12.));
#31565=CARTESIAN_POINT('',(88.,-18.,28.));
#31566=CARTESIAN_POINT('',(88.,-18.,34.));
#31567=CARTESIAN_POINT('',(88.,-15.,28.));
#31568=CARTESIAN_POINT('Origin',(88.,30.,40.));
#31569=CARTESIAN_POINT('',(95.3939201416946,30.,40.));
#31570=CARTESIAN_POINT('',(95.3939201416946,30.,10.));
#31571=CARTESIAN_POINT('',(95.3939201416946,30.,0.));
#31572=CARTESIAN_POINT('',(44.,30.,40.));
#31573=CARTESIAN_POINT('',(108.,30.,10.));
#31574=CARTESIAN_POINT('Origin',(98.,0.,10.));
#31575=CARTESIAN_POINT('Origin',(0.,0.,10.));
#31576=CARTESIAN_POINT('Origin',(-18.,-18.,28.));
#31577=CARTESIAN_POINT('',(-90.,-18.,28.));
#31578=CARTESIAN_POINT('',(-90.,-18.,12.));
#31579=CARTESIAN_POINT('Origin',(-54.,0.,28.));
#31580=CARTESIAN_POINT('',(-18.,-12.,28.));
#31581=CARTESIAN_POINT('',(-90.,-12.,28.));
#31582=CARTESIAN_POINT('',(-18.,-18.,28.));
#31583=CARTESIAN_POINT('Origin',(-18.,-12.,40.));
#31584=CARTESIAN_POINT('',(-18.,-12.,40.));
#31585=CARTESIAN_POINT('Origin',(0.,0.,0.));
#31586=CARTESIAN_POINT('',(-100.,-1.22464679914735E-14,0.));
#31587=CARTESIAN_POINT('',(-100.,-1.22464679914735E-14,0.));
#31588=CARTESIAN_POINT('Origin',(0.,0.,0.));
#31589=CARTESIAN_POINT('Origin',(0.,0.,40.));
#31590=CARTESIAN_POINT('Origin',(90.,-12.,40.));
#31591=CARTESIAN_POINT('',(18.,-12.,28.));
#31592=CARTESIAN_POINT('',(18.,-12.,28.));
#31593=CARTESIAN_POINT('',(18.,-12.,40.));
#31594=CARTESIAN_POINT('Origin',(54.,0.,28.));
#31595=CARTESIAN_POINT('',(18.,-18.,28.));
#31596=CARTESIAN_POINT('',(18.,18.,28.));
#31597=CARTESIAN_POINT('Origin',(0.,0.,40.));
#31598=CARTESIAN_POINT('',(18.,12.,40.));
#31599=CARTESIAN_POINT('',(18.,-6.,40.));
#31600=CARTESIAN_POINT('',(9.,12.,40.));
#31601=CARTESIAN_POINT('Origin',(90.,-18.,28.));
#31602=CARTESIAN_POINT('',(18.,-18.,12.));
#31603=CARTESIAN_POINT('Origin',(54.,0.,12.));
#31604=CARTESIAN_POINT('',(90.,18.,12.));
#31605=CARTESIAN_POINT('',(18.,18.,12.));
#31606=CARTESIAN_POINT('',(18.,18.,12.));
#31607=CARTESIAN_POINT('Origin',(18.,18.,28.));
#31608=CARTESIAN_POINT('',(90.,18.,28.));
#31609=CARTESIAN_POINT('Origin',(-54.,0.,12.));
#31610=CARTESIAN_POINT('',(-18.,-18.,12.));
#31611=CARTESIAN_POINT('',(-18.,-18.,12.));
#31612=CARTESIAN_POINT('',(-18.,18.,12.));
#31613=CARTESIAN_POINT('Origin',(-54.,0.,28.));
#31614=CARTESIAN_POINT('',(-18.,18.,28.));
#31615=CARTESIAN_POINT('',(-18.,12.,28.));
#31616=CARTESIAN_POINT('',(-18.,-18.,28.));
#31617=CARTESIAN_POINT('',(-18.,12.,28.));
#31618=CARTESIAN_POINT('Origin',(-90.,18.,28.));
#31619=CARTESIAN_POINT('Origin',(54.,0.,28.));
#31620=CARTESIAN_POINT('',(18.,12.,28.));
#31621=CARTESIAN_POINT('',(90.,12.,28.));
#31622=CARTESIAN_POINT('',(18.,18.,28.));
#31623=CARTESIAN_POINT('Origin',(-18.,12.,40.));
#31624=CARTESIAN_POINT('Origin',(-18.,12.,40.));
#31625=CARTESIAN_POINT('',(-18.,12.,40.));
#31626=CARTESIAN_POINT('Origin',(-90.,12.,40.));
#31627=CARTESIAN_POINT('Origin',(18.,-12.,40.));
#31628=CARTESIAN_POINT('Origin',(18.,12.,40.));
#31629=CARTESIAN_POINT('',(18.,12.,40.));
#31630=CARTESIAN_POINT('Origin',(18.,-12.,40.));
#31631=CARTESIAN_POINT('Origin',(0.,0.,2.));
#31632=CARTESIAN_POINT('',(40.,4.89858719658941E-15,0.));
#31633=CARTESIAN_POINT('Origin',(0.,0.,0.));
#31634=CARTESIAN_POINT('',(40.,4.89858719658941E-15,4.));
#31635=CARTESIAN_POINT('',(40.,4.89858719658941E-15,2.));
#31636=CARTESIAN_POINT('Origin',(0.,0.,4.));
#31637=CARTESIAN_POINT('Origin',(0.,0.,4.));
#31638=CARTESIAN_POINT('Origin',(0.,0.,0.));
#31639=CARTESIAN_POINT('',(0.,0.,0.));
#31640=CARTESIAN_POINT('Origin',(-46.,-46.,-5.));
#31641=CARTESIAN_POINT('',(-49.3908050820932,-46.0028114959068,-8.26601780324957));
#31642=CARTESIAN_POINT('',(-49.3955875711091,-46.0001574069683,-8.60898219675042));
#31643=CARTESIAN_POINT('',(-49.38975,-46.,-5.));
#31644=CARTESIAN_POINT('',(-44.696617959125,-42.8708467090881,-9.));
#31645=CARTESIAN_POINT('Ctrl Pts',(-49.3955875711091,-46.0001574069683,
-8.60898219675042));
#31646=CARTESIAN_POINT('Ctrl Pts',(-49.3946782964034,-44.8964214045499,
-8.67403394523185));
#31647=CARTESIAN_POINT('Ctrl Pts',(-48.8034217891345,-43.7921194509379,
-8.73908569371328));
#31648=CARTESIAN_POINT('Ctrl Pts',(-47.8878787982433,-43.1790120886306,
-8.80413744219471));
#31649=CARTESIAN_POINT('Ctrl Pts',(-46.9690175523237,-42.5636826061082,
-8.86942496146314));
#31650=CARTESIAN_POINT('Ctrl Pts',(-45.723514902722,-42.4431146967252,-8.93471248073157));
#31651=CARTESIAN_POINT('Ctrl Pts',(-44.696617959125,-42.8708467090881,-9.));
#31652=CARTESIAN_POINT('',(-49.38975,-46.,-9.));
#31653=CARTESIAN_POINT('Origin',(-46.,-46.,-9.));
#31654=CARTESIAN_POINT('',(-49.38975,-46.,-10.));
#31655=CARTESIAN_POINT('',(-49.38975,-46.,-5.));
#31656=CARTESIAN_POINT('Origin',(-46.,-46.,-10.));
#31657=CARTESIAN_POINT('',(-43.1019982053025,-47.7690579931343,-9.));
#31658=CARTESIAN_POINT('Origin',(-46.,-46.,-9.));
#31659=CARTESIAN_POINT('Ctrl Pts',(-43.1019720879323,-47.7690801693092,
-9.));
#31660=CARTESIAN_POINT('Ctrl Pts',(-42.5564934135711,-46.8680833947406,
-8.9379383670794));
#31661=CARTESIAN_POINT('Ctrl Pts',(-42.4589272462208,-45.6899359380158,
-8.87587673415881));
#31662=CARTESIAN_POINT('Ctrl Pts',(-42.857579160951,-44.7152009935522,-8.81381510123821));
#31663=CARTESIAN_POINT('Ctrl Pts',(-43.2769525054721,-43.6898005412357,
-8.74852758196978));
#31664=CARTESIAN_POINT('Ctrl Pts',(-44.2454702047504,-42.8895084371012,
-8.68324006270134));
#31665=CARTESIAN_POINT('Ctrl Pts',(-45.3313096516499,-42.6714409964239,
-8.61795254343291));
#31666=CARTESIAN_POINT('Ctrl Pts',(-46.4171490985494,-42.4533735557466,
-8.55266502416448));
#31667=CARTESIAN_POINT('Ctrl Pts',(-47.6203102930703,-42.8175307785264,
-8.48737750489605));
#31668=CARTESIAN_POINT('Ctrl Pts',(-48.4028923648305,-43.6014277710615,
-8.42208998562762));
#31669=CARTESIAN_POINT('Ctrl Pts',(-49.0264893054514,-44.2260725002811,
-8.37006592483494));
#31670=CARTESIAN_POINT('Ctrl Pts',(-49.3830342221214,-45.1172362956638,
-8.31804186404226));
#31671=CARTESIAN_POINT('Ctrl Pts',(-49.3908050820932,-46.0028114959068,
-8.26601780324957));
#31672=CARTESIAN_POINT('Origin',(-46.,-46.,-5.));
#31673=CARTESIAN_POINT('',(-49.3915791156511,-45.9973272796015,-7.01601780324957));
#31674=CARTESIAN_POINT('',(-49.3858576553579,-45.9980711564067,-7.35898219675043));
#31675=CARTESIAN_POINT('',(-49.38975,-46.,-5.));
#31676=CARTESIAN_POINT('Ctrl Pts',(-49.3858576553579,-45.9980711564067,
-7.35898219675043));
#31677=CARTESIAN_POINT('Ctrl Pts',(-49.3881113941792,-45.5759581157443,
-7.3836879770195));
#31678=CARTESIAN_POINT('Ctrl Pts',(-49.3147699482676,-45.154598996582,-7.40839375728857));
#31679=CARTESIAN_POINT('Ctrl Pts',(-49.1621982248071,-44.7642017499235,
-7.43309953755765));
#31680=CARTESIAN_POINT('Ctrl Pts',(-48.7590120381433,-43.7325376014544,
-7.49838705682608));
#31681=CARTESIAN_POINT('Ctrl Pts',(-47.8025338878601,-42.9170907346222,
-7.56367457609451));
#31682=CARTESIAN_POINT('Ctrl Pts',(-46.7201047416051,-42.6821547425348,
-7.62896209536294));
#31683=CARTESIAN_POINT('Ctrl Pts',(-45.63767559535,-42.4472187504474,-7.69424961463137));
#31684=CARTESIAN_POINT('Ctrl Pts',(-44.4292954531231,-42.7927936331048,
-7.7595371338998));
#31685=CARTESIAN_POINT('Ctrl Pts',(-43.6346772179205,-43.5644833691861,
-7.82482465316823));
#31686=CARTESIAN_POINT('Ctrl Pts',(-42.840058982718,-44.3361731052674,-7.89011217243666));
#31687=CARTESIAN_POINT('Ctrl Pts',(-42.4592026545397,-45.5339776947726,
-7.9553996917051));
#31688=CARTESIAN_POINT('Ctrl Pts',(-42.6624687214266,-46.622835827247,-8.02068721097353));
#31689=CARTESIAN_POINT('Ctrl Pts',(-42.8657347883135,-47.7116939597214,
-8.08597473024196));
#31690=CARTESIAN_POINT('Ctrl Pts',(-43.6531232502656,-48.691605635165,-8.15126224951039));
#31691=CARTESIAN_POINT('Ctrl Pts',(-44.6724331904996,-49.1247427427676,
-8.21654976877882));
#31692=CARTESIAN_POINT('Ctrl Pts',(-45.6917431307337,-49.5578798503701,
-8.28183728804725));
#31693=CARTESIAN_POINT('Ctrl Pts',(-46.9429745492497,-49.4442423901316,
-8.34712480731569));
#31694=CARTESIAN_POINT('Ctrl Pts',(-47.8680858853197,-48.8347434521096,
-8.41241232658412));
#31695=CARTESIAN_POINT('Ctrl Pts',(-48.7931972213897,-48.2252445140876,
-8.47769984585255));
#31696=CARTESIAN_POINT('Ctrl Pts',(-49.3921884750137,-47.1198840982822,
-8.54298736512098));
#31697=CARTESIAN_POINT('Ctrl Pts',(-49.395574180707,-46.0121583625486,-8.60827488438941));
#31698=CARTESIAN_POINT('Ctrl Pts',(-49.3955864074006,-46.0081580670644,
-8.60851065517641));
#31699=CARTESIAN_POINT('Ctrl Pts',(-49.3955908666456,-46.0041577407335,
-8.60874642596342));
#31700=CARTESIAN_POINT('Ctrl Pts',(-49.3955875711091,-46.0001574069683,
-8.60898219675042));
#31701=CARTESIAN_POINT('Ctrl Pts',(-49.3908050820932,-46.0028114959068,
-8.26601780324957));
#31702=CARTESIAN_POINT('Ctrl Pts',(-49.3927862515173,-46.2285876025122,
-8.25275434477382));
#31703=CARTESIAN_POINT('Ctrl Pts',(-49.3720975399661,-46.4540004573671,
-8.23949088629807));
#31704=CARTESIAN_POINT('Ctrl Pts',(-49.3273847039345,-46.6745408721824,
-8.22622742782233));
#31705=CARTESIAN_POINT('Ctrl Pts',(-49.1072920222784,-47.7601202184779,
-8.1609399085539));
#31706=CARTESIAN_POINT('Ctrl Pts',(-48.3051037099665,-48.7276421487786,
-8.09565238928547));
#31707=CARTESIAN_POINT('Ctrl Pts',(-47.2790835032418,-49.1449315523856,
-8.03036487001703));
#31708=CARTESIAN_POINT('Ctrl Pts',(-46.2530632965171,-49.5622209559926,
-7.9650773507486));
#31709=CARTESIAN_POINT('Ctrl Pts',(-45.0032111953795,-49.4292778329058,
-7.89978983148017));
#31710=CARTESIAN_POINT('Ctrl Pts',(-44.0879228271742,-48.805469104904,-7.83450231221174));
#31711=CARTESIAN_POINT('Ctrl Pts',(-43.1726344589688,-48.1816603769021,
-7.76921479294331));
#31712=CARTESIAN_POINT('Ctrl Pts',(-42.5919098236955,-47.0669860439851,
-7.70392727367488));
#31713=CARTESIAN_POINT('Ctrl Pts',(-42.6051529380119,-45.9594166616959,
-7.63863975440645));
#31714=CARTESIAN_POINT('Ctrl Pts',(-42.6183960523284,-44.8518472794067,
-7.57335223513802));
#31715=CARTESIAN_POINT('Ctrl Pts',(-43.2256069162345,-43.7513828477454,
-7.50806471586959));
#31716=CARTESIAN_POINT('Ctrl Pts',(-44.155537258283,-43.149629262965,-7.44277719660115));
#31717=CARTESIAN_POINT('Ctrl Pts',(-45.0854676003314,-42.5478756781846,
-7.37748967733272));
#31718=CARTESIAN_POINT('Ctrl Pts',(-46.3381174205223,-42.4448329402852,
-7.31220215806429));
#31719=CARTESIAN_POINT('Ctrl Pts',(-47.3538838078074,-42.8865360920784,
-7.24691463879586));
#31720=CARTESIAN_POINT('Ctrl Pts',(-48.3696501950926,-43.3282392438716,
-7.18162711952743));
#31721=CARTESIAN_POINT('Ctrl Pts',(-49.1485331494721,-44.3146882853574,
-7.116339600259));
#31722=CARTESIAN_POINT('Ctrl Pts',(-49.3425844160128,-45.4052047263581,
-7.05105208099057));
#31723=CARTESIAN_POINT('Ctrl Pts',(-49.3772947049224,-45.6002673064819,
-7.03937398841023));
#31724=CARTESIAN_POINT('Ctrl Pts',(-49.3932932445553,-45.7986595336273,
-7.0276958958299));
#31725=CARTESIAN_POINT('Ctrl Pts',(-49.3915791156511,-45.9973272796015,
-7.01601780324957));
#31726=CARTESIAN_POINT('Origin',(-46.,-46.,-5.));
#31727=CARTESIAN_POINT('',(-49.3849269836833,-46.0010327956957,-5.76601780324957));
#31728=CARTESIAN_POINT('',(-49.3896326160374,-46.0028925919798,-6.10898219675042));
#31729=CARTESIAN_POINT('',(-49.38975,-46.,-5.));
#31730=CARTESIAN_POINT('Ctrl Pts',(-49.3896326160374,-46.0028925919798,
-6.10898219675042));
#31731=CARTESIAN_POINT('Ctrl Pts',(-49.3822316042023,-45.1570406462268,
-6.15862952807558));
#31732=CARTESIAN_POINT('Ctrl Pts',(-49.0605617986376,-44.3061622980437,
-6.20827685940073));
#31733=CARTESIAN_POINT('Ctrl Pts',(-48.4872408503176,-43.6890939238723,
-6.25792419072589));
#31734=CARTESIAN_POINT('Ctrl Pts',(-47.7333090384487,-42.8776331203741,
-6.32321170999432));
#31735=CARTESIAN_POINT('Ctrl Pts',(-46.5441987345435,-42.470498205483,-6.38849922926275));
#31736=CARTESIAN_POINT('Ctrl Pts',(-45.4511228720662,-42.6495690045761,
-6.45378674853118));
#31737=CARTESIAN_POINT('Ctrl Pts',(-44.3580470095889,-42.8286398036693,
-6.51907426779961));
#31738=CARTESIAN_POINT('Ctrl Pts',(-43.3610055885394,-43.5939163167467,
-6.58436178706804));
#31739=CARTESIAN_POINT('Ctrl Pts',(-42.9054062548915,-44.6035257121301,
-6.64964930633647));
#31740=CARTESIAN_POINT('Ctrl Pts',(-42.4498069212435,-45.6131351075136,
-6.71493682560491));
#31741=CARTESIAN_POINT('Ctrl Pts',(-42.5356496749971,-46.8670773852031,
-6.78022434487333));
#31742=CARTESIAN_POINT('Ctrl Pts',(-43.1245889322668,-47.8051783725204,
-6.84551186414177));
#31743=CARTESIAN_POINT('Ctrl Pts',(-43.7135281895365,-48.7432793598376,
-6.9107993834102));
#31744=CARTESIAN_POINT('Ctrl Pts',(-44.8055639503223,-49.3655390567825,
-6.97608690267863));
#31745=CARTESIAN_POINT('Ctrl Pts',(-45.9128440217905,-49.3939739060678,
-7.04137442194706));
#31746=CARTESIAN_POINT('Ctrl Pts',(-47.0201240932587,-49.4224087553532,
-7.10666194121549));
#31747=CARTESIAN_POINT('Ctrl Pts',(-48.1426484754094,-48.857018756979,-7.17194946048392));
#31748=CARTESIAN_POINT('Ctrl Pts',(-48.7789635549624,-47.9503830427389,
-7.23723697975236));
#31749=CARTESIAN_POINT('Ctrl Pts',(-49.174487427965,-47.3868319331997,-7.27781871875171));
#31750=CARTESIAN_POINT('Ctrl Pts',(-49.3821556617506,-46.6914344526808,
-7.31840045775107));
#31751=CARTESIAN_POINT('Ctrl Pts',(-49.3858576553579,-45.9980711564067,
-7.35898219675043));
#31752=CARTESIAN_POINT('Ctrl Pts',(-49.3915791156511,-45.9973272796015,
-7.01601780324957));
#31753=CARTESIAN_POINT('Ctrl Pts',(-49.3837102391892,-46.909331007079,-6.96240837656147));
#31754=CARTESIAN_POINT('Ctrl Pts',(-49.0025718726505,-47.8271409050093,
-6.90879894987337));
#31755=CARTESIAN_POINT('Ctrl Pts',(-48.3448154570193,-48.4552994801616,
-6.85518952318527));
#31756=CARTESIAN_POINT('Ctrl Pts',(-47.5437756527831,-49.2202939524488,
-6.78990200391684));
#31757=CARTESIAN_POINT('Ctrl Pts',(-46.3324764656086,-49.5556990565077,
-6.72461448464841));
#31758=CARTESIAN_POINT('Ctrl Pts',(-45.2520432244852,-49.3116786847004,
-6.65932696537998));
#31759=CARTESIAN_POINT('Ctrl Pts',(-44.1716099833619,-49.0676583128931,
-6.59403944611155));
#31760=CARTESIAN_POINT('Ctrl Pts',(-43.2220426882898,-48.2442124652195,
-6.52875192684312));
#31761=CARTESIAN_POINT('Ctrl Pts',(-42.8275419844485,-47.209199926625,-6.46346440757469));
#31762=CARTESIAN_POINT('Ctrl Pts',(-42.4330412806072,-46.1741873880306,
-6.39817688830626));
#31763=CARTESIAN_POINT('Ctrl Pts',(-42.5936071679967,-44.9276081585153,
-6.33288936903782));
#31764=CARTESIAN_POINT('Ctrl Pts',(-43.2375100754716,-44.026347513733,-6.26760184976939));
#31765=CARTESIAN_POINT('Ctrl Pts',(-43.8814129829466,-43.1250868689506,
-6.20231433050096));
#31766=CARTESIAN_POINT('Ctrl Pts',(-45.008652910507,-42.5691448089011,-6.13702681123253));
#31767=CARTESIAN_POINT('Ctrl Pts',(-46.1156569734068,-42.6068778178316,
-6.0717392919641));
#31768=CARTESIAN_POINT('Ctrl Pts',(-47.2226610363066,-42.6446108267621,
-6.00645177269567));
#31769=CARTESIAN_POINT('Ctrl Pts',(-48.3094292345459,-43.2760189046725,
-5.94116425342724));
#31770=CARTESIAN_POINT('Ctrl Pts',(-48.8904687669622,-44.2190325906619,
-5.87587673415881));
#31771=CARTESIAN_POINT('Ctrl Pts',(-49.2163727200328,-44.7479671483254,
-5.83925709052239));
#31772=CARTESIAN_POINT('Ctrl Pts',(-49.383171073577,-45.3749349013358,-5.80263744688598));
#31773=CARTESIAN_POINT('Ctrl Pts',(-49.3849269836833,-46.0010327956957,
-5.76601780324957));
#31774=CARTESIAN_POINT('Origin',(-46.,-46.,-5.));
#31775=CARTESIAN_POINT('',(-49.3946337481228,-46.0010845676627,-4.51601780324957));
#31776=CARTESIAN_POINT('',(-49.3926793474262,-45.9976551524526,-4.85898219675043));
#31777=CARTESIAN_POINT('',(-49.38975,-46.,-5.));
#31778=CARTESIAN_POINT('Ctrl Pts',(-49.3926793474262,-45.9976551524526,
-4.85898219675043));
#31779=CARTESIAN_POINT('Ctrl Pts',(-49.3939351810614,-45.8395538986053,
-4.86828355986323));
#31780=CARTESIAN_POINT('Ctrl Pts',(-49.3838123532219,-45.6816141300476,
-4.87758492297603));
#31781=CARTESIAN_POINT('Ctrl Pts',(-49.3617510816055,-45.5253599306122,
-4.88688628608883));
#31782=CARTESIAN_POINT('Ctrl Pts',(-49.206900047593,-44.4285906794074,-4.95217380535726));
#31783=CARTESIAN_POINT('Ctrl Pts',(-48.4638627815182,-43.4148664690314,
-5.0174613246257));
#31784=CARTESIAN_POINT('Ctrl Pts',(-47.4645769192664,-42.9370491377502,
-5.08274884389413));
#31785=CARTESIAN_POINT('Ctrl Pts',(-46.4652910570147,-42.459231806469,-5.14803636316256));
#31786=CARTESIAN_POINT('Ctrl Pts',(-45.2097565985859,-42.5173213542825,
-5.21332388243099));
#31787=CARTESIAN_POINT('Ctrl Pts',(-44.2588594812185,-43.0853673919219,
-5.27861140169942));
#31788=CARTESIAN_POINT('Ctrl Pts',(-43.307962363851,-43.6534134295613,-5.34389892096785));
#31789=CARTESIAN_POINT('Ctrl Pts',(-42.6617025875449,-44.7314159570266,
-5.40918644023628));
#31790=CARTESIAN_POINT('Ctrl Pts',(-42.6087842862726,-45.8377980273576,
-5.47447395950471));
#31791=CARTESIAN_POINT('Ctrl Pts',(-42.5558659850004,-46.9441800976885,
-5.53976147877314));
#31792=CARTESIAN_POINT('Ctrl Pts',(-43.0962891587621,-48.0789417108851,
-5.60504899804157));
#31793=CARTESIAN_POINT('Ctrl Pts',(-43.9886301660516,-48.7351498973253,
-5.67033651731001));
#31794=CARTESIAN_POINT('Ctrl Pts',(-44.8809711733411,-49.3913580837655,
-5.73562403657844));
#31795=CARTESIAN_POINT('Ctrl Pts',(-46.1252300141585,-49.5690128434493,
-5.80091155584687));
#31796=CARTESIAN_POINT('Ctrl Pts',(-47.1655578423799,-49.1887503080326,
-5.8661990751153));
#31797=CARTESIAN_POINT('Ctrl Pts',(-48.2058856706013,-48.8084877726158,
-5.93148659438373));
#31798=CARTESIAN_POINT('Ctrl Pts',(-49.0422824862267,-47.8703079420985,
-5.99677411365216));
#31799=CARTESIAN_POINT('Ctrl Pts',(-49.3011042341231,-46.7933246807872,
-6.06206163292059));
#31800=CARTESIAN_POINT('Ctrl Pts',(-49.3631072145742,-46.5353240581962,
-6.07770182086387));
#31801=CARTESIAN_POINT('Ctrl Pts',(-49.3919641253649,-46.2693577382557,
-6.09334200880715));
#31802=CARTESIAN_POINT('Ctrl Pts',(-49.3896326160374,-46.0028925919798,
-6.10898219675042));
#31803=CARTESIAN_POINT('Ctrl Pts',(-49.3849269836833,-46.0010327956957,
-5.76601780324957));
#31804=CARTESIAN_POINT('Ctrl Pts',(-49.3863016069059,-46.4911767399457,
-5.73734992761755));
#31805=CARTESIAN_POINT('Ctrl Pts',(-49.2865279643948,-46.980787580758,-5.70868205198553));
#31806=CARTESIAN_POINT('Ctrl Pts',(-49.0827576637059,-47.4224133864494,
-5.68001417635351));
#31807=CARTESIAN_POINT('Ctrl Pts',(-48.61869616144,-48.428161202179,-5.61472665708508));
#31808=CARTESIAN_POINT('Ctrl Pts',(-47.6152622903149,-49.1850375395698,
-5.54943913781665));
#31809=CARTESIAN_POINT('Ctrl Pts',(-46.5207208867884,-49.354922414,-5.48415161854822));
#31810=CARTESIAN_POINT('Ctrl Pts',(-45.426179483262,-49.5248072884302,-5.41886409927979));
#31811=CARTESIAN_POINT('Ctrl Pts',(-44.2405305473341,-49.1077006998998,
-5.35357658001135));
#31812=CARTESIAN_POINT('Ctrl Pts',(-43.4934399857245,-48.2899370152651,
-5.28828906074292));
#31813=CARTESIAN_POINT('Ctrl Pts',(-42.7463494241149,-47.4721733306304,
-5.22300154147449));
#31814=CARTESIAN_POINT('Ctrl Pts',(-42.4378172368234,-46.2537525498914,
-5.15771402220606));
#31815=CARTESIAN_POINT('Ctrl Pts',(-42.7056742603893,-45.1789807759279,
-5.09242650293763));
#31816=CARTESIAN_POINT('Ctrl Pts',(-42.9735312839552,-44.1042090019644,
-5.0271389836692));
#31817=CARTESIAN_POINT('Ctrl Pts',(-43.8177775183786,-43.1730862347763,
-4.96185146440077));
#31818=CARTESIAN_POINT('Ctrl Pts',(-44.8612621572759,-42.801573704276,-4.89656394513234));
#31819=CARTESIAN_POINT('Ctrl Pts',(-45.9047467961732,-42.4300611737756,
-4.83127642586391));
#31820=CARTESIAN_POINT('Ctrl Pts',(-47.1474698395444,-42.618158879963,-4.76598890659548));
#31821=CARTESIAN_POINT('Ctrl Pts',(-48.0342686144742,-43.2818377814125,
-4.70070138732704));
#31822=CARTESIAN_POINT('Ctrl Pts',(-48.8704528139696,-43.9076368089027,
-4.63914019263455));
#31823=CARTESIAN_POINT('Ctrl Pts',(-49.3901824623747,-44.9562781289759,
-4.57757899794206));
#31824=CARTESIAN_POINT('Ctrl Pts',(-49.3946337481228,-46.0010845676627,
-4.51601780324957));
#31825=CARTESIAN_POINT('Origin',(-46.,-46.,-5.));
#31826=CARTESIAN_POINT('',(-49.3870908106244,-45.9974837229373,-3.26601780324957));
#31827=CARTESIAN_POINT('',(-49.3846593199306,-46.0004230001441,-3.60898219675043));
#31828=CARTESIAN_POINT('',(-49.38975,-46.,-5.));
#31829=CARTESIAN_POINT('Ctrl Pts',(-49.3846593199306,-46.0004230001441,
-3.60898219675043));
#31830=CARTESIAN_POINT('Ctrl Pts',(-49.3839900131623,-45.4148448050876,
-3.64322511091931));
#31831=CARTESIAN_POINT('Ctrl Pts',(-49.2392620998284,-44.8289567285941,
-3.67746802508819));
#31832=CARTESIAN_POINT('Ctrl Pts',(-48.9524290200888,-44.3237492993344,
-3.71171093925707));
#31833=CARTESIAN_POINT('Ctrl Pts',(-48.4055532452068,-43.3605211228516,
-3.7769984585255));
#31834=CARTESIAN_POINT('Ctrl Pts',(-47.3421079624348,-42.6905768803167,
-3.84228597779393));
#31835=CARTESIAN_POINT('Ctrl Pts',(-46.2371669440815,-42.6132013085067,
-3.90757349706236));
#31836=CARTESIAN_POINT('Ctrl Pts',(-45.1322259257282,-42.5358257366966,
-3.97286101633079));
#31837=CARTESIAN_POINT('Ctrl Pts',(-43.9857891717937,-43.0510188356115,
-4.03814853559923));
#31838=CARTESIAN_POINT('Ctrl Pts',(-43.3100053044936,-43.9286279733269,
-4.10343605486766));
#31839=CARTESIAN_POINT('Ctrl Pts',(-42.6342214371935,-44.8062371110423,
-4.16872357413609));
#31840=CARTESIAN_POINT('Ctrl Pts',(-42.4290904565277,-46.0462622875582,
-4.23401109340452));
#31841=CARTESIAN_POINT('Ctrl Pts',(-42.7862506912548,-47.0947460500201,
-4.29929861267295));
#31842=CARTESIAN_POINT('Ctrl Pts',(-43.1434109259818,-48.143229812482,-4.36458613194138));
#31843=CARTESIAN_POINT('Ctrl Pts',(-44.0628623761017,-49.0001721608899,
-4.42987365120981));
#31844=CARTESIAN_POINT('Ctrl Pts',(-45.1338577500445,-49.2827505445249,
-4.49516117047825));
#31845=CARTESIAN_POINT('Ctrl Pts',(-46.2048531239873,-49.56532892816,-4.56044868974668));
#31846=CARTESIAN_POINT('Ctrl Pts',(-47.427392421753,-49.2735433470222,-4.62573620901511));
#31847=CARTESIAN_POINT('Ctrl Pts',(-48.2553296696607,-48.5377434104365,
-4.69102372828354));
#31848=CARTESIAN_POINT('Ctrl Pts',(-48.9653125969923,-47.9067712030286,
-4.74700988443917));
#31849=CARTESIAN_POINT('Ctrl Pts',(-49.3851203157927,-46.9492878732649,
-4.8029960405948));
#31850=CARTESIAN_POINT('Ctrl Pts',(-49.3926793474262,-45.9976551524526,
-4.85898219675043));
#31851=CARTESIAN_POINT('Ctrl Pts',(-49.3946337481228,-46.0010845676627,
-4.51601780324957));
#31852=CARTESIAN_POINT('Ctrl Pts',(-49.3949031862901,-46.0643271335198,
-4.51229147867363));
#31853=CARTESIAN_POINT('Ctrl Pts',(-49.3932846801065,-46.1275556486361,
-4.50856515409769));
#31854=CARTESIAN_POINT('Ctrl Pts',(-49.3897341345749,-46.1906754848652,
-4.50483882952175));
#31855=CARTESIAN_POINT('Ctrl Pts',(-49.3275263732576,-47.2965741901566,
-4.43955131025332));
#31856=CARTESIAN_POINT('Ctrl Pts',(-48.6722363441346,-48.3691115040278,
-4.37426379098489));
#31857=CARTESIAN_POINT('Ctrl Pts',(-47.7166022939084,-48.9291519608081,
-4.30897627171646));
#31858=CARTESIAN_POINT('Ctrl Pts',(-46.7609682436823,-49.4891924175884,
-4.24368875244803));
#31859=CARTESIAN_POINT('Ctrl Pts',(-45.504990172353,-49.5367360172778,-4.1784012331796));
#31860=CARTESIAN_POINT('Ctrl Pts',(-44.5097521823566,-49.0505435714074,
-4.11311371391116));
#31861=CARTESIAN_POINT('Ctrl Pts',(-43.5145141923602,-48.564351125537,-4.04782619464273));
#31862=CARTESIAN_POINT('Ctrl Pts',(-42.7800162836966,-47.5444226341068,
-3.9825386753743));
#31863=CARTESIAN_POINT('Ctrl Pts',(-42.6343813038521,-46.4463915747831,
-3.91725115610587));
#31864=CARTESIAN_POINT('Ctrl Pts',(-42.4887463240076,-45.3483605154594,
-3.85196363683744));
#31865=CARTESIAN_POINT('Ctrl Pts',(-42.9319742729821,-44.1722268882422,
-3.78667611756901));
#31866=CARTESIAN_POINT('Ctrl Pts',(-43.766061567924,-43.4434058326004,-3.72138859830058));
#31867=CARTESIAN_POINT('Ctrl Pts',(-44.6001488628658,-42.7145847769586,
-3.65610107903215));
#31868=CARTESIAN_POINT('Ctrl Pts',(-45.8250955037749,-42.4330762928922,
-3.59081355976371));
#31869=CARTESIAN_POINT('Ctrl Pts',(-46.8936800870826,-42.724638873672,-3.52552604049528));
#31870=CARTESIAN_POINT('Ctrl Pts',(-47.9622646703903,-43.0162014544519,
-3.46023852122685));
#31871=CARTESIAN_POINT('Ctrl Pts',(-48.8744871960966,-43.880835100078,-3.39495100195842));
#31872=CARTESIAN_POINT('Ctrl Pts',(-49.2228297485814,-44.9322813618375,
-3.32966348268999));
#31873=CARTESIAN_POINT('Ctrl Pts',(-49.3360239122814,-45.2739495830363,
-3.30844825620985));
#31874=CARTESIAN_POINT('Ctrl Pts',(-49.3896763141562,-45.6353439034476,
-3.28723302972971));
#31875=CARTESIAN_POINT('Ctrl Pts',(-49.3870908106244,-45.9974837229373,
-3.26601780324957));
#31876=CARTESIAN_POINT('Origin',(-46.,-46.,-5.));
#31877=CARTESIAN_POINT('',(-49.3879806100937,-46.0027475395409,-2.01601780324957));
#31878=CARTESIAN_POINT('',(-49.393944259473,-46.0016943208402,-2.35898219675043));
#31879=CARTESIAN_POINT('',(-49.38975,-46.,-5.));
#31880=CARTESIAN_POINT('Ctrl Pts',(-49.393944259473,-46.0016943208402,-2.35898219675043));
#31881=CARTESIAN_POINT('Ctrl Pts',(-49.3877066726979,-44.9966831864109,
-2.41816666197539));
#31882=CARTESIAN_POINT('Ctrl Pts',(-48.9121874363056,-43.9865344276296,
-2.47735112720035));
#31883=CARTESIAN_POINT('Ctrl Pts',(-48.1303608079629,-43.3564765857691,
-2.53653559242531));
#31884=CARTESIAN_POINT('Ctrl Pts',(-47.2679128519243,-42.6614476903598,
-2.60182311169374));
#31885=CARTESIAN_POINT('Ctrl Pts',(-46.0327280241684,-42.4289407681851,
-2.66711063096217));
#31886=CARTESIAN_POINT('Ctrl Pts',(-44.9766013247455,-42.7628239525169,
-2.7323981502306));
#31887=CARTESIAN_POINT('Ctrl Pts',(-43.9204746253226,-43.0967071368487,
-2.79768566949903));
#31888=CARTESIAN_POINT('Ctrl Pts',(-43.0434060542328,-43.9969804276871,
-2.86297318876746));
#31889=CARTESIAN_POINT('Ctrl Pts',(-42.7372092246985,-45.0614639450911,
-2.9282607080359));
#31890=CARTESIAN_POINT('Ctrl Pts',(-42.4310123951642,-46.1259474624951,
-2.99354822730433));
#31891=CARTESIAN_POINT('Ctrl Pts',(-42.6956873071853,-47.3546412064646,
-3.05883574657276));
#31892=CARTESIAN_POINT('Ctrl Pts',(-43.4129954937812,-48.1986498542888,
-3.12412326584119));
#31893=CARTESIAN_POINT('Ctrl Pts',(-44.1303036803771,-49.0426585021129,
-3.18941078510962));
#31894=CARTESIAN_POINT('Ctrl Pts',(-45.3002451415477,-49.5019820537916,
-3.25469830437805));
#31895=CARTESIAN_POINT('Ctrl Pts',(-46.4001709931723,-49.371426511499,-3.31998582364648));
#31896=CARTESIAN_POINT('Ctrl Pts',(-47.500096844797,-49.2408709692064,-3.38527334291492));
#31897=CARTESIAN_POINT('Ctrl Pts',(-48.5300070868757,-48.5204363329426,
-3.45056086218335));
#31898=CARTESIAN_POINT('Ctrl Pts',(-49.0298090744191,-47.5319629595953,
-3.51584838145178));
#31899=CARTESIAN_POINT('Ctrl Pts',(-49.2674679027085,-47.0619379705799,
-3.54689298655133));
#31900=CARTESIAN_POINT('Ctrl Pts',(-49.3852661130384,-46.5313078346175,
-3.57793759165088));
#31901=CARTESIAN_POINT('Ctrl Pts',(-49.3846593199306,-46.0004230001441,
-3.60898219675043));
#31902=CARTESIAN_POINT('Ctrl Pts',(-49.3870908106244,-45.9974837229373,
-3.26601780324957));
#31903=CARTESIAN_POINT('Ctrl Pts',(-49.3817197122406,-46.749789250752,-3.22194551046128));
#31904=CARTESIAN_POINT('Ctrl Pts',(-49.1336512376201,-47.5053120155708,
-3.17787321767299));
#31905=CARTESIAN_POINT('Ctrl Pts',(-48.6725047066197,-48.0938895178028,
-3.1338009248847));
#31906=CARTESIAN_POINT('Ctrl Pts',(-47.9893745329099,-48.9657925341156,
-3.06851340561626));
#31907=CARTESIAN_POINT('Ctrl Pts',(-46.838651606227,-49.4713396888484,-3.00322588634783));
#31908=CARTESIAN_POINT('Ctrl Pts',(-45.734399285881,-49.38468766412,-2.9379383670794));
#31909=CARTESIAN_POINT('Ctrl Pts',(-44.630146965535,-49.2980356393917,-2.87265084781097));
#31910=CARTESIAN_POINT('Ctrl Pts',(-43.572365251526,-48.6191844352022,-2.80736332854254));
#31911=CARTESIAN_POINT('Ctrl Pts',(-43.0335978832048,-47.651397447682,-2.74207580927411));
#31912=CARTESIAN_POINT('Ctrl Pts',(-42.4948305148836,-46.6836104601617,
-2.67678829000568));
#31913=CARTESIAN_POINT('Ctrl Pts',(-42.4750774922503,-45.4268876893108,
-2.61150077073725));
#31914=CARTESIAN_POINT('Ctrl Pts',(-42.9831629846654,-44.4426466400763,
-2.54621325146882));
#31915=CARTESIAN_POINT('Ctrl Pts',(-43.4912484770806,-43.4584055908418,
-2.48092573220038));
#31916=CARTESIAN_POINT('Ctrl Pts',(-44.5271724845442,-42.7466462632239,
-2.41563821293195));
#31917=CARTESIAN_POINT('Ctrl Pts',(-45.6281560686778,-42.6253320035213,
-2.35035069366352));
#31918=CARTESIAN_POINT('Ctrl Pts',(-46.7291396528114,-42.5040177438187,
-2.28506317439509));
#31919=CARTESIAN_POINT('Ctrl Pts',(-47.895182813615,-42.9731485520315,-2.21977565512666));
#31920=CARTESIAN_POINT('Ctrl Pts',(-48.6053776654248,-43.8231522580853,
-2.15448813585823));
#31921=CARTESIAN_POINT('Ctrl Pts',(-49.1074691240937,-44.4240853675818,
-2.10833135832201));
#31922=CARTESIAN_POINT('Ctrl Pts',(-49.38172005634,-45.2153850526079,-2.06217458078579));
#31923=CARTESIAN_POINT('Ctrl Pts',(-49.3879806100937,-46.0027475395409,
-2.01601780324957));
#31924=CARTESIAN_POINT('Origin',(-46.,-46.,-5.));
#31925=CARTESIAN_POINT('',(-49.3940299756876,-45.9984545908008,-0.766017803249567));
#31926=CARTESIAN_POINT('',(-49.3881103126091,-45.9972329022571,-1.10898219675043));
#31927=CARTESIAN_POINT('',(-49.38975,-46.,-5.));
#31928=CARTESIAN_POINT('',(-43.4267655729853,-43.7934484719077,0.));
#31929=CARTESIAN_POINT('Ctrl Pts',(-49.3940299756876,-45.9984545908008,
-0.766017803249567));
#31930=CARTESIAN_POINT('Ctrl Pts',(-49.3879993454613,-47.0081806098787,
-0.706541093305005));
#31931=CARTESIAN_POINT('Ctrl Pts',(-48.9072380108242,-48.0226965014984,
-0.647064383360443));
#31932=CARTESIAN_POINT('Ctrl Pts',(-48.1187311062663,-48.6526393867237,
-0.58758767341588));
#31933=CARTESIAN_POINT('Ctrl Pts',(-47.253187942016,-49.3441270008755,-0.522300154147449));
#31934=CARTESIAN_POINT('Ctrl Pts',(-46.0168289438377,-49.5722261083817,
-0.457012634879018));
#31935=CARTESIAN_POINT('Ctrl Pts',(-44.9622730887946,-49.2331401883368,
-0.391725115610587));
#31936=CARTESIAN_POINT('Ctrl Pts',(-43.9077172337516,-48.8940542682919,
-0.326437596342156));
#31937=CARTESIAN_POINT('Ctrl Pts',(-43.0349645218439,-47.9877833206959,
-0.261150077073725));
#31938=CARTESIAN_POINT('Ctrl Pts',(-42.7336951254951,-46.9237470138282,
-0.195862557805293));
#31939=CARTESIAN_POINT('Ctrl Pts',(-42.4324257291462,-45.8597107069604,
-0.130575038536862));
#31940=CARTESIAN_POINT('Ctrl Pts',(-42.7026396483563,-44.6379090408209,
-0.0652875192684313));
#31941=CARTESIAN_POINT('Ctrl Pts',(-43.4267655729853,-43.7934484719077,
0.));
#31942=CARTESIAN_POINT('',(-48.5780058196814,-43.790505499672,-2.89031293644395E-15));
#31943=CARTESIAN_POINT('Origin',(-46.,-46.,0.));
#31944=CARTESIAN_POINT('Ctrl Pts',(-48.5780349767683,-43.7904875157198,
-1.87350135405495E-15));
#31945=CARTESIAN_POINT('Ctrl Pts',(-47.8896982724427,-42.9932829946826,
-0.0620616329205986));
#31946=CARTESIAN_POINT('Ctrl Pts',(-46.7993631439962,-42.5364248278905,
-0.124123265841195));
#31947=CARTESIAN_POINT('Ctrl Pts',(-45.7491449767911,-42.6143557375973,
-0.186184898761792));
#31948=CARTESIAN_POINT('Ctrl Pts',(-44.6443377778701,-42.6963373988856,
-0.251472418030223));
#31949=CARTESIAN_POINT('Ctrl Pts',(-43.5839263871456,-43.3701483645673,
-0.316759937298654));
#31950=CARTESIAN_POINT('Ctrl Pts',(-43.0409891061667,-44.3354564071969,
-0.382047456567084));
#31951=CARTESIAN_POINT('Ctrl Pts',(-42.4980518251879,-45.3007644498266,
-0.447334975835515));
#31952=CARTESIAN_POINT('Ctrl Pts',(-42.4725886539547,-46.5575695694043,
-0.512622495103946));
#31953=CARTESIAN_POINT('Ctrl Pts',(-42.9762878118604,-47.5440868195973,
-0.577910014372377));
#31954=CARTESIAN_POINT('Ctrl Pts',(-43.4799869697661,-48.5306040697903,
-0.643197533640808));
#31955=CARTESIAN_POINT('Ctrl Pts',(-44.5128484568107,-49.2468334505987,
-0.708485052909239));
#31956=CARTESIAN_POINT('Ctrl Pts',(-45.6133080961662,-49.3729753177135,
-0.773772572177669));
#31957=CARTESIAN_POINT('Ctrl Pts',(-46.7137677355217,-49.4991171848283,
-0.8390600914461));
#31958=CARTESIAN_POINT('Ctrl Pts',(-47.8818255271881,-49.0351715382496,
-0.904347610714531));
#31959=CARTESIAN_POINT('Ctrl Pts',(-48.5957489780033,-48.1883179007084,
-0.969635129982962));
#31960=CARTESIAN_POINT('Ctrl Pts',(-49.1036721864121,-47.5858210697928,
-1.01608415223878));
#31961=CARTESIAN_POINT('Ctrl Pts',(-49.3817281116383,-46.7895092998299,
-1.06253317449461));
#31962=CARTESIAN_POINT('Ctrl Pts',(-49.3881103126091,-45.9972329022571,
-1.10898219675043));
#31963=CARTESIAN_POINT('Origin',(-46.,-46.,2.76038497140452));
#31964=CARTESIAN_POINT('',(-50.0803093213768,-45.997675543601,-7.76038497140452));
#31965=CARTESIAN_POINT('',(-50.0862714832512,-46.0033881438983,-7.86461502859548));
#31966=CARTESIAN_POINT('',(-50.085,-45.9999999999999,2.76038497140452));
#31967=CARTESIAN_POINT('',(-49.4256147683784,-48.2253962475631,-9.));
#31968=CARTESIAN_POINT('Ctrl Pts',(-50.0862714832512,-46.0033881438983,
-7.86461502859548));
#31969=CARTESIAN_POINT('Ctrl Pts',(-50.0769067917592,-44.9361782632308,
-7.91663908938817));
#31970=CARTESIAN_POINT('Ctrl Pts',(-49.1080150008643,-42.5144881890784,
-8.03395066944929));
#31971=CARTESIAN_POINT('Ctrl Pts',(-45.0527739768292,-41.2871004410853,
-8.21654976877883));
#31972=CARTESIAN_POINT('Ctrl Pts',(-41.5512814170077,-44.1804051792425,
-8.41241232658412));
#31973=CARTESIAN_POINT('Ctrl Pts',(-42.020443960099,-48.7013832307533,-8.60827488438941));
#31974=CARTESIAN_POINT('Ctrl Pts',(-46.0536368602338,-50.8047688779136,
-8.80413744219471));
#31975=CARTESIAN_POINT('Ctrl Pts',(-48.6953045558515,-49.3495832107922,
-8.93471248073157));
#31976=CARTESIAN_POINT('Ctrl Pts',(-49.4256147683784,-48.2253962475631,
-9.));
#31977=CARTESIAN_POINT('',(-50.0861550027666,-46.2124414226054,-9.));
#31978=CARTESIAN_POINT('Origin',(-46.,-46.,-9.));
#31979=CARTESIAN_POINT('Ctrl Pts',(-50.0803093213768,-45.997675543601,-7.76038497140452));
#31980=CARTESIAN_POINT('Ctrl Pts',(-50.0830253101917,-45.4889855897383,
-7.78509075167359));
#31981=CARTESIAN_POINT('Ctrl Pts',(-49.761077511572,-43.6393405608411,-7.8750840512111));
#31982=CARTESIAN_POINT('Ctrl Pts',(-47.0195848331003,-41.3020769083036,
-8.03036487001704));
#31983=CARTESIAN_POINT('Ctrl Pts',(-42.6509149775089,-42.5514375357737,
-8.22622742782233));
#31984=CARTESIAN_POINT('Ctrl Pts',(-41.2740009567628,-46.8818734807212,
-8.42208998562762));
#31985=CARTESIAN_POINT('Ctrl Pts',(-44.1206550171574,-50.4245588063534,
-8.61795254343291));
#31986=CARTESIAN_POINT('Ctrl Pts',(-48.5697413278868,-50.0204905730501,
-8.81058921489038));
#31987=CARTESIAN_POINT('Ctrl Pts',(-50.0156455888524,-47.4797542540496,
-8.9379383670794));
#31988=CARTESIAN_POINT('Ctrl Pts',(-50.0861960634202,-46.2124371387131,
-9.));
#31989=CARTESIAN_POINT('Origin',(-46.,-46.,2.76038497140452));
#31990=CARTESIAN_POINT('',(-50.0848585401616,-46.0034858730695,-6.51038497140452));
#31991=CARTESIAN_POINT('',(-50.0872042738947,-45.9967790949693,-6.61461502859548));
#31992=CARTESIAN_POINT('',(-50.085,-45.9999999999999,2.76038497140452));
#31993=CARTESIAN_POINT('Ctrl Pts',(-50.0872042738947,-45.9967790949692,
-6.61461502859548));
#31994=CARTESIAN_POINT('Ctrl Pts',(-50.0892699768444,-45.757363874878,-6.62629312117581));
#31995=CARTESIAN_POINT('Ctrl Pts',(-49.9622039222413,-44.1816627080423,
-6.70325873302458));
#31996=CARTESIAN_POINT('Ctrl Pts',(-47.9170393622873,-41.5914781257455,
-6.84551186414177));
#31997=CARTESIAN_POINT('Ctrl Pts',(-43.3883208590233,-41.9640096554919,
-7.04137442194707));
#31998=CARTESIAN_POINT('Ctrl Pts',(-41.1930648262276,-45.9425306703187,
-7.23723697975236));
#31999=CARTESIAN_POINT('Ctrl Pts',(-43.2925649089103,-49.9724248955266,
-7.43309953755766));
#32000=CARTESIAN_POINT('Ctrl Pts',(-47.8111687880873,-50.4530556126673,
-7.62896209536294));
#32001=CARTESIAN_POINT('Ctrl Pts',(-49.9410024707322,-47.8842562868416,
-7.77280059237556));
#32002=CARTESIAN_POINT('Ctrl Pts',(-50.0886589976984,-46.2754717475514,
-7.85135157011974));
#32003=CARTESIAN_POINT('Ctrl Pts',(-50.0862714832512,-46.0033881438983,
-7.86461502859548));
#32004=CARTESIAN_POINT('Ctrl Pts',(-50.0848585401615,-46.0034858730695,
-6.51038497140452));
#32005=CARTESIAN_POINT('Ctrl Pts',(-50.0759395539985,-44.9841466302342,
-6.56003230272967));
#32006=CARTESIAN_POINT('Ctrl Pts',(-49.1785303598923,-42.6103271435563,
-6.67496715332326));
#32007=CARTESIAN_POINT('Ctrl Pts',(-45.2228147324014,-41.2559448461001,
-6.85518952318528));
#32008=CARTESIAN_POINT('Ctrl Pts',(-41.6182000513892,-44.022657337512,-7.05105208099056));
#32009=CARTESIAN_POINT('Ctrl Pts',(-41.9285482915987,-48.5560484764118,
-7.24691463879586));
#32010=CARTESIAN_POINT('Ctrl Pts',(-45.8765970410433,-50.8057107187776,
-7.44277719660115));
#32011=CARTESIAN_POINT('Ctrl Pts',(-49.4229675651535,-49.0194845514499,
-7.61393397413737));
#32012=CARTESIAN_POINT('Ctrl Pts',(-50.075848035475,-46.8332501627557,-7.71980323240516));
#32013=CARTESIAN_POINT('Ctrl Pts',(-50.0803093213768,-45.997675543601,-7.76038497140452));
#32014=CARTESIAN_POINT('Origin',(-46.,-46.,2.76038497140452));
#32015=CARTESIAN_POINT('',(-50.0885301671912,-45.9971742157295,-5.26038497140452));
#32016=CARTESIAN_POINT('',(-50.0791877655715,-46.0012446258329,-5.36461502859548));
#32017=CARTESIAN_POINT('',(-50.085,-45.9999999999999,2.76038497140452));
#32018=CARTESIAN_POINT('Ctrl Pts',(-50.0791877655715,-46.0012446258329,
-5.36461502859548));
#32019=CARTESIAN_POINT('Ctrl Pts',(-50.0770717119439,-45.2467317861072,
-5.40123467223189));
#32020=CARTESIAN_POINT('Ctrl Pts',(-49.5176919519867,-43.1441146815151,
-5.50314183513674));
#32021=CARTESIAN_POINT('Ctrl Pts',(-46.1637649512516,-41.195496195607,-5.67033651731001));
#32022=CARTESIAN_POINT('Ctrl Pts',(-42.0884421952216,-43.2053995648544,
-5.86619907511531));
#32023=CARTESIAN_POINT('Ctrl Pts',(-41.5079465982135,-47.7121709957002,
-6.0620616329206));
#32024=CARTESIAN_POINT('Ctrl Pts',(-44.9409275558383,-50.6891837144081,
-6.25792419072589));
#32025=CARTESIAN_POINT('Ctrl Pts',(-49.0590442379987,-49.5488895831714,
-6.44210865595085));
#32026=CARTESIAN_POINT('Ctrl Pts',(-50.0777214623756,-47.0958380895104,
-6.56100560190738));
#32027=CARTESIAN_POINT('Ctrl Pts',(-50.0872042738947,-45.9967790949692,
-6.61461502859548));
#32028=CARTESIAN_POINT('Ctrl Pts',(-50.0885301671911,-45.9971742157295,
-5.26038497140452));
#32029=CARTESIAN_POINT('Ctrl Pts',(-50.0900435768525,-45.8066458222,-5.26968633451732));
#32030=CARTESIAN_POINT('Ctrl Pts',(-49.9922177014,-44.2803335729962,-5.34427521689855));
#32031=CARTESIAN_POINT('Ctrl Pts',(-48.0737730601331,-41.6630035036824,
-5.48415161854822));
#32032=CARTESIAN_POINT('Ctrl Pts',(-43.5346256929101,-41.8730152769562,
-5.68001417635351));
#32033=CARTESIAN_POINT('Ctrl Pts',(-41.1981957029014,-45.7703295255252,
-5.87587673415881));
#32034=CARTESIAN_POINT('Ctrl Pts',(-43.1519934739611,-49.8728455133488,
-6.0717392919641));
#32035=CARTESIAN_POINT('Ctrl Pts',(-47.6503759783394,-50.5151226960096,
-6.26760184976939));
#32036=CARTESIAN_POINT('Ctrl Pts',(-49.9077275125445,-47.9830689624062,
-6.41381707624954));
#32037=CARTESIAN_POINT('Ctrl Pts',(-50.087668250495,-46.3246039857731,-6.49474478346124));
#32038=CARTESIAN_POINT('Ctrl Pts',(-50.0848585401615,-46.0034858730695,
-6.51038497140452));
#32039=CARTESIAN_POINT('Origin',(-46.,-46.,2.76038497140452));
#32040=CARTESIAN_POINT('',(-50.0788652030139,-46.0005097590054,-4.01038497140452));
#32041=CARTESIAN_POINT('',(-50.0908854225478,-46.0013070164178,-4.11461502859548));
#32042=CARTESIAN_POINT('',(-50.085,-45.9999999999999,2.76038497140452));
#32043=CARTESIAN_POINT('Ctrl Pts',(-50.0908854225478,-46.0013070164178,
-4.11461502859548));
#32044=CARTESIAN_POINT('Ctrl Pts',(-50.0855211619739,-44.7422069936917,
-4.17617622328797));
#32045=CARTESIAN_POINT('Ctrl Pts',(-48.7949531014785,-42.1382705071838,
-4.3030249372489));
#32046=CARTESIAN_POINT('Ctrl Pts',(-44.3875999794073,-41.4711765661473,
-4.49516117047825));
#32047=CARTESIAN_POINT('Ctrl Pts',(-41.3353873965154,-44.8374748217385,
-4.69102372828354));
#32048=CARTESIAN_POINT('Ctrl Pts',(-42.4508271650107,-49.2424447068201,
-4.88688628608884));
#32049=CARTESIAN_POINT('Ctrl Pts',(-46.7373166435254,-50.7504146876272,
-5.08274884389413));
#32050=CARTESIAN_POINT('Ctrl Pts',(-49.6867806300422,-48.5256746587921,
-5.24199175806301));
#32051=CARTESIAN_POINT('Ctrl Pts',(-50.080844328995,-46.5919188679631,-5.33594715296346));
#32052=CARTESIAN_POINT('Ctrl Pts',(-50.0791877655715,-46.0012446258329,
-5.36461502859548));
#32053=CARTESIAN_POINT('Ctrl Pts',(-50.0788652030139,-46.0005097590054,
-4.01038497140452));
#32054=CARTESIAN_POINT('Ctrl Pts',(-50.0780586190038,-45.2948273556406,
-4.0446278855734));
#32055=CARTESIAN_POINT('Ctrl Pts',(-49.5711124212075,-43.2426058741684,
-4.14415831901071));
#32056=CARTESIAN_POINT('Ctrl Pts',(-46.3358174043579,-41.204449981662,-4.30897627171646));
#32057=CARTESIAN_POINT('Ctrl Pts',(-42.1910921533903,-43.0670331890375,
-4.50483882952175));
#32058=CARTESIAN_POINT('Ctrl Pts',(-41.4494798905217,-47.5501096808741,
-4.70070138732705));
#32059=CARTESIAN_POINT('Ctrl Pts',(-44.7735827067234,-50.6482226625802,
-4.89656394513233));
#32060=CARTESIAN_POINT('Ctrl Pts',(-48.9835465579835,-49.6434232658214,
-5.08312513982483));
#32061=CARTESIAN_POINT('Ctrl Pts',(-50.0794207507967,-47.1439902536432,
-5.20439881524889));
#32062=CARTESIAN_POINT('Ctrl Pts',(-50.0885301671911,-45.9971742157295,
-5.26038497140452));
#32063=CARTESIAN_POINT('Origin',(-46.,-46.,2.76038497140452));
#32064=CARTESIAN_POINT('',(-50.0900545172792,-46.0020418321801,-2.76038497140452));
#32065=CARTESIAN_POINT('',(-50.081795401254,-45.9969676253998,-2.86461502859548));
#32066=CARTESIAN_POINT('',(-50.085,-45.9999999999999,2.76038497140452));
#32067=CARTESIAN_POINT('Ctrl Pts',(-50.081795401254,-45.9969676253998,-2.86461502859548));
#32068=CARTESIAN_POINT('Ctrl Pts',(-50.0849112009229,-45.560551617548,-2.88583025507562));
#32069=CARTESIAN_POINT('Ctrl Pts',(-49.8212806234326,-43.7847766277542,
-2.97233300082419));
#32070=CARTESIAN_POINT('Ctrl Pts',(-47.2654095909828,-41.362240430431,-3.1241232658412));
#32071=CARTESIAN_POINT('Ctrl Pts',(-42.8368466927335,-42.379981111081,-3.31998582364649));
#32072=CARTESIAN_POINT('Ctrl Pts',(-41.2344398737399,-46.6320697906436,
-3.51584838145178));
#32073=CARTESIAN_POINT('Ctrl Pts',(-43.8898781422471,-50.3194283458399,
-3.71171093925708));
#32074=CARTESIAN_POINT('Ctrl Pts',(-48.4306293080085,-50.1475434533866,
-3.90757349706237));
#32075=CARTESIAN_POINT('Ctrl Pts',(-50.0550862518107,-47.4887349722982,
-4.04187486017517));
#32076=CARTESIAN_POINT('Ctrl Pts',(-50.091210123459,-46.0775208615468,-4.11088870401954));
#32077=CARTESIAN_POINT('Ctrl Pts',(-50.0908854225478,-46.0013070164178,
-4.11461502859548));
#32078=CARTESIAN_POINT('Ctrl Pts',(-50.0900545172792,-46.0020418321801,
-2.76038497140452));
#32079=CARTESIAN_POINT('Ctrl Pts',(-50.0825375788689,-44.7908992747219,
-2.81956943662948));
#32080=CARTESIAN_POINT('Ctrl Pts',(-48.8773452250357,-42.2307009333171,
-2.94404142112287));
#32081=CARTESIAN_POINT('Ctrl Pts',(-44.5509149516467,-41.4163086543115,
-3.1338009248847));
#32082=CARTESIAN_POINT('Ctrl Pts',(-41.3800394184348,-44.6710764629181,
-3.32966348268999));
#32083=CARTESIAN_POINT('Ctrl Pts',(-42.3369215031958,-49.1131863035692,
-3.52552604049529));
#32084=CARTESIAN_POINT('Ctrl Pts',(-46.5666235775808,-50.7737837298756,
-3.72138859830058));
#32085=CARTESIAN_POINT('Ctrl Pts',(-49.6390942515875,-48.6245534357952,
-3.88300824193699));
#32086=CARTESIAN_POINT('Ctrl Pts',(-50.0795964515855,-46.6402809954754,
-3.97934036630497));
#32087=CARTESIAN_POINT('Ctrl Pts',(-50.0788652030139,-46.0005097590054,
-4.01038497140452));
#32088=CARTESIAN_POINT('Origin',(-46.,-46.,2.76038497140452));
#32089=CARTESIAN_POINT('',(-50.0830240067876,-45.9966653604899,-1.51038497140452));
#32090=CARTESIAN_POINT('',(-50.0828677018166,-46.0033110698502,-1.61461502859548));
#32091=CARTESIAN_POINT('',(-50.085,-45.9999999999999,2.76038497140452));
#32092=CARTESIAN_POINT('Ctrl Pts',(-50.0828677018166,-46.0033110698502,
-1.61461502859548));
#32093=CARTESIAN_POINT('Ctrl Pts',(-50.0753230858173,-45.0544576856415,
-1.6607718061317));
#32094=CARTESIAN_POINT('Ctrl Pts',(-49.2773378217668,-42.7520207060235,
-1.77221610293635));
#32095=CARTESIAN_POINT('Ctrl Pts',(-45.4734860003987,-41.2216278875877,
-1.94894791900943));
#32096=CARTESIAN_POINT('Ctrl Pts',(-41.7282986823175,-43.794859117017,-2.14481047681473));
#32097=CARTESIAN_POINT('Ctrl Pts',(-41.7997119996332,-48.3383026030494,
-2.34067303462002));
#32098=CARTESIAN_POINT('Ctrl Pts',(-45.6239217216425,-50.7925607363461,
-2.53653559242531));
#32099=CARTESIAN_POINT('Ctrl Pts',(-49.3335205372955,-49.1628225231174,
-2.71118292375047));
#32100=CARTESIAN_POINT('Ctrl Pts',(-50.0753226711417,-46.9035737412263,
-2.82054273580719));
#32101=CARTESIAN_POINT('Ctrl Pts',(-50.081795401254,-45.9969676253998,-2.86461502859548));
#32102=CARTESIAN_POINT('Ctrl Pts',(-50.0830240067876,-45.9966653604899,
-1.51038497140452));
#32103=CARTESIAN_POINT('Ctrl Pts',(-50.0861433599091,-45.6094337666882,
-1.52922346841713));
#32104=CARTESIAN_POINT('Ctrl Pts',(-49.8595841509064,-43.8837675877116,
-1.61334948469817));
#32105=CARTESIAN_POINT('Ctrl Pts',(-47.4307680051951,-41.41057421285,-1.76276302024764));
#32106=CARTESIAN_POINT('Ctrl Pts',(-42.9685984702712,-42.2689561020525,
-1.95862557805293));
#32107=CARTESIAN_POINT('Ctrl Pts',(-41.2148490309835,-46.4609045794214,
-2.15448813585823));
#32108=CARTESIAN_POINT('Ctrl Pts',(-43.7364585340961,-50.2410417148001,
-2.35035069366352));
#32109=CARTESIAN_POINT('Ctrl Pts',(-48.2804504821097,-50.2319761154881,
-2.54621325146882));
#32110=CARTESIAN_POINT('Ctrl Pts',(-50.0295523051546,-47.5870903820588,
-2.68289134404915));
#32111=CARTESIAN_POINT('Ctrl Pts',(-50.0908296578703,-46.1269338702245,
-2.75428191736105));
#32112=CARTESIAN_POINT('Ctrl Pts',(-50.0900545172792,-46.0020418321801,
-2.76038497140452));
#32113=CARTESIAN_POINT('Origin',(-46.,-46.,2.76038497140452));
#32114=CARTESIAN_POINT('',(-50.0805802565567,-46.0038346370175,-0.260384971404518));
#32115=CARTESIAN_POINT('',(-50.0901578141997,-45.9981376217778,-0.364615028595479));
#32116=CARTESIAN_POINT('',(-50.085,-45.9999999999999,2.76038497140452));
#32117=CARTESIAN_POINT('',(-47.057904422973,-49.9456385074984,0.));
#32118=CARTESIAN_POINT('Ctrl Pts',(-47.0579044229729,-49.9456385074984,
5.55111512312578E-16));
#32119=CARTESIAN_POINT('Ctrl Pts',(-48.3527480267224,-49.5984650974504,
-0.0652875192684306));
#32120=CARTESIAN_POINT('Ctrl Pts',(-49.8153067462896,-48.2273633419822,
-0.152082509736604));
#32121=CARTESIAN_POINT('Ctrl Pts',(-50.0835490595066,-46.4463082039673,
-0.238877500204776));
#32122=CARTESIAN_POINT('Ctrl Pts',(-50.0805802565567,-46.0038346370175,
-0.260384971404518));
#32123=CARTESIAN_POINT('',(-44.9393523503947,-49.9518124380696,-3.33880900068018E-15));
#32124=CARTESIAN_POINT('Origin',(-46.,-46.,0.));
#32125=CARTESIAN_POINT('Ctrl Pts',(-44.9393355849193,-49.9518501705994,
6.45100292628875E-17));
#32126=CARTESIAN_POINT('Ctrl Pts',(-46.166426942727,-50.2763750719212,-0.0620616329205977));
#32127=CARTESIAN_POINT('Ctrl Pts',(-48.8989758948986,-49.7132910486246,
-0.183599975785757));
#32128=CARTESIAN_POINT('Ctrl Pts',(-50.0828902798758,-47.2149621037996,
-0.305138318650917));
#32129=CARTESIAN_POINT('Ctrl Pts',(-50.0901578141997,-45.9981376217778,
-0.364615028595479));
#32130=CARTESIAN_POINT('Origin',(46.,-46.,-5.));
#32131=CARTESIAN_POINT('',(42.6091952652934,-46.0028114996479,-8.26601780324956));
#32132=CARTESIAN_POINT('',(42.6044125646165,-46.0001574521336,-8.60898219675043));
#32133=CARTESIAN_POINT('',(42.61025,-46.,-5.));
#32134=CARTESIAN_POINT('',(47.303382040875,-42.8708467090881,-9.));
#32135=CARTESIAN_POINT('Ctrl Pts',(42.6044125646165,-46.0001574521336,-8.60898219675043));
#32136=CARTESIAN_POINT('Ctrl Pts',(42.6053219601772,-44.8964212032941,-8.67403394523185));
#32137=CARTESIAN_POINT('Ctrl Pts',(43.1965789016692,-43.7921183414524,-8.73908569371328));
#32138=CARTESIAN_POINT('Ctrl Pts',(44.1121218294326,-43.1790110276343,-8.80413744219471));
#32139=CARTESIAN_POINT('Ctrl Pts',(45.0309830119955,-42.5636815937768,-8.86942496146314));
#32140=CARTESIAN_POINT('Ctrl Pts',(46.2764850972779,-42.4431146967252,-8.93471248073157));
#32141=CARTESIAN_POINT('Ctrl Pts',(47.3033820408749,-42.8708467090881,-9.));
#32142=CARTESIAN_POINT('',(42.61025,-46.,-9.));
#32143=CARTESIAN_POINT('Origin',(46.,-46.,-9.));
#32144=CARTESIAN_POINT('',(42.61025,-46.,-10.));
#32145=CARTESIAN_POINT('',(42.61025,-46.,-5.));
#32146=CARTESIAN_POINT('Origin',(46.,-46.,-10.));
#32147=CARTESIAN_POINT('',(48.8980017072691,-47.7690577679613,-9.));
#32148=CARTESIAN_POINT('Origin',(46.,-46.,-9.));
#32149=CARTESIAN_POINT('Ctrl Pts',(48.8980278172144,-47.7690799369094,-9.));
#32150=CARTESIAN_POINT('Ctrl Pts',(49.4435067823307,-46.8680830001505,-8.9379383670794));
#32151=CARTESIAN_POINT('Ctrl Pts',(49.5410722981907,-45.6899359369109,-8.8758767341588));
#32152=CARTESIAN_POINT('Ctrl Pts',(49.1424202878046,-44.7152011753849,-8.81381510123821));
#32153=CARTESIAN_POINT('Ctrl Pts',(48.7230468426555,-43.689800915515,-8.74852758196978));
#32154=CARTESIAN_POINT('Ctrl Pts',(47.7545296578687,-42.8895087708225,-8.68324006270134));
#32155=CARTESIAN_POINT('Ctrl Pts',(46.6686904094295,-42.6714413128456,-8.61795254343291));
#32156=CARTESIAN_POINT('Ctrl Pts',(45.5828511609903,-42.4533738548687,-8.55266502416448));
#32157=CARTESIAN_POINT('Ctrl Pts',(44.3796898488986,-42.8175310836074,-8.48737750489605));
#32158=CARTESIAN_POINT('Ctrl Pts',(43.5971078026617,-43.6014280129255,-8.42208998562762));
#32159=CARTESIAN_POINT('Ctrl Pts',(42.973510882379,-44.2260726917709,-8.37006592483494));
#32160=CARTESIAN_POINT('Ctrl Pts',(42.6169660769066,-45.1172363928553,-8.31804186404225));
#32161=CARTESIAN_POINT('Ctrl Pts',(42.6091952652934,-46.0028114996479,-8.26601780324956));
#32162=CARTESIAN_POINT('Origin',(46.,-46.,-5.));
#32163=CARTESIAN_POINT('',(42.6084212224847,-45.9973272800439,-7.01601780324956));
#32164=CARTESIAN_POINT('',(42.6141425307955,-45.9980711599138,-7.35898219675043));
#32165=CARTESIAN_POINT('',(42.61025,-46.,-5.));
#32166=CARTESIAN_POINT('Ctrl Pts',(42.6141425307955,-45.9980711599138,-7.35898219675043));
#32167=CARTESIAN_POINT('Ctrl Pts',(42.6118887907293,-45.575958143871,-7.3836879770195));
#32168=CARTESIAN_POINT('Ctrl Pts',(42.6852302319893,-45.154599048709,-7.40839375728858));
#32169=CARTESIAN_POINT('Ctrl Pts',(42.8378019484186,-44.7642018229609,-7.43309953755765));
#32170=CARTESIAN_POINT('Ctrl Pts',(43.2409881165019,-43.7325377297497,-7.49838705682608));
#32171=CARTESIAN_POINT('Ctrl Pts',(44.197466231587,-42.9170908965982,-7.56367457609451));
#32172=CARTESIAN_POINT('Ctrl Pts',(45.2798953093061,-42.6821549238822,-7.62896209536294));
#32173=CARTESIAN_POINT('Ctrl Pts',(46.3623243870251,-42.4472189511661,-7.69424961463137));
#32174=CARTESIAN_POINT('Ctrl Pts',(47.570704427378,-42.7927938388857,-7.7595371338998));
#32175=CARTESIAN_POINT('Ctrl Pts',(48.3653226299911,-43.5644835193059,-7.82482465316823));
#32176=CARTESIAN_POINT('Ctrl Pts',(49.1599408326043,-44.3361731997261,-7.89011217243666));
#32177=CARTESIAN_POINT('Ctrl Pts',(49.5407971974777,-45.5339776728469,-7.95539969170509));
#32178=CARTESIAN_POINT('Ctrl Pts',(49.3375311222527,-46.6228357674574,-8.02068721097353));
#32179=CARTESIAN_POINT('Ctrl Pts',(49.1342650470278,-47.7116938620679,-8.08597473024196));
#32180=CARTESIAN_POINT('Ctrl Pts',(48.3468765317045,-48.6916055781681,-8.15126224951039));
#32181=CARTESIAN_POINT('Ctrl Pts',(47.3275666791222,-49.1247426138568,-8.21654976877882));
#32182=CARTESIAN_POINT('Ctrl Pts',(46.3082568265399,-49.5578796495455,-8.28183728804725));
#32183=CARTESIAN_POINT('Ctrl Pts',(45.0570256366986,-49.4442420048227,-8.34712480731568));
#32184=CARTESIAN_POINT('Ctrl Pts',(44.1319143151655,-48.8347431895811,-8.41241232658411));
#32185=CARTESIAN_POINT('Ctrl Pts',(43.2068029936325,-48.2252443743394,-8.47769984585254));
#32186=CARTESIAN_POINT('Ctrl Pts',(42.6078115404076,-47.119884388579,-8.54298736512097));
#32187=CARTESIAN_POINT('Ctrl Pts',(42.604425953717,-46.0121584103671,-8.60827488438941));
#32188=CARTESIAN_POINT('Ctrl Pts',(42.6044137274531,-46.0081581140073,-8.60851065517642));
#32189=CARTESIAN_POINT('Ctrl Pts',(42.6044092686419,-46.004157786792,-8.60874642596342));
#32190=CARTESIAN_POINT('Ctrl Pts',(42.6044125646165,-46.0001574521336,-8.60898219675043));
#32191=CARTESIAN_POINT('Ctrl Pts',(42.6091952652934,-46.0028114996479,-8.26601780324956));
#32192=CARTESIAN_POINT('Ctrl Pts',(42.6072141081983,-46.2285875824282,-8.25275434477382));
#32193=CARTESIAN_POINT('Ctrl Pts',(42.6279028279941,-46.4540004135131,-8.23949088629807));
#32194=CARTESIAN_POINT('Ctrl Pts',(42.6726156656388,-46.6745408053554,-8.22622742782233));
#32195=CARTESIAN_POINT('Ctrl Pts',(42.8927083552351,-47.7601200385699,-8.16093990855389));
#32196=CARTESIAN_POINT('Ctrl Pts',(43.6948965148099,-48.7276418751015,-8.09565238928547));
#32197=CARTESIAN_POINT('Ctrl Pts',(44.7209166029033,-49.1449312387884,-8.03036487001703));
#32198=CARTESIAN_POINT('Ctrl Pts',(45.7469366909968,-49.5622206024753,-7.9650773507486));
#32199=CARTESIAN_POINT('Ctrl Pts',(46.9967887076088,-49.4292774933176,-7.89978983148017));
#32200=CARTESIAN_POINT('Ctrl Pts',(47.9120769940113,-48.8054688270359,-7.83450231221174));
#32201=CARTESIAN_POINT('Ctrl Pts',(48.8273652804138,-48.1816601607542,-7.76921479294331));
#32202=CARTESIAN_POINT('Ctrl Pts',(49.4080898366068,-47.0669859373486,-7.70392727367488));
#32203=CARTESIAN_POINT('Ctrl Pts',(49.3948467186262,-45.959416665038,-7.63863975440645));
#32204=CARTESIAN_POINT('Ctrl Pts',(49.3816036006456,-44.8518473927274,-7.57335223513801));
#32205=CARTESIAN_POINT('Ctrl Pts',(48.7743928084915,-43.7513830715118,-7.50806471586958));
#32206=CARTESIAN_POINT('Ctrl Pts',(47.8444625615455,-43.1496295467018,-7.44277719660115));
#32207=CARTESIAN_POINT('Ctrl Pts',(46.9145323145995,-42.5478760218918,-7.37748967733272));
#32208=CARTESIAN_POINT('Ctrl Pts',(45.6618826128616,-42.4448332934873,-7.31220215806429));
#32209=CARTESIAN_POINT('Ctrl Pts',(44.6461163251007,-42.8865364012444,-7.24691463879586));
#32210=CARTESIAN_POINT('Ctrl Pts',(43.6303500373398,-43.3282395090014,-7.18162711952743));
#32211=CARTESIAN_POINT('Ctrl Pts',(42.8514671635558,-44.3146884529201,-7.116339600259));
#32212=CARTESIAN_POINT('Ctrl Pts',(42.6574159170588,-45.405204785632,-7.05105208099057));
#32213=CARTESIAN_POINT('Ctrl Pts',(42.6227056317345,-45.600267346386,-7.03937398841023));
#32214=CARTESIAN_POINT('Ctrl Pts',(42.6067070937495,-45.7986595538186,-7.0276958958299));
#32215=CARTESIAN_POINT('Ctrl Pts',(42.6084212224847,-45.9973272800439,-7.01601780324956));
#32216=CARTESIAN_POINT('Origin',(46.,-46.,-5.));
#32217=CARTESIAN_POINT('',(42.6150733527443,-46.0010327955954,-5.76601780324956));
#32218=CARTESIAN_POINT('',(42.610367575631,-46.0028925918188,-6.10898219675042));
#32219=CARTESIAN_POINT('',(42.61025,-46.,-5.));
#32220=CARTESIAN_POINT('Ctrl Pts',(42.610367575631,-46.0028925918188,-6.10898219675042));
#32221=CARTESIAN_POINT('Ctrl Pts',(42.6177685869596,-45.1570406939323,-6.15862952807558));
#32222=CARTESIAN_POINT('Ctrl Pts',(42.9394383742148,-44.3061623939123,-6.20827685940073));
#32223=CARTESIAN_POINT('Ctrl Pts',(43.5127592901994,-43.6890940545951,-6.25792419072588));
#32224=CARTESIAN_POINT('Ctrl Pts',(44.2666910595466,-42.877633296931,-6.32321170999432));
#32225=CARTESIAN_POINT('Ctrl Pts',(45.4558012966754,-42.4704984048589,-6.38849922926275));
#32226=CARTESIAN_POINT('Ctrl Pts',(46.5488770971372,-42.6495691939267,-6.45378674853118));
#32227=CARTESIAN_POINT('Ctrl Pts',(47.641952897599,-42.8286399829945,-6.51907426779961));
#32228=CARTESIAN_POINT('Ctrl Pts',(48.6389942613939,-43.5939164532021,-6.58436178706804));
#32229=CARTESIAN_POINT('Ctrl Pts',(49.0945935696661,-44.6035257912972,-6.64964930633647));
#32230=CARTESIAN_POINT('Ctrl Pts',(49.5501928779384,-45.6131351293924,-6.7149368256049));
#32231=CARTESIAN_POINT('Ctrl Pts',(49.4643501306881,-46.8670773353749,-6.78022434487333));
#32232=CARTESIAN_POINT('Ctrl Pts',(48.8754109060044,-47.8051782700423,-6.84551186414176));
#32233=CARTESIAN_POINT('Ctrl Pts',(48.2864716813207,-48.7432792047097,-6.91079938341019));
#32234=CARTESIAN_POINT('Ctrl Pts',(47.1944359792037,-49.3655388680619,-6.97608690267863));
#32235=CARTESIAN_POINT('Ctrl Pts',(46.0871559716595,-49.3939737149546,-7.04137442194706));
#32236=CARTESIAN_POINT('Ctrl Pts',(44.9798759641153,-49.4224085618473,-7.10666194121549));
#32237=CARTESIAN_POINT('Ctrl Pts',(43.8573516511439,-48.8570185922806,-7.17194946048392));
#32238=CARTESIAN_POINT('Ctrl Pts',(43.221036605199,-47.9503829308618,-7.23723697975235));
#32239=CARTESIAN_POINT('Ctrl Pts',(42.8255127530867,-47.3868318541555,-7.27781871875171));
#32240=CARTESIAN_POINT('Ctrl Pts',(42.6178445264477,-46.6914344157477,-7.31840045775107));
#32241=CARTESIAN_POINT('Ctrl Pts',(42.6141425307955,-45.9980711599138,-7.35898219675043));
#32242=CARTESIAN_POINT('Ctrl Pts',(42.6084212224847,-45.9973272800439,-7.01601780324956));
#32243=CARTESIAN_POINT('Ctrl Pts',(42.6162900981709,-46.9093309168622,-6.96240837656147));
#32244=CARTESIAN_POINT('Ctrl Pts',(42.9974284256452,-47.8271407233737,-6.90879894987337));
#32245=CARTESIAN_POINT('Ctrl Pts',(43.6551847755762,-48.4552992360462,-6.85518952318527));
#32246=CARTESIAN_POINT('Ctrl Pts',(44.4562244998004,-49.2202936322432,-6.78990200391684));
#32247=CARTESIAN_POINT('Ctrl Pts',(45.6675235674587,-49.5556987031322,-6.72461448464841));
#32248=CARTESIAN_POINT('Ctrl Pts',(46.7479567014102,-49.3116783556131,-6.65932696537998));
#32249=CARTESIAN_POINT('Ctrl Pts',(47.8283898353616,-49.067658008094,-6.59403944611154));
#32250=CARTESIAN_POINT('Ctrl Pts',(48.7779570356062,-48.2442122421669,-6.52875192684312));
#32251=CARTESIAN_POINT('Ctrl Pts',(49.1724577001302,-47.2091998064185,-6.46346440757469));
#32252=CARTESIAN_POINT('Ctrl Pts',(49.5669583646541,-46.1741873706701,-6.39817688830625));
#32253=CARTESIAN_POINT('Ctrl Pts',(49.4063924934574,-44.9276082651004,-6.33288936903782));
#32254=CARTESIAN_POINT('Ctrl Pts',(48.7624896500348,-44.0263477099034,-6.26760184976939));
#32255=CARTESIAN_POINT('Ctrl Pts',(48.1185868066121,-43.1250871547063,-6.20231433050096));
#32256=CARTESIAN_POINT('Ctrl Pts',(46.9913469909636,-42.5691451498819,-6.13702681123253));
#32257=CARTESIAN_POINT('Ctrl Pts',(45.8843430380562,-42.6068781550557,-6.0717392919641));
#32258=CARTESIAN_POINT('Ctrl Pts',(44.7773390851488,-42.6446111602295,-6.00645177269567));
#32259=CARTESIAN_POINT('Ctrl Pts',(43.6905709949825,-43.2760191754015,-5.94116425342724));
#32260=CARTESIAN_POINT('Ctrl Pts',(43.1095315203292,-44.2190327676712,-5.8758767341588));
#32261=CARTESIAN_POINT('Ctrl Pts',(42.7836275996577,-44.7479672727674,-5.83925709052239));
#32262=CARTESIAN_POINT('Ctrl Pts',(42.6168292626847,-45.3749349634637,-5.80263744688598));
#32263=CARTESIAN_POINT('Ctrl Pts',(42.6150733527443,-46.0010327955954,-5.76601780324956));
#32264=CARTESIAN_POINT('Origin',(46.,-46.,-5.));
#32265=CARTESIAN_POINT('',(42.6053665892596,-46.0010845675542,-4.51601780324957));
#32266=CARTESIAN_POINT('',(42.6073208444166,-45.9976551525847,-4.85898219675043));
#32267=CARTESIAN_POINT('',(42.61025,-46.,-5.));
#32268=CARTESIAN_POINT('Ctrl Pts',(42.6073208444166,-45.9976551525847,-4.85898219675043));
#32269=CARTESIAN_POINT('Ctrl Pts',(42.6060650108524,-45.8395539076774,-4.86828355986323));
#32270=CARTESIAN_POINT('Ctrl Pts',(42.6161878381193,-45.6816141480506,-4.87758492297603));
#32271=CARTESIAN_POINT('Ctrl Pts',(42.6382491084881,-45.5253599574508,-4.88688628608883));
#32272=CARTESIAN_POINT('Ctrl Pts',(42.7931001337434,-44.4285907682639,-4.95217380535726));
#32273=CARTESIAN_POINT('Ctrl Pts',(43.5361373577979,-43.4148666152112,-5.01746132462569));
#32274=CARTESIAN_POINT('Ctrl Pts',(44.5354231635466,-42.9370493109476,-5.08274884389412));
#32275=CARTESIAN_POINT('Ctrl Pts',(45.5347089692953,-42.459232006684,-5.14803636316255));
#32276=CARTESIAN_POINT('Ctrl Pts',(46.7902433567382,-42.5173215512096,-5.21332388243098));
#32277=CARTESIAN_POINT('Ctrl Pts',(47.7411404203322,-43.0853675567301,-5.27861140169942));
#32278=CARTESIAN_POINT('Ctrl Pts',(48.6920374839263,-43.6534135622506,-5.34389892096785));
#32279=CARTESIAN_POINT('Ctrl Pts',(49.3382972236715,-44.7314160287659,-5.40918644023628));
#32280=CARTESIAN_POINT('Ctrl Pts',(49.3912155219598,-45.8377980365326,-5.47447395950471));
#32281=CARTESIAN_POINT('Ctrl Pts',(49.444133820248,-46.9441800442992,-5.53976147877314));
#32282=CARTESIAN_POINT('Ctrl Pts',(48.9037106770792,-48.0789415933172,-5.60504899804157));
#32283=CARTESIAN_POINT('Ctrl Pts',(48.0113697202318,-48.735149742658,-5.67033651731));
#32284=CARTESIAN_POINT('Ctrl Pts',(47.1190287633844,-49.3913578919989,-5.73562403657843));
#32285=CARTESIAN_POINT('Ctrl Pts',(45.8747699928583,-49.5690126416627,-5.80091155584687));
#32286=CARTESIAN_POINT('Ctrl Pts',(44.8344422234934,-49.1887501277354,-5.8661990751153));
#32287=CARTESIAN_POINT('Ctrl Pts',(43.7941144541285,-48.8084876138081,-5.93148659438373));
#32288=CARTESIAN_POINT('Ctrl Pts',(42.9577176859246,-47.8703078362897,-5.99677411365216));
#32289=CARTESIAN_POINT('Ctrl Pts',(42.6988959526055,-46.7933246359025,-6.06206163292059));
#32290=CARTESIAN_POINT('Ctrl Pts',(42.6368929756464,-46.5353240279064,-6.07770182086387));
#32291=CARTESIAN_POINT('Ctrl Pts',(42.608036066463,-46.2693577230156,-6.09334200880715));
#32292=CARTESIAN_POINT('Ctrl Pts',(42.610367575631,-46.0028925918188,-6.10898219675042));
#32293=CARTESIAN_POINT('Ctrl Pts',(42.6150733527443,-46.0010327955954,-5.76601780324956));
#32294=CARTESIAN_POINT('Ctrl Pts',(42.6136987296515,-46.4911766911296,-5.73734992761755));
#32295=CARTESIAN_POINT('Ctrl Pts',(42.7134723622383,-46.980787483279,-5.70868205198553));
#32296=CARTESIAN_POINT('Ctrl Pts',(42.9172426426718,-47.4224132450777,-5.68001417635351));
#32297=CARTESIAN_POINT('Ctrl Pts',(43.3813040988082,-48.4281609608471,-5.61472665708508));
#32298=CARTESIAN_POINT('Ctrl Pts',(44.3847378702214,-49.1850372230187,-5.54943913781665));
#32299=CARTESIAN_POINT('Ctrl Pts',(45.4792791649687,-49.3549220805656,-5.48415161854822));
#32300=CARTESIAN_POINT('Ctrl Pts',(46.573820459716,-49.5248069381124,-5.41886409927979));
#32301=CARTESIAN_POINT('Ctrl Pts',(47.7594692777973,-49.1077003910346,-5.35357658001136));
#32302=CARTESIAN_POINT('Ctrl Pts',(48.5065597651538,-48.2899367876744,-5.28828906074293));
#32303=CARTESIAN_POINT('Ctrl Pts',(49.2536502525103,-47.4721731843143,-5.22300154147449));
#32304=CARTESIAN_POINT('Ctrl Pts',(49.562182409142,-46.2537525246719,-5.15771402220606));
#32305=CARTESIAN_POINT('Ctrl Pts',(49.2943254121986,-45.178980857527,-5.09242650293763));
#32306=CARTESIAN_POINT('Ctrl Pts',(49.0264684152553,-44.104209190382,-5.0271389836692));
#32307=CARTESIAN_POINT('Ctrl Pts',(48.1822222647368,-43.1730865157345,-4.96185146440077));
#32308=CARTESIAN_POINT('Ctrl Pts',(47.1387377295478,-42.8015740221576,-4.89656394513234));
#32309=CARTESIAN_POINT('Ctrl Pts',(46.0952531943588,-42.4300615285808,-4.83127642586391));
#32310=CARTESIAN_POINT('Ctrl Pts',(44.8525302744992,-42.6181592160746,-4.76598890659548));
#32311=CARTESIAN_POINT('Ctrl Pts',(43.965731587706,-43.2818380515628,-4.70070138732704));
#32312=CARTESIAN_POINT('Ctrl Pts',(43.1295474713166,-43.9076370168566,-4.63914019263455));
#32313=CARTESIAN_POINT('Ctrl Pts',(42.6098178745654,-44.9562782327072,-4.57757899794206));
#32314=CARTESIAN_POINT('Ctrl Pts',(42.6053665892596,-46.0010845675542,-4.51601780324957));
#32315=CARTESIAN_POINT('Origin',(46.,-46.,-5.));
#32316=CARTESIAN_POINT('',(42.6129095260066,-45.9974837232043,-3.26601780324956));
#32317=CARTESIAN_POINT('',(42.6153408714561,-46.0004230001184,-3.60898219675043));
#32318=CARTESIAN_POINT('',(42.61025,-46.,-5.));
#32319=CARTESIAN_POINT('Ctrl Pts',(42.6153408714561,-46.0004230001184,-3.60898219675043));
#32320=CARTESIAN_POINT('Ctrl Pts',(42.6160101781871,-45.4148448381747,-3.64322511091931));
#32321=CARTESIAN_POINT('Ctrl Pts',(42.7607380833382,-44.828956794812,-3.67746802508819));
#32322=CARTESIAN_POINT('Ctrl Pts',(43.047571146859,-44.3237493941201,-3.71171093925707));
#32323=CARTESIAN_POINT('Ctrl Pts',(43.5944468908181,-43.3605212721047,-3.7769984585255));
#32324=CARTESIAN_POINT('Ctrl Pts',(44.6578921134554,-42.6905770674502,-3.84228597779393));
#32325=CARTESIAN_POINT('Ctrl Pts',(45.7628330693288,-42.6132015000149,-3.90757349706236));
#32326=CARTESIAN_POINT('Ctrl Pts',(46.8677740252022,-42.5358259325796,-3.97286101633079));
#32327=CARTESIAN_POINT('Ctrl Pts',(48.0142107143115,-43.0510190023635,-4.03814853559923));
#32328=CARTESIAN_POINT('Ctrl Pts',(48.6899945433991,-43.9286280904542,-4.10343605486766));
#32329=CARTESIAN_POINT('Ctrl Pts',(49.3657783724867,-44.8062371785449,-4.16872357413609));
#32330=CARTESIAN_POINT('Ctrl Pts',(49.5709093415525,-46.0462622849423,-4.23401109340452));
#32331=CARTESIAN_POINT('Ctrl Pts',(49.2137491270214,-47.0947459881169,-4.29929861267295));
#32332=CARTESIAN_POINT('Ctrl Pts',(48.8565889124903,-48.1432296912914,-4.36458613194138));
#32333=CARTESIAN_POINT('Ctrl Pts',(47.9371375143622,-49.000171991243,-4.42987365120981));
#32334=CARTESIAN_POINT('Ctrl Pts',(46.8661422009793,-49.2827503588996,-4.49516117047824));
#32335=CARTESIAN_POINT('Ctrl Pts',(45.7951468875964,-49.5653287265562,-4.56044868974667));
#32336=CARTESIAN_POINT('Ctrl Pts',(44.5726076589586,-49.273543161918,-4.62573620901511));
#32337=CARTESIAN_POINT('Ctrl Pts',(43.7446704578678,-48.5377432669383,-4.69102372828354));
#32338=CARTESIAN_POINT('Ctrl Pts',(43.034687570683,-47.9067710952089,-4.74700988443917));
#32339=CARTESIAN_POINT('Ctrl Pts',(42.6148798756228,-46.9492878195862,-4.8029960405948));
#32340=CARTESIAN_POINT('Ctrl Pts',(42.6073208444166,-45.9976551525847,-4.85898219675043));
#32341=CARTESIAN_POINT('Ctrl Pts',(42.6053665892596,-46.0010845675542,-4.51601780324957));
#32342=CARTESIAN_POINT('Ctrl Pts',(42.605097151119,-46.0643271271258,-4.51229147867363));
#32343=CARTESIAN_POINT('Ctrl Pts',(42.6067156571417,-46.1275556359581,-4.50856515409769));
#32344=CARTESIAN_POINT('Ctrl Pts',(42.6102662023204,-46.1906754659139,-4.50483882952175));
#32345=CARTESIAN_POINT('Ctrl Pts',(42.672473957455,-47.2965740612939,-4.43955131025332));
#32346=CARTESIAN_POINT('Ctrl Pts',(43.327763921451,-48.3691112685711,-4.37426379098489));
#32347=CARTESIAN_POINT('Ctrl Pts',(44.2833978766996,-48.9291516696896,-4.30897627171646));
#32348=CARTESIAN_POINT('Ctrl Pts',(45.2390318319482,-49.4891920708081,-4.24368875244802));
#32349=CARTESIAN_POINT('Ctrl Pts',(46.4950097784494,-49.5367356657678,-4.1784012331796));
#32350=CARTESIAN_POINT('Ctrl Pts',(47.4902476695321,-49.0505432682207,-4.11311371391116));
#32351=CARTESIAN_POINT('Ctrl Pts',(48.4854855606147,-48.5643508706737,-4.04782619464273));
#32352=CARTESIAN_POINT('Ctrl Pts',(49.2199833962787,-47.5444224806199,-3.9825386753743));
#32353=CARTESIAN_POINT('Ctrl Pts',(49.3656183616491,-46.446391530422,-3.91725115610587));
#32354=CARTESIAN_POINT('Ctrl Pts',(49.5112533270196,-45.3483605802242,-3.85196363683744));
#32355=CARTESIAN_POINT('Ctrl Pts',(49.0680254220965,-44.1722270698824,-3.78667611756901));
#32356=CARTESIAN_POINT('Ctrl Pts',(48.2339382100517,-43.443406086684,-3.72138859830058));
#32357=CARTESIAN_POINT('Ctrl Pts',(47.399850998007,-42.7145851034855,-3.65610107903215));
#32358=CARTESIAN_POINT('Ctrl Pts',(46.1749044788406,-42.4330766474304,-3.59081355976371));
#32359=CARTESIAN_POINT('Ctrl Pts',(45.1063200017372,-42.7246391992172,-3.52552604049528));
#32360=CARTESIAN_POINT('Ctrl Pts',(44.0377355246337,-43.016201751004,-3.46023852122685));
#32361=CARTESIAN_POINT('Ctrl Pts',(43.1255130895933,-43.8808353106326,-3.39495100195842));
#32362=CARTESIAN_POINT('Ctrl Pts',(42.7771705717271,-44.932281467922,-3.32966348268999));
#32363=CARTESIAN_POINT('Ctrl Pts',(42.6639764192765,-45.2739496551732,-3.30844825620985));
#32364=CARTESIAN_POINT('Ctrl Pts',(42.6103240227328,-45.6353439396863,-3.28723302972971));
#32365=CARTESIAN_POINT('Ctrl Pts',(42.6129095260066,-45.9974837232043,-3.26601780324956));
#32366=CARTESIAN_POINT('Origin',(46.,-46.,-5.));
#32367=CARTESIAN_POINT('',(42.6120197259946,-46.0027475428216,-2.01601780324957));
#32368=CARTESIAN_POINT('',(42.6060559323604,-46.0016943206056,-2.35898219675043));
#32369=CARTESIAN_POINT('',(42.61025,-46.,-5.));
#32370=CARTESIAN_POINT('Ctrl Pts',(42.6060559323604,-46.0016943206056,-2.35898219675043));
#32371=CARTESIAN_POINT('Ctrl Pts',(42.6122935187612,-44.9966832429612,-2.41816666197539));
#32372=CARTESIAN_POINT('Ctrl Pts',(43.0878127283745,-43.9865345414923,-2.47735112720035));
#32373=CARTESIAN_POINT('Ctrl Pts',(43.869639312536,-43.3564767353091,-2.53653559242531));
#32374=CARTESIAN_POINT('Ctrl Pts',(44.7320872198372,-42.6614478792562,-2.60182311169374));
#32375=CARTESIAN_POINT('Ctrl Pts',(45.9672719776796,-42.4289409701107,-2.66711063096218));
#32376=CARTESIAN_POINT('Ctrl Pts',(47.0233986173667,-42.7628241355343,-2.73239815023061));
#32377=CARTESIAN_POINT('Ctrl Pts',(48.0795252570539,-43.0967073009578,-2.79768566949904));
#32378=CARTESIAN_POINT('Ctrl Pts',(48.9565937785859,-43.9969805409503,-2.86297318876747));
#32379=CARTESIAN_POINT('Ctrl Pts',(49.2627905908148,-45.0614639981771,-2.9282607080359));
#32380=CARTESIAN_POINT('Ctrl Pts',(49.5689874030437,-46.1259474554039,-2.99354822730433));
#32381=CARTESIAN_POINT('Ctrl Pts',(49.3043125059696,-47.3546411298651,-3.05883574657276));
#32382=CARTESIAN_POINT('Ctrl Pts',(48.5870043599298,-48.1986497299566,-3.12412326584119));
#32383=CARTESIAN_POINT('Ctrl Pts',(47.86969621389,-49.0426583300481,-3.18941078510962));
#32384=CARTESIAN_POINT('Ctrl Pts',(46.6997548188846,-49.5019818557699,-3.25469830437805));
#32385=CARTESIAN_POINT('Ctrl Pts',(45.5998290294583,-49.3714263208636,-3.31998582364648));
#32386=CARTESIAN_POINT('Ctrl Pts',(44.4999032400321,-49.2408707859573,-3.38527334291491));
#32387=CARTESIAN_POINT('Ctrl Pts',(43.469993056185,-48.5204361904228,-3.45056086218334));
#32388=CARTESIAN_POINT('Ctrl Pts',(42.970191096902,-47.5319628729674,-3.51584838145177));
#32389=CARTESIAN_POINT('Ctrl Pts',(42.7325322820506,-47.0619379105289,-3.54689298655132));
#32390=CARTESIAN_POINT('Ctrl Pts',(42.6147340783819,-46.5313078045718,-3.57793759165088));
#32391=CARTESIAN_POINT('Ctrl Pts',(42.6153408714561,-46.0004230001184,-3.60898219675043));
#32392=CARTESIAN_POINT('Ctrl Pts',(42.6129095260066,-45.9974837232043,-3.26601780324956));
#32393=CARTESIAN_POINT('Ctrl Pts',(42.6182806238543,-46.7497891762914,-3.22194551046127));
#32394=CARTESIAN_POINT('Ctrl Pts',(42.8663490738179,-47.505311866065,-3.17787321767298));
#32395=CARTESIAN_POINT('Ctrl Pts',(43.3274955589895,-48.093889309761,-3.13380092488469));
#32396=CARTESIAN_POINT('Ctrl Pts',(44.0106256648098,-48.9657922393603,-3.06851340561626));
#32397=CARTESIAN_POINT('Ctrl Pts',(45.1613484771422,-49.4713393436086,-3.00322588634783));
#32398=CARTESIAN_POINT('Ctrl Pts',(46.2656006877289,-49.3846873276029,-2.9379383670794));
#32399=CARTESIAN_POINT('Ctrl Pts',(47.3698528983157,-49.2980353115972,-2.87265084781097));
#32400=CARTESIAN_POINT('Ctrl Pts',(48.4276345071569,-48.6191841753375,-2.80736332854254));
#32401=CARTESIAN_POINT('Ctrl Pts',(48.9664018219562,-47.651397283792,-2.74207580927411));
#32402=CARTESIAN_POINT('Ctrl Pts',(49.5051691367556,-46.6836103922464,-2.67678829000568));
#32403=CARTESIAN_POINT('Ctrl Pts',(49.5249221575132,-45.426887745415,-2.61150077073725));
#32404=CARTESIAN_POINT('Ctrl Pts',(49.0168367155399,-44.442646794401,-2.54621325146882));
#32405=CARTESIAN_POINT('Ctrl Pts',(48.5087512735665,-43.4584058433871,-2.48092573220038));
#32406=CARTESIAN_POINT('Ctrl Pts',(47.4728273688623,-42.7466465881905,-2.41563821293195));
#32407=CARTESIAN_POINT('Ctrl Pts',(46.3718438942752,-42.6253323397915,-2.35035069366352));
#32408=CARTESIAN_POINT('Ctrl Pts',(45.2708604196881,-42.5040180913925,-2.28506317439509));
#32409=CARTESIAN_POINT('Ctrl Pts',(44.1048173752182,-42.973148849791,-2.21977565512666));
#32410=CARTESIAN_POINT('Ctrl Pts',(43.3946225937203,-43.8231524727757,-2.15448813585823));
#32411=CARTESIAN_POINT('Ctrl Pts',(42.8925311847605,-44.4240855235442,-2.10833135832201));
#32412=CARTESIAN_POINT('Ctrl Pts',(42.6182802792207,-45.2153851332211,-2.06217458078579));
#32413=CARTESIAN_POINT('Ctrl Pts',(42.6120197259946,-46.0027475428216,-2.01601780324957));
#32414=CARTESIAN_POINT('Origin',(46.,-46.,-5.));
#32415=CARTESIAN_POINT('',(42.6059703323355,-45.9984546826137,-0.766017803249566));
#32416=CARTESIAN_POINT('',(42.6118898788522,-45.9972329038001,-1.10898219675043));
#32417=CARTESIAN_POINT('',(42.61025,-46.,-5.));
#32418=CARTESIAN_POINT('',(48.5732344270147,-43.7934484719077,0.));
#32419=CARTESIAN_POINT('Ctrl Pts',(42.6059703323355,-45.9984546826137,-0.766017803249566));
#32420=CARTESIAN_POINT('Ctrl Pts',(42.6120010430613,-47.0081804904946,-0.706541093305004));
#32421=CARTESIAN_POINT('Ctrl Pts',(43.092762513117,-48.0226959853748,-0.647064383360442));
#32422=CARTESIAN_POINT('Ctrl Pts',(43.881269223622,-48.652638909118,-0.58758767341588));
#32423=CARTESIAN_POINT('Ctrl Pts',(44.7468121748606,-49.3441265655507,-0.522300154147449));
#32424=CARTESIAN_POINT('Ctrl Pts',(45.9831705630329,-49.572226239798,-0.457012634879018));
#32425=CARTESIAN_POINT('Ctrl Pts',(47.0377267586678,-49.2331399892057,-0.391725115610587));
#32426=CARTESIAN_POINT('Ctrl Pts',(48.0922829543027,-48.8940537386135,-0.326437596342156));
#32427=CARTESIAN_POINT('Ctrl Pts',(48.9650369574003,-47.9877815631816,-0.261150077073725));
#32428=CARTESIAN_POINT('Ctrl Pts',(49.2663063067355,-46.9237453887335,-0.195862557805293));
#32429=CARTESIAN_POINT('Ctrl Pts',(49.5675756560707,-45.8597092142853,-0.130575038536862));
#32430=CARTESIAN_POINT('Ctrl Pts',(49.2973603516436,-44.6379090408209,-0.065287519268431));
#32431=CARTESIAN_POINT('Ctrl Pts',(48.5732344270147,-43.7934484719077,1.57716942569499E-16));
#32432=CARTESIAN_POINT('',(43.4219943175761,-43.7905055070549,-2.82134898316155E-15));
#32433=CARTESIAN_POINT('Origin',(46.,-46.,0.));
#32434=CARTESIAN_POINT('Ctrl Pts',(43.4219651657257,-43.7904875258606,-1.80411241501588E-15));
#32435=CARTESIAN_POINT('Ctrl Pts',(44.1103019067085,-42.9932828189542,-0.0620616329205985));
#32436=CARTESIAN_POINT('Ctrl Pts',(45.2006369367306,-42.5364250742059,-0.124123265841195));
#32437=CARTESIAN_POINT('Ctrl Pts',(46.2508550217425,-42.6143560679205,-0.186184898761792));
#32438=CARTESIAN_POINT('Ctrl Pts',(47.3556621341977,-42.6963378175832,-0.251472418030223));
#32439=CARTESIAN_POINT('Ctrl Pts',(48.4160734564188,-43.3701484975484,-0.316759937298653));
#32440=CARTESIAN_POINT('Ctrl Pts',(48.9590107118729,-44.3354564297113,-0.382047456567084));
#32441=CARTESIAN_POINT('Ctrl Pts',(49.501947967327,-45.3007643618741,-0.447334975835515));
#32442=CARTESIAN_POINT('Ctrl Pts',(49.5274111560141,-46.5575695462346,-0.512622495103946));
#32443=CARTESIAN_POINT('Ctrl Pts',(49.0237120278267,-47.5440867715274,-0.577910014372376));
#32444=CARTESIAN_POINT('Ctrl Pts',(48.5200128996393,-48.5306039968202,-0.643197533640807));
#32445=CARTESIAN_POINT('Ctrl Pts',(47.4871514545773,-49.2468332630454,-0.708485052909238));
#32446=CARTESIAN_POINT('Ctrl Pts',(46.3866918750129,-49.372975105968,-0.773772572177669));
#32447=CARTESIAN_POINT('Ctrl Pts',(45.2862322954484,-49.4991169488906,-0.8390600914461));
#32448=CARTESIAN_POINT('Ctrl Pts',(44.1181745813813,-49.0351713685107,-0.904347610714531));
#32449=CARTESIAN_POINT('Ctrl Pts',(43.404251173025,-48.1883177881507,-0.969635129982962));
#32450=CARTESIAN_POINT('Ctrl Pts',(42.8963279948238,-47.5858209979168,-1.01608415223878));
#32451=CARTESIAN_POINT('Ctrl Pts',(42.618272082018,-46.7895092640711,-1.06253317449461));
#32452=CARTESIAN_POINT('Ctrl Pts',(42.6118898788522,-45.9972329038001,-1.10898219675043));
#32453=CARTESIAN_POINT('Origin',(46.,-46.,2.76038497140452));
#32454=CARTESIAN_POINT('',(41.9196909029574,-45.9976755478274,-7.76038497140452));
#32455=CARTESIAN_POINT('',(41.9137289353857,-46.0033881484067,-7.86461502859548));
#32456=CARTESIAN_POINT('',(41.915,-45.9999999999999,2.76038497140452));
#32457=CARTESIAN_POINT('',(42.5743852316216,-48.2253962475631,-9.));
#32458=CARTESIAN_POINT('Ctrl Pts',(41.9137289353857,-46.0033881484067,-7.86461502859549));
#32459=CARTESIAN_POINT('Ctrl Pts',(41.9230935686005,-44.9361783803566,-7.91663908938817));
#32460=CARTESIAN_POINT('Ctrl Pts',(42.891985057322,-42.5144885624548,-8.03395066944928));
#32461=CARTESIAN_POINT('Ctrl Pts',(46.947226477628,-41.2871007943775,-8.21654976877883));
#32462=CARTESIAN_POINT('Ctrl Pts',(50.4487171774031,-44.1804056791643,-8.41241232658412));
#32463=CARTESIAN_POINT('Ctrl Pts',(49.979557221961,-48.7013821925377,-8.60827488438941));
#32464=CARTESIAN_POINT('Ctrl Pts',(45.946358746692,-50.8047710666759,-8.80413744219471));
#32465=CARTESIAN_POINT('Ctrl Pts',(43.3046954441484,-49.3495832107922,-8.93471248073157));
#32466=CARTESIAN_POINT('Ctrl Pts',(42.5743852316216,-48.2253962475631,-9.));
#32467=CARTESIAN_POINT('',(41.9138451336777,-46.212441516533,-8.99999999999999));
#32468=CARTESIAN_POINT('Origin',(46.,-46.,-9.));
#32469=CARTESIAN_POINT('Ctrl Pts',(41.9196909029574,-45.9976755478274,-7.76038497140452));
#32470=CARTESIAN_POINT('Ctrl Pts',(41.9169749126423,-45.4889856236339,-7.78509075167359));
#32471=CARTESIAN_POINT('Ctrl Pts',(42.2389226908427,-43.6393407000909,-7.8750840512111));
#32472=CARTESIAN_POINT('Ctrl Pts',(44.9804152684286,-41.3020771440901,-8.03036487001703));
#32473=CARTESIAN_POINT('Ctrl Pts',(49.3490847557137,-42.5514377898613,-8.22622742782233));
#32474=CARTESIAN_POINT('Ctrl Pts',(50.7259989091243,-46.8818733140433,-8.42208998562761));
#32475=CARTESIAN_POINT('Ctrl Pts',(47.8793446557761,-50.4245587866615,-8.61795254343292));
#32476=CARTESIAN_POINT('Ctrl Pts',(43.4302591581606,-50.0204898973754,-8.81058921489037));
#32477=CARTESIAN_POINT('Ctrl Pts',(41.9843544528723,-47.4797545535775,-8.9379383670794));
#32478=CARTESIAN_POINT('Ctrl Pts',(41.9138040800513,-46.2124372338608,-9.));
#32479=CARTESIAN_POINT('Origin',(46.,-46.,2.76038497140452));
#32480=CARTESIAN_POINT('',(41.9151416908186,-46.0034858728755,-6.51038497140452));
#32481=CARTESIAN_POINT('',(41.912796133594,-45.9967790955024,-6.61461502859548));
#32482=CARTESIAN_POINT('',(41.915,-45.9999999999999,2.76038497140452));
#32483=CARTESIAN_POINT('Ctrl Pts',(41.912796133594,-45.9967790955024,-6.61461502859548));
#32484=CARTESIAN_POINT('Ctrl Pts',(41.9107304308479,-45.7573638992105,-6.62629312117581));
#32485=CARTESIAN_POINT('Ctrl Pts',(42.0377964723628,-44.1816628889412,-6.70325873302458));
#32486=CARTESIAN_POINT('Ctrl Pts',(44.0829608206919,-41.591478562833,-6.84551186414177));
#32487=CARTESIAN_POINT('Ctrl Pts',(48.6116788957116,-41.9640100582522,-7.04137442194706));
#32488=CARTESIAN_POINT('Ctrl Pts',(50.8069346691015,-45.9425306737833,-7.23723697975236));
#32489=CARTESIAN_POINT('Ctrl Pts',(48.7074348723187,-49.9724245030734,-7.43309953755765));
#32490=CARTESIAN_POINT('Ctrl Pts',(44.1888312987275,-50.4530551698565,-7.62896209536294));
#32491=CARTESIAN_POINT('Ctrl Pts',(42.0589980216041,-47.8842560929907,-7.77280059237556));
#32492=CARTESIAN_POINT('Ctrl Pts',(41.9113414357962,-46.2754717233481,-7.85135157011974));
#32493=CARTESIAN_POINT('Ctrl Pts',(41.9137289353857,-46.0033881484067,-7.86461502859549));
#32494=CARTESIAN_POINT('Ctrl Pts',(41.9151416908186,-46.0034858728755,-6.51038497140452));
#32495=CARTESIAN_POINT('Ctrl Pts',(41.9240606763713,-44.9841466877243,-6.56003230272967));
#32496=CARTESIAN_POINT('Ctrl Pts',(42.8214698193968,-42.6103273354142,-6.67496715332326));
#32497=CARTESIAN_POINT('Ctrl Pts',(46.777185224748,-41.255945113868,-6.85518952318527));
#32498=CARTESIAN_POINT('Ctrl Pts',(50.3817996987672,-44.0226574502926,-7.05105208099057));
#32499=CARTESIAN_POINT('Ctrl Pts',(50.071451482069,-48.5560483299491,-7.24691463879586));
#32500=CARTESIAN_POINT('Ctrl Pts',(46.1234029447301,-50.8057104508671,-7.44277719660115));
#32501=CARTESIAN_POINT('Ctrl Pts',(42.5770326391767,-49.01948437455,-7.61393397413737));
#32502=CARTESIAN_POINT('Ctrl Pts',(41.9241521913235,-46.8332501182475,-7.71980323240516));
#32503=CARTESIAN_POINT('Ctrl Pts',(41.9196909029574,-45.9976755478274,-7.76038497140452));
#32504=CARTESIAN_POINT('Origin',(46.,-46.,2.76038497140452));
#32505=CARTESIAN_POINT('',(41.9114700639993,-45.9971742158887,-5.26038497140452));
#32506=CARTESIAN_POINT('',(41.9208126398586,-46.001244625712,-5.36461502859548));
#32507=CARTESIAN_POINT('',(41.915,-45.9999999999999,2.76038497140452));
#32508=CARTESIAN_POINT('Ctrl Pts',(41.9208126398586,-46.001244625712,-5.36461502859548));
#32509=CARTESIAN_POINT('Ctrl Pts',(41.9229286932863,-45.2467318609778,-5.40123467223189));
#32510=CARTESIAN_POINT('Ctrl Pts',(42.4823083976697,-43.1441149653643,-5.50314183513673));
#32511=CARTESIAN_POINT('Ctrl Pts',(45.8362350648755,-41.1954966730761,-5.67033651731001));
#32512=CARTESIAN_POINT('Ctrl Pts',(49.9115574163095,-43.2053998426678,-5.86619907511531));
#32513=CARTESIAN_POINT('Ctrl Pts',(50.4920529547756,-47.7121708254118,-6.0620616329206));
#32514=CARTESIAN_POINT('Ctrl Pts',(47.0590723399817,-50.6891832485807,-6.25792419072589));
#32515=CARTESIAN_POINT('Ctrl Pts',(42.9409560641467,-49.5488892301137,-6.44210865595086));
#32516=CARTESIAN_POINT('Ctrl Pts',(41.9222789441782,-47.0958379807898,-6.56100560190738));
#32517=CARTESIAN_POINT('Ctrl Pts',(41.912796133594,-45.9967790955024,-6.61461502859548));
#32518=CARTESIAN_POINT('Ctrl Pts',(41.9114700639993,-45.9971742158887,-5.26038497140452));
#32519=CARTESIAN_POINT('Ctrl Pts',(41.9099566544234,-45.8066458331328,-5.26968633451732));
#32520=CARTESIAN_POINT('Ctrl Pts',(42.0077825243435,-44.2803336702357,-5.34427521689855));
#32521=CARTESIAN_POINT('Ctrl Pts',(43.9262270571184,-41.6630037489246,-5.48415161854821));
#32522=CARTESIAN_POINT('Ctrl Pts',(48.4653741677054,-41.8730155103115,-5.68001417635351));
#32523=CARTESIAN_POINT('Ctrl Pts',(50.8018040255352,-45.7703295385275,-5.8758767341588));
#32524=CARTESIAN_POINT('Ctrl Pts',(48.8480063650781,-49.8728452943253,-6.0717392919641));
#32525=CARTESIAN_POINT('Ctrl Pts',(44.349624114825,-50.5151224407608,-6.26760184976939));
#32526=CARTESIAN_POINT('Ctrl Pts',(42.0922727086059,-47.9830688501961,-6.41381707624953));
#32527=CARTESIAN_POINT('Ctrl Pts',(41.9123319806774,-46.3246039674072,-6.49474478346124));
#32528=CARTESIAN_POINT('Ctrl Pts',(41.9151416908186,-46.0034858728755,-6.51038497140452));
#32529=CARTESIAN_POINT('Origin',(46.,-46.,2.76038497140452));
#32530=CARTESIAN_POINT('',(41.9211350276268,-46.0005097589745,-4.01038497140452));
#32531=CARTESIAN_POINT('',(41.9091149840328,-46.0013070162871,-4.11461502859548));
#32532=CARTESIAN_POINT('',(41.915,-45.9999999999999,2.76038497140452));
#32533=CARTESIAN_POINT('Ctrl Pts',(41.9091149840328,-46.0013070162871,-4.11461502859548));
#32534=CARTESIAN_POINT('Ctrl Pts',(41.9144792440739,-44.7422071186988,-4.17617622328797));
#32535=CARTESIAN_POINT('Ctrl Pts',(43.2050471763048,-42.1382708909912,-4.30302493724889));
#32536=CARTESIAN_POINT('Ctrl Pts',(47.6123998603384,-41.4711770162521,-4.49516117047826));
#32537=CARTESIAN_POINT('Ctrl Pts',(50.6646121398881,-44.8374749372802,-4.69102372828354));
#32538=CARTESIAN_POINT('Ctrl Pts',(49.5491724822373,-49.2424443845602,-4.88688628608884));
#32539=CARTESIAN_POINT('Ctrl Pts',(45.2626834297744,-50.7504142155033,-5.08274884389412));
#32540=CARTESIAN_POINT('Ctrl Pts',(42.3132197363476,-48.5256744077654,-5.24199175806301));
#32541=CARTESIAN_POINT('Ctrl Pts',(41.9191560765917,-46.5919188091348,-5.33594715296346));
#32542=CARTESIAN_POINT('Ctrl Pts',(41.9208126398586,-46.001244625712,-5.36461502859548));
#32543=CARTESIAN_POINT('Ctrl Pts',(41.9211350276268,-46.0005097589745,-4.01038497140452));
#32544=CARTESIAN_POINT('Ctrl Pts',(41.9219416115921,-45.294827395514,-4.0446278855734));
#32545=CARTESIAN_POINT('Ctrl Pts',(42.428887780726,-43.242606030091,-4.14415831901071));
#32546=CARTESIAN_POINT('Ctrl Pts',(45.6641826146291,-41.204450252827,-4.30897627171645));
#32547=CARTESIAN_POINT('Ctrl Pts',(49.8089076312337,-43.0670333548852,-4.50483882952175));
#32548=CARTESIAN_POINT('Ctrl Pts',(50.5505198521649,-47.5501095932216,-4.70070138732704));
#32549=CARTESIAN_POINT('Ctrl Pts',(47.2264172239299,-50.6482223997432,-4.89656394513234));
#32550=CARTESIAN_POINT('Ctrl Pts',(43.0164536107202,-49.6434230598024,-5.08312513982483));
#32551=CARTESIAN_POINT('Ctrl Pts',(41.9205794798788,-47.1439901889548,-5.20439881524889));
#32552=CARTESIAN_POINT('Ctrl Pts',(41.9114700639993,-45.9971742158887,-5.26038497140452));
#32553=CARTESIAN_POINT('Origin',(46.,-46.,2.76038497140452));
#32554=CARTESIAN_POINT('',(41.9099457138999,-46.0020418318974,-2.76038497140452));
#32555=CARTESIAN_POINT('',(41.9182050044213,-45.9969676257214,-2.86461502859548));
#32556=CARTESIAN_POINT('',(41.915,-45.9999999999999,2.76038497140452));
#32557=CARTESIAN_POINT('Ctrl Pts',(41.9182050044213,-45.9969676257214,-2.86461502859548));
#32558=CARTESIAN_POINT('Ctrl Pts',(41.9150892050634,-45.5605516612194,-2.88583025507562));
#32559=CARTESIAN_POINT('Ctrl Pts',(42.178719756358,-43.7847768478177,-2.97233300082419));
#32560=CARTESIAN_POINT('Ctrl Pts',(44.7345905347796,-41.3622408914429,-3.12412326584119));
#32561=CARTESIAN_POINT('Ctrl Pts',(49.1631529928913,-42.3799814708233,-3.31998582364649));
#32562=CARTESIAN_POINT('Ctrl Pts',(50.765559652625,-46.6320697278449,-3.51584838145178));
#32563=CARTESIAN_POINT('Ctrl Pts',(48.1101216480341,-50.3194279165342,-3.71171093925708));
#32564=CARTESIAN_POINT('Ctrl Pts',(43.5693709335647,-50.1475430411802,-3.90757349706237));
#32565=CARTESIAN_POINT('Ctrl Pts',(41.9449141512117,-47.488734824337,-4.04187486017517));
#32566=CARTESIAN_POINT('Ctrl Pts',(41.9087902831539,-46.0775208538414,-4.11088870401954));
#32567=CARTESIAN_POINT('Ctrl Pts',(41.9091149840328,-46.0013070162871,-4.11461502859548));
#32568=CARTESIAN_POINT('Ctrl Pts',(41.9099457138999,-46.0020418318974,-2.76038497140452));
#32569=CARTESIAN_POINT('Ctrl Pts',(41.9174626518591,-44.7908993428709,-2.81956943662948));
#32570=CARTESIAN_POINT('Ctrl Pts',(43.1226549378218,-42.230701146723,-2.94404142112287));
#32571=CARTESIAN_POINT('Ctrl Pts',(47.4490849663269,-41.4163089133544,-3.13380092488469));
#32572=CARTESIAN_POINT('Ctrl Pts',(50.6199603203723,-44.6710765381374,-3.32966348268999));
#32573=CARTESIAN_POINT('Ctrl Pts',(49.6630782896489,-49.1131861274939,-3.52552604049528));
#32574=CARTESIAN_POINT('Ctrl Pts',(45.433376454472,-50.7737834599584,-3.72138859830057));
#32575=CARTESIAN_POINT('Ctrl Pts',(42.3609059541842,-48.6245532873833,-3.88300824193699));
#32576=CARTESIAN_POINT('Ctrl Pts',(41.9204037790959,-46.6402809592672,-3.97934036630497));
#32577=CARTESIAN_POINT('Ctrl Pts',(41.9211350276268,-46.0005097589745,-4.01038497140452));
#32578=CARTESIAN_POINT('Origin',(46.,-46.,2.76038497140452));
#32579=CARTESIAN_POINT('',(41.9169762239431,-45.9966653623493,-1.51038497140452));
#32580=CARTESIAN_POINT('',(41.9171327032046,-46.0033110738038,-1.61461502859548));
#32581=CARTESIAN_POINT('',(41.915,-45.9999999999999,2.76038497140452));
#32582=CARTESIAN_POINT('Ctrl Pts',(41.9171327032046,-46.0033110738038,-1.61461502859548));
#32583=CARTESIAN_POINT('Ctrl Pts',(41.9246773185682,-45.0544577827888,-1.6607718061317));
#32584=CARTESIAN_POINT('Ctrl Pts',(42.7226625049108,-42.7520210224136,-1.77221610293635));
#32585=CARTESIAN_POINT('Ctrl Pts',(46.5265139467765,-41.2216283664815,-1.94894791900943));
#32586=CARTESIAN_POINT('Ctrl Pts',(50.2717008933508,-43.7948593340848,-2.14481047681473));
#32587=CARTESIAN_POINT('Ctrl Pts',(50.2002875828164,-48.338302371748,-2.34067303462002));
#32588=CARTESIAN_POINT('Ctrl Pts',(46.3760782410217,-50.7925602594573,-2.53653559242531));
#32589=CARTESIAN_POINT('Ctrl Pts',(42.6664797940018,-49.1628222089761,-2.71118292375047));
#32590=CARTESIAN_POINT('Ctrl Pts',(41.9246777338874,-46.9035736514935,-2.82054273580719));
#32591=CARTESIAN_POINT('Ctrl Pts',(41.9182050044213,-45.9969676257214,-2.86461502859548));
#32592=CARTESIAN_POINT('Ctrl Pts',(41.9169762239431,-45.9966653623493,-1.51038497140452));
#32593=CARTESIAN_POINT('Ctrl Pts',(41.9138568697487,-45.6094337867792,-1.52922346841713));
#32594=CARTESIAN_POINT('Ctrl Pts',(42.1404160610226,-43.8837676902663,-1.61334948469817));
#32595=CARTESIAN_POINT('Ctrl Pts',(44.5692320816632,-41.4105744865513,-1.76276302024764));
#32596=CARTESIAN_POINT('Ctrl Pts',(49.0314013549138,-42.268956305567,-1.95862557805293));
#32597=CARTESIAN_POINT('Ctrl Pts',(50.7851507003408,-46.4609045572623,-2.15448813585823));
#32598=CARTESIAN_POINT('Ctrl Pts',(48.263541336862,-50.2410414729541,-2.35035069366352));
#32599=CARTESIAN_POINT('Ctrl Pts',(43.7195496474102,-50.2319758772438,-2.54621325146881));
#32600=CARTESIAN_POINT('Ctrl Pts',(41.9704479226572,-47.5870902922536,-2.68289134404915));
#32601=CARTESIAN_POINT('Ctrl Pts',(41.9091705733553,-46.1269338628851,-2.75428191736105));
#32602=CARTESIAN_POINT('Ctrl Pts',(41.9099457138999,-46.0020418318974,-2.76038497140452));
#32603=CARTESIAN_POINT('Origin',(46.,-46.,2.76038497140452));
#32604=CARTESIAN_POINT('',(41.9194196464784,-46.0038358614086,-0.260384971404518));
#32605=CARTESIAN_POINT('',(41.9098425569998,-45.9981377324218,-0.364615028595479));
#32606=CARTESIAN_POINT('',(41.915,-45.9999999999999,2.76038497140452));
#32607=CARTESIAN_POINT('',(44.942095577027,-49.9456385074984,0.));
#32608=CARTESIAN_POINT('Ctrl Pts',(44.942095577027,-49.9456385074984,5.55111512312578E-16));
#32609=CARTESIAN_POINT('Ctrl Pts',(43.6472519732776,-49.5984650974504,-0.0652875192684306));
#32610=CARTESIAN_POINT('Ctrl Pts',(42.1846929797356,-48.2273651784823,-0.152082509736603));
#32611=CARTESIAN_POINT('Ctrl Pts',(41.9164508003806,-46.4463095999464,-0.238877500204776));
#32612=CARTESIAN_POINT('Ctrl Pts',(41.9194196464784,-46.0038358614086,-0.260384971404518));
#32613=CARTESIAN_POINT('',(47.0606474189675,-49.9518122604704,1.27273922847335E-15));
#32614=CARTESIAN_POINT('Origin',(46.,-46.,0.));
#32615=CARTESIAN_POINT('Ctrl Pts',(47.0606641786102,-49.9518499819597,3.86518074491082E-16));
#32616=CARTESIAN_POINT('Ctrl Pts',(45.8335725344782,-50.2763751643415,-0.0620616329205975));
#32617=CARTESIAN_POINT('Ctrl Pts',(43.101024906791,-49.7132899277509,-0.183599975785757));
#32618=CARTESIAN_POINT('Ctrl Pts',(41.917110188334,-47.2149619599294,-0.305138318650917));
#32619=CARTESIAN_POINT('Ctrl Pts',(41.9098425569998,-45.9981377324218,-0.364615028595479));
#32620=CARTESIAN_POINT('Origin',(-46.,46.,-5.));
#32621=CARTESIAN_POINT('',(-49.390804277264,45.9971884954151,-8.26601780324957));
#32622=CARTESIAN_POINT('',(-49.3955878307095,45.9998426774376,-8.60898219675043));
#32623=CARTESIAN_POINT('',(-49.38975,46.,-5.));
#32624=CARTESIAN_POINT('',(-44.696617959125,49.1291532909119,-9.));
#32625=CARTESIAN_POINT('Ctrl Pts',(-49.3955878307095,45.9998426774376,-8.60898219675043));
#32626=CARTESIAN_POINT('Ctrl Pts',(-49.3946787862589,47.103578210484,-8.67403394523185));
#32627=CARTESIAN_POINT('Ctrl Pts',(-48.8034231054609,48.2078784353154,-8.73908569371328));
#32628=CARTESIAN_POINT('Ctrl Pts',(-47.8878799940434,48.8209858903891,-8.8041374421947));
#32629=CARTESIAN_POINT('Ctrl Pts',(-46.9690186271608,49.4363154660142,-8.86942496146314));
#32630=CARTESIAN_POINT('Ctrl Pts',(-45.723514902722,49.5568853032748,-8.93471248073157));
#32631=CARTESIAN_POINT('Ctrl Pts',(-44.696617959125,49.1291532909119,-9.));
#32632=CARTESIAN_POINT('',(-49.38975,46.,-9.));
#32633=CARTESIAN_POINT('Origin',(-46.,46.,-9.));
#32634=CARTESIAN_POINT('',(-49.38975,46.,-10.));
#32635=CARTESIAN_POINT('',(-49.38975,46.,-5.));
#32636=CARTESIAN_POINT('Origin',(-46.,46.,-10.));
#32637=CARTESIAN_POINT('',(-43.101998404785,44.230942529973,-9.00000000000001));
#32638=CARTESIAN_POINT('Origin',(-46.,46.,-9.));
#32639=CARTESIAN_POINT('Ctrl Pts',(-43.1019723047815,44.2309203707046,-9.00000000000001));
#32640=CARTESIAN_POINT('Ctrl Pts',(-42.5564929566499,45.1319175212271,-8.93793836707941));
#32641=CARTESIAN_POINT('Ctrl Pts',(-42.4589283016514,46.3100640648579,-8.87587673415881));
#32642=CARTESIAN_POINT('Ctrl Pts',(-42.8575804387187,47.2847985850388,-8.81381510123821));
#32643=CARTESIAN_POINT('Ctrl Pts',(-43.2769540171336,48.3101985910188,-8.74852758196978));
#32644=CARTESIAN_POINT('Ctrl Pts',(-44.2454705226989,49.1104907897642,-8.68324006270135));
#32645=CARTESIAN_POINT('Ctrl Pts',(-45.3313095094966,49.3285582706994,-8.61795254343292));
#32646=CARTESIAN_POINT('Ctrl Pts',(-46.4171484962944,49.5466257516345,-8.55266502416448));
#32647=CARTESIAN_POINT('Ctrl Pts',(-47.6203099643246,49.1824685147595,-8.48737750489605));
#32648=CARTESIAN_POINT('Ctrl Pts',(-48.4028919771909,48.3985716685866,-8.42208998562762));
#32649=CARTESIAN_POINT('Ctrl Pts',(-49.0264888708823,47.773927055995,-8.37006592483494));
#32650=CARTESIAN_POINT('Ctrl Pts',(-49.383033529559,46.8827634791248,-8.31804186404225));
#32651=CARTESIAN_POINT('Ctrl Pts',(-49.390804277264,45.9971884954151,-8.26601780324957));
#32652=CARTESIAN_POINT('Origin',(-46.,46.,-5.));
#32653=CARTESIAN_POINT('',(-49.3915783323198,46.002672719373,-7.01601780324957));
#32654=CARTESIAN_POINT('',(-49.3858580102862,46.0019288502567,-7.35898219675043));
#32655=CARTESIAN_POINT('',(-49.38975,46.,-5.));
#32656=CARTESIAN_POINT('Ctrl Pts',(-49.3858580102862,46.0019288502567,-7.35898219675043));
#32657=CARTESIAN_POINT('Ctrl Pts',(-49.3881117467423,46.4240419378505,-7.3836879770195));
#32658=CARTESIAN_POINT('Ctrl Pts',(-49.314770291966,46.8454011027671,-7.40839375728858));
#32659=CARTESIAN_POINT('Ctrl Pts',(-49.1621985550924,47.2357983892983,-7.43309953755765));
#32660=CARTESIAN_POINT('Ctrl Pts',(-48.7590123329831,48.2674626431351,-7.49838705682608));
#32661=CARTESIAN_POINT('Ctrl Pts',(-47.8025341154912,49.0829095742609,-7.56367457609451));
#32662=CARTESIAN_POINT('Ctrl Pts',(-46.7201048386092,49.3178456032442,-7.62896209536294));
#32663=CARTESIAN_POINT('Ctrl Pts',(-45.6376755617271,49.5527816322275,-7.69424961463137));
#32664=CARTESIAN_POINT('Ctrl Pts',(-44.4292952254548,49.2072067590683,-7.75953713389981));
#32665=CARTESIAN_POINT('Ctrl Pts',(-43.6346769280645,48.4355169169347,-7.82482465316824));
#32666=CARTESIAN_POINT('Ctrl Pts',(-42.8400586306741,47.663827074801,-7.89011217243667));
#32667=CARTESIAN_POINT('Ctrl Pts',(-42.4592023721657,46.4660222636928,-7.9553996917051));
#32668=CARTESIAN_POINT('Ctrl Pts',(-42.6624684232406,45.3771640589127,-8.02068721097353));
#32669=CARTESIAN_POINT('Ctrl Pts',(-42.8657344743155,44.2883058541325,-8.08597473024196));
#32670=CARTESIAN_POINT('Ctrl Pts',(-43.6531228349737,43.3083942556804,-8.15126224951039));
#32671=CARTESIAN_POINT('Ctrl Pts',(-44.6724329422056,42.8752570111787,-8.21654976877882));
#32672=CARTESIAN_POINT('Ctrl Pts',(-45.6917430494375,42.4421197666769,-8.28183728804725));
#32673=CARTESIAN_POINT('Ctrl Pts',(-46.942974903243,42.5557568761255,-8.34712480731569));
#32674=CARTESIAN_POINT('Ctrl Pts',(-47.8680862672342,43.1652560477182,-8.41241232658412));
#32675=CARTESIAN_POINT('Ctrl Pts',(-48.7931976312253,43.7747552193109,-8.47769984585255));
#32676=CARTESIAN_POINT('Ctrl Pts',(-49.3921885054021,44.8801164530478,-8.54298736512098));
#32677=CARTESIAN_POINT('Ctrl Pts',(-49.3955744378273,45.9878417269111,-8.60827488438941));
#32678=CARTESIAN_POINT('Ctrl Pts',(-49.3955866653397,45.9918420207273,-8.60851065517642));
#32679=CARTESIAN_POINT('Ctrl Pts',(-49.3955911254115,45.9958423453736,-8.60874642596342));
#32680=CARTESIAN_POINT('Ctrl Pts',(-49.3955878307095,45.9998426774376,-8.60898219675043));
#32681=CARTESIAN_POINT('Ctrl Pts',(-49.390804277264,45.9971884954151,-8.26601780324957));
#32682=CARTESIAN_POINT('Ctrl Pts',(-49.3927854180658,45.7714124440146,-8.25275434477382));
#32683=CARTESIAN_POINT('Ctrl Pts',(-49.3720966873643,45.5459996442359,-8.23949088629808));
#32684=CARTESIAN_POINT('Ctrl Pts',(-49.327383847567,45.3254592826471,-8.22622742782233));
#32685=CARTESIAN_POINT('Ctrl Pts',(-49.1072911473747,44.2398801983513,-8.1609399085539));
#32686=CARTESIAN_POINT('Ctrl Pts',(-48.305103189288,43.2723584852303,-8.09565238928547));
#32687=CARTESIAN_POINT('Ctrl Pts',(-47.2790832574686,42.8550691740869,-8.03036487001704));
#32688=CARTESIAN_POINT('Ctrl Pts',(-46.2530633256491,42.4377798629434,-7.96507735074861));
#32689=CARTESIAN_POINT('Ctrl Pts',(-45.003211420097,42.5707229537774,-7.89978983148017));
#32690=CARTESIAN_POINT('Ctrl Pts',(-44.0879232413465,43.1945315388044,-7.83450231221174));
#32691=CARTESIAN_POINT('Ctrl Pts',(-43.1726350625961,43.8183401238314,-7.76921479294331));
#32692=CARTESIAN_POINT('Ctrl Pts',(-42.5919106106473,44.9330142030514,-7.70392727367488));
#32693=CARTESIAN_POINT('Ctrl Pts',(-42.6051537334803,46.0405833305628,-7.63863975440645));
#32694=CARTESIAN_POINT('Ctrl Pts',(-42.6183968563134,47.1481524580742,-7.57335223513801));
#32695=CARTESIAN_POINT('Ctrl Pts',(-43.2256075539281,48.2486166338769,-7.50806471586958));
#32696=CARTESIAN_POINT('Ctrl Pts',(-44.1555376756467,48.8503700797306,-7.44277719660115));
#32697=CARTESIAN_POINT('Ctrl Pts',(-45.0854677973652,49.4521235255844,-7.37748967733272));
#32698=CARTESIAN_POINT('Ctrl Pts',(-46.3381173431877,49.5551662414892,-7.31220215806429));
#32699=CARTESIAN_POINT('Ctrl Pts',(-47.3538834999244,49.1134631917099,-7.24691463879586));
#32700=CARTESIAN_POINT('Ctrl Pts',(-48.3696496566611,48.6717601419306,-7.18162711952743));
#32701=CARTESIAN_POINT('Ctrl Pts',(-49.1485324243119,47.6853113264672,-7.116339600259));
#32702=CARTESIAN_POINT('Ctrl Pts',(-49.3425836444144,46.5947951363276,-7.05105208099057));
#32703=CARTESIAN_POINT('Ctrl Pts',(-49.3772939250174,46.3997326010758,-7.03937398841023));
#32704=CARTESIAN_POINT('Ctrl Pts',(-49.3932924608325,46.201340419597,-7.0276958958299));
#32705=CARTESIAN_POINT('Ctrl Pts',(-49.3915783323198,46.002672719373,-7.01601780324957));
#32706=CARTESIAN_POINT('Origin',(-46.,46.,-5.));
#32707=CARTESIAN_POINT('',(-49.3849262043165,45.9989672045366,-5.76601780324957));
#32708=CARTESIAN_POINT('',(-49.3896329814502,45.9971074077133,-6.10898219675043));
#32709=CARTESIAN_POINT('',(-49.38975,46.,-5.));
#32710=CARTESIAN_POINT('Ctrl Pts',(-49.3896329814502,45.9971074077133,-6.10898219675043));
#32711=CARTESIAN_POINT('Ctrl Pts',(-49.3822319686501,46.8429594447226,-6.15862952807558));
#32712=CARTESIAN_POINT('Ctrl Pts',(-49.0605621281795,47.6938378847277,-6.20827685940074));
#32713=CARTESIAN_POINT('Ctrl Pts',(-48.4872411182123,48.3109063253483,-6.25792419072589));
#32714=CARTESIAN_POINT('Ctrl Pts',(-47.7333092252755,49.122367216229,-6.32321170999432));
#32715=CARTESIAN_POINT('Ctrl Pts',(-46.5441987940589,49.5295021746259,-6.38849922926275));
#32716=CARTESIAN_POINT('Ctrl Pts',(-45.4511228133513,49.3504313564188,-6.45378674853118));
#32717=CARTESIAN_POINT('Ctrl Pts',(-44.3580468326437,49.1713605382117,-6.51907426779961));
#32718=CARTESIAN_POINT('Ctrl Pts',(-43.3610053024451,48.4060839434005,-6.58436178706805));
#32719=CARTESIAN_POINT('Ctrl Pts',(-42.9054059204164,47.3964744387992,-6.64964930633648));
#32720=CARTESIAN_POINT('Ctrl Pts',(-42.4498065383877,46.3868649341978,-6.71493682560491));
#32721=CARTESIAN_POINT('Ctrl Pts',(-42.5356493045288,45.1329225198063,-6.78022434487333));
#32722=CARTESIAN_POINT('Ctrl Pts',(-43.1245886239275,44.19482143211,-6.84551186414177));
#32723=CARTESIAN_POINT('Ctrl Pts',(-43.7135279433262,43.2567203444137,-6.9107993834102));
#32724=CARTESIAN_POINT('Ctrl Pts',(-44.8055638159825,42.6344605834126,-6.97608690267863));
#32725=CARTESIAN_POINT('Ctrl Pts',(-45.9128440093134,42.6060257295712,-7.04137442194706));
#32726=CARTESIAN_POINT('Ctrl Pts',(-47.0201242026443,42.5775908757298,-7.1066619412155));
#32727=CARTESIAN_POINT('Ctrl Pts',(-48.1426487166498,43.142980929048,-7.17194946048392));
#32728=CARTESIAN_POINT('Ctrl Pts',(-48.7789638602892,44.049616743981,-7.23723697975235));
#32729=CARTESIAN_POINT('Ctrl Pts',(-49.1744877731268,44.6131679161094,-7.27781871875171));
#32730=CARTESIAN_POINT('Ctrl Pts',(-49.3821560205639,45.3085654768932,-7.31840045775107));
#32731=CARTESIAN_POINT('Ctrl Pts',(-49.3858580102862,46.0019288502567,-7.35898219675043));
#32732=CARTESIAN_POINT('Ctrl Pts',(-49.3915783323198,46.002672719373,-7.01601780324957));
#32733=CARTESIAN_POINT('Ctrl Pts',(-49.3837094576552,45.0906692019163,-6.96240837656147));
#32734=CARTESIAN_POINT('Ctrl Pts',(-49.0025711816212,44.1728595157671,-6.90879894987337));
#32735=CARTESIAN_POINT('Ctrl Pts',(-48.3448149181929,43.5447010853554,-6.85518952318527));
#32736=CARTESIAN_POINT('Ctrl Pts',(-47.5437752993149,42.7797067893384,-6.78990200391684));
#32737=CARTESIAN_POINT('Ctrl Pts',(-46.3324763890047,42.4443017621203,-6.72461448464841));
#32738=CARTESIAN_POINT('Ctrl Pts',(-45.2520433961537,42.6883220776615,-6.65932696537998));
#32739=CARTESIAN_POINT('Ctrl Pts',(-44.1716104033028,42.9323423932026,-6.59403944611155));
#32740=CARTESIAN_POINT('Ctrl Pts',(-43.2220433279111,43.7557880515031,-6.52875192684312));
#32741=CARTESIAN_POINT('Ctrl Pts',(-42.827542715153,44.7908003518449,-6.46346440757469));
#32742=CARTESIAN_POINT('Ctrl Pts',(-42.4330421023949,45.8258126521868,-6.39817688830625));
#32743=CARTESIAN_POINT('Ctrl Pts',(-42.5936079522705,47.07239159457,-6.33288936903782));
#32744=CARTESIAN_POINT('Ctrl Pts',(-43.2375107113618,47.9736520318194,-6.26760184976939));
#32745=CARTESIAN_POINT('Ctrl Pts',(-43.881413470453,48.8749124690688,-6.20231433050096));
#32746=CARTESIAN_POINT('Ctrl Pts',(-45.00865313876,49.4308544011843,-6.13702681123253));
#32747=CARTESIAN_POINT('Ctrl Pts',(-46.1156569468521,49.3931214009566,-6.0717392919641));
#32748=CARTESIAN_POINT('Ctrl Pts',(-47.2226607549441,49.3553884007288,-6.00645177269567));
#32749=CARTESIAN_POINT('Ctrl Pts',(-48.3094287028214,48.7239804681578,-5.94116425342724));
#32750=CARTESIAN_POINT('Ctrl Pts',(-48.8904681014242,47.780966999279,-5.8758767341588));
#32751=CARTESIAN_POINT('Ctrl Pts',(-49.2163719794391,47.2520325633926,-5.83925709052239));
#32752=CARTESIAN_POINT('Ctrl Pts',(-49.3831702945945,46.6250649547388,-5.80263744688598));
#32753=CARTESIAN_POINT('Ctrl Pts',(-49.3849262043165,45.9989672045366,-5.76601780324957));
#32754=CARTESIAN_POINT('Origin',(-46.,46.,-5.));
#32755=CARTESIAN_POINT('',(-49.3946329665444,45.9989154325886,-4.51601780324957));
#32756=CARTESIAN_POINT('',(-49.3926797131717,46.0023448477992,-4.85898219675043));
#32757=CARTESIAN_POINT('',(-49.38975,46.,-5.));
#32758=CARTESIAN_POINT('Ctrl Pts',(-49.3926797131717,46.0023448477992,-4.85898219675043));
#32759=CARTESIAN_POINT('Ctrl Pts',(-49.3939355469422,46.1604461186904,-4.86828355986323));
#32760=CARTESIAN_POINT('Ctrl Pts',(-49.3838127180113,46.3183859042746,-4.87758492297603));
#32761=CARTESIAN_POINT('Ctrl Pts',(-49.3617514440163,46.4746401205548,-4.88688628608883));
#32762=CARTESIAN_POINT('Ctrl Pts',(-49.2069003933082,47.571409489996,-4.95217380535726));
#32763=CARTESIAN_POINT('Ctrl Pts',(-48.4638630471224,48.585133809658,-5.0174613246257));
#32764=CARTESIAN_POINT('Ctrl Pts',(-47.4645770771483,49.0629511924481,-5.08274884389413));
#32765=CARTESIAN_POINT('Ctrl Pts',(-46.4652911071743,49.5407685752381,-5.14803636316256));
#32766=CARTESIAN_POINT('Ctrl Pts',(-45.209756513412,49.4826790211562,-5.21332388243099));
#32767=CARTESIAN_POINT('Ctrl Pts',(-44.2588592935263,48.9146329222825,-5.27861140169942));
#32768=CARTESIAN_POINT('Ctrl Pts',(-43.3079620736407,48.3465868234088,-5.34389892096785));
#32769=CARTESIAN_POINT('Ctrl Pts',(-42.6617022276319,47.2685841797434,-5.40918644023628));
#32770=CARTESIAN_POINT('Ctrl Pts',(-42.6087839206706,46.1622019901345,-5.47447395950472));
#32771=CARTESIAN_POINT('Ctrl Pts',(-42.5558656137093,45.0558198005256,-5.53976147877315));
#32772=CARTESIAN_POINT('Ctrl Pts',(-43.0962888457956,43.9210580649734,-5.60504899804157));
#32773=CARTESIAN_POINT('Ctrl Pts',(-43.9886299492523,43.2648498078038,-5.67033651731001));
#32774=CARTESIAN_POINT('Ctrl Pts',(-44.8809710527091,42.6086415506342,-5.73562403657844));
#32775=CARTESIAN_POINT('Ctrl Pts',(-46.1252300275364,42.4309867718473,-5.80091155584687));
#32776=CARTESIAN_POINT('Ctrl Pts',(-47.1655579679665,42.8112493482335,-5.8661990751153));
#32777=CARTESIAN_POINT('Ctrl Pts',(-48.2058859083967,43.1915119246197,-5.93148659438373));
#32778=CARTESIAN_POINT('Ctrl Pts',(-49.0422828144297,44.1296918561791,-5.99677411365216));
#32779=CARTESIAN_POINT('Ctrl Pts',(-49.3011045901178,45.206675233641,-6.06206163292059));
#32780=CARTESIAN_POINT('Ctrl Pts',(-49.3631075772268,45.4646758840569,-6.07770182086387));
#32781=CARTESIAN_POINT('Ctrl Pts',(-49.3919644910817,45.7306422326894,-6.09334200880715));
#32782=CARTESIAN_POINT('Ctrl Pts',(-49.3896329814502,45.9971074077133,-6.10898219675043));
#32783=CARTESIAN_POINT('Ctrl Pts',(-49.3849262043165,45.9989672045366,-5.76601780324957));
#32784=CARTESIAN_POINT('Ctrl Pts',(-49.3863008272383,45.5088233731412,-5.73734992761755));
#32785=CARTESIAN_POINT('Ctrl Pts',(-49.2865272077179,45.0192126450613,-5.70868205198553));
#32786=CARTESIAN_POINT('Ctrl Pts',(-49.0827569539528,44.5775869410516,-5.68001417635351));
#32787=CARTESIAN_POINT('Ctrl Pts',(-48.6186955585504,43.5718393568893,-5.61472665708508));
#32788=CARTESIAN_POINT('Ctrl Pts',(-47.6152619184171,42.814963193751,-5.54943913781665));
#32789=CARTESIAN_POINT('Ctrl Pts',(-46.520720766888,42.6450783584327,-5.48415161854822));
#32790=CARTESIAN_POINT('Ctrl Pts',(-45.4261796153588,42.4751935231143,-5.41886409927979));
#32791=CARTESIAN_POINT('Ctrl Pts',(-44.2405309524337,42.8923000156159,-5.35357658001136));
#32792=CARTESIAN_POINT('Ctrl Pts',(-43.4934405628386,43.7100635119704,-5.28828906074292));
#32793=CARTESIAN_POINT('Ctrl Pts',(-42.7463501732435,44.5278270083248,-5.22300154147449));
#32794=CARTESIAN_POINT('Ctrl Pts',(-42.4378180569783,45.746247508532,-5.15771402220606));
#32795=CARTESIAN_POINT('Ctrl Pts',(-42.7056750188706,46.8210190350401,-5.09242650293763));
#32796=CARTESIAN_POINT('Ctrl Pts',(-42.9735319807628,47.8957905615482,-5.0271389836692));
#32797=CARTESIAN_POINT('Ctrl Pts',(-43.8177780208124,48.8269131143573,-4.96185146440077));
#32798=CARTESIAN_POINT('Ctrl Pts',(-44.8612624194596,49.1984255593208,-4.89656394513234));
#32799=CARTESIAN_POINT('Ctrl Pts',(-45.9047468181068,49.5699380042843,-4.83127642586391));
#32800=CARTESIAN_POINT('Ctrl Pts',(-47.1474695753515,49.3818403414024,-4.76598890659548));
#32801=CARTESIAN_POINT('Ctrl Pts',(-48.0342681461046,48.7181615927584,-4.70070138732704));
#32802=CARTESIAN_POINT('Ctrl Pts',(-48.8704521530768,48.0923627093522,-4.63914019263455));
#32803=CARTESIAN_POINT('Ctrl Pts',(-49.3901816818208,47.0437216307205,-4.57757899794206));
#32804=CARTESIAN_POINT('Ctrl Pts',(-49.3946329665444,45.9989154325886,-4.51601780324957));
#32805=CARTESIAN_POINT('Origin',(-46.,46.,-5.));
#32806=CARTESIAN_POINT('',(-49.3870900307866,46.0025162764443,-3.26601780324957));
#32807=CARTESIAN_POINT('',(-49.3846596848065,45.9995769998069,-3.60898219675043));
#32808=CARTESIAN_POINT('',(-49.38975,46.,-5.));
#32809=CARTESIAN_POINT('Ctrl Pts',(-49.3846596848065,45.9995769998069,-3.60898219675043));
#32810=CARTESIAN_POINT('Ctrl Pts',(-49.3839903779672,46.5851552579925,-3.64322511091931));
#32811=CARTESIAN_POINT('Ctrl Pts',(-49.2392624490329,47.1710433976494,-3.67746802508819));
#32812=CARTESIAN_POINT('Ctrl Pts',(-48.9524293383723,47.6762508813733,-3.71171093925707));
#32813=CARTESIAN_POINT('Ctrl Pts',(-48.4055535045364,48.6394791616974,-3.7769984585255));
#32814=CARTESIAN_POINT('Ctrl Pts',(-47.3421081071184,49.3094234764506,-3.84228597779394));
#32815=CARTESIAN_POINT('Ctrl Pts',(-46.2371669696481,49.386799056601,-3.90757349706237));
#32816=CARTESIAN_POINT('Ctrl Pts',(-45.1322258321778,49.4641746367513,-3.9728610163308));
#32817=CARTESIAN_POINT('Ctrl Pts',(-43.9857889546551,48.9489814822988,-4.03814853559923));
#32818=CARTESIAN_POINT('Ctrl Pts',(-43.3100050145034,48.0713722499747,-4.10343605486766));
#32819=CARTESIAN_POINT('Ctrl Pts',(-42.6342210743516,47.1937630176505,-4.16872357413609));
#32820=CARTESIAN_POINT('Ctrl Pts',(-42.4290900715707,45.9537377074547,-4.23401109340452));
#32821=CARTESIAN_POINT('Ctrl Pts',(-42.786250344801,44.9052538319623,-4.29929861267295));
#32822=CARTESIAN_POINT('Ctrl Pts',(-43.1434106180313,43.8567699564698,-4.36458613194138));
#32823=CARTESIAN_POINT('Ctrl Pts',(-44.0628621672728,42.9998275156808,-4.42987365120982));
#32824=CARTESIAN_POINT('Ctrl Pts',(-45.1338576566721,42.7172491015831,-4.49516117047825));
#32825=CARTESIAN_POINT('Ctrl Pts',(-46.2048531460714,42.4346706874855,-4.56044868974668));
#32826=CARTESIAN_POINT('Ctrl Pts',(-47.4273925756286,42.7264563000792,-4.62573620901511));
#32827=CARTESIAN_POINT('Ctrl Pts',(-48.2553299127918,43.4622563159863,-4.69102372828354));
#32828=CARTESIAN_POINT('Ctrl Pts',(-48.965312916663,44.0932285914148,-4.74700988443917));
#32829=CARTESIAN_POINT('Ctrl Pts',(-49.3851206807237,45.0507120243974,-4.8029960405948));
#32830=CARTESIAN_POINT('Ctrl Pts',(-49.3926797131717,46.0023448477992,-4.85898219675043));
#32831=CARTESIAN_POINT('Ctrl Pts',(-49.3946329665444,45.9989154325886,-4.51601780324957));
#32832=CARTESIAN_POINT('Ctrl Pts',(-49.3949024046497,45.9356728812925,-4.51229147867363));
#32833=CARTESIAN_POINT('Ctrl Pts',(-49.3932838988388,45.8724443807338,-4.50856515409769));
#32834=CARTESIAN_POINT('Ctrl Pts',(-49.3897333541247,45.8093245590373,-4.50483882952175));
#32835=CARTESIAN_POINT('Ctrl Pts',(-49.3275256071303,44.7034261083662,-4.43955131025332));
#32836=CARTESIAN_POINT('Ctrl Pts',(-48.6722357288803,43.63088904143,-4.37426379098489));
#32837=CARTESIAN_POINT('Ctrl Pts',(-47.7166018986786,43.0708487135956,-4.30897627171646));
#32838=CARTESIAN_POINT('Ctrl Pts',(-46.7609680684769,42.5108083857612,-4.24368875244803));
#32839=CARTESIAN_POINT('Ctrl Pts',(-45.5049902863237,42.4632647970286,-4.1784012331796));
#32840=CARTESIAN_POINT('Ctrl Pts',(-44.5097525254705,42.9494571309534,-4.11311371391116));
#32841=CARTESIAN_POINT('Ctrl Pts',(-43.5145147646174,43.4356494648782,-4.04782619464273));
#32842=CARTESIAN_POINT('Ctrl Pts',(-42.7800170250644,44.4555777214603,-3.9825386753743));
#32843=CARTESIAN_POINT('Ctrl Pts',(-42.6343820787504,45.5536085279835,-3.91725115610587));
#32844=CARTESIAN_POINT('Ctrl Pts',(-42.4887471324365,46.6516393345068,-3.85196363683744));
#32845=CARTESIAN_POINT('Ctrl Pts',(-42.9319749793616,47.8277726909711,-3.78667611756901));
#32846=CARTESIAN_POINT('Ctrl Pts',(-43.7660620822644,48.5565935787908,-3.72138859830058));
#32847=CARTESIAN_POINT('Ctrl Pts',(-44.6001491851673,49.2854144666106,-3.65610107903214));
#32848=CARTESIAN_POINT('Ctrl Pts',(-45.8250955440479,49.5669228857858,-3.59081355976371));
#32849=CARTESIAN_POINT('Ctrl Pts',(-46.8936798813232,49.2753603721713,-3.52552604049528));
#32850=CARTESIAN_POINT('Ctrl Pts',(-47.9622642185986,48.9837978585568,-3.46023852122685));
#32851=CARTESIAN_POINT('Ctrl Pts',(-48.8744865342686,48.1191644121527,-3.39495100195842));
#32852=CARTESIAN_POINT('Ctrl Pts',(-49.222829006556,47.0677183924078,-3.32966348268999));
#32853=CARTESIAN_POINT('Ctrl Pts',(-49.3360231441957,46.7260502498519,-3.30844825620985));
#32854=CARTESIAN_POINT('Ctrl Pts',(-49.3896755337205,46.364656012602,-3.28723302972971));
#32855=CARTESIAN_POINT('Ctrl Pts',(-49.3870900307866,46.0025162764443,-3.26601780324957));
#32856=CARTESIAN_POINT('Origin',(-46.,46.,-5.));
#32857=CARTESIAN_POINT('',(-49.387979831519,45.997252452837,-2.01601780324957));
#32858=CARTESIAN_POINT('',(-49.3939446252011,45.9983056787136,-2.35898219675043));
#32859=CARTESIAN_POINT('',(-49.38975,46.,-5.));
#32860=CARTESIAN_POINT('Ctrl Pts',(-49.3939446252011,45.9983056787136,-2.35898219675043));
#32861=CARTESIAN_POINT('Ctrl Pts',(-49.3877070377124,47.0033169214029,-2.41816666197539));
#32862=CARTESIAN_POINT('Ctrl Pts',(-48.9121877502659,48.0134657894478,-2.47735112720035));
#32863=CARTESIAN_POINT('Ctrl Pts',(-48.130361037692,48.6435236993263,-2.53653559242531));
#32864=CARTESIAN_POINT('Ctrl Pts',(-47.2679129887364,49.3385526697674,-2.60182311169374));
#32865=CARTESIAN_POINT('Ctrl Pts',(-46.0327280276914,49.5710596167832,-2.66711063096217));
#32866=CARTESIAN_POINT('Ctrl Pts',(-44.9766012143833,49.2371763964032,-2.7323981502306));
#32867=CARTESIAN_POINT('Ctrl Pts',(-43.9204744010753,48.9032931760232,-2.79768566949903));
#32868=CARTESIAN_POINT('Ctrl Pts',(-43.0434057355042,48.0030197882473,-2.86297318876747));
#32869=CARTESIAN_POINT('Ctrl Pts',(-42.7372088729773,46.9385361561164,-2.9282607080359));
#32870=CARTESIAN_POINT('Ctrl Pts',(-42.4310120104504,45.8740525239854,-2.99354822730433));
#32871=CARTESIAN_POINT('Ctrl Pts',(-42.6956869509677,44.6453586474994,-3.05883574657276));
#32872=CARTESIAN_POINT('Ctrl Pts',(-43.4129952148832,43.8013499086738,-3.12412326584119));
#32873=CARTESIAN_POINT('Ctrl Pts',(-44.1303034787986,42.9573411698482,-3.18941078510962));
#32874=CARTESIAN_POINT('Ctrl Pts',(-45.3002450661123,42.498017568683,-3.25469830437805));
#32875=CARTESIAN_POINT('Ctrl Pts',(-46.4001710363173,42.6285731250573,-3.31998582364648));
#32876=CARTESIAN_POINT('Ctrl Pts',(-47.5000970065224,42.7591286814316,-3.38527334291492));
#32877=CARTESIAN_POINT('Ctrl Pts',(-48.5300073596189,43.4795633953454,-3.45056086218335));
#32878=CARTESIAN_POINT('Ctrl Pts',(-49.0298094010404,44.4680368752498,-3.51584838145178));
#32879=CARTESIAN_POINT('Ctrl Pts',(-49.2674682549491,44.9380619149337,-3.54689298655133));
#32880=CARTESIAN_POINT('Ctrl Pts',(-49.3852664779787,45.4686921081007,-3.57793759165088));
#32881=CARTESIAN_POINT('Ctrl Pts',(-49.3846596848065,45.9995769998069,-3.60898219675043));
#32882=CARTESIAN_POINT('Ctrl Pts',(-49.3870900307866,46.0025162764443,-3.26601780324957));
#32883=CARTESIAN_POINT('Ctrl Pts',(-49.3817189336448,45.2502109217426,-3.22194551046128));
#32884=CARTESIAN_POINT('Ctrl Pts',(-49.1336505161444,44.4946883307728,-3.17787321767299));
#32885=CARTESIAN_POINT('Ctrl Pts',(-48.6725040913107,43.9061109641452,-3.1338009248847));
#32886=CARTESIAN_POINT('Ctrl Pts',(-47.9893740748734,43.0342081487129,-3.06851340561626));
#32887=CARTESIAN_POINT('Ctrl Pts',(-46.838651413094,42.5286611109342,-3.00322588634783));
#32888=CARTESIAN_POINT('Ctrl Pts',(-45.7343993470158,42.6153131154549,-2.9379383670794));
#32889=CARTESIAN_POINT('Ctrl Pts',(-44.6301472809376,42.7019651199757,-2.87265084781097));
#32890=CARTESIAN_POINT('Ctrl Pts',(-43.5723658105607,43.3808161667959,-2.80736332854254));
#32891=CARTESIAN_POINT('Ctrl Pts',(-43.0335985662276,44.3486029319831,-2.74207580927411));
#32892=CARTESIAN_POINT('Ctrl Pts',(-42.4948313218946,45.3163896971703,-2.67678829000568));
#32893=CARTESIAN_POINT('Ctrl Pts',(-42.4750783036054,46.5731121807244,-2.61150077073725));
#32894=CARTESIAN_POINT('Ctrl Pts',(-42.9831636791679,47.5573530024191,-2.54621325146882));
#32895=CARTESIAN_POINT('Ctrl Pts',(-43.4912490547304,48.5415938241138,-2.48092573220038));
#32896=CARTESIAN_POINT('Ctrl Pts',(-44.5271728241445,49.2533529839491,-2.41563821293195));
#32897=CARTESIAN_POINT('Ctrl Pts',(-45.6281561545019,49.3746672174706,-2.35035069366352));
#32898=CARTESIAN_POINT('Ctrl Pts',(-46.7291394848593,49.4959814509922,-2.28506317439509));
#32899=CARTESIAN_POINT('Ctrl Pts',(-47.89518237616,49.0268507581999,-2.21977565512666));
#32900=CARTESIAN_POINT('Ctrl Pts',(-48.6053770650879,48.1768472445751,-2.15448813585823));
#32901=CARTESIAN_POINT('Ctrl Pts',(-49.1074684086029,47.5759142711215,-2.10833135832201));
#32902=CARTESIAN_POINT('Ctrl Pts',(-49.3817192789863,46.7846147606282,-2.06217458078579));
#32903=CARTESIAN_POINT('Ctrl Pts',(-49.387979831519,45.997252452837,-2.01601780324957));
#32904=CARTESIAN_POINT('Origin',(-46.,46.,-5.));
#32905=CARTESIAN_POINT('',(-49.3940292623548,46.0015451960205,-0.766017803249567));
#32906=CARTESIAN_POINT('',(-49.3881106776293,46.0027671006797,-1.10898219675043));
#32907=CARTESIAN_POINT('',(-49.38975,46.,-5.));
#32908=CARTESIAN_POINT('',(-43.4267655729853,48.2065515280923,0.));
#32909=CARTESIAN_POINT('Ctrl Pts',(-49.3940292623548,46.0015451960205,-0.766017803249567));
#32910=CARTESIAN_POINT('Ctrl Pts',(-49.3879984452729,44.9918196666451,-0.706541093305005));
#32911=CARTESIAN_POINT('Ctrl Pts',(-48.9072367960306,43.9773046953768,-0.647064383360443));
#32912=CARTESIAN_POINT('Ctrl Pts',(-48.1187303416659,43.3473617203725,-0.58758767341588));
#32913=CARTESIAN_POINT('Ctrl Pts',(-47.2531876715922,42.6558740076704,-0.522300154147449));
#32914=CARTESIAN_POINT('Ctrl Pts',(-46.0168300891286,42.4277735844645,-0.457012634879018));
#32915=CARTESIAN_POINT('Ctrl Pts',(-44.962273444483,42.7668602707044,-0.391725115610587));
#32916=CARTESIAN_POINT('Ctrl Pts',(-43.9077167998373,43.1059469569444,-0.326437596342156));
#32917=CARTESIAN_POINT('Ctrl Pts',(-43.0349610930096,44.0122207526302,-0.261150077073725));
#32918=CARTESIAN_POINT('Ctrl Pts',(-42.7336918051393,45.0762567531889,-0.195862557805293));
#32919=CARTESIAN_POINT('Ctrl Pts',(-42.4324225172691,46.1402927537476,-0.130575038536862));
#32920=CARTESIAN_POINT('Ctrl Pts',(-42.7026396483563,47.3620909591791,-0.0652875192684313));
#32921=CARTESIAN_POINT('Ctrl Pts',(-43.4267655729853,48.2065515280923,0.));
#32922=CARTESIAN_POINT('',(-48.5780060810925,48.2094945163745,-2.82133879660966E-15));
#32923=CARTESIAN_POINT('Origin',(-46.,46.,0.));
#32924=CARTESIAN_POINT('Ctrl Pts',(-48.5780352480409,48.2095125055216,-1.80411241501588E-15));
#32925=CARTESIAN_POINT('Ctrl Pts',(-47.8896986135138,49.0067166723596,-0.0620616329205985));
#32926=CARTESIAN_POINT('Ctrl Pts',(-46.7993632977221,49.4635756417559,-0.124123265841195));
#32927=CARTESIAN_POINT('Ctrl Pts',(-45.7491449739559,49.3856448917061,-0.186184898761792));
#32928=CARTESIAN_POINT('Ctrl Pts',(-44.644337610336,49.3036633983736,-0.251472418030223));
#32929=CARTESIAN_POINT('Ctrl Pts',(-43.58392608898,48.6298518891241,-0.316759937298654));
#32930=CARTESIAN_POINT('Ctrl Pts',(-43.0409887593006,47.6645436361188,-0.382047456567084));
#32931=CARTESIAN_POINT('Ctrl Pts',(-42.4980514296212,46.6992353831134,-0.447334975835515));
#32932=CARTESIAN_POINT('Ctrl Pts',(-42.4725882916183,45.4424303863521,-0.512622495103946));
#32933=CARTESIAN_POINT('Ctrl Pts',(-42.9762875061872,44.4559130885416,-0.577910014372377));
#32934=CARTESIAN_POINT('Ctrl Pts',(-43.4799867207561,43.4693957907312,-0.643197533640808));
#32935=CARTESIAN_POINT('Ctrl Pts',(-44.5128482878968,42.7531661918715,-0.708485052909239));
#32936=CARTESIAN_POINT('Ctrl Pts',(-45.6133080412482,42.6270242787203,-0.773772572177669));
#32937=CARTESIAN_POINT('Ctrl Pts',(-46.7137677945997,42.5008823655691,-0.8390600914461));
#32938=CARTESIAN_POINT('Ctrl Pts',(-47.881825734162,42.9648281381265,-0.904347610714531));
#32939=CARTESIAN_POINT('Ctrl Pts',(-48.5957492659174,43.8116818846328,-0.969635129982962));
#32940=CARTESIAN_POINT('Ctrl Pts',(-49.1036725319113,44.414178793072,-1.01608415223878));
#32941=CARTESIAN_POINT('Ctrl Pts',(-49.3817284808321,45.210490631947,-1.06253317449461));
#32942=CARTESIAN_POINT('Ctrl Pts',(-49.3881106776293,46.0027671006797,-1.10898219675043));
#32943=CARTESIAN_POINT('Origin',(-46.,46.,2.76038497140452));
#32944=CARTESIAN_POINT('',(-50.0803097491022,46.0023244644292,-7.76038497140452));
#32945=CARTESIAN_POINT('',(-50.0862705133486,45.9966118456437,-7.86461502859548));
#32946=CARTESIAN_POINT('',(-50.085,46.,2.76038497140452));
#32947=CARTESIAN_POINT('',(-49.4256147683784,43.7746037524369,-9.));
#32948=CARTESIAN_POINT('Ctrl Pts',(-50.0862705133486,45.9966118456437,-7.86461502859549));
#32949=CARTESIAN_POINT('Ctrl Pts',(-50.0769059571497,47.0638214653661,-7.91663908938817));
#32950=CARTESIAN_POINT('Ctrl Pts',(-49.1080148673377,49.4855109457225,-8.03395066944928));
#32951=CARTESIAN_POINT('Ctrl Pts',(-45.0527729214423,50.7128987412233,-8.21654976877883));
#32952=CARTESIAN_POINT('Ctrl Pts',(-41.5512846772643,47.8195936610183,-8.41241232658412));
#32953=CARTESIAN_POINT('Ctrl Pts',(-42.0204412135141,43.2986191788456,-8.60827488438942));
#32954=CARTESIAN_POINT('Ctrl Pts',(-46.0536470456105,41.195226046819,-8.80413744219471));
#32955=CARTESIAN_POINT('Ctrl Pts',(-48.6953045558515,42.6504167892078,-8.93471248073157));
#32956=CARTESIAN_POINT('Ctrl Pts',(-49.4256147683784,43.7746037524369,-9.));
#32957=CARTESIAN_POINT('',(-50.0861552640897,45.7875587543876,-9.));
#32958=CARTESIAN_POINT('Origin',(-46.,46.,-9.));
#32959=CARTESIAN_POINT('Ctrl Pts',(-50.0803097491022,46.0023244644292,-7.76038497140452));
#32960=CARTESIAN_POINT('Ctrl Pts',(-50.0830257350667,46.5110144748489,-7.78509075167359));
#32961=CARTESIAN_POINT('Ctrl Pts',(-49.7610778975337,48.3606597045947,-7.8750840512111));
#32962=CARTESIAN_POINT('Ctrl Pts',(-47.0195850264259,50.6979235414129,-8.03036487001704));
#32963=CARTESIAN_POINT('Ctrl Pts',(-42.6509144693004,49.448562948282,-8.22622742782232));
#32964=CARTESIAN_POINT('Ctrl Pts',(-41.274000700432,45.1181262021708,-8.42208998562762));
#32965=CARTESIAN_POINT('Ctrl Pts',(-44.1206543946181,41.5754411548869,-8.61795254343291));
#32966=CARTESIAN_POINT('Ctrl Pts',(-48.5697422531351,41.9795081408631,-8.81058921489038));
#32967=CARTESIAN_POINT('Ctrl Pts',(-50.0156456694632,44.5202463146725,-8.9379383670794));
#32968=CARTESIAN_POINT('Ctrl Pts',(-50.0861963379778,45.7875630405758,-9.));
#32969=CARTESIAN_POINT('Origin',(-46.,46.,2.76038497140452));
#32970=CARTESIAN_POINT('',(-50.0848589805219,45.9965141265607,-6.51038497140452));
#32971=CARTESIAN_POINT('',(-50.0872033298994,46.003220903795,-6.61461502859548));
#32972=CARTESIAN_POINT('',(-50.085,46.,2.76038497140452));
#32973=CARTESIAN_POINT('Ctrl Pts',(-50.0872033298994,46.003220903795,-6.61461502859548));
#32974=CARTESIAN_POINT('Ctrl Pts',(-50.0892690323773,46.2426360687525,-6.62629312117581));
#32975=CARTESIAN_POINT('Ctrl Pts',(-49.9622030080971,47.8183368728873,-6.70325873302458));
#32976=CARTESIAN_POINT('Ctrl Pts',(-47.9170389384488,50.4085208617021,-6.84551186414178));
#32977=CARTESIAN_POINT('Ctrl Pts',(-43.3883214271118,50.0359894114731,-7.04137442194707));
#32978=CARTESIAN_POINT('Ctrl Pts',(-41.1930659955112,46.0574693216547,-7.23723697975236));
#32979=CARTESIAN_POINT('Ctrl Pts',(-43.2925654154187,42.0275760136403,-7.43309953755766));
#32980=CARTESIAN_POINT('Ctrl Pts',(-47.8111685874939,41.5469454131034,-7.62896209536294));
#32981=CARTESIAN_POINT('Ctrl Pts',(-49.9410013296604,44.1157441623102,-7.77280059237556));
#32982=CARTESIAN_POINT('Ctrl Pts',(-50.0886579933029,45.7245283085182,-7.85135157011974));
#32983=CARTESIAN_POINT('Ctrl Pts',(-50.0862705133486,45.9966118456437,-7.86461502859549));
#32984=CARTESIAN_POINT('Ctrl Pts',(-50.0848589805219,45.9965141265607,-6.51038497140452));
#32985=CARTESIAN_POINT('Ctrl Pts',(-50.0759399931959,47.0158534793692,-6.56003230272967));
#32986=CARTESIAN_POINT('Ctrl Pts',(-49.1785307017076,49.3896732222161,-6.67496715332326));
#32987=CARTESIAN_POINT('Ctrl Pts',(-45.2228146507001,50.7440556643996,-6.85518952318527));
#32988=CARTESIAN_POINT('Ctrl Pts',(-41.6181995750799,47.9773428774946,-7.05105208099057));
#32989=CARTESIAN_POINT('Ctrl Pts',(-41.9285478600743,43.4439512443748,-7.24691463879586));
#32990=CARTESIAN_POINT('Ctrl Pts',(-45.8765970139655,41.1942887704259,-7.44277719660115));
#32991=CARTESIAN_POINT('Ctrl Pts',(-49.4229679546423,42.9805151113374,-7.61393397413737));
#32992=CARTESIAN_POINT('Ctrl Pts',(-50.0758484678822,45.1667497523738,-7.71980323240516));
#32993=CARTESIAN_POINT('Ctrl Pts',(-50.0803097491022,46.0023244644292,-7.76038497140452));
#32994=CARTESIAN_POINT('Origin',(-46.,46.,2.76038497140452));
#32995=CARTESIAN_POINT('',(-50.0885306079523,46.002825784574,-5.26038497140452));
#32996=CARTESIAN_POINT('',(-50.0791868263538,45.9987553744471,-5.36461502859548));
#32997=CARTESIAN_POINT('',(-50.085,46.,2.76038497140452));
#32998=CARTESIAN_POINT('Ctrl Pts',(-50.0791868263538,45.9987553744471,-5.36461502859548));
#32999=CARTESIAN_POINT('Ctrl Pts',(-50.0770707731893,46.7532680404479,-5.40123467223189));
#33000=CARTESIAN_POINT('Ctrl Pts',(-49.5176911419739,48.8558846609211,-5.50314183513674));
#33001=CARTESIAN_POINT('Ctrl Pts',(-46.1637649138928,50.8045026982905,-5.67033651731001));
#33002=CARTESIAN_POINT('Ctrl Pts',(-42.0884430951448,48.7945997915639,-5.86619907511531));
#33003=CARTESIAN_POINT('Ctrl Pts',(-41.507947633761,44.2878293987898,-6.0620616329206));
#33004=CARTESIAN_POINT('Ctrl Pts',(-44.940927797173,41.3108173647246,-6.25792419072589));
#33005=CARTESIAN_POINT('Ctrl Pts',(-49.0590435380633,42.4511112347217,-6.44210865595086));
#33006=CARTESIAN_POINT('Ctrl Pts',(-50.0777205205462,44.9041621623507,-6.56100560190738));
#33007=CARTESIAN_POINT('Ctrl Pts',(-50.0872033298994,46.003220903795,-6.61461502859548));
#33008=CARTESIAN_POINT('Ctrl Pts',(-50.0885306079524,46.002825784574,-5.26038497140452));
#33009=CARTESIAN_POINT('Ctrl Pts',(-50.0900440177768,46.1933541986431,-5.26968633451732));
#33010=CARTESIAN_POINT('Ctrl Pts',(-49.9922181317767,47.7196666123893,-5.34427521689856));
#33011=CARTESIAN_POINT('Ctrl Pts',(-48.0737732836718,50.3369969638681,-5.48415161854822));
#33012=CARTESIAN_POINT('Ctrl Pts',(-43.5346254271756,50.1269851679324,-5.68001417635351));
#33013=CARTESIAN_POINT('Ctrl Pts',(-41.19819518517,46.2296704992633,-5.87587673415881));
#33014=CARTESIAN_POINT('Ctrl Pts',(-43.1519931670912,42.1271540690863,-6.07173929196409));
#33015=CARTESIAN_POINT('Ctrl Pts',(-47.650376155957,41.4848768173615,-6.2676018497694));
#33016=CARTESIAN_POINT('Ctrl Pts',(-49.9077279341632,44.0169308236675,-6.41381707624953));
#33017=CARTESIAN_POINT('Ctrl Pts',(-50.0876686912218,45.6753959792127,-6.49474478346124));
#33018=CARTESIAN_POINT('Ctrl Pts',(-50.0848589805219,45.9965141265607,-6.51038497140452));
#33019=CARTESIAN_POINT('Origin',(-46.,46.,2.76038497140452));
#33020=CARTESIAN_POINT('',(-50.0788656427272,45.9994902409355,-4.01038497140452));
#33021=CARTESIAN_POINT('',(-50.0908844806649,45.9986929838851,-4.11461502859548));
#33022=CARTESIAN_POINT('',(-50.085,46.,2.76038497140452));
#33023=CARTESIAN_POINT('Ctrl Pts',(-50.0908844806649,45.9986929838851,-4.11461502859548));
#33024=CARTESIAN_POINT('Ctrl Pts',(-50.0855202213255,47.2577927167175,-4.17617622328797));
#33025=CARTESIAN_POINT('Ctrl Pts',(-48.7949524579669,49.8617286036896,-4.3030249372489));
#33026=CARTESIAN_POINT('Ctrl Pts',(-44.3876003506517,50.5288223911423,-4.49516117047825));
#33027=CARTESIAN_POINT('Ctrl Pts',(-41.3353884704811,47.1625249105979,-4.69102372828355));
#33028=CARTESIAN_POINT('Ctrl Pts',(-42.4508279821942,42.7575560397258,-4.88688628608884));
#33029=CARTESIAN_POINT('Ctrl Pts',(-46.7373164737192,41.2495864060927,-5.08274884389414));
#33030=CARTESIAN_POINT('Ctrl Pts',(-49.6867797812653,43.4743259227351,-5.24199175806301));
#33031=CARTESIAN_POINT('Ctrl Pts',(-50.0808433894147,45.4080812683183,-5.33594715296346));
#33032=CARTESIAN_POINT('Ctrl Pts',(-50.0791868263538,45.9987553744471,-5.36461502859548));
#33033=CARTESIAN_POINT('Ctrl Pts',(-50.0788656427272,45.9994902409355,-4.01038497140452));
#33034=CARTESIAN_POINT('Ctrl Pts',(-50.0780590586315,46.7051727203774,-4.0446278855734));
#33035=CARTESIAN_POINT('Ctrl Pts',(-49.5711128061907,48.7573944230954,-4.14415831901071));
#33036=CARTESIAN_POINT('Ctrl Pts',(-46.3358174405565,50.7955505353102,-4.30897627171646));
#33037=CARTESIAN_POINT('Ctrl Pts',(-42.1910917427793,48.9329671271487,-4.50483882952175));
#33038=CARTESIAN_POINT('Ctrl Pts',(-41.4494793999576,44.4498901520179,-4.70070138732704));
#33039=CARTESIAN_POINT('Ctrl Pts',(-44.7735825745146,41.351776836325,-4.89656394513234));
#33040=CARTESIAN_POINT('Ctrl Pts',(-48.9835468796149,42.3565763414064,-5.08312513982483));
#33041=CARTESIAN_POINT('Ctrl Pts',(-50.0794211905764,44.8560096230292,-5.20439881524889));
#33042=CARTESIAN_POINT('Ctrl Pts',(-50.0885306079524,46.002825784574,-5.26038497140452));
#33043=CARTESIAN_POINT('Origin',(-46.,46.,2.76038497140452));
#33044=CARTESIAN_POINT('',(-50.0900549580195,45.9979581672823,-2.76038497140452));
#33045=CARTESIAN_POINT('',(-50.0817944614686,46.0030323738549,-2.86461502859548));
#33046=CARTESIAN_POINT('',(-50.085,46.,2.76038497140452));
#33047=CARTESIAN_POINT('Ctrl Pts',(-50.0817944614686,46.0030323738549,-2.86461502859548));
#33048=CARTESIAN_POINT('Ctrl Pts',(-50.0849102604169,46.439448281283,-2.88583025507562));
#33049=CARTESIAN_POINT('Ctrl Pts',(-49.8212797436113,48.2152228624484,-2.97233300082419));
#33050=CARTESIAN_POINT('Ctrl Pts',(-47.2654092996424,50.6377585015902,-3.1241232658412));
#33051=CARTESIAN_POINT('Ctrl Pts',(-42.8368474210137,49.6200180555421,-3.31998582364649));
#33052=CARTESIAN_POINT('Ctrl Pts',(-41.2344409709606,45.3679303548353,-3.51584838145178));
#33053=CARTESIAN_POINT('Ctrl Pts',(-43.8898786280806,41.6805726486878,-3.71171093925708));
#33054=CARTESIAN_POINT('Ctrl Pts',(-48.430628748381,41.8524575015287,-3.90757349706237));
#33055=CARTESIAN_POINT('Ctrl Pts',(-50.0550853181707,44.5112653704681,-4.04187486017517));
#33056=CARTESIAN_POINT('Ctrl Pts',(-50.0912091815013,45.9224791563035,-4.11088870401954));
#33057=CARTESIAN_POINT('Ctrl Pts',(-50.0908844806649,45.9986929838851,-4.11461502859548));
#33058=CARTESIAN_POINT('Ctrl Pts',(-50.0900549580195,45.9979581672823,-2.76038497140452));
#33059=CARTESIAN_POINT('Ctrl Pts',(-50.0825380187493,47.2091008552049,-2.81956943662948));
#33060=CARTESIAN_POINT('Ctrl Pts',(-48.87734553552,49.7692994735359,-2.94404142112287));
#33061=CARTESIAN_POINT('Ctrl Pts',(-44.5509147952652,50.5836918395513,-3.13380092488469));
#33062=CARTESIAN_POINT('Ctrl Pts',(-41.380038920474,47.3289236804855,-3.32966348268999));
#33063=CARTESIAN_POINT('Ctrl Pts',(-42.3369211082577,42.8868133607463,-3.52552604049528));
#33064=CARTESIAN_POINT('Ctrl Pts',(-46.5666236386886,41.2262157555308,-3.72138859830058));
#33065=CARTESIAN_POINT('Ctrl Pts',(-49.6390946438884,43.3754462812598,-3.88300824193699));
#33066=CARTESIAN_POINT('Ctrl Pts',(-50.0795968913763,45.3597189354941,-3.97934036630497));
#33067=CARTESIAN_POINT('Ctrl Pts',(-50.0788656427272,45.9994902409355,-4.01038497140452));
#33068=CARTESIAN_POINT('Origin',(-46.,46.,2.76038497140452));
#33069=CARTESIAN_POINT('',(-50.0830244466748,46.0033346430494,-1.51038497140452));
#33070=CARTESIAN_POINT('',(-50.0828667635534,45.9966889209644,-1.61461502859548));
#33071=CARTESIAN_POINT('',(-50.085,46.,2.76038497140452));
#33072=CARTESIAN_POINT('Ctrl Pts',(-50.0828667635534,45.9966889209644,-1.61461502859548));
#33073=CARTESIAN_POINT('Ctrl Pts',(-50.0753221490254,46.9455420892886,-1.6607718061317));
#33074=CARTESIAN_POINT('Ctrl Pts',(-49.2773370649769,49.24797856107,-1.77221610293635));
#33075=CARTESIAN_POINT('Ctrl Pts',(-45.4734861227781,50.7783710029823,-1.94894791900944));
#33076=CARTESIAN_POINT('Ctrl Pts',(-41.7282996653196,48.2051403801394,-2.14481047681473));
#33077=CARTESIAN_POINT('Ctrl Pts',(-41.7997129669298,43.6616979327745,-2.34067303462002));
#33078=CARTESIAN_POINT('Ctrl Pts',(-45.6239218081334,41.2074403684165,-2.53653559242531));
#33079=CARTESIAN_POINT('Ctrl Pts',(-49.3335197698138,42.8371782046192,-2.71118292375047));
#33080=CARTESIAN_POINT('Ctrl Pts',(-50.0753217328532,45.0964264666476,-2.82054273580719));
#33081=CARTESIAN_POINT('Ctrl Pts',(-50.0817944614686,46.0030323738549,-2.86461502859548));
#33082=CARTESIAN_POINT('Ctrl Pts',(-50.0830244466748,46.0033346430494,-1.51038497140452));
#33083=CARTESIAN_POINT('Ctrl Pts',(-50.0861437977564,46.390566271631,-1.52922346841713));
#33084=CARTESIAN_POINT('Ctrl Pts',(-49.859584554975,48.116232607913,-1.61334948469817));
#33085=CARTESIAN_POINT('Ctrl Pts',(-47.4307681707597,50.5894263088653,-1.76276302024764));
#33086=CARTESIAN_POINT('Ctrl Pts',(-42.968598137007,49.7310442859955,-1.95862557805294));
#33087=CARTESIAN_POINT('Ctrl Pts',(-41.2148485187469,45.539095378305,-2.15448813585823));
#33088=CARTESIAN_POINT('Ctrl Pts',(-43.7364582880855,41.758957824139,-2.35035069366352));
#33089=CARTESIAN_POINT('Ctrl Pts',(-48.2804507290339,41.7680234302945,-2.54621325146882));
#33090=CARTESIAN_POINT('Ctrl Pts',(-50.0295527394747,44.4129094467295,-2.68289134404915));
#33091=CARTESIAN_POINT('Ctrl Pts',(-50.0908300986993,45.8730661157845,-2.75428191736105));
#33092=CARTESIAN_POINT('Ctrl Pts',(-50.0900549580195,45.9979581672823,-2.76038497140452));
#33093=CARTESIAN_POINT('Origin',(-46.,46.,2.76038497140452));
#33094=CARTESIAN_POINT('',(-50.0805800719598,45.9961676961768,-0.260384971404518));
#33095=CARTESIAN_POINT('',(-50.0901569545599,46.0018621213198,-0.364615028595478));
#33096=CARTESIAN_POINT('',(-50.085,46.,2.76038497140452));
#33097=CARTESIAN_POINT('',(-47.057904422973,42.0543614925016,0.));
#33098=CARTESIAN_POINT('Ctrl Pts',(-47.0579044229729,42.0543614925016,5.55111512312578E-16));
#33099=CARTESIAN_POINT('Ctrl Pts',(-48.3527480267224,42.4015349025495,-0.0652875192684306));
#33100=CARTESIAN_POINT('Ctrl Pts',(-49.8153062247254,43.7726401555849,-0.152082509736603));
#33101=CARTESIAN_POINT('Ctrl Pts',(-50.0835487927699,45.5536944557427,-0.238877500204777));
#33102=CARTESIAN_POINT('Ctrl Pts',(-50.0805800719598,45.9961676961768,-0.260384971404518));
#33103=CARTESIAN_POINT('',(-44.9393528874294,42.0481879703258,-3.26985762221281E-15));
#33104=CARTESIAN_POINT('Origin',(-46.,46.,0.));
#33105=CARTESIAN_POINT('Ctrl Pts',(-44.9393361356002,42.0481502636203,8.02309607639273E-17));
#33106=CARTESIAN_POINT('Ctrl Pts',(-46.1664281570359,41.7236247110316,-0.0620616329205977));
#33107=CARTESIAN_POINT('Ctrl Pts',(-48.8989740353372,42.2867115510563,-0.183599975785758));
#33108=CARTESIAN_POINT('Ctrl Pts',(-50.0828891950556,44.7850382294403,-0.305138318650917));
#33109=CARTESIAN_POINT('Ctrl Pts',(-50.0901569545599,46.0018621213198,-0.364615028595479));
#33110=CARTESIAN_POINT('Origin',(46.,46.,-5.));
#33111=CARTESIAN_POINT('',(42.6091954699811,45.9971884981445,-8.26601780324957));
#33112=CARTESIAN_POINT('',(42.6044122534151,45.9998426503687,-8.60898219675043));
#33113=CARTESIAN_POINT('',(42.61025,46.,-5.));
#33114=CARTESIAN_POINT('',(47.303382040875,49.1291532909119,-9.));
#33115=CARTESIAN_POINT('Ctrl Pts',(42.6044122534151,45.9998426503687,-8.60898219675043));
#33116=CARTESIAN_POINT('Ctrl Pts',(42.6053213723518,47.1035783352378,-8.67403394523186));
#33117=CARTESIAN_POINT('Ctrl Pts',(43.1965773203909,48.2078791190907,-8.73908569371329));
#33118=CARTESIAN_POINT('Ctrl Pts',(44.1121203927824,48.8209865441,-8.80413744219471));
#33119=CARTESIAN_POINT('Ctrl Pts',(45.0309817204976,49.4363160895516,-8.86942496146314));
#33120=CARTESIAN_POINT('Ctrl Pts',(46.276485097278,49.5568853032748,-8.93471248073157));
#33121=CARTESIAN_POINT('Ctrl Pts',(47.303382040875,49.1291532909119,-9.));
#33122=CARTESIAN_POINT('',(42.61025,46.,-9.));
#33123=CARTESIAN_POINT('Origin',(46.,46.,-9.));
#33124=CARTESIAN_POINT('',(42.61025,46.,-10.));
#33125=CARTESIAN_POINT('',(42.61025,46.,-5.));
#33126=CARTESIAN_POINT('Origin',(46.,46.,-10.));
#33127=CARTESIAN_POINT('',(48.898001656697,44.2309423651523,-9.));
#33128=CARTESIAN_POINT('Origin',(46.,46.,-9.));
#33129=CARTESIAN_POINT('Ctrl Pts',(48.8980277622168,44.2309202005125,-9.));
#33130=CARTESIAN_POINT('Ctrl Pts',(49.4435068986972,45.1319172328957,-8.9379383670794));
#33131=CARTESIAN_POINT('Ctrl Pts',(49.5410720297735,46.3100640638366,-8.8758767341588));
#33132=CARTESIAN_POINT('Ctrl Pts',(49.1424199628038,47.2847987174335,-8.81381510123821));
#33133=CARTESIAN_POINT('Ctrl Pts',(48.7230464581302,48.3101988637643,-8.74852758196978));
#33134=CARTESIAN_POINT('Ctrl Pts',(47.7545295770243,49.1104910325523,-8.68324006270134));
#33135=CARTESIAN_POINT('Ctrl Pts',(46.6686904456162,49.3285585007771,-8.61795254343291));
#33136=CARTESIAN_POINT('Ctrl Pts',(45.5828513142082,49.5466259690018,-8.55266502416448));
#33137=CARTESIAN_POINT('Ctrl Pts',(44.3796899324978,49.1824687366633,-8.48737750489605));
#33138=CARTESIAN_POINT('Ctrl Pts',(43.5971079012266,48.3985718445634,-8.42208998562762));
#33139=CARTESIAN_POINT('Ctrl Pts',(42.9735109928692,47.7739271953753,-8.37006592483494));
#33140=CARTESIAN_POINT('Ctrl Pts',(42.6169662530301,46.882763549866,-8.31804186404225));
#33141=CARTESIAN_POINT('Ctrl Pts',(42.6091954699811,45.9971884981445,-8.26601780324957));
#33142=CARTESIAN_POINT('Origin',(46.,46.,-5.));
#33143=CARTESIAN_POINT('',(42.6084214217016,46.0026727196953,-7.01601780324957));
#33144=CARTESIAN_POINT('',(42.6141421045691,46.0019288481038,-7.35898219675043));
#33145=CARTESIAN_POINT('',(42.61025,46.,-5.));
#33146=CARTESIAN_POINT('Ctrl Pts',(42.6141421045691,46.0019288481038,-7.35898219675043));
#33147=CARTESIAN_POINT('Ctrl Pts',(42.6118883673488,46.4240419205118,-7.38368797701951));
#33148=CARTESIAN_POINT('Ctrl Pts',(42.6852298192571,46.8454010706231,-7.40839375728858));
#33149=CARTESIAN_POINT('Ctrl Pts',(42.8378015517891,47.2357983442509,-7.43309953755765));
#33150=CARTESIAN_POINT('Ctrl Pts',(43.2409877624255,48.267462563989,-7.49838705682608));
#33151=CARTESIAN_POINT('Ctrl Pts',(44.1974659581544,49.0829094742983,-7.56367457609451));
#33152=CARTESIAN_POINT('Ctrl Pts',(45.2798951927721,49.3178454913476,-7.62896209536294));
#33153=CARTESIAN_POINT('Ctrl Pts',(46.3623244273898,49.5527815083968,-7.69424961463137));
#33154=CARTESIAN_POINT('Ctrl Pts',(47.5707047008963,49.207206632186,-7.75953713389981));
#33155=CARTESIAN_POINT('Ctrl Pts',(48.3653229781552,48.4355168243605,-7.82482465316824));
#33156=CARTESIAN_POINT('Ctrl Pts',(49.1599412554142,47.663827016535,-7.89011217243667));
#33157=CARTESIAN_POINT('Ctrl Pts',(49.5407975364256,46.4660222770948,-7.9553996917051));
#33158=CARTESIAN_POINT('Ctrl Pts',(49.3375314802461,45.3771640957291,-8.02068721097353));
#33159=CARTESIAN_POINT('Ctrl Pts',(49.1342654240667,44.2883059143633,-8.08597473024196));
#33160=CARTESIAN_POINT('Ctrl Pts',(48.3468770306965,43.308394291072,-8.15126224951039));
#33161=CARTESIAN_POINT('Ctrl Pts',(47.3275669774877,42.8752570908402,-8.21654976877882));
#33162=CARTESIAN_POINT('Ctrl Pts',(46.308256924279,42.4421198906085,-8.28183728804726));
#33163=CARTESIAN_POINT('Ctrl Pts',(45.0570252112318,42.5557571134363,-8.34712480731569));
#33164=CARTESIAN_POINT('Ctrl Pts',(44.1319138563052,43.1652562095208,-8.41241232658412));
#33165=CARTESIAN_POINT('Ctrl Pts',(43.2068025013787,43.7747553056054,-8.47769984585255));
#33166=CARTESIAN_POINT('Ctrl Pts',(42.6078115045729,44.8801162749467,-8.54298736512098));
#33167=CARTESIAN_POINT('Ctrl Pts',(42.604425645495,45.9878416982074,-8.60827488438941));
#33168=CARTESIAN_POINT('Ctrl Pts',(42.6044134182475,45.9918419925632,-8.60851065517642));
#33169=CARTESIAN_POINT('Ctrl Pts',(42.6044089584431,45.9958423177544,-8.60874642596342));
#33170=CARTESIAN_POINT('Ctrl Pts',(42.6044122534151,45.9998426503687,-8.60898219675043));
#33171=CARTESIAN_POINT('Ctrl Pts',(42.6091954699811,45.9971884981445,-8.26601780324957));
#33172=CARTESIAN_POINT('Ctrl Pts',(42.6072143201684,45.7714124294044,-8.25275434477382));
#33173=CARTESIAN_POINT('Ctrl Pts',(42.6279030448371,45.545999612327,-8.23949088629807));
#33174=CARTESIAN_POINT('Ctrl Pts',(42.672615883441,45.3254592340216,-8.22622742782233));
#33175=CARTESIAN_POINT('Ctrl Pts',(42.8927085777588,44.2398800674407,-8.1609399085539));
#33176=CARTESIAN_POINT('Ctrl Pts',(43.6948966472266,43.2723582861398,-8.09565238928547));
#33177=CARTESIAN_POINT('Ctrl Pts',(44.7209166654019,42.8550689459674,-8.03036487001703));
#33178=CARTESIAN_POINT('Ctrl Pts',(45.7469366835771,42.437779605795,-7.9650773507486));
#33179=CARTESIAN_POINT('Ctrl Pts',(46.9967886504598,42.570722706751,-7.89978983148017));
#33180=CARTESIAN_POINT('Ctrl Pts',(47.9120768886828,43.1945313366717,-7.83450231221174));
#33181=CARTESIAN_POINT('Ctrl Pts',(48.8273651269058,43.8183399665924,-7.76921479294331));
#33182=CARTESIAN_POINT('Ctrl Pts',(49.4080896364691,44.9330141254778,-7.70392727367488));
#33183=CARTESIAN_POINT('Ctrl Pts',(49.3948465163211,46.0405833329933,-7.63863975440645));
#33184=CARTESIAN_POINT('Ctrl Pts',(49.3816033961731,47.1481525405088,-7.57335223513802));
#33185=CARTESIAN_POINT('Ctrl Pts',(48.7743926463139,48.2486167966545,-7.50806471586959));
#33186=CARTESIAN_POINT('Ctrl Pts',(47.8444624554029,48.8503702861328,-7.44277719660115));
#33187=CARTESIAN_POINT('Ctrl Pts',(46.9145322644919,49.4521237756111,-7.37748967733272));
#33188=CARTESIAN_POINT('Ctrl Pts',(45.6618826325292,49.555166498422,-7.31220215806428));
#33189=CARTESIAN_POINT('Ctrl Pts',(44.6461164034007,49.1134634166091,-7.24691463879585));
#33190=CARTESIAN_POINT('Ctrl Pts',(43.6303501742723,48.6717603347961,-7.18162711952743));
#33191=CARTESIAN_POINT('Ctrl Pts',(42.8514673479782,47.6853114483593,-7.116339600259));
#33192=CARTESIAN_POINT('Ctrl Pts',(42.6574161132917,46.5947951794462,-7.05105208099057));
#33193=CARTESIAN_POINT('Ctrl Pts',(42.62270583008,46.399732630104,-7.03937398841023));
#33194=CARTESIAN_POINT('Ctrl Pts',(42.6067072930659,46.2013404342854,-7.0276958958299));
#33195=CARTESIAN_POINT('Ctrl Pts',(42.6084214217016,46.0026727196953,-7.01601780324957));
#33196=CARTESIAN_POINT('Origin',(46.,46.,-5.));
#33197=CARTESIAN_POINT('',(42.6150735509525,45.9989672044636,-5.76601780324957));
#33198=CARTESIAN_POINT('',(42.6103671367935,45.9971074078126,-6.10898219675043));
#33199=CARTESIAN_POINT('',(42.61025,46.,-5.));
#33200=CARTESIAN_POINT('Ctrl Pts',(42.6103671367935,45.9971074078126,-6.10898219675043));
#33201=CARTESIAN_POINT('Ctrl Pts',(42.6177681492814,46.8429594152923,-6.15862952807558));
#33202=CARTESIAN_POINT('Ctrl Pts',(42.939437978457,47.6938378255849,-6.20827685940074));
#33203=CARTESIAN_POINT('Ctrl Pts',(43.5127589684757,48.3109062447032,-6.25792419072589));
#33204=CARTESIAN_POINT('Ctrl Pts',(44.2666908351797,49.1223671073078,-6.32321170999432));
#33205=CARTESIAN_POINT('Ctrl Pts',(45.4558012251992,49.5295020516264,-6.38849922926275));
#33206=CARTESIAN_POINT('Ctrl Pts',(46.5488771676489,49.3504312396045,-6.45378674853118));
#33207=CARTESIAN_POINT('Ctrl Pts',(47.6419531100986,49.1713604275825,-6.51907426779961));
#33208=CARTESIAN_POINT('Ctrl Pts',(48.6389946049786,48.4060838592201,-6.58436178706805));
#33209=CARTESIAN_POINT('Ctrl Pts',(49.0945939713514,47.3964743899603,-6.64964930633648));
#33210=CARTESIAN_POINT('Ctrl Pts',(49.5501933377243,46.3868649207005,-6.71493682560491));
#33211=CARTESIAN_POINT('Ctrl Pts',(49.46435057559,45.1329225505433,-6.78022434487334));
#33212=CARTESIAN_POINT('Ctrl Pts',(48.8754112762962,44.1948214953291,-6.84551186414177));
#33213=CARTESIAN_POINT('Ctrl Pts',(48.2864719770025,43.2567204401148,-6.9107993834102));
#33214=CARTESIAN_POINT('Ctrl Pts',(47.1944361405491,42.6344606998434,-6.97608690267863));
#33215=CARTESIAN_POINT('Ctrl Pts',(46.0871559866506,42.6060258474755,-7.04137442194706));
#33216=CARTESIAN_POINT('Ctrl Pts',(44.9798758327521,42.5775909951076,-7.1066619412155));
#33217=CARTESIAN_POINT('Ctrl Pts',(43.8573513614085,43.1429810306431,-7.17194946048392));
#33218=CARTESIAN_POINT('Ctrl Pts',(43.2210362385086,44.0496168129944,-7.23723697975236));
#33219=CARTESIAN_POINT('Ctrl Pts',(42.8255123385624,44.6131679648705,-7.27781871875171));
#33220=CARTESIAN_POINT('Ctrl Pts',(42.6178440955465,45.3085654996843,-7.31840045775107));
#33221=CARTESIAN_POINT('Ctrl Pts',(42.6141421045691,46.0019288481038,-7.35898219675043));
#33222=CARTESIAN_POINT('Ctrl Pts',(42.6084214217016,46.0026727196953,-7.01601780324957));
#33223=CARTESIAN_POINT('Ctrl Pts',(42.6162902969306,45.0906691362893,-6.96240837656147));
#33224=CARTESIAN_POINT('Ctrl Pts',(42.9974286013873,44.1728593836379,-6.90879894987337));
#33225=CARTESIAN_POINT('Ctrl Pts',(43.65518491261,43.5447009077758,-6.85518952318527));
#33226=CARTESIAN_POINT('Ctrl Pts',(44.4562245896939,42.7797065564077,-6.78990200391684));
#33227=CARTESIAN_POINT('Ctrl Pts',(45.6675235869406,42.4443015050609,-6.72461448464841));
#33228=CARTESIAN_POINT('Ctrl Pts',(46.7479566577516,42.6883218382704,-6.65932696537998));
#33229=CARTESIAN_POINT('Ctrl Pts',(47.8283897285627,42.9323421714799,-6.59403944611155));
#33230=CARTESIAN_POINT('Ctrl Pts',(48.7779568729381,43.7557878892457,-6.52875192684311));
#33231=CARTESIAN_POINT('Ctrl Pts',(49.1724575142977,44.7908002644018,-6.46346440757468));
#33232=CARTESIAN_POINT('Ctrl Pts',(49.5669581556574,45.8258126395579,-6.39817688830625));
#33233=CARTESIAN_POINT('Ctrl Pts',(49.4063922940013,47.0723916721042,-6.33288936903782));
#33234=CARTESIAN_POINT('Ctrl Pts',(48.7624894883155,47.9736521745216,-6.26760184976939));
#33235=CARTESIAN_POINT('Ctrl Pts',(48.1185866826298,48.874912676939,-6.20231433050096));
#33236=CARTESIAN_POINT('Ctrl Pts',(46.9913469329144,49.4308546492274,-6.13702681123253));
#33237=CARTESIAN_POINT('Ctrl Pts',(45.8843430448095,49.3931216462669,-6.0717392919641));
#33238=CARTESIAN_POINT('Ctrl Pts',(44.7773391567047,49.3553886433064,-6.00645177269566));
#33239=CARTESIAN_POINT('Ctrl Pts',(43.6905711302104,48.723980665097,-5.94116425342724));
#33240=CARTESIAN_POINT('Ctrl Pts',(43.1095316895885,47.7809671280428,-5.87587673415881));
#33241=CARTESIAN_POINT('Ctrl Pts',(42.7836277880051,47.2520326539168,-5.83925709052239));
#33242=CARTESIAN_POINT('Ctrl Pts',(42.6168294607952,46.6250649999332,-5.80263744688598));
#33243=CARTESIAN_POINT('Ctrl Pts',(42.6150735509525,45.9989672044636,-5.76601780324957));
#33244=CARTESIAN_POINT('Origin',(46.,46.,-5.));
#33245=CARTESIAN_POINT('',(42.6053667880302,45.9989154325097,-4.51601780324956));
#33246=CARTESIAN_POINT('',(42.6073204051797,46.0023448477177,-4.85898219675043));
#33247=CARTESIAN_POINT('',(42.61025,46.,-5.));
#33248=CARTESIAN_POINT('Ctrl Pts',(42.6073204051797,46.0023448477177,-4.85898219675043));
#33249=CARTESIAN_POINT('Ctrl Pts',(42.6060645714529,46.1604461130937,-4.86828355986323));
#33250=CARTESIAN_POINT('Ctrl Pts',(42.6161874000306,46.3183858931683,-4.87758492297603));
#33251=CARTESIAN_POINT('Ctrl Pts',(42.638248673256,46.4746401039977,-4.88688628608884));
#33252=CARTESIAN_POINT('Ctrl Pts',(42.7930997185616,47.5714094351789,-4.95217380535727));
#33253=CARTESIAN_POINT('Ctrl Pts',(43.5361370388243,48.585133719477,-5.0174613246257));
#33254=CARTESIAN_POINT('Ctrl Pts',(44.5354229739406,49.0629510855994,-5.08274884389413));
#33255=CARTESIAN_POINT('Ctrl Pts',(45.5347089090568,49.5407684517217,-5.14803636316256));
#33256=CARTESIAN_POINT('Ctrl Pts',(46.7902434590266,49.4826788996682,-5.21332388243099));
#33257=CARTESIAN_POINT('Ctrl Pts',(47.7411406457384,48.9146328206093,-5.27861140169942));
#33258=CARTESIAN_POINT('Ctrl Pts',(48.6920378324503,48.3465867415504,-5.34389892096786));
#33259=CARTESIAN_POINT('Ctrl Pts',(49.3382976559041,47.268584135486,-5.40918644023628));
#33260=CARTESIAN_POINT('Ctrl Pts',(49.3912159610244,46.1622019844742,-5.47447395950471));
#33261=CARTESIAN_POINT('Ctrl Pts',(49.4441342661448,45.0558198334624,-5.53976147877314));
#33262=CARTESIAN_POINT('Ctrl Pts',(48.9037110529317,43.9210581375031,-5.60504899804158));
#33263=CARTESIAN_POINT('Ctrl Pts',(48.0113699805936,43.2648499032208,-5.67033651731001));
#33264=CARTESIAN_POINT('Ctrl Pts',(47.1190289082556,42.6086416689385,-5.73562403657844));
#33265=CARTESIAN_POINT('Ctrl Pts',(45.8747699767926,42.4309868963332,-5.80091155584687));
#33266=CARTESIAN_POINT('Ctrl Pts',(44.834442072672,42.8112494594622,-5.8661990751153));
#33267=CARTESIAN_POINT('Ctrl Pts',(43.7941141685514,43.1915120225911,-5.93148659438373));
#33268=CARTESIAN_POINT('Ctrl Pts',(42.9577172917731,44.1296919214543,-5.99677411365216));
#33269=CARTESIAN_POINT('Ctrl Pts',(42.6988955250782,45.2066752613311,-6.06206163292059));
#33270=CARTESIAN_POINT('Ctrl Pts',(42.6368925401237,45.4646759027431,-6.07770182086387));
#33271=CARTESIAN_POINT('Ctrl Pts',(42.6080356272603,45.7306422420912,-6.09334200880715));
#33272=CARTESIAN_POINT('Ctrl Pts',(42.6103671367935,45.9971074078126,-6.10898219675043));
#33273=CARTESIAN_POINT('Ctrl Pts',(42.6150735509525,45.9989672044636,-5.76601780324957));
#33274=CARTESIAN_POINT('Ctrl Pts',(42.6136989279362,45.5088233376305,-5.73734992761755));
#33275=CARTESIAN_POINT('Ctrl Pts',(42.713472554676,45.0192125741512,-5.70868205198553));
#33276=CARTESIAN_POINT('Ctrl Pts',(42.9172428231758,44.5775868382122,-5.68001417635351));
#33277=CARTESIAN_POINT('Ctrl Pts',(43.3813042521348,43.5718391813348,-5.61472665708508));
#33278=CARTESIAN_POINT('Ctrl Pts',(44.3847379648023,42.814962963479,-5.54943913781665));
#33279=CARTESIAN_POINT('Ctrl Pts',(45.4792791954617,42.6450781158791,-5.48415161854822));
#33280=CARTESIAN_POINT('Ctrl Pts',(46.5738204261212,42.4751932682792,-5.41886409927979));
#33281=CARTESIAN_POINT('Ctrl Pts',(47.7594691747726,42.8922997909351,-5.35357658001136));
#33282=CARTESIAN_POINT('Ctrl Pts',(48.5065596183824,43.7100633464118,-5.28828906074292));
#33283=CARTESIAN_POINT('Ctrl Pts',(49.2536500619923,44.5278269018886,-5.22300154147449));
#33284=CARTESIAN_POINT('Ctrl Pts',(49.5621822005606,45.7462474901862,-5.15771402220606));
#33285=CARTESIAN_POINT('Ctrl Pts',(49.294325219302,46.8210190943985,-5.09242650293763));
#33286=CARTESIAN_POINT('Ctrl Pts',(49.0264682380435,47.8957906986107,-5.0271389836692));
#33287=CARTESIAN_POINT('Ctrl Pts',(48.1822221369581,48.8269133187375,-4.96185146440077));
#33288=CARTESIAN_POINT('Ctrl Pts',(47.1387376628694,49.1984257905606,-4.89656394513234));
#33289=CARTESIAN_POINT('Ctrl Pts',(46.0952531887807,49.5699382623838,-4.83127642586391));
#33290=CARTESIAN_POINT('Ctrl Pts',(44.8525303416886,49.3818405859034,-4.76598890659547));
#33291=CARTESIAN_POINT('Ctrl Pts',(43.9657317068215,48.7181617892766,-4.70070138732704));
#33292=CARTESIAN_POINT('Ctrl Pts',(43.1295476393945,48.0923628606262,-4.63914019263455));
#33293=CARTESIAN_POINT('Ctrl Pts',(42.6098180730754,47.0437217061788,-4.57757899794206));
#33294=CARTESIAN_POINT('Ctrl Pts',(42.6053667880302,45.9989154325097,-4.51601780324956));
#33295=CARTESIAN_POINT('Origin',(46.,46.,-5.));
#33296=CARTESIAN_POINT('',(42.6129097243346,46.0025162766385,-3.26601780324956));
#33297=CARTESIAN_POINT('',(42.6153404332635,45.9995769998228,-3.60898219675043));
#33298=CARTESIAN_POINT('',(42.61025,46.,-5.));
#33299=CARTESIAN_POINT('Ctrl Pts',(42.6153404332635,45.9995769998228,-3.60898219675043));
#33300=CARTESIAN_POINT('Ctrl Pts',(42.6160097400798,46.5851552375805,-3.64322511091931));
#33301=CARTESIAN_POINT('Ctrl Pts',(42.760737663966,47.1710433567983,-3.67746802508819));
#33302=CARTESIAN_POINT('Ctrl Pts',(43.0475707646209,47.6762508228982,-3.71171093925708));
#33303=CARTESIAN_POINT('Ctrl Pts',(43.5944465793799,48.6394790696203,-3.77699845852551));
#33304=CARTESIAN_POINT('Ctrl Pts',(44.6578919396997,49.3094233610044,-3.84228597779394));
#33305=CARTESIAN_POINT('Ctrl Pts',(45.762833038625,49.3867989384559,-3.90757349706237));
#33306=CARTESIAN_POINT('Ctrl Pts',(46.8677741375502,49.4641745159074,-3.9728610163308));
#33307=CARTESIAN_POINT('Ctrl Pts',(48.0142109750811,48.9489813794264,-4.03814853559923));
#33308=CARTESIAN_POINT('Ctrl Pts',(48.6899948916588,48.0713721777166,-4.10343605486766));
#33309=CARTESIAN_POINT('Ctrl Pts',(49.3657788082366,47.1937629760069,-4.16872357413609));
#33310=CARTESIAN_POINT('Ctrl Pts',(49.5709098038613,45.9537377090685,-4.23401109340452));
#33311=CARTESIAN_POINT('Ctrl Pts',(49.2137495430902,44.9052538701515,-4.29929861267296));
#33312=CARTESIAN_POINT('Ctrl Pts',(48.8565892823191,43.8567700312346,-4.36458613194139));
#33313=CARTESIAN_POINT('Ctrl Pts',(47.9371377651523,42.9998276203391,-4.42987365120982));
#33314=CARTESIAN_POINT('Ctrl Pts',(46.8661423131135,42.7172492160988,-4.49516117047825));
#33315=CARTESIAN_POINT('Ctrl Pts',(45.7951468610747,42.4346708118586,-4.56044868974668));
#33316=CARTESIAN_POINT('Ctrl Pts',(44.5726074741639,42.7264564142735,-4.62573620901511));
#33317=CARTESIAN_POINT('Ctrl Pts',(43.7446701658828,43.462256404513,-4.69102372828354));
#33318=CARTESIAN_POINT('Ctrl Pts',(43.034687186779,44.0932286579308,-4.74700988443917));
#33319=CARTESIAN_POINT('Ctrl Pts',(42.6148794373641,45.0507120575128,-4.8029960405948));
#33320=CARTESIAN_POINT('Ctrl Pts',(42.6073204051797,46.0023448477177,-4.85898219675043));
#33321=CARTESIAN_POINT('Ctrl Pts',(42.6053667880302,45.9989154325097,-4.51601780324956));
#33322=CARTESIAN_POINT('Ctrl Pts',(42.6050973499054,45.9356728766413,-4.51229147867363));
#33323=CARTESIAN_POINT('Ctrl Pts',(42.6067158558333,45.8724443715113,-4.50856515409769));
#33324=CARTESIAN_POINT('Ctrl Pts',(42.6102664008042,45.8093245452514,-4.50483882952175));
#33325=CARTESIAN_POINT('Ctrl Pts',(42.6724741522961,44.7034260146263,-4.43955131025332));
#33326=CARTESIAN_POINT('Ctrl Pts',(43.3277640779222,43.6308888701494,-4.37426379098489));
#33327=CARTESIAN_POINT('Ctrl Pts',(44.2833979772143,43.0708485018244,-4.30897627171646));
#33328=CARTESIAN_POINT('Ctrl Pts',(45.2390318765064,42.5108081334994,-4.24368875244803));
#33329=CARTESIAN_POINT('Ctrl Pts',(46.4950097494645,42.4632645413262,-4.17840123317959));
#33330=CARTESIAN_POINT('Ctrl Pts',(47.4902475822715,42.9494569104033,-4.11311371391116));
#33331=CARTESIAN_POINT('Ctrl Pts',(48.4854854150785,43.4356492794804,-4.04782619464273));
#33332=CARTESIAN_POINT('Ctrl Pts',(49.2199832077344,44.4555776098078,-3.9825386753743));
#33333=CARTESIAN_POINT('Ctrl Pts',(49.3656181645774,45.5536084957135,-3.91725115610587));
#33334=CARTESIAN_POINT('Ctrl Pts',(49.5112531214204,46.6516393816192,-3.85196363683744));
#33335=CARTESIAN_POINT('Ctrl Pts',(49.0680252424504,47.8277728231033,-3.78667611756901));
#33336=CARTESIAN_POINT('Ctrl Pts',(48.2339380792449,48.5565937636213,-3.72138859830058));
#33337=CARTESIAN_POINT('Ctrl Pts',(47.3998509160394,49.2854147041394,-3.65610107903214));
#33338=CARTESIAN_POINT('Ctrl Pts',(46.1749044685984,49.5669231436913,-3.59081355976371));
#33339=CARTESIAN_POINT('Ctrl Pts',(45.1063200540658,49.275360608986,-3.52552604049528));
#33340=CARTESIAN_POINT('Ctrl Pts',(44.0377356395332,48.9837980742807,-3.46023852122685));
#33341=CARTESIAN_POINT('Ctrl Pts',(43.125513257909,48.1191645653182,-3.39495100195842));
#33342=CARTESIAN_POINT('Ctrl Pts',(42.7771707604387,47.0677184695778,-3.32966348268999));
#33343=CARTESIAN_POINT('Ctrl Pts',(42.6639766146157,46.726050302327,-3.30844825620985));
#33344=CARTESIAN_POINT('Ctrl Pts',(42.6103242212129,46.3646560389635,-3.28723302972971));
#33345=CARTESIAN_POINT('Ctrl Pts',(42.6129097243346,46.0025162766385,-3.26601780324956));
#33346=CARTESIAN_POINT('Origin',(46.,46.,-5.));
#33347=CARTESIAN_POINT('',(42.612019924001,45.9972524552388,-2.01601780324957));
#33348=CARTESIAN_POINT('',(42.6060554931448,45.9983056788579,-2.35898219675043));
#33349=CARTESIAN_POINT('',(42.61025,46.,-5.));
#33350=CARTESIAN_POINT('Ctrl Pts',(42.6060554931448,45.9983056788579,-2.35898219675043));
#33351=CARTESIAN_POINT('Ctrl Pts',(42.6122930804025,47.0033168865153,-2.41816666197539));
#33352=CARTESIAN_POINT('Ctrl Pts',(43.0878123513283,48.0134657192039,-2.47735112720035));
#33353=CARTESIAN_POINT('Ctrl Pts',(43.8696390366459,48.6435236070725,-2.53653559242531));
#33354=CARTESIAN_POINT('Ctrl Pts',(44.7320870555345,49.3385525532341,-2.60182311169375));
#33355=CARTESIAN_POINT('Ctrl Pts',(45.9672719734487,49.5710594922115,-2.66711063096218));
#33356=CARTESIAN_POINT('Ctrl Pts',(47.0233987499047,49.2371762834963,-2.73239815023061));
#33357=CARTESIAN_POINT('Ctrl Pts',(48.0795255263607,48.903293074781,-2.79768566949904));
#33358=CARTESIAN_POINT('Ctrl Pts',(48.9565941613586,48.0030197183732,-2.86297318876747));
#33359=CARTESIAN_POINT('Ctrl Pts',(49.2627910132094,46.9385361233667,-2.9282607080359));
#33360=CARTESIAN_POINT('Ctrl Pts',(49.5689878650602,45.8740525283602,-2.99354822730433));
#33361=CARTESIAN_POINT('Ctrl Pts',(49.304312933764,44.6453586947551,-3.05883574657276));
#33362=CARTESIAN_POINT('Ctrl Pts',(48.5870046948683,43.8013499853766,-3.12412326584119));
#33363=CARTESIAN_POINT('Ctrl Pts',(47.8696964559727,42.9573412759981,-3.18941078510963));
#33364=CARTESIAN_POINT('Ctrl Pts',(46.6997549094776,42.4980176908463,-3.25469830437806));
#33365=CARTESIAN_POINT('Ctrl Pts',(45.5998289776439,42.6285732426639,-3.31998582364649));
#33366=CARTESIAN_POINT('Ctrl Pts',(44.4999030458102,42.7591287944815,-3.38527334291492));
#33367=CARTESIAN_POINT('Ctrl Pts',(43.4699927286378,43.4795634832685,-3.45056086218335));
#33368=CARTESIAN_POINT('Ctrl Pts',(42.9701907046508,44.4680369286922,-3.51584838145178));
#33369=CARTESIAN_POINT('Ctrl Pts',(42.7325318590322,44.9380619519803,-3.54689298655133));
#33370=CARTESIAN_POINT('Ctrl Pts',(42.6147336401121,45.4686921266364,-3.57793759165088));
#33371=CARTESIAN_POINT('Ctrl Pts',(42.6153404332635,45.9995769998228,-3.60898219675043));
#33372=CARTESIAN_POINT('Ctrl Pts',(42.6129097243346,46.0025162766385,-3.26601780324956));
#33373=CARTESIAN_POINT('Ctrl Pts',(42.6182808218664,45.2502108675773,-3.22194551046127));
#33374=CARTESIAN_POINT('Ctrl Pts',(42.8663492573033,44.4946882220169,-3.17787321767299));
#33375=CARTESIAN_POINT('Ctrl Pts',(43.3274957154746,43.9061108128077,-3.1338009248847));
#33376=CARTESIAN_POINT('Ctrl Pts',(44.0106257812974,43.0342079342963,-3.06851340561626));
#33377=CARTESIAN_POINT('Ctrl Pts',(45.1613485262596,42.5286608597917,-3.00322588634783));
#33378=CARTESIAN_POINT('Ctrl Pts',(46.2656006721812,42.6153128706582,-2.9379383670794));
#33379=CARTESIAN_POINT('Ctrl Pts',(47.3698528181026,42.7019648815247,-2.87265084781097));
#33380=CARTESIAN_POINT('Ctrl Pts',(48.4276343649834,43.3808159777622,-2.80736332854254));
#33381=CARTESIAN_POINT('Ctrl Pts',(48.9664016482502,44.3486028127642,-2.74207580927411));
#33382=CARTESIAN_POINT('Ctrl Pts',(49.505168931517,45.3163896477662,-2.67678829000568));
#33383=CARTESIAN_POINT('Ctrl Pts',(49.5249219511698,46.5731122215327,-2.61150077073725));
#33384=CARTESIAN_POINT('Ctrl Pts',(49.0168365389143,47.5573531146787,-2.54621325146882));
#33385=CARTESIAN_POINT('Ctrl Pts',(48.5087511266589,48.5415940078247,-2.48092573220038));
#33386=CARTESIAN_POINT('Ctrl Pts',(47.4728272824952,49.2533532203503,-2.41563821293195));
#33387=CARTESIAN_POINT('Ctrl Pts',(46.3718438724484,49.3746674620912,-2.35035069366352));
#33388=CARTESIAN_POINT('Ctrl Pts',(45.2708604624016,49.4959817038321,-2.28506317439509));
#33389=CARTESIAN_POINT('Ctrl Pts',(44.1048174864718,49.0268509747885,-2.21977565512666));
#33390=CARTESIAN_POINT('Ctrl Pts',(43.3946227463979,48.1768474007417,-2.15448813585823));
#33391=CARTESIAN_POINT('Ctrl Pts',(42.8925313667238,47.5759143845713,-2.10833135832201));
#33392=CARTESIAN_POINT('Ctrl Pts',(42.6182804769167,46.7846148192803,-2.06217458078579));
#33393=CARTESIAN_POINT('Ctrl Pts',(42.612019924001,45.9972524552388,-2.01601780324957));
#33394=CARTESIAN_POINT('Origin',(46.,46.,-5.));
#33395=CARTESIAN_POINT('',(42.6059705137377,46.0015452631454,-0.766017803249565));
#33396=CARTESIAN_POINT('',(42.6118894404877,46.0027670997301,-1.10898219675043));
#33397=CARTESIAN_POINT('',(42.61025,46.,-5.));
#33398=CARTESIAN_POINT('',(48.5732344270147,48.2065515280923,2.77555756156289E-16));
#33399=CARTESIAN_POINT('Ctrl Pts',(42.6059705137377,46.0015452631454,-0.766017803249565));
#33400=CARTESIAN_POINT('Ctrl Pts',(42.612001272004,44.9918195798286,-0.706541093305003));
#33401=CARTESIAN_POINT('Ctrl Pts',(43.0927628221167,43.977304319078,-0.647064383360442));
#33402=CARTESIAN_POINT('Ctrl Pts',(43.8812694180946,43.3473613724735,-0.58758767341588));
#33403=CARTESIAN_POINT('Ctrl Pts',(44.746812243617,42.6558736909459,-0.522300154147449));
#33404=CARTESIAN_POINT('Ctrl Pts',(45.9831702716104,42.4277736819444,-0.457012634879018));
#33405=CARTESIAN_POINT('Ctrl Pts',(47.0377266680876,42.7668601274187,-0.391725115610586));
#33406=CARTESIAN_POINT('Ctrl Pts',(48.0922830645648,43.105946572893,-0.326437596342155));
#33407=CARTESIAN_POINT('Ctrl Pts',(48.9650378295259,44.0122194728431,-0.261150077073724));
#33408=CARTESIAN_POINT('Ctrl Pts',(49.2663071512956,45.0762555694146,-0.195862557805293));
#33409=CARTESIAN_POINT('Ctrl Pts',(49.5675764730653,46.1402916659861,-0.130575038536862));
#33410=CARTESIAN_POINT('Ctrl Pts',(49.2973603516437,47.3620909591791,-0.0652875192684305));
#33411=CARTESIAN_POINT('Ctrl Pts',(48.5732344270147,48.2065515280923,6.43618311088306E-16));
#33412=CARTESIAN_POINT('',(43.4219940034589,48.2094945108994,-4.30182186788769E-15));
#33413=CARTESIAN_POINT('Origin',(46.,46.,0.));
#33414=CARTESIAN_POINT('Ctrl Pts',(43.4219648396841,48.2095124983745,-2.91433543964104E-15));
#33415=CARTESIAN_POINT('Ctrl Pts',(44.1103014967847,49.006716779805,-0.0620616329205997));
#33416=CARTESIAN_POINT('Ctrl Pts',(45.2006367519963,49.463575489776,-0.124123265841196));
#33417=CARTESIAN_POINT('Ctrl Pts',(46.2508550251211,49.3856446881349,-0.186184898761793));
#33418=CARTESIAN_POINT('Ctrl Pts',(47.3556623354671,49.3036631405295,-0.251472418030224));
#33419=CARTESIAN_POINT('Ctrl Pts',(48.4160738145477,48.6298518070086,-0.316759937298655));
#33420=CARTESIAN_POINT('Ctrl Pts',(48.9590111284627,47.664543622046,-0.382047456567087));
#33421=CARTESIAN_POINT('Ctrl Pts',(49.5019484423776,46.6992354370834,-0.447334975835518));
#33422=CARTESIAN_POINT('Ctrl Pts',(49.527411591127,45.442430400679,-0.512622495103949));
#33423=CARTESIAN_POINT('Ctrl Pts',(49.0237123948945,44.4559131182979,-0.57791001437238));
#33424=CARTESIAN_POINT('Ctrl Pts',(48.520013198662,43.4693958359168,-0.643197533640811));
#33425=CARTESIAN_POINT('Ctrl Pts',(47.4871516574478,42.7531663075589,-0.708485052909242));
#33426=CARTESIAN_POINT('Ctrl Pts',(46.3866919409849,42.6270244092924,-0.773772572177674));
#33427=CARTESIAN_POINT('Ctrl Pts',(45.2862322245221,42.5008825110258,-0.839060091446105));
#33428=CARTESIAN_POINT('Ctrl Pts',(44.1181743328107,42.9648282428506,-0.904347610714536));
#33429=CARTESIAN_POINT('Ctrl Pts',(43.4042508272458,43.811681954104,-0.969635129982967));
#33430=CARTESIAN_POINT('Ctrl Pts',(42.8963275798851,44.4141788374625,-1.01608415223879));
#33431=CARTESIAN_POINT('Ctrl Pts',(42.6182716386338,45.2104906540304,-1.06253317449461));
#33432=CARTESIAN_POINT('Ctrl Pts',(42.6118894404877,46.0027670997301,-1.10898219675043));
#33433=CARTESIAN_POINT('Origin',(46.,46.,2.76038497140452));
#33434=CARTESIAN_POINT('',(41.9196903893103,46.0023244618346,-7.76038497140452));
#33435=CARTESIAN_POINT('',(41.9137291820556,45.9966118489329,-7.86461502859548));
#33436=CARTESIAN_POINT('',(41.915,46.0000000000001,2.76038497140452));
#33437=CARTESIAN_POINT('',(42.5743852316216,43.7746037524369,-9.));
#33438=CARTESIAN_POINT('Ctrl Pts',(41.9137291820556,45.9966118489329,-7.86461502859548));
#33439=CARTESIAN_POINT('Ctrl Pts',(41.9230937808476,47.0638215506166,-7.91663908938816));
#33440=CARTESIAN_POINT('Ctrl Pts',(42.8919850912141,49.4855112174958,-8.03395066944928));
#33441=CARTESIAN_POINT('Ctrl Pts',(46.9472267461691,50.7128989977065,-8.21654976877883));
#33442=CARTESIAN_POINT('Ctrl Pts',(50.4487163480431,47.8195940258066,-8.41241232658412));
#33443=CARTESIAN_POINT('Ctrl Pts',(49.9795579209025,43.2986184205048,-8.6082748843894));
#33444=CARTESIAN_POINT('Ctrl Pts',(45.9463561559116,41.1952276423334,-8.80413744219472));
#33445=CARTESIAN_POINT('Ctrl Pts',(43.3046954441484,42.6504167892078,-8.93471248073157));
#33446=CARTESIAN_POINT('Ctrl Pts',(42.5743852316216,43.7746037524369,-9.));
#33447=CARTESIAN_POINT('',(41.9138448206429,45.7875586974126,-9.));
#33448=CARTESIAN_POINT('Origin',(46.,46.,-9.));
#33449=CARTESIAN_POINT('Ctrl Pts',(41.9196903893103,46.0023244618346,-7.76038497140452));
#33450=CARTESIAN_POINT('Ctrl Pts',(41.9169744024249,46.5110144539541,-7.78509075167359));
#33451=CARTESIAN_POINT('Ctrl Pts',(42.2389222273681,48.3606596187085,-7.8750840512111));
#33452=CARTESIAN_POINT('Ctrl Pts',(44.9804150360981,50.6979233958617,-8.03036487001703));
#33453=CARTESIAN_POINT('Ctrl Pts',(49.3490853663058,49.448562791698,-8.22622742782233));
#33454=CARTESIAN_POINT('Ctrl Pts',(50.7259992165293,45.1181263046889,-8.42208998562762));
#33455=CARTESIAN_POINT('Ctrl Pts',(47.8793454040792,41.5754411676036,-8.61795254343291));
#33456=CARTESIAN_POINT('Ctrl Pts',(43.4302580460658,41.9795085567297,-8.81058921489037));
#33457=CARTESIAN_POINT('Ctrl Pts',(41.9843543567741,44.5202461309732,-8.9379383670794));
#33458=CARTESIAN_POINT('Ctrl Pts',(41.913803751014,45.7875629828622,-9.));
#33459=CARTESIAN_POINT('Origin',(46.,46.,2.76038497140452));
#33460=CARTESIAN_POINT('',(41.915141161974,45.9965141266804,-6.51038497140452));
#33461=CARTESIAN_POINT('',(41.9127963736709,46.0032209041833,-6.61461502859548));
#33462=CARTESIAN_POINT('',(41.915,46.0000000000001,2.76038497140452));
#33463=CARTESIAN_POINT('Ctrl Pts',(41.9127963736709,46.0032209041833,-6.61461502859548));
#33464=CARTESIAN_POINT('Ctrl Pts',(41.9107306710448,46.2426360864535,-6.62629312117581));
#33465=CARTESIAN_POINT('Ctrl Pts',(42.0377967048478,47.818337004481,-6.70325873302458));
#33466=CARTESIAN_POINT('Ctrl Pts',(44.0829609284797,50.4085211796553,-6.84551186414177));
#33467=CARTESIAN_POINT('Ctrl Pts',(48.6116787512404,50.0359897044587,-7.04137442194707));
#33468=CARTESIAN_POINT('Ctrl Pts',(50.8069343717212,46.0574693241754,-7.23723697975236));
#33469=CARTESIAN_POINT('Ctrl Pts',(48.7074347435192,42.027575728146,-7.43309953755765));
#33470=CARTESIAN_POINT('Ctrl Pts',(44.1888313497151,41.5469450910147,-7.62896209536295));
#33471=CARTESIAN_POINT('Ctrl Pts',(42.0589983118285,44.1157440212414,-7.77280059237555));
#33472=CARTESIAN_POINT('Ctrl Pts',(41.9113416912421,45.7245282909115,-7.85135157011973));
#33473=CARTESIAN_POINT('Ctrl Pts',(41.9137291820556,45.9966118489329,-7.86461502859548));
#33474=CARTESIAN_POINT('Ctrl Pts',(41.915141161974,45.9965141266804,-6.51038497140452));
#33475=CARTESIAN_POINT('Ctrl Pts',(41.9240601489239,47.0158534439028,-6.56003230272967));
#33476=CARTESIAN_POINT('Ctrl Pts',(42.8214694089007,49.3896731038562,-6.67496715332326));
#33477=CARTESIAN_POINT('Ctrl Pts',(46.7771853228611,50.7440554992066,-6.85518952318527));
#33478=CARTESIAN_POINT('Ctrl Pts',(50.3818002707934,47.9773428079219,-7.05105208099057));
#33479=CARTESIAN_POINT('Ctrl Pts',(50.0714520002853,43.4439513347231,-7.24691463879585));
#33480=CARTESIAN_POINT('Ctrl Pts',(46.1234029772789,41.1942889357184,-7.44277719660116));
#33481=CARTESIAN_POINT('Ctrl Pts',(42.577032171383,42.9805152204495,-7.61393397413737));
#33482=CARTESIAN_POINT('Ctrl Pts',(41.924151672043,45.1667497798393,-7.71980323240516));
#33483=CARTESIAN_POINT('Ctrl Pts',(41.9196903893103,46.0023244618346,-7.76038497140452));
#33484=CARTESIAN_POINT('Origin',(46.,46.,2.76038497140452));
#33485=CARTESIAN_POINT('',(41.9114695346733,46.0028257844758,-5.26038497140452));
#33486=CARTESIAN_POINT('',(41.92081287872,45.9987553743592,-5.36461502859548));
#33487=CARTESIAN_POINT('',(41.915,46.0000000000001,2.76038497140452));
#33488=CARTESIAN_POINT('Ctrl Pts',(41.92081287872,45.9987553743592,-5.36461502859548));
#33489=CARTESIAN_POINT('Ctrl Pts',(41.9229289320299,46.7532680949118,-5.40123467223189));
#33490=CARTESIAN_POINT('Ctrl Pts',(42.4823086036718,48.8558848674044,-5.50314183513673));
#33491=CARTESIAN_POINT('Ctrl Pts',(45.8362350743765,50.8045030456205,-5.67033651731001));
#33492=CARTESIAN_POINT('Ctrl Pts',(49.9115571874415,48.7945999936567,-5.86619907511531));
#33493=CARTESIAN_POINT('Ctrl Pts',(50.4920526914155,44.2878292749147,-6.0620616329206));
#33494=CARTESIAN_POINT('Ctrl Pts',(47.059072278606,41.3108170258638,-6.2579241907259));
#33495=CARTESIAN_POINT('Ctrl Pts',(42.9409562421533,42.4511109778925,-6.44210865595085));
#33496=CARTESIAN_POINT('Ctrl Pts',(41.9222791837043,44.9041620832633,-6.56100560190738));
#33497=CARTESIAN_POINT('Ctrl Pts',(41.9127963736709,46.0032209041833,-6.61461502859548));
#33498=CARTESIAN_POINT('Ctrl Pts',(41.9114695346733,46.0028257844758,-5.26038497140452));
#33499=CARTESIAN_POINT('Ctrl Pts',(41.9099561249016,46.1933541918985,-5.26968633451732));
#33500=CARTESIAN_POINT('Ctrl Pts',(42.0077820074887,47.7196665524005,-5.34427521689856));
#33501=CARTESIAN_POINT('Ctrl Pts',(43.926226788663,50.3369968125737,-5.48415161854822));
#33502=CARTESIAN_POINT('Ctrl Pts',(48.4653744868355,50.126985023971,-5.68001417635351));
#33503=CARTESIAN_POINT('Ctrl Pts',(50.8018046472976,46.229670491242,-5.87587673415881));
#33504=CARTESIAN_POINT('Ctrl Pts',(48.8480067336088,42.1271542042059,-6.07173929196409));
#33505=CARTESIAN_POINT('Ctrl Pts',(44.3496239015183,41.4848769748296,-6.26760184976939));
#33506=CARTESIAN_POINT('Ctrl Pts',(42.092272202268,44.0169308928917,-6.41381707624953));
#33507=CARTESIAN_POINT('Ctrl Pts',(41.9123314513927,45.6753959905429,-6.49474478346124));
#33508=CARTESIAN_POINT('Ctrl Pts',(41.915141161974,45.9965141266804,-6.51038497140452));
#33509=CARTESIAN_POINT('Origin',(46.,46.,2.76038497140452));
#33510=CARTESIAN_POINT('',(41.9211344995594,45.9994902409546,-4.01038497140451));
#33511=CARTESIAN_POINT('',(41.909115223572,45.99869298379,-4.11461502859548));
#33512=CARTESIAN_POINT('',(41.915,46.0000000000001,2.76038497140452));
#33513=CARTESIAN_POINT('Ctrl Pts',(41.909115223572,45.99869298379,-4.11461502859548));
#33514=CARTESIAN_POINT('Ctrl Pts',(41.9144794832991,47.2577928076527,-4.17617622328797));
#33515=CARTESIAN_POINT('Ctrl Pts',(43.2050473399624,49.8617288828865,-4.3030249372489));
#33516=CARTESIAN_POINT('Ctrl Pts',(47.6123997659237,50.5288227185664,-4.49516117047825));
#33517=CARTESIAN_POINT('Ctrl Pts',(50.6646118667576,47.1625249946476,-4.69102372828354));
#33518=CARTESIAN_POINT('Ctrl Pts',(49.5491722744117,42.7575558053009,-4.88688628608884));
#33519=CARTESIAN_POINT('Ctrl Pts',(45.2626834729594,41.249586062651,-5.08274884389413));
#33520=CARTESIAN_POINT('Ctrl Pts',(42.3132199522082,43.4743257401283,-5.24199175806301));
#33521=CARTESIAN_POINT('Ctrl Pts',(41.9191563155453,45.4080812255242,-5.33594715296346));
#33522=CARTESIAN_POINT('Ctrl Pts',(41.92081287872,45.9987553743592,-5.36461502859548));
#33523=CARTESIAN_POINT('Ctrl Pts',(41.9211344995594,45.9994902409546,-4.01038497140451));
#33524=CARTESIAN_POINT('Ctrl Pts',(41.9219410836274,46.7051726957788,-4.0446278855734));
#33525=CARTESIAN_POINT('Ctrl Pts',(42.4288873183858,48.757394326904,-4.14415831901071));
#33526=CARTESIAN_POINT('Ctrl Pts',(45.664182571157,50.7955503680233,-4.30897627171645));
#33527=CARTESIAN_POINT('Ctrl Pts',(49.8089081243513,48.9329670248342,-4.50483882952175));
#33528=CARTESIAN_POINT('Ctrl Pts',(50.5505204413009,44.4498902060922,-4.70070138732704));
#33529=CARTESIAN_POINT('Ctrl Pts',(47.226417382704,41.351776998474,-4.89656394513234));
#33530=CARTESIAN_POINT('Ctrl Pts',(43.0164532244616,42.3565764685033,-5.08312513982482));
#33531=CARTESIAN_POINT('Ctrl Pts',(41.9205789517317,44.8560096629367,-5.20439881524889));
#33532=CARTESIAN_POINT('Ctrl Pts',(41.9114695346733,46.0028257844758,-5.26038497140452));
#33533=CARTESIAN_POINT('Origin',(46.,46.,2.76038497140452));
#33534=CARTESIAN_POINT('',(41.9099451845995,45.9979581674561,-2.76038497140452));
#33535=CARTESIAN_POINT('',(41.9182052434271,46.003032374089,-2.86461502859548));
#33536=CARTESIAN_POINT('',(41.915,46.0000000000001,2.76038497140452));
#33537=CARTESIAN_POINT('Ctrl Pts',(41.918205243427,46.003032374089,-2.86461502859548));
#33538=CARTESIAN_POINT('Ctrl Pts',(41.9150894442525,46.4394483130513,-2.88583025507562));
#33539=CARTESIAN_POINT('Ctrl Pts',(42.1787199801138,48.2152230225309,-2.97233300082419));
#33540=CARTESIAN_POINT('Ctrl Pts',(44.7345906088731,50.6377588369492,-3.1241232658412));
#33541=CARTESIAN_POINT('Ctrl Pts',(49.1631528076755,49.6200183172327,-3.31998582364649));
#33542=CARTESIAN_POINT('Ctrl Pts',(50.7655593735804,45.3679303091532,-3.51584838145178));
#33543=CARTESIAN_POINT('Ctrl Pts',(48.1101215244772,41.6805723363936,-3.71171093925708));
#33544=CARTESIAN_POINT('Ctrl Pts',(43.5693710758889,41.8524572016734,-3.90757349706237));
#33545=CARTESIAN_POINT('Ctrl Pts',(41.9449143886546,44.5112652628352,-4.04187486017517));
#33546=CARTESIAN_POINT('Ctrl Pts',(41.9087905227121,45.9224791506983,-4.11088870401954));
#33547=CARTESIAN_POINT('Ctrl Pts',(41.909115223572,45.99869298379,-4.11461502859548));
#33548=CARTESIAN_POINT('Ctrl Pts',(41.9099451845995,45.9979581674561,-2.76038497140452));
#33549=CARTESIAN_POINT('Ctrl Pts',(41.9174621235915,47.2091008131617,-2.81956943662948));
#33550=CARTESIAN_POINT('Ctrl Pts',(43.1226545649493,49.769299341883,-2.94404142112287));
#33551=CARTESIAN_POINT('Ctrl Pts',(47.4490851541316,50.5836916797423,-3.1338009248847));
#33552=CARTESIAN_POINT('Ctrl Pts',(50.619960918391,47.3289236340817,-3.32966348268999));
#33553=CARTESIAN_POINT('Ctrl Pts',(49.6630787639445,42.8868134693702,-3.52552604049528));
#33554=CARTESIAN_POINT('Ctrl Pts',(45.4333763810852,41.2262159220479,-3.72138859830058));
#33555=CARTESIAN_POINT('Ctrl Pts',(42.3609054830561,43.3754463728178,-3.88300824193698));
#33556=CARTESIAN_POINT('Ctrl Pts',(41.9204032509354,45.3597189578316,-3.97934036630497));
#33557=CARTESIAN_POINT('Ctrl Pts',(41.9211344995594,45.9994902409546,-4.01038497140451));
#33558=CARTESIAN_POINT('Origin',(46.,46.,2.76038497140452));
#33559=CARTESIAN_POINT('',(41.9169756956685,46.0033346419049,-1.51038497140452));
#33560=CARTESIAN_POINT('',(41.9171329418229,45.9966889238588,-1.61461502859548));
#33561=CARTESIAN_POINT('',(41.915,46.0000000000001,2.76038497140452));
#33562=CARTESIAN_POINT('Ctrl Pts',(41.9171329418229,45.9966889238588,-1.61461502859548));
#33563=CARTESIAN_POINT('Ctrl Pts',(41.9246775568123,46.9455421599706,-1.6607718061317));
#33564=CARTESIAN_POINT('Ctrl Pts',(42.7226626973778,49.2479787911961,-1.77221610293635));
#33565=CARTESIAN_POINT('Ctrl Pts',(46.5265139156528,50.7783713513675,-1.94894791900943));
#33566=CARTESIAN_POINT('Ctrl Pts',(50.2717006433544,48.205140538033,-2.14481047681473));
#33567=CARTESIAN_POINT('Ctrl Pts',(50.2002873368139,43.661697764522,-2.34067303462002));
#33568=CARTESIAN_POINT('Ctrl Pts',(46.3760782190255,41.2074400215055,-2.53653559242531));
#33569=CARTESIAN_POINT('Ctrl Pts',(42.6664799891873,42.8371779761014,-2.71118292375047));
#33570=CARTESIAN_POINT('Ctrl Pts',(41.9246779725125,45.0964264013728,-2.82054273580719));
#33571=CARTESIAN_POINT('Ctrl Pts',(41.918205243427,46.003032374089,-2.86461502859548));
#33572=CARTESIAN_POINT('Ctrl Pts',(41.9169756956685,46.0033346419049,-1.51038497140452));
#33573=CARTESIAN_POINT('Ctrl Pts',(41.9138563439275,46.390566259229,-1.52922346841713));
#33574=CARTESIAN_POINT('Ctrl Pts',(42.1404155757815,48.1162325445959,-1.61334948469817));
#33575=CARTESIAN_POINT('Ctrl Pts',(44.5692318828111,50.5894261400569,-1.76276302024764));
#33576=CARTESIAN_POINT('Ctrl Pts',(49.0314017551548,49.7310441604199,-1.95862557805294));
#33577=CARTESIAN_POINT('Ctrl Pts',(50.7851513154972,45.5390953919881,-2.15448813585823));
#33578=CARTESIAN_POINT('Ctrl Pts',(48.2635416323089,41.7589579733313,-2.35035069366352));
#33579=CARTESIAN_POINT('Ctrl Pts',(43.7195493508676,41.7680235772757,-2.54621325146881));
#33580=CARTESIAN_POINT('Ctrl Pts',(41.9704474010668,44.4129095021318,-2.68289134404915));
#33581=CARTESIAN_POINT('Ctrl Pts',(41.9091700439484,45.8730661203117,-2.75428191736105));
#33582=CARTESIAN_POINT('Ctrl Pts',(41.9099451845995,45.9979581674561,-2.76038497140452));
#33583=CARTESIAN_POINT('Origin',(46.,46.,2.76038497140452));
#33584=CARTESIAN_POINT('',(41.9194198683446,45.9961669413359,-0.260384971404518));
#33585=CARTESIAN_POINT('',(41.9098427756084,46.0018622022123,-0.364615028595478));
#33586=CARTESIAN_POINT('',(41.915,46.0000000000001,2.76038497140452));
#33587=CARTESIAN_POINT('',(44.942095577027,42.0543614925016,0.));
#33588=CARTESIAN_POINT('Ctrl Pts',(44.942095577027,42.0543614925016,0.));
#33589=CARTESIAN_POINT('Ctrl Pts',(43.6472519732775,42.4015349025496,-0.0652875192684312));
#33590=CARTESIAN_POINT('Ctrl Pts',(42.1846936066115,43.7726390243385,-0.152082509736604));
#33591=CARTESIAN_POINT('Ctrl Pts',(41.9164511209723,45.5536935953327,-0.238877500204776));
#33592=CARTESIAN_POINT('Ctrl Pts',(41.9194198683446,45.9961669413359,-0.260384971404518));
#33593=CARTESIAN_POINT('',(47.0606472822454,42.0481878432335,2.51247271755868E-15));
#33594=CARTESIAN_POINT('Origin',(46.,46.,0.));
#33595=CARTESIAN_POINT('Ctrl Pts',(47.0606640384105,42.0481501283249,1.75098650856409E-16));
#33596=CARTESIAN_POINT('Ctrl Pts',(45.8335722254876,41.7236247803045,-0.0620616329205975));
#33597=CARTESIAN_POINT('Ctrl Pts',(43.1010253798376,42.2867107335592,-0.183599975785757));
#33598=CARTESIAN_POINT('Ctrl Pts',(41.9171104642337,44.7850381248174,-0.305138318650916));
#33599=CARTESIAN_POINT('Ctrl Pts',(41.9098427756084,46.0018622022123,-0.364615028595478));
#33600=CARTESIAN_POINT('Origin',(60.,-60.,-6.));
#33601=CARTESIAN_POINT('',(64.262772575926,-60.0000736173382,-4.57968167058906));
#33602=CARTESIAN_POINT('',(64.2633463740757,-59.9999932305335,-4.17031832941094));
#33603=CARTESIAN_POINT('',(64.263,-60.,-6.));
#33604=CARTESIAN_POINT('',(60.8043894954945,-64.1864216867795,-3.));
#33605=CARTESIAN_POINT('Ctrl Pts',(64.2633463740757,-59.9999932305335,-4.17031832941094));
#33606=CARTESIAN_POINT('Ctrl Pts',(64.2633470323478,-59.99313820065,-4.16993434591159));
#33607=CARTESIAN_POINT('Ctrl Pts',(64.263330832606,-59.9862831738927,-4.16955036241224));
#33608=CARTESIAN_POINT('Ctrl Pts',(64.2632977556816,-59.9794282285766,-4.1691663789129));
#33609=CARTESIAN_POINT('Ctrl Pts',(64.259940629834,-59.2836889926924,-4.13019416628246));
#33610=CARTESIAN_POINT('Ctrl Pts',(64.0827293990401,-58.588788693418,-4.09122195365203));
#33611=CARTESIAN_POINT('Ctrl Pts',(63.7524939347896,-57.9764089025128,-4.0522497410216));
#33612=CARTESIAN_POINT('Ctrl Pts',(63.4222584705391,-57.3640291116076,-4.01327752839118));
#33613=CARTESIAN_POINT('Ctrl Pts',(62.9389987728321,-56.8341698290715,-3.97430531576075));
#33614=CARTESIAN_POINT('Ctrl Pts',(62.3595200338666,-56.4491133284713,-3.93533310313032));
#33615=CARTESIAN_POINT('Ctrl Pts',(61.780041294901,-56.0640568278712,-3.89636089049989));
#33616=CARTESIAN_POINT('Ctrl Pts',(61.104343514677,-55.8238031092071,-3.85738867786946));
#33617=CARTESIAN_POINT('Ctrl Pts',(60.4118497430403,-55.7565921213005,-3.81841646523903));
#33618=CARTESIAN_POINT('Ctrl Pts',(59.7193559714036,-55.689381133394,-3.77944425260859));
#33619=CARTESIAN_POINT('Ctrl Pts',(59.0100662083542,-55.7952128762451,-3.74047203997817));
#33620=CARTESIAN_POINT('Ctrl Pts',(58.367356732413,-56.0616485702291,-3.70149982734774));
#33621=CARTESIAN_POINT('Ctrl Pts',(57.7246472564718,-56.3280842642132,-3.66252761471731));
#33622=CARTESIAN_POINT('Ctrl Pts',(57.1485180676388,-56.7551239093303,-3.62355540208688));
#33623=CARTESIAN_POINT('Ctrl Pts',(56.7066830424806,-57.2925687565161,-3.58458318945645));
#33624=CARTESIAN_POINT('Ctrl Pts',(56.2648480173224,-57.8300136037019,-3.54561097682602));
#33625=CARTESIAN_POINT('Ctrl Pts',(55.9573071558389,-58.4778636529564,-3.50663876419559));
#33626=CARTESIAN_POINT('Ctrl Pts',(55.8202250112632,-59.1599728770642,-3.46766655156516));
#33627=CARTESIAN_POINT('Ctrl Pts',(55.6831428666875,-59.842082101172,-3.42869433893473));
#33628=CARTESIAN_POINT('Ctrl Pts',(55.7165194390194,-60.558450500133,-3.3897221263043));
#33629=CARTESIAN_POINT('Ctrl Pts',(55.9163989736504,-61.2248597751814,-3.35074991367387));
#33630=CARTESIAN_POINT('Ctrl Pts',(56.1162785082814,-61.8912690502299,-3.31177770104344));
#33631=CARTESIAN_POINT('Ctrl Pts',(56.4826610052114,-62.5077192013657,-3.27280548841301));
#33632=CARTESIAN_POINT('Ctrl Pts',(56.9725485708617,-63.0017699164546,-3.23383327578258));
#33633=CARTESIAN_POINT('Ctrl Pts',(57.462436136512,-63.4958206315434,-3.19486106315215));
#33634=CARTESIAN_POINT('Ctrl Pts',(58.0758287708825,-63.8674719105853,-3.15588885052172));
#33635=CARTESIAN_POINT('Ctrl Pts',(58.740462519741,-64.0729506012584,-3.11691663789129));
#33636=CARTESIAN_POINT('Ctrl Pts',(59.4050962685994,-64.2784292919315,-3.07794442526086));
#33637=CARTESIAN_POINT('Ctrl Pts',(60.1209711319459,-64.3177353942359,-3.03897221263043));
#33638=CARTESIAN_POINT('Ctrl Pts',(60.8043894954946,-64.1864216867795,-3.));
#33639=CARTESIAN_POINT('',(64.0279239112946,-58.6032685651144,-3.00000000000001));
#33640=CARTESIAN_POINT('Origin',(60.,-60.,-3.));
#33641=CARTESIAN_POINT('',(64.2630923571199,-60.0000961870058,-3.07968167058906));
#33642=CARTESIAN_POINT('Ctrl Pts',(64.0279239112946,-58.6032685651144,-3.00000000000001));
#33643=CARTESIAN_POINT('Ctrl Pts',(64.1829036812454,-59.0514416549545,-3.02656055686302));
#33644=CARTESIAN_POINT('Ctrl Pts',(64.2626358475693,-59.5258438271314,-3.05312111372604));
#33645=CARTESIAN_POINT('Ctrl Pts',(64.2630923571199,-60.0000961870058,-3.07968167058906));
#33646=CARTESIAN_POINT('',(64.263,-60.,-2.));
#33647=CARTESIAN_POINT('',(64.263,-60.,-6.));
#33648=CARTESIAN_POINT('Origin',(60.,-60.,-2.));
#33649=CARTESIAN_POINT('Ctrl Pts',(64.2630923571199,-60.0000961870058,-3.07968167058906));
#33650=CARTESIAN_POINT('Ctrl Pts',(64.2632197548392,-60.1324453765281,-3.08709390186401));
#33651=CARTESIAN_POINT('Ctrl Pts',(64.2571731981271,-60.264782898732,-3.09450613313896));
#33652=CARTESIAN_POINT('Ctrl Pts',(64.2448651421447,-60.396535440406,-3.10191836441391));
#33653=CARTESIAN_POINT('Ctrl Pts',(64.1801515414727,-61.0892672074344,-3.14089057704434));
#33654=CARTESIAN_POINT('Ctrl Pts',(63.9423405435201,-61.7658273512139,-3.17986278967477));
#33655=CARTESIAN_POINT('Ctrl Pts',(63.5593783222426,-62.3466916938238,-3.2188350023052));
#33656=CARTESIAN_POINT('Ctrl Pts',(63.1764161009651,-62.9275560364337,-3.25780721493563));
#33657=CARTESIAN_POINT('Ctrl Pts',(62.6483026563626,-63.4127245778742,-3.29677942756606));
#33658=CARTESIAN_POINT('Ctrl Pts',(62.037118094178,-63.7451676100945,-3.33575164019649));
#33659=CARTESIAN_POINT('Ctrl Pts',(61.4259335319934,-64.0776106423148,-3.37472385282692));
#33660=CARTESIAN_POINT('Ctrl Pts',(60.7316778522266,-64.257328165315,-3.41369606545735));
#33661=CARTESIAN_POINT('Ctrl Pts',(60.03595543146,-64.2631957584035,-3.45266827808778));
#33662=CARTESIAN_POINT('Ctrl Pts',(59.3402330106934,-64.269063351492,-3.49164049071821));
#33663=CARTESIAN_POINT('Ctrl Pts',(58.6430438489269,-64.1010810146688,-3.53061270334864));
#33664=CARTESIAN_POINT('Ctrl Pts',(58.0263393834232,-63.7789939606085,-3.56958491597907));
#33665=CARTESIAN_POINT('Ctrl Pts',(57.4096349179195,-63.4569069065482,-3.6085571286095));
#33666=CARTESIAN_POINT('Ctrl Pts',(56.8734151486786,-62.9807151352507,-3.64752934123993));
#33667=CARTESIAN_POINT('Ctrl Pts',(56.4807094070791,-62.4063924445202,-3.68650155387036));
#33668=CARTESIAN_POINT('Ctrl Pts',(56.0880036654796,-61.8320697537898,-3.72547376650079));
#33669=CARTESIAN_POINT('Ctrl Pts',(55.8388119515216,-61.1596161436264,-3.76444597913122));
#33670=CARTESIAN_POINT('Ctrl Pts',(55.7624255353169,-60.4680747538138,-3.80341819176165));
#33671=CARTESIAN_POINT('Ctrl Pts',(55.6860391191123,-59.7765333640012,-3.84239040439208));
#33672=CARTESIAN_POINT('Ctrl Pts',(55.7824580006609,-59.0659041945396,-3.88136261702251));
#33673=CARTESIAN_POINT('Ctrl Pts',(56.0403485787269,-58.4197178343383,-3.92033482965294));
#33674=CARTESIAN_POINT('Ctrl Pts',(56.298239156793,-57.7735314741371,-3.95930704228337));
#33675=CARTESIAN_POINT('Ctrl Pts',(56.7176014313765,-57.1917879231964,-3.9982792549138));
#33676=CARTESIAN_POINT('Ctrl Pts',(57.2491417753782,-56.7428678065456,-4.03725146754423));
#33677=CARTESIAN_POINT('Ctrl Pts',(57.7806821193799,-56.2939476898949,-4.07622368017466));
#33678=CARTESIAN_POINT('Ctrl Pts',(58.4244005327997,-55.977851007534,-4.11519589280509));
#33679=CARTESIAN_POINT('Ctrl Pts',(59.1046313480008,-55.8317333957891,-4.15416810543552));
#33680=CARTESIAN_POINT('Ctrl Pts',(59.7848621632019,-55.6856157840441,-4.19314031806595));
#33681=CARTESIAN_POINT('Ctrl Pts',(60.5016053801842,-55.709477242915,-4.23211253069638));
#33682=CARTESIAN_POINT('Ctrl Pts',(61.1706120606455,-55.9005125186762,-4.27108474332681));
#33683=CARTESIAN_POINT('Ctrl Pts',(61.8396187411067,-56.0915477944374,-4.31005695595724));
#33684=CARTESIAN_POINT('Ctrl Pts',(62.4608888850469,-56.4497568870889,-4.34902916858767));
#33685=CARTESIAN_POINT('Ctrl Pts',(62.9613950792328,-56.9330353155764,-4.3880013812181));
#33686=CARTESIAN_POINT('Ctrl Pts',(63.4619012734186,-57.4163137440639,-4.42697359384853));
#33687=CARTESIAN_POINT('Ctrl Pts',(63.8416435178501,-58.0246615083876,-4.46594580647895));
#33688=CARTESIAN_POINT('Ctrl Pts',(64.0559863899328,-58.6865685071185,-4.50491801910938));
#33689=CARTESIAN_POINT('Ctrl Pts',(64.1930503363015,-59.1098323390043,-4.52983923626927));
#33690=CARTESIAN_POINT('Ctrl Pts',(64.262480725507,-59.5549971097538,-4.55476045342917));
#33691=CARTESIAN_POINT('Ctrl Pts',(64.262772575926,-60.0000736173382,-4.57968167058906));
#33692=CARTESIAN_POINT('Origin',(60.,-60.,-6.));
#33693=CARTESIAN_POINT('',(64.2626973681969,-59.9946117577646,-6.07968167058905));
#33694=CARTESIAN_POINT('',(64.2632169240698,-60.0000544407254,-5.67031832941094));
#33695=CARTESIAN_POINT('',(64.263,-60.,-6.));
#33696=CARTESIAN_POINT('Ctrl Pts',(64.2632169240698,-60.0000544407254,-5.67031832941094));
#33697=CARTESIAN_POINT('Ctrl Pts',(64.2626871719434,-59.4158863751755,-5.63760089747675));
#33698=CARTESIAN_POINT('Ctrl Pts',(64.1414983098939,-58.8315462195081,-5.60488346554256));
#33699=CARTESIAN_POINT('Ctrl Pts',(63.9080437096925,-58.2961477521629,-5.57216603360837));
#33700=CARTESIAN_POINT('Ctrl Pts',(63.6299582432996,-57.65839406314,-5.53319382097794));
#33701=CARTESIAN_POINT('Ctrl Pts',(63.1925789493251,-57.0900837233481,-5.49422160834751));
#33702=CARTESIAN_POINT('Ctrl Pts',(62.6472141694011,-56.6580726270348,-5.45524939571708));
#33703=CARTESIAN_POINT('Ctrl Pts',(62.1018493894771,-56.2260615307214,-5.41627718308665));
#33704=CARTESIAN_POINT('Ctrl Pts',(61.4484991236035,-55.9303496778867,-5.37730497045622));
#33705=CARTESIAN_POINT('Ctrl Pts',(60.7640088680538,-55.805671270223,-5.33833275782579));
#33706=CARTESIAN_POINT('Ctrl Pts',(60.0795186125042,-55.6809928625592,-5.29936054519536));
#33707=CARTESIAN_POINT('Ctrl Pts',(59.3638883672783,-55.7273479000665,-5.26038833256493));
#33708=CARTESIAN_POINT('Ctrl Pts',(58.7012143744383,-55.9392992230255,-5.2214161199345));
#33709=CARTESIAN_POINT('Ctrl Pts',(58.0385403815983,-56.1512505459845,-5.18244390730407));
#33710=CARTESIAN_POINT('Ctrl Pts',(57.428822641144,-56.5287981543954,-5.14347169467364));
#33711=CARTESIAN_POINT('Ctrl Pts',(56.9437403484681,-57.0275580359404,-5.10449948204321));
#33712=CARTESIAN_POINT('Ctrl Pts',(56.4586580557921,-57.5263179174854,-5.06552726941278));
#33713=CARTESIAN_POINT('Ctrl Pts',(56.0982112108944,-58.1462900721645,-5.02655505678235));
#33714=CARTESIAN_POINT('Ctrl Pts',(55.9047635971807,-58.8146026972723,-4.98758284415192));
#33715=CARTESIAN_POINT('Ctrl Pts',(55.711315983467,-59.4829153223801,-4.94861063152149));
#33716=CARTESIAN_POINT('Ctrl Pts',(55.6848676009373,-60.1995684179167,-4.90963841889106));
#33717=CARTESIAN_POINT('Ctrl Pts',(55.8285295105432,-60.8803222262535,-4.87066620626063));
#33718=CARTESIAN_POINT('Ctrl Pts',(55.972191420149,-61.5610760345903,-4.8316939936302));
#33719=CARTESIAN_POINT('Ctrl Pts',(56.2859636218904,-62.2059305557273,-4.79272178099977));
#33720=CARTESIAN_POINT('Ctrl Pts',(56.7329629091576,-62.7390872440468,-4.75374956836934));
#33721=CARTESIAN_POINT('Ctrl Pts',(57.1799621964249,-63.2722439323662,-4.71477735573891));
#33722=CARTESIAN_POINT('Ctrl Pts',(57.7601885692179,-63.693702787868,-4.67580514310848));
#33723=CARTESIAN_POINT('Ctrl Pts',(58.4054401079131,-63.9539234102185,-4.63683293047805));
#33724=CARTESIAN_POINT('Ctrl Pts',(59.0506916466083,-64.214144032569,-4.59786071784762));
#33725=CARTESIAN_POINT('Ctrl Pts',(59.7609683512056,-64.3131264217682,-4.55888850521719));
#33726=CARTESIAN_POINT('Ctrl Pts',(60.4527808941947,-64.239235855233,-4.51991629258676));
#33727=CARTESIAN_POINT('Ctrl Pts',(61.1445934371838,-64.1653452886979,-4.48094407995633));
#33728=CARTESIAN_POINT('Ctrl Pts',(61.8179418185646,-63.9185817664285,-4.4419718673259));
#33729=CARTESIAN_POINT('Ctrl Pts',(62.393677796486,-63.527950932842,-4.40299965469547));
#33730=CARTESIAN_POINT('Ctrl Pts',(62.9694137744075,-63.1373200992555,-4.36402744206504));
#33731=CARTESIAN_POINT('Ctrl Pts',(63.4475373488694,-62.6028219543521,-4.32505522943461));
#33732=CARTESIAN_POINT('Ctrl Pts',(63.7718476256499,-61.9872837956534,-4.28608301680418));
#33733=CARTESIAN_POINT('Ctrl Pts',(64.0929625540898,-61.377810381043,-4.2474947876731));
#33734=CARTESIAN_POINT('Ctrl Pts',(64.263280221346,-60.6888860196627,-4.20890655854202));
#33735=CARTESIAN_POINT('Ctrl Pts',(64.2633463740757,-59.9999932305335,-4.17031832941094));
#33736=CARTESIAN_POINT('Ctrl Pts',(64.262772575926,-60.0000736173382,-4.57968167058906));
#33737=CARTESIAN_POINT('Ctrl Pts',(64.2629371260315,-60.2510151324331,-4.5937326660596));
#33738=CARTESIAN_POINT('Ctrl Pts',(64.2411232856546,-60.5019285896265,-4.60778366153014));
#33739=CARTESIAN_POINT('Ctrl Pts',(64.1970613151823,-60.7488728385771,-4.62183465700067));
#33740=CARTESIAN_POINT('Ctrl Pts',(64.0748498686155,-61.4338039381665,-4.6608068696311));
#33741=CARTESIAN_POINT('Ctrl Pts',(63.7814834757479,-62.0881999042072,-4.69977908226153));
#33742=CARTESIAN_POINT('Ctrl Pts',(63.3514512075064,-62.6351299077276,-4.73875129489196));
#33743=CARTESIAN_POINT('Ctrl Pts',(62.9214189392649,-63.1820599112481,-4.77772350752239));
#33744=CARTESIAN_POINT('Ctrl Pts',(62.3547207956494,-63.6215239522483,-4.81669572015282));
#33745=CARTESIAN_POINT('Ctrl Pts',(61.7179571845381,-63.9018875004117,-4.85566793278325));
#33746=CARTESIAN_POINT('Ctrl Pts',(61.0811935734268,-64.1822510485752,-4.89464014541368));
#33747=CARTESIAN_POINT('Ctrl Pts',(60.3743644948197,-64.3035141039018,-4.93361235804411));
#33748=CARTESIAN_POINT('Ctrl Pts',(59.6805793190517,-64.2513752851793,-4.97258457067454));
#33749=CARTESIAN_POINT('Ctrl Pts',(58.9867941432837,-64.1992364664568,-5.01155678330497));
#33750=CARTESIAN_POINT('Ctrl Pts',(58.3060528703548,-63.9736957736851,-5.0505289959354));
#33751=CARTESIAN_POINT('Ctrl Pts',(57.7183177603327,-63.6013669799594,-5.08950120856583));
#33752=CARTESIAN_POINT('Ctrl Pts',(57.1305826503106,-63.2290381862337,-5.12847342119626));
#33753=CARTESIAN_POINT('Ctrl Pts',(56.6358537031954,-62.7099212915541,-5.16744563382669));
#33754=CARTESIAN_POINT('Ctrl Pts',(56.2924025713763,-62.1048137589543,-5.20641784645712));
#33755=CARTESIAN_POINT('Ctrl Pts',(55.9489514395571,-61.4997062263544,-5.24539005908755));
#33756=CARTESIAN_POINT('Ctrl Pts',(55.756778123034,-60.8086080558343,-5.28436227171798));
#33757=CARTESIAN_POINT('Ctrl Pts',(55.7382146651663,-60.1132326609549,-5.32333448434841));
#33758=CARTESIAN_POINT('Ctrl Pts',(55.7196512072987,-59.4178572660755,-5.36230669697884));
#33759=CARTESIAN_POINT('Ctrl Pts',(55.8746976080865,-58.7182046468368,-5.40127890960927));
#33760=CARTESIAN_POINT('Ctrl Pts',(56.1856839927028,-58.095480130689,-5.4402511222397));
#33761=CARTESIAN_POINT('Ctrl Pts',(56.4966703773191,-57.4727556145412,-5.47922333487013));
#33762=CARTESIAN_POINT('Ctrl Pts',(56.9635967457639,-56.9269592014842,-5.51819554750056));
#33763=CARTESIAN_POINT('Ctrl Pts',(57.5303812800693,-56.5244725420488,-5.55716776013099));
#33764=CARTESIAN_POINT('Ctrl Pts',(58.0971658143748,-56.1219858826134,-5.59613997276142));
#33765=CARTESIAN_POINT('Ctrl Pts',(58.7638085145408,-55.8628089767996,-5.63511218539185));
#33766=CARTESIAN_POINT('Ctrl Pts',(59.4545507191691,-55.772604446058,-5.67408439802228));
#33767=CARTESIAN_POINT('Ctrl Pts',(60.1452929237973,-55.6823999153164,-5.71305661065271));
#33768=CARTESIAN_POINT('Ctrl Pts',(60.8601346328878,-55.761167759647,-5.75202882328314));
#33769=CARTESIAN_POINT('Ctrl Pts',(61.5092342355577,-56.009115703567,-5.79100103591357));
#33770=CARTESIAN_POINT('Ctrl Pts',(62.8074334408974,-56.5050115914071,-5.86894546117443));
#33771=CARTESIAN_POINT('Ctrl Pts',(63.8426642205549,-57.6776278776046,-5.94688988643529));
#33772=CARTESIAN_POINT('Ctrl Pts',(64.1576092650939,-59.0258076707621,-6.02483431169615));
#33773=CARTESIAN_POINT('Ctrl Pts',(64.2314820012626,-59.3420334120301,-6.04311676466045));
#33774=CARTESIAN_POINT('Ctrl Pts',(64.2657266032027,-59.6679181731568,-6.06139921762475));
#33775=CARTESIAN_POINT('Ctrl Pts',(64.2626973681969,-59.9946117577646,-6.07968167058905));
#33776=CARTESIAN_POINT('Origin',(60.,-60.,-6.));
#33777=CARTESIAN_POINT('',(64.2628730310814,-59.999902186829,-7.57968167058906));
#33778=CARTESIAN_POINT('',(64.2625444778277,-60.0004819773136,-7.17031832941094));
#33779=CARTESIAN_POINT('',(64.263,-60.,-6.));
#33780=CARTESIAN_POINT('Ctrl Pts',(64.2625444778277,-60.0004819773136,-7.17031832941094));
#33781=CARTESIAN_POINT('Ctrl Pts',(64.2617098238277,-59.5354191820522,-7.14423966167234));
#33782=CARTESIAN_POINT('Ctrl Pts',(64.1851000643309,-59.0702106162843,-7.11816099393373));
#33783=CARTESIAN_POINT('Ctrl Pts',(64.0358045844181,-58.6286233477238,-7.09208232619513));
#33784=CARTESIAN_POINT('Ctrl Pts',(63.8126959790919,-57.9687110739172,-7.0531101135647));
#33785=CARTESIAN_POINT('Ctrl Pts',(63.4272612479163,-57.3615513028208,-7.01413790093427));
#33786=CARTESIAN_POINT('Ctrl Pts',(62.9188673674461,-56.8879014639496,-6.97516568830384));
#33787=CARTESIAN_POINT('Ctrl Pts',(61.9020796065058,-55.9406017862071,-6.89722126304298));
#33788=CARTESIAN_POINT('Ctrl Pts',(60.3934552483873,-55.5273418373652,-6.81927683778212));
#33789=CARTESIAN_POINT('Ctrl Pts',(59.0443044051678,-55.8381001101711,-6.74133241252126));
#33790=CARTESIAN_POINT('Ctrl Pts',(57.6951535619483,-56.1488583829769,-6.6633879872604));
#33791=CARTESIAN_POINT('Ctrl Pts',(56.5054762336278,-57.1836348774304,-6.58544356199954));
#33792=CARTESIAN_POINT('Ctrl Pts',(56.01072650476,-58.476693811765,-6.50749913673868));
#33793=CARTESIAN_POINT('Ctrl Pts',(55.5159767758922,-59.7697527460996,-6.42955471147783));
#33794=CARTESIAN_POINT('Ctrl Pts',(55.7161546464771,-61.3210941203152,-6.35161028621697));
#33795=CARTESIAN_POINT('Ctrl Pts',(56.5133859887326,-62.4593630767463,-6.27366586095611));
#33796=CARTESIAN_POINT('Ctrl Pts',(56.9120016598604,-63.0284975549619,-6.23469364832568));
#33797=CARTESIAN_POINT('Ctrl Pts',(57.4598806989058,-63.4943639287313,-6.19572143569525));
#33798=CARTESIAN_POINT('Ctrl Pts',(58.0825013140338,-63.8067822836796,-6.15674922306482));
#33799=CARTESIAN_POINT('Ctrl Pts',(58.7051219291619,-64.1192006386278,-6.11777701043439));
#33800=CARTESIAN_POINT('Ctrl Pts',(59.4024841203727,-64.2781709747548,-6.07880479780396));
#33801=CARTESIAN_POINT('Ctrl Pts',(60.0974621223944,-64.2624885664828,-6.03983258517353));
#33802=CARTESIAN_POINT('Ctrl Pts',(60.7924401244162,-64.2468061582107,-6.0008603725431));
#33803=CARTESIAN_POINT('Ctrl Pts',(61.4850339372488,-64.0564710055396,-5.96188815991267));
#33804=CARTESIAN_POINT('Ctrl Pts',(62.0915941530894,-63.7150284794136,-5.92291594728224));
#33805=CARTESIAN_POINT('Ctrl Pts',(62.6981543689299,-63.3735859532875,-5.88394373465181));
#33806=CARTESIAN_POINT('Ctrl Pts',(63.2186809877783,-62.8810360537067,-5.84497152202138));
#33807=CARTESIAN_POINT('Ctrl Pts',(63.5930284383828,-62.2947293311775,-5.80599930939095));
#33808=CARTESIAN_POINT('Ctrl Pts',(63.9673758889872,-61.7084226086483,-5.76702709676052));
#33809=CARTESIAN_POINT('Ctrl Pts',(64.1955441713478,-61.0283590631708,-5.72805488413009));
#33810=CARTESIAN_POINT('Ctrl Pts',(64.2502324931223,-60.3347287713052,-5.68908267149966));
#33811=CARTESIAN_POINT('Ctrl Pts',(64.2590096047169,-60.2234057268317,-5.68282789080342));
#33812=CARTESIAN_POINT('Ctrl Pts',(64.2633181998478,-60.1117332285689,-5.67657311010718));
#33813=CARTESIAN_POINT('Ctrl Pts',(64.2632169240698,-60.0000544407254,-5.67031832941094));
#33814=CARTESIAN_POINT('Ctrl Pts',(64.2626973681969,-59.9946117577646,-6.07968167058905));
#33815=CARTESIAN_POINT('Ctrl Pts',(64.2528119258362,-61.0607260058028,-6.13934364288561));
#33816=CARTESIAN_POINT('Ctrl Pts',(63.8459814397295,-62.1354537612865,-6.19900561518217));
#33817=CARTESIAN_POINT('Ctrl Pts',(63.1240242614618,-62.9112261865645,-6.25866758747873));
#33818=CARTESIAN_POINT('Ctrl Pts',(62.1808349038704,-63.924721609092,-6.33661201273959));
#33819=CARTESIAN_POINT('Ctrl Pts',(60.6997968792671,-64.4279691540293,-6.41455643800045));
#33820=CARTESIAN_POINT('Ctrl Pts',(59.3267918264532,-64.2132809306245,-6.49250086326131));
#33821=CARTESIAN_POINT('Ctrl Pts',(58.6402893000462,-64.1059368189221,-6.53147307589174));
#33822=CARTESIAN_POINT('Ctrl Pts',(57.9807950165867,-63.8191087651342,-6.57044528852217));
#33823=CARTESIAN_POINT('Ctrl Pts',(57.4261724663064,-63.3976167992062,-6.6094175011526));
#33824=CARTESIAN_POINT('Ctrl Pts',(56.8715499160262,-62.9761248332783,-6.64838971378303));
#33825=CARTESIAN_POINT('Ctrl Pts',(56.4217990989253,-62.4199689552105,-6.68736192641346));
#33826=CARTESIAN_POINT('Ctrl Pts',(56.1299141641273,-61.7890621441924,-6.72633413904389));
#33827=CARTESIAN_POINT('Ctrl Pts',(55.8380292293292,-61.1581553331743,-6.76530635167432));
#33828=CARTESIAN_POINT('Ctrl Pts',(55.7040101768341,-60.4524975892059,-6.80427856430475));
#33829=CARTESIAN_POINT('Ctrl Pts',(55.7435429828512,-59.7575619722766,-6.84325077693518));
#33830=CARTESIAN_POINT('Ctrl Pts',(55.7830757888683,-59.0626263553473,-6.88222298956561));
#33831=CARTESIAN_POINT('Ctrl Pts',(55.9961604533976,-58.3784128654571,-6.92119520219604));
#33832=CARTESIAN_POINT('Ctrl Pts',(56.3577826811561,-57.7841730938475,-6.96016741482647));
#33833=CARTESIAN_POINT('Ctrl Pts',(56.7194049089147,-57.1899333222379,-6.9991396274569));
#33834=CARTESIAN_POINT('Ctrl Pts',(57.2295646999025,-56.685667268909,-7.03811184008733));
#33835=CARTESIAN_POINT('Ctrl Pts',(57.828280682058,-56.3311916298766,-7.07708405271776));
#33836=CARTESIAN_POINT('Ctrl Pts',(58.4269966642135,-55.9767159908442,-7.11605626534819));
#33837=CARTESIAN_POINT('Ctrl Pts',(59.1142688375368,-55.7720307661083,-7.15502847797862));
#33838=CARTESIAN_POINT('Ctrl Pts',(59.8093191217818,-55.7409439109291,-7.19400069060904));
#33839=CARTESIAN_POINT('Ctrl Pts',(60.5043694060268,-55.70985705575,-7.23297290323947));
#33840=CARTESIAN_POINT('Ctrl Pts',(61.2071978011936,-55.8523685701277,-7.2719451158699));
#33841=CARTESIAN_POINT('Ctrl Pts',(61.8351875089724,-56.1518435330984,-7.31091732850033));
#33842=CARTESIAN_POINT('Ctrl Pts',(62.4631772167512,-56.4513184960691,-7.34988954113076));
#33843=CARTESIAN_POINT('Ctrl Pts',(63.016328237142,-56.9077569076329,-7.38886175376119));
#33844=CARTESIAN_POINT('Ctrl Pts',(63.4296222200028,-57.4674529852744,-7.42783396639163));
#33845=CARTESIAN_POINT('Ctrl Pts',(63.8429162028636,-58.0271490629158,-7.46680617902206));
#33846=CARTESIAN_POINT('Ctrl Pts',(64.1163531481944,-58.6901028066351,-7.50577839165248));
#33847=CARTESIAN_POINT('Ctrl Pts',(64.2177913673386,-59.3784126701003,-7.54475060428291));
#33848=CARTESIAN_POINT('Ctrl Pts',(64.2480979620442,-59.5840583156947,-7.55639429305163));
#33849=CARTESIAN_POINT('Ctrl Pts',(64.2630514496097,-59.7919673223717,-7.56803798182034));
#33850=CARTESIAN_POINT('Ctrl Pts',(64.2628730310814,-59.999902186829,-7.57968167058906));
#33851=CARTESIAN_POINT('Origin',(60.,-60.,-6.));
#33852=CARTESIAN_POINT('',(64.2632129993401,-59.9999237120662,-9.07968167058906));
#33853=CARTESIAN_POINT('',(64.2626697207193,-59.9999992453659,-8.67031832941094));
#33854=CARTESIAN_POINT('',(64.263,-60.,-6.));
#33855=CARTESIAN_POINT('',(56.7766472160421,-57.2101674189746,-10.));
#33856=CARTESIAN_POINT('Ctrl Pts',(64.2632129993401,-59.9999237120662,-9.07968167058906));
#33857=CARTESIAN_POINT('Ctrl Pts',(64.2627031276559,-60.6063764566768,-9.11364895864636));
#33858=CARTESIAN_POINT('Ctrl Pts',(64.1318733554661,-61.2130420411853,-9.14761624670366));
#33859=CARTESIAN_POINT('Ctrl Pts',(63.8808238845651,-61.7650315954715,-9.18158353476097));
#33860=CARTESIAN_POINT('Ctrl Pts',(63.5927834221001,-62.3983542865008,-9.2205557473914));
#33861=CARTESIAN_POINT('Ctrl Pts',(63.1464855643694,-62.9597013677154,-9.25952796002183));
#33862=CARTESIAN_POINT('Ctrl Pts',(62.5943907479285,-63.3830862528202,-9.29850017265226));
#33863=CARTESIAN_POINT('Ctrl Pts',(62.0422959314875,-63.8064711379249,-9.33747238528269));
#33864=CARTESIAN_POINT('Ctrl Pts',(61.3844041563363,-64.0918938269197,-9.37644459791312));
#33865=CARTESIAN_POINT('Ctrl Pts',(60.6980457544028,-64.2058117593792,-9.41541681054355));
#33866=CARTESIAN_POINT('Ctrl Pts',(60.0116873524693,-64.3197296918386,-9.45438902317398));
#33867=CARTESIAN_POINT('Ctrl Pts',(59.2968623237536,-64.2621428677627,-9.49336123580441));
#33868=CARTESIAN_POINT('Ctrl Pts',(58.6375973345399,-64.0398048735937,-9.53233344843484));
#33869=CARTESIAN_POINT('Ctrl Pts',(57.9783323453263,-63.8174668794247,-9.57130566106527));
#33870=CARTESIAN_POINT('Ctrl Pts',(57.3746273956147,-63.4303777151625,-9.6102778736957));
#33871=CARTESIAN_POINT('Ctrl Pts',(56.8974398008335,-62.9240723226063,-9.64925008632613));
#33872=CARTESIAN_POINT('Ctrl Pts',(56.4202522060524,-62.4177669300501,-9.68822229895656));
#33873=CARTESIAN_POINT('Ctrl Pts',(56.0695819662017,-61.7922453091999,-9.72719451158699));
#33874=CARTESIAN_POINT('Ctrl Pts',(55.8866652661684,-61.1209648644822,-9.76616672421742));
#33875=CARTESIAN_POINT('Ctrl Pts',(55.703748566135,-60.4496844197645,-9.80513893684785));
#33876=CARTESIAN_POINT('Ctrl Pts',(55.6885854059191,-59.7326451511795,-9.84411114947828));
#33877=CARTESIAN_POINT('Ctrl Pts',(55.8429525213217,-59.0543161036114,-9.88308336210871));
#33878=CARTESIAN_POINT('Ctrl Pts',(55.9973196367243,-58.3759870560434,-9.92205557473914));
#33879=CARTESIAN_POINT('Ctrl Pts',(56.3212170277455,-57.7363682294923,-9.96102778736957));
#33880=CARTESIAN_POINT('Ctrl Pts',(56.7766472160421,-57.2101674189746,-10.));
#33881=CARTESIAN_POINT('',(63.2235668665311,-57.2100812780843,-10.));
#33882=CARTESIAN_POINT('Origin',(60.,-60.,-10.));
#33883=CARTESIAN_POINT('Ctrl Pts',(63.2235668665311,-57.2100812780843,-10.));
#33884=CARTESIAN_POINT('Ctrl Pts',(62.8262376065631,-56.7517870228408,-9.96602721186203));
#33885=CARTESIAN_POINT('Ctrl Pts',(62.3301929068535,-56.3786504290086,-9.93205442372406));
#33886=CARTESIAN_POINT('Ctrl Pts',(61.7790228098056,-56.125571221051,-9.89808163558608));
#33887=CARTESIAN_POINT('Ctrl Pts',(61.1467426998997,-55.8352489588686,-9.85910942295565));
#33888=CARTESIAN_POINT('Ctrl Pts',(60.441918927478,-55.7029192537276,-9.82013721032522));
#33889=CARTESIAN_POINT('Ctrl Pts',(59.7473945386634,-55.7441420953322,-9.78116499769479));
#33890=CARTESIAN_POINT('Ctrl Pts',(59.0528701498489,-55.7853649369367,-9.74219278506436));
#33891=CARTESIAN_POINT('Ctrl Pts',(58.3686451446415,-56.0001403252867,-9.70322057243393));
#33892=CARTESIAN_POINT('Ctrl Pts',(57.7751487508423,-56.3632201670063,-9.6642483598035));
#33893=CARTESIAN_POINT('Ctrl Pts',(57.1816523570431,-56.7263000087259,-9.62527614717308));
#33894=CARTESIAN_POINT('Ctrl Pts',(56.6788845746522,-57.2376843038151,-9.58630393454264));
#33895=CARTESIAN_POINT('Ctrl Pts',(56.325941879404,-57.8372637991282,-9.54733172191221));
#33896=CARTESIAN_POINT('Ctrl Pts',(55.9729991841559,-58.4368432944413,-9.50835950928178));
#33897=CARTESIAN_POINT('Ctrl Pts',(55.7698815760507,-59.1246179899783,-9.46938729665135));
#33898=CARTESIAN_POINT('Ctrl Pts',(55.7404649130753,-59.8197432519075,-9.43041508402093));
#33899=CARTESIAN_POINT('Ctrl Pts',(55.7110482500999,-60.5148685138366,-9.39144287139049));
#33900=CARTESIAN_POINT('Ctrl Pts',(55.8553325322544,-61.217344342158,-9.35247065876006));
#33901=CARTESIAN_POINT('Ctrl Pts',(56.156357704853,-61.8445988379219,-9.31349844612963));
#33902=CARTESIAN_POINT('Ctrl Pts',(56.4573828774516,-62.4718533336857,-9.2745262334992));
#33903=CARTESIAN_POINT('Ctrl Pts',(56.9151489404942,-63.023886496892,-9.23555402086877));
#33904=CARTESIAN_POINT('Ctrl Pts',(57.475848139259,-63.4358097682661,-9.19658180823834));
#33905=CARTESIAN_POINT('Ctrl Pts',(58.0365473380239,-63.8477330396401,-9.15760959560792));
#33906=CARTESIAN_POINT('Ctrl Pts',(58.700179672511,-64.1195464191819,-9.11863738297749));
#33907=CARTESIAN_POINT('Ctrl Pts',(59.3887387787435,-64.2192998103684,-9.07966517034706));
#33908=CARTESIAN_POINT('Ctrl Pts',(60.0772978849761,-64.3190532015549,-9.04069295771663));
#33909=CARTESIAN_POINT('Ctrl Pts',(60.7907837629541,-64.2467466043861,-9.0017207450862));
#33910=CARTESIAN_POINT('Ctrl Pts',(61.445330135215,-64.0108792149673,-8.96274853245577));
#33911=CARTESIAN_POINT('Ctrl Pts',(62.0998765074759,-63.7750118255484,-8.92377631982534));
#33912=CARTESIAN_POINT('Ctrl Pts',(62.6954833740198,-63.3755836438795,-8.88480410719491));
#33913=CARTESIAN_POINT('Ctrl Pts',(63.1621404033453,-62.859545295653,-8.84583189456448));
#33914=CARTESIAN_POINT('Ctrl Pts',(63.6287974326707,-62.3435069474265,-8.80685968193405));
#33915=CARTESIAN_POINT('Ctrl Pts',(63.9665046247778,-61.7108584326424,-8.76788746930362));
#33916=CARTESIAN_POINT('Ctrl Pts',(64.1355664404059,-61.0359639838401,-8.72891525667318));
#33917=CARTESIAN_POINT('Ctrl Pts',(64.2202977762693,-60.6977166510445,-8.70938294758577));
#33918=CARTESIAN_POINT('Ctrl Pts',(64.2626675966367,-60.3488576914975,-8.68985063849835));
#33919=CARTESIAN_POINT('Ctrl Pts',(64.2626697207193,-59.9999992453659,-8.67031832941094));
#33920=CARTESIAN_POINT('Origin',(60.,-60.,-13.3123464956316));
#33921=CARTESIAN_POINT('',(65.0994143001201,-59.9999919030003,-3.68765350436841));
#33922=CARTESIAN_POINT('',(65.0991104689079,-60.0001150498576,-3.56234649563159));
#33923=CARTESIAN_POINT('',(65.099,-60.,-13.3123464956316));
#33924=CARTESIAN_POINT('',(56.3967816198432,-56.392144916311,-3.));
#33925=CARTESIAN_POINT('Ctrl Pts',(65.0991104689079,-60.0001150498576,-3.56234649563159));
#33926=CARTESIAN_POINT('Ctrl Pts',(65.0984616565564,-59.3260858024822,-3.53078651427611));
#33927=CARTESIAN_POINT('Ctrl Pts',(64.7978132229132,-57.8191582297671,-3.4602543202902));
#33928=CARTESIAN_POINT('Ctrl Pts',(63.355584325901,-55.888083148428,-3.35074991367387));
#33929=CARTESIAN_POINT('Ctrl Pts',(61.0270447294087,-54.7929300306235,-3.23383327578258));
#33930=CARTESIAN_POINT('Ctrl Pts',(58.4567444358424,-54.9220255059251,-3.11691663789129));
#33931=CARTESIAN_POINT('Ctrl Pts',(56.9857510552447,-55.8039324061735,-3.03897221263043));
#33932=CARTESIAN_POINT('Ctrl Pts',(56.3967816198431,-56.3921449163111,-3.));
#33933=CARTESIAN_POINT('',(55.0736213077518,-58.683468118019,-3.));
#33934=CARTESIAN_POINT('Origin',(60.,-60.,-3.));
#33935=CARTESIAN_POINT('Ctrl Pts',(65.0994143001201,-59.9999919030003,-3.68765350436841));
#33936=CARTESIAN_POINT('Ctrl Pts',(65.0994150874834,-59.9917925604302,-3.68726952086906));
#33937=CARTESIAN_POINT('Ctrl Pts',(65.0974290916723,-59.151405440399,-3.64791332473929));
#33938=CARTESIAN_POINT('Ctrl Pts',(64.6714138259177,-57.4808672112921,-3.56958491597907));
#33939=CARTESIAN_POINT('Ctrl Pts',(62.9373243124707,-55.5795635648098,-3.45266827808779));
#33940=CARTESIAN_POINT('Ctrl Pts',(60.5127057471208,-54.7174568009332,-3.3357516401965));
#33941=CARTESIAN_POINT('Ctrl Pts',(57.9675484622588,-55.0972147578633,-3.21883500230521));
#33942=CARTESIAN_POINT('Ctrl Pts',(55.9886141307795,-56.5640444741926,-3.10691778890637));
#33943=CARTESIAN_POINT('Ctrl Pts',(55.2615313586432,-57.9827262758446,-3.03397278813797));
#33944=CARTESIAN_POINT('Ctrl Pts',(55.0736213077518,-58.683468118019,-3.));
#33945=CARTESIAN_POINT('Origin',(60.,-60.,-13.3123464956316));
#33946=CARTESIAN_POINT('',(65.0992594641877,-60.00006511688,-5.18765350436841));
#33947=CARTESIAN_POINT('',(65.098727976694,-60.000088054142,-5.06234649563159));
#33948=CARTESIAN_POINT('',(65.099,-60.,-13.3123464956316));
#33949=CARTESIAN_POINT('Ctrl Pts',(65.098727976694,-60.000088054142,-5.06234649563159));
#33950=CARTESIAN_POINT('Ctrl Pts',(65.0983788926485,-59.4677293602239,-5.0374252784717));
#33951=CARTESIAN_POINT('Ctrl Pts',(64.885463906226,-58.1025886458417,-4.97353184868138));
#33952=CARTESIAN_POINT('Ctrl Pts',(63.6865889957319,-56.1819888648126,-4.87066620626063));
#33953=CARTESIAN_POINT('Ctrl Pts',(61.4572741020296,-54.8966206991336,-4.75374956836934));
#33954=CARTESIAN_POINT('Ctrl Pts',(58.885371453618,-54.8109981947122,-4.63683293047805));
#33955=CARTESIAN_POINT('Ctrl Pts',(56.5755050285457,-55.9452536369063,-4.51991629258676));
#33956=CARTESIAN_POINT('Ctrl Pts',(55.0706997941323,-58.0327345420765,-4.40299965469547));
#33957=CARTESIAN_POINT('Ctrl Pts',(54.7247181776535,-60.582698043192,-4.28608301680418));
#33958=CARTESIAN_POINT('Ctrl Pts',(55.6188973116942,-62.9956754944399,-4.16916637891289));
#33959=CARTESIAN_POINT('Ctrl Pts',(57.5430244076546,-64.704403039722,-4.0522497410216));
#33960=CARTESIAN_POINT('Ctrl Pts',(60.0447608860831,-65.3071770970488,-3.93533310313031));
#33961=CARTESIAN_POINT('Ctrl Pts',(62.5359710979979,-64.6622934589222,-3.81841646523902));
#33962=CARTESIAN_POINT('Ctrl Pts',(64.4310101226481,-62.9213544069835,-3.70149982734774));
#33963=CARTESIAN_POINT('Ctrl Pts',(65.0540042410307,-61.148967957511,-3.61614317081192));
#33964=CARTESIAN_POINT('Ctrl Pts',(65.099262850088,-60.158418713328,-3.56975872690654));
#33965=CARTESIAN_POINT('Ctrl Pts',(65.0991104689079,-60.0001150498576,-3.56234649563159));
#33966=CARTESIAN_POINT('Ctrl Pts',(65.0992594641877,-60.00006511688,-5.18765350436841));
#33967=CARTESIAN_POINT('Ctrl Pts',(65.0986258244756,-59.3013381719494,-5.15493607243422));
#33968=CARTESIAN_POINT('Ctrl Pts',(64.7810045336314,-57.7698535833796,-5.0832464278696));
#33969=CARTESIAN_POINT('Ctrl Pts',(63.2955109178121,-55.8396721751708,-4.97258457067455));
#33970=CARTESIAN_POINT('Ctrl Pts',(60.9510823423798,-54.7785639854422,-4.85566793278326));
#33971=CARTESIAN_POINT('Ctrl Pts',(58.3831733906512,-54.9449006048999,-4.73875129489197));
#33972=CARTESIAN_POINT('Ctrl Pts',(56.1953121953125,-56.2996615164319,-4.62183465700068));
#33973=CARTESIAN_POINT('Ctrl Pts',(54.9019142627768,-58.5243188117934,-4.50491801910939));
#33974=CARTESIAN_POINT('Ctrl Pts',(54.8070090534039,-61.0958980757912,-4.3880013812181));
#33975=CARTESIAN_POINT('Ctrl Pts',(55.932923519751,-63.4098412167327,-4.27108474332681));
#33976=CARTESIAN_POINT('Ctrl Pts',(58.0149603071344,-64.9221696503736,-4.15416810543553));
#33977=CARTESIAN_POINT('Ctrl Pts',(60.5636590522025,-65.2773499477182,-4.03725146754423));
#33978=CARTESIAN_POINT('Ctrl Pts',(62.9798472271926,-64.3918839378294,-3.92033482965295));
#33979=CARTESIAN_POINT('Ctrl Pts',(64.6898720416353,-62.4802336033169,-3.803802175261));
#33980=CARTESIAN_POINT('Ctrl Pts',(65.0993351744413,-60.8239807211494,-3.72624173349949));
#33981=CARTESIAN_POINT('Ctrl Pts',(65.0994143001201,-59.9999919030003,-3.68765350436841));
#33982=CARTESIAN_POINT('Origin',(60.,-60.,-13.3123464956316));
#33983=CARTESIAN_POINT('',(65.0984551471835,-60.0005764959704,-6.68765350436841));
#33984=CARTESIAN_POINT('',(65.0986380202759,-59.9935550909786,-6.56234649563159));
#33985=CARTESIAN_POINT('',(65.099,-60.,-13.3123464956316));
#33986=CARTESIAN_POINT('Ctrl Pts',(65.0986380202759,-59.9935550909786,-6.56234649563159));
#33987=CARTESIAN_POINT('Ctrl Pts',(65.1022613065284,-59.6027949249183,-6.54406404266729));
#33988=CARTESIAN_POINT('Ctrl Pts',(64.8866737284852,-57.5511808779631,-6.44783716444213));
#33989=CARTESIAN_POINT('Ctrl Pts',(62.7388651753224,-55.1183365899423,-6.31263807358654));
#33990=CARTESIAN_POINT('Ctrl Pts',(59.3187592643186,-54.7414778160817,-6.15674922306481));
#33991=CARTESIAN_POINT('Ctrl Pts',(56.9266332065095,-55.6714869946495,-6.03983258517353));
#33992=CARTESIAN_POINT('Ctrl Pts',(55.2511528738565,-57.6299781348164,-5.92291594728223));
#33993=CARTESIAN_POINT('Ctrl Pts',(54.6947970697628,-60.1405542822466,-5.80599930939095));
#33994=CARTESIAN_POINT('Ctrl Pts',(55.3843760570615,-62.6204343466251,-5.68908267149966));
#33995=CARTESIAN_POINT('Ctrl Pts',(57.159620885591,-64.483190888477,-5.57216603360837));
#33996=CARTESIAN_POINT('Ctrl Pts',(59.6023371070298,-65.292502635446,-5.45524939571708));
#33997=CARTESIAN_POINT('Ctrl Pts',(62.1386646734039,-64.8573722208712,-5.33833275782579));
#33998=CARTESIAN_POINT('Ctrl Pts',(64.1721578713598,-63.2804354544672,-5.2214161199345));
#33999=CARTESIAN_POINT('Ctrl Pts',(65.0004645952953,-61.4327780814141,-5.1294206992031));
#34000=CARTESIAN_POINT('Ctrl Pts',(65.0989247960673,-60.3002407131776,-5.07639749110213));
#34001=CARTESIAN_POINT('Ctrl Pts',(65.098727976694,-60.000088054142,-5.06234649563159));
#34002=CARTESIAN_POINT('Ctrl Pts',(65.0984551471835,-60.0005764959704,-6.68765350436841));
#34003=CARTESIAN_POINT('Ctrl Pts',(65.0974568125024,-59.4443120828723,-6.66157483662981));
#34004=CARTESIAN_POINT('Ctrl Pts',(64.8688855876321,-58.0563258472263,-6.59652395626078));
#34005=CARTESIAN_POINT('Ctrl Pts',(63.1773262290866,-55.3916806820179,-6.45352865063089));
#34006=CARTESIAN_POINT('Ctrl Pts',(58.6661395049216,-54.1559238915272,-6.25866758747873));
#34007=CARTESIAN_POINT('Ctrl Pts',(54.3971988313774,-57.8690311013926,-6.02483431169616));
#34008=CARTESIAN_POINT('Ctrl Pts',(54.9957837258839,-62.5079530267534,-5.82997324854401));
#34009=CARTESIAN_POINT('Ctrl Pts',(57.6170694121072,-64.7368553395382,-5.67408439802229));
#34010=CARTESIAN_POINT('Ctrl Pts',(60.1194267752203,-65.3072914717773,-5.557167760131));
#34011=CARTESIAN_POINT('Ctrl Pts',(62.6046736799591,-64.6243084010734,-5.44025112223971));
#34012=CARTESIAN_POINT('Ctrl Pts',(64.4724887605417,-62.8568826882213,-5.32333448434842));
#34013=CARTESIAN_POINT('Ctrl Pts',(65.0621164699687,-61.0994766787787,-5.23913527839132));
#34014=CARTESIAN_POINT('Ctrl Pts',(65.0993806007563,-60.1336447882883,-5.19390828506465));
#34015=CARTESIAN_POINT('Ctrl Pts',(65.0992594641877,-60.00006511688,-5.18765350436841));
#34016=CARTESIAN_POINT('Origin',(60.,-60.,-13.3123464956316));
#34017=CARTESIAN_POINT('',(65.0986049509612,-59.9999990973777,-8.18765350436841));
#34018=CARTESIAN_POINT('',(65.0988481317111,-59.9998830050765,-8.06234649563159));
#34019=CARTESIAN_POINT('',(65.099,-60.,-13.3123464956316));
#34020=CARTESIAN_POINT('Ctrl Pts',(65.0988481317111,-59.9998830050765,-8.06234649563159));
#34021=CARTESIAN_POINT('Ctrl Pts',(65.0990615391883,-59.7511708601392,-8.05070280686288));
#34022=CARTESIAN_POINT('Ctrl Pts',(65.0213100778608,-58.6701368189858,-8.00008690546373));
#34023=CARTESIAN_POINT('Ctrl Pts',(64.2694756589632,-56.8472981310306,-7.91049879143416));
#34024=CARTESIAN_POINT('Ctrl Pts',(62.2845938482857,-55.2094519237375,-7.79358215354287));
#34025=CARTESIAN_POINT('Ctrl Pts',(59.7626220066562,-54.6980752792535,-7.67666551565158));
#34026=CARTESIAN_POINT('Ctrl Pts',(57.2964708372155,-55.4325509730806,-7.55974887776029));
#34027=CARTESIAN_POINT('Ctrl Pts',(55.4658552325379,-57.2420179723235,-7.442832239869));
#34028=CARTESIAN_POINT('Ctrl Pts',(54.701239676989,-59.6971936126827,-7.32591560197771));
#34029=CARTESIAN_POINT('Ctrl Pts',(55.1821426669066,-62.2293180577881,-7.20899896408642));
#34030=CARTESIAN_POINT('Ctrl Pts',(56.7959916580377,-64.2249822536134,-7.09208232619513));
#34031=CARTESIAN_POINT('Ctrl Pts',(59.9512920111792,-65.5972893108641,-6.93619347567341));
#34032=CARTESIAN_POINT('Ctrl Pts',(63.964474637114,-64.2336347183845,-6.75961486548557));
#34033=CARTESIAN_POINT('Ctrl Pts',(65.0868139830726,-61.2687407702531,-6.62200846792815));
#34034=CARTESIAN_POINT('Ctrl Pts',(65.0986380202759,-59.9935550909786,-6.56234649563159));
#34035=CARTESIAN_POINT('Ctrl Pts',(65.0986049509612,-59.9999990973777,-8.18765350436841));
#34036=CARTESIAN_POINT('Ctrl Pts',(65.0986074795697,-59.5847014805283,-8.1682136008254));
#34037=CARTESIAN_POINT('Ctrl Pts',(64.9477827615392,-58.3368363840766,-8.10980148465195));
#34038=CARTESIAN_POINT('Ctrl Pts',(63.9406234799139,-56.4447764036095,-8.01241715584808));
#34039=CARTESIAN_POINT('Ctrl Pts',(61.8050635175092,-55.0090188089158,-7.89550051795678));
#34040=CARTESIAN_POINT('Ctrl Pts',(59.2451498180026,-54.7465902155457,-7.7785838800655));
#34041=CARTESIAN_POINT('Ctrl Pts',(56.8627001404056,-55.7191702005741,-7.66166724217421));
#34042=CARTESIAN_POINT('Ctrl Pts',(55.217779590162,-57.6981472392852,-7.54475060428292));
#34043=CARTESIAN_POINT('Ctrl Pts',(54.6971392178688,-60.21821824206,-7.42783396639163));
#34044=CARTESIAN_POINT('Ctrl Pts',(55.4230712207726,-62.6870881580822,-7.31091732850034));
#34045=CARTESIAN_POINT('Ctrl Pts',(57.2251428783372,-64.5240383042407,-7.19400069060906));
#34046=CARTESIAN_POINT('Ctrl Pts',(59.6792195378112,-65.2979014573777,-7.07708405271776));
#34047=CARTESIAN_POINT('Ctrl Pts',(62.2094281655486,-64.8252835759928,-6.96016741482648));
#34048=CARTESIAN_POINT('Ctrl Pts',(64.2186727163164,-63.2204586132884,-6.84325077693518));
#34049=CARTESIAN_POINT('Ctrl Pts',(65.0118135613323,-61.3817369404773,-6.7524128067825));
#34050=CARTESIAN_POINT('Ctrl Pts',(65.09894873348,-60.2755989876827,-6.70054704926024));
#34051=CARTESIAN_POINT('Ctrl Pts',(65.0984551471835,-60.0005764959704,-6.68765350436841));
#34052=CARTESIAN_POINT('Origin',(60.,-60.,-13.3123464956316));
#34053=CARTESIAN_POINT('',(65.0987893869763,-59.9998803238954,-9.68765350436841));
#34054=CARTESIAN_POINT('',(65.0992547697948,-59.9999087515425,-9.56234649563159));
#34055=CARTESIAN_POINT('',(65.099,-60.,-13.3123464956316));
#34056=CARTESIAN_POINT('',(61.322884965569,-64.9244061944433,-10.));
#34057=CARTESIAN_POINT('Ctrl Pts',(61.322884965569,-64.9244061944433,-10.));
#34058=CARTESIAN_POINT('Ctrl Pts',(62.1267766598728,-64.7084499564018,-9.96102778736957));
#34059=CARTESIAN_POINT('Ctrl Pts',(63.6260271020141,-63.8754856296126,-9.88308336210871));
#34060=CARTESIAN_POINT('Ctrl Pts',(64.8700259293115,-61.9507383889051,-9.77896786356485));
#34061=CARTESIAN_POINT('Ctrl Pts',(65.0983672591983,-60.5589068688162,-9.71382457765142));
#34062=CARTESIAN_POINT('Ctrl Pts',(65.0987893869763,-59.9998803238954,-9.68765350436841));
#34063=CARTESIAN_POINT('',(58.6769607093948,-64.9246350255102,-10.));
#34064=CARTESIAN_POINT('Origin',(60.,-60.,-10.));
#34065=CARTESIAN_POINT('Ctrl Pts',(58.6769607093948,-64.9246350255102,-10.));
#34066=CARTESIAN_POINT('Ctrl Pts',(59.3777759715939,-65.1122710698436,-9.96602721186203));
#34067=CARTESIAN_POINT('Ctrl Pts',(60.9699318324407,-65.1919398158278,-9.89308221109363));
#34068=CARTESIAN_POINT('Ctrl Pts',(63.2297107943118,-64.2115472768226,-9.78116499769479));
#34069=CARTESIAN_POINT('Ctrl Pts',(64.7626148130399,-62.283482461386,-9.66925328437663));
#34070=CARTESIAN_POINT('Ctrl Pts',(65.0986449091995,-60.7252905354434,-9.5963137836889));
#34071=CARTESIAN_POINT('Ctrl Pts',(65.0992547697949,-59.9999087515425,-9.56234649563159));
#34072=CARTESIAN_POINT('Origin',(-60.,-60.,-6.));
#34073=CARTESIAN_POINT('',(-55.7372274017113,-60.0000736188739,-4.57968167058906));
#34074=CARTESIAN_POINT('',(-55.7366536901661,-59.9999932304475,-4.17031832941095));
#34075=CARTESIAN_POINT('',(-55.737,-60.,-6.));
#34076=CARTESIAN_POINT('',(-59.1956105045055,-64.1864216867795,-3.));
#34077=CARTESIAN_POINT('Ctrl Pts',(-55.7366536901661,-59.9999932304475,
-4.17031832941095));
#34078=CARTESIAN_POINT('Ctrl Pts',(-55.7366530318933,-59.9931382006682,
-4.1699343459116));
#34079=CARTESIAN_POINT('Ctrl Pts',(-55.7366692316342,-59.9862831740153,
-4.16955036241225));
#34080=CARTESIAN_POINT('Ctrl Pts',(-55.7367023085573,-59.9794282288035,
-4.1691663789129));
#34081=CARTESIAN_POINT('Ctrl Pts',(-55.7400594342771,-59.2836890035115,
-4.13019416628247));
#34082=CARTESIAN_POINT('Ctrl Pts',(-55.9172706620175,-58.5887887151182,
-4.09122195365204));
#34083=CARTESIAN_POINT('Ctrl Pts',(-56.2475061214605,-57.9764089332034,
-4.05224974102161));
#34084=CARTESIAN_POINT('Ctrl Pts',(-56.5777415809036,-57.3640291512886,
-4.01327752839118));
#34085=CARTESIAN_POINT('Ctrl Pts',(-57.0610012720493,-56.8341698758524,
-3.97430531576075));
#34086=CARTESIAN_POINT('Ctrl Pts',(-57.6404800019574,-56.4491133816137,
-3.93533310313032));
#34087=CARTESIAN_POINT('Ctrl Pts',(-58.2199587318654,-56.064056887375,-3.89636089049989));
#34088=CARTESIAN_POINT('Ctrl Pts',(-58.8956565005358,-55.8238031743338,
-3.85738867786946));
#34089=CARTESIAN_POINT('Ctrl Pts',(-59.5881502622955,-55.7565921866708,
-3.81841646523903));
#34090=CARTESIAN_POINT('Ctrl Pts',(-60.2806440240553,-55.6893811990077,
-3.7794442526086));
#34091=CARTESIAN_POINT('Ctrl Pts',(-60.9899337789045,-55.7952129367229,
-3.74047203997817));
#34092=CARTESIAN_POINT('Ctrl Pts',(-61.632643243836,-56.0616486298365,-3.70149982734774));
#34093=CARTESIAN_POINT('Ctrl Pts',(-62.2753527087675,-56.32808432295,-3.66252761471731));
#34094=CARTESIAN_POINT('Ctrl Pts',(-62.8514818837812,-56.7551239714621,
-3.62355540208688));
#34095=CARTESIAN_POINT('Ctrl Pts',(-63.2933169034021,-57.2925688095136,
-3.58458318945645));
#34096=CARTESIAN_POINT('Ctrl Pts',(-63.7351519230229,-57.8300136475652,
-3.54561097682602));
#34097=CARTESIAN_POINT('Ctrl Pts',(-64.0426927872508,-58.4778636751564,
-3.50663876419559));
#34098=CARTESIAN_POINT('Ctrl Pts',(-64.1797749238076,-59.1599729097974,
-3.46766655156516));
#34099=CARTESIAN_POINT('Ctrl Pts',(-64.3168570603643,-59.8420821444384,
-3.42869433893473));
#34100=CARTESIAN_POINT('Ctrl Pts',(-64.2834804692498,-60.5584505861292,
-3.3897221263043));
#34101=CARTESIAN_POINT('Ctrl Pts',(-64.0836009345363,-61.224859865863,-3.35074991367387));
#34102=CARTESIAN_POINT('Ctrl Pts',(-63.8837213998229,-61.8912691455967,
-3.31177770104344));
#34103=CARTESIAN_POINT('Ctrl Pts',(-63.5173389215105,-62.5077192633734,
-3.27280548841301));
#34104=CARTESIAN_POINT('Ctrl Pts',(-63.0274513378467,-63.001770094789,-3.23383327578258));
#34105=CARTESIAN_POINT('Ctrl Pts',(-62.537563754183,-63.4958209262046,-3.19486106315215));
#34106=CARTESIAN_POINT('Ctrl Pts',(-61.9241710651678,-63.8674724712591,
-3.15588885052172));
#34107=CARTESIAN_POINT('Ctrl Pts',(-61.2595373436356,-64.0729510882669,
-3.11691663789129));
#34108=CARTESIAN_POINT('Ctrl Pts',(-60.5949036221034,-64.2784297052747,
-3.07794442526086));
#34109=CARTESIAN_POINT('Ctrl Pts',(-59.8790288680541,-64.3177353942359,
-3.03897221263043));
#34110=CARTESIAN_POINT('Ctrl Pts',(-59.1956105045054,-64.1864216867795,
-3.));
#34111=CARTESIAN_POINT('',(-55.9720760639888,-58.6032685615972,-3.));
#34112=CARTESIAN_POINT('Origin',(-60.,-60.,-3.));
#34113=CARTESIAN_POINT('',(-55.7369076166092,-60.0000961895604,-3.07968167058906));
#34114=CARTESIAN_POINT('Ctrl Pts',(-55.9720760639888,-58.6032685615972,
-3.));
#34115=CARTESIAN_POINT('Ctrl Pts',(-55.8170962955876,-59.0514416515873,
-3.02656055686302));
#34116=CARTESIAN_POINT('Ctrl Pts',(-55.737364127205,-59.5258438267831,-3.05312111372604));
#34117=CARTESIAN_POINT('Ctrl Pts',(-55.7369076166092,-60.0000961895604,
-3.07968167058906));
#34118=CARTESIAN_POINT('',(-55.737,-60.,-2.));
#34119=CARTESIAN_POINT('',(-55.737,-60.,-6.));
#34120=CARTESIAN_POINT('Origin',(-60.,-60.,-2.));
#34121=CARTESIAN_POINT('Ctrl Pts',(-55.7369076166092,-60.0000961895604,
-3.07968167058906));
#34122=CARTESIAN_POINT('Ctrl Pts',(-55.7367802185982,-60.1324453798928,
-3.08709390186401));
#34123=CARTESIAN_POINT('Ctrl Pts',(-55.7428267750975,-60.2647829028978,
-3.09450613313897));
#34124=CARTESIAN_POINT('Ctrl Pts',(-55.7551348310466,-60.396535445299,-3.10191836441392));
#34125=CARTESIAN_POINT('Ctrl Pts',(-55.8198484315432,-61.0892672161508,
-3.14089057704435));
#34126=CARTESIAN_POINT('Ctrl Pts',(-56.0576594342791,-61.7658273617105,
-3.17986278967478));
#34127=CARTESIAN_POINT('Ctrl Pts',(-56.4406216586579,-62.3466917067985,
-3.21883500230521));
#34128=CARTESIAN_POINT('Ctrl Pts',(-56.8235838830368,-62.9275560518864,
-3.25780721493564));
#34129=CARTESIAN_POINT('Ctrl Pts',(-57.3516973290586,-63.4127245965028,
-3.29677942756607));
#34130=CARTESIAN_POINT('Ctrl Pts',(-57.9628818942373,-63.7451676306387,
-3.3357516401965));
#34131=CARTESIAN_POINT('Ctrl Pts',(-58.574066459416,-64.0776106647747,-3.37472385282693));
#34132=CARTESIAN_POINT('Ctrl Pts',(-59.2683221437516,-64.2573281884304,
-3.41369606545736));
#34133=CARTESIAN_POINT('Ctrl Pts',(-59.9640445684965,-64.2631957814501,
-3.45266827808779));
#34134=CARTESIAN_POINT('Ctrl Pts',(-60.6597669932415,-64.2690633744698,
-3.49164049071822));
#34135=CARTESIAN_POINT('Ctrl Pts',(-61.3569561583957,-64.1010810368534,
-3.53061270334865));
#34136=CARTESIAN_POINT('Ctrl Pts',(-61.9736606271436,-63.7789939810841,
-3.56958491597907));
#34137=CARTESIAN_POINT('Ctrl Pts',(-62.5903650958916,-63.4569069253149,
-3.60855712860951));
#34138=CARTESIAN_POINT('Ctrl Pts',(-63.1265848682333,-62.9807151513927,
-3.64752934123993));
#34139=CARTESIAN_POINT('Ctrl Pts',(-63.5192906120051,-62.4063924575338,
-3.68650155387036));
#34140=CARTESIAN_POINT('Ctrl Pts',(-63.9119963557769,-61.8320697636749,
-3.72547376650079));
#34141=CARTESIAN_POINT('Ctrl Pts',(-64.1611880709788,-61.1596161498792,
-3.76444597913122));
#34142=CARTESIAN_POINT('Ctrl Pts',(-64.2375744875774,-60.4680747563421,
-3.80341819176165));
#34143=CARTESIAN_POINT('Ctrl Pts',(-64.313960904176,-59.776533362805,-3.84239040439208));
#34144=CARTESIAN_POINT('Ctrl Pts',(-64.2175420221713,-59.0659041895265,
-3.88136261702251));
#34145=CARTESIAN_POINT('Ctrl Pts',(-63.9596514427128,-58.4197178258067,
-3.92033482965294));
#34146=CARTESIAN_POINT('Ctrl Pts',(-63.7017608632543,-57.773531462087,-3.95930704228337));
#34147=CARTESIAN_POINT('Ctrl Pts',(-63.282398586342,-57.1917879079259,-3.9982792549138));
#34148=CARTESIAN_POINT('Ctrl Pts',(-62.7508582394783,-56.7428677888888,
-4.03725146754424));
#34149=CARTESIAN_POINT('Ctrl Pts',(-62.2193178926146,-56.2939476698518,
-4.07622368017466));
#34150=CARTESIAN_POINT('Ctrl Pts',(-61.5755994757997,-55.9778509859388,
-4.1151958928051));
#34151=CARTESIAN_POINT('Ctrl Pts',(-60.895368656883,-55.8317333733196,-4.15416810543553));
#34152=CARTESIAN_POINT('Ctrl Pts',(-60.2151378379662,-55.6856157607004,
-4.19314031806596));
#34153=CARTESIAN_POINT('Ctrl Pts',(-59.4983946169477,-55.7094772193751,
-4.23211253069638));
#34154=CARTESIAN_POINT('Ctrl Pts',(-58.8293879329443,-55.9005124963388,
-4.27108474332681));
#34155=CARTESIAN_POINT('Ctrl Pts',(-58.1603812489408,-56.0915477733025,
-4.31005695595724));
#34156=CARTESIAN_POINT('Ctrl Pts',(-57.5391111019523,-56.4497568685552,
-4.34902916858767));
#34157=CARTESIAN_POINT('Ctrl Pts',(-57.0386049049034,-56.9330352993155,
-4.3880013812181));
#34158=CARTESIAN_POINT('Ctrl Pts',(-56.5380987078546,-57.4163137300757,
-4.42697359384853));
#34159=CARTESIAN_POINT('Ctrl Pts',(-56.1583564607454,-58.0246614963435,
-4.46594580647896));
#34160=CARTESIAN_POINT('Ctrl Pts',(-55.944013587813,-58.6865684993411,-4.50491801910939));
#34161=CARTESIAN_POINT('Ctrl Pts',(-55.8069496409009,-59.1098323339553,
-4.52983923626928));
#34162=CARTESIAN_POINT('Ctrl Pts',(-55.7375192518995,-59.5549971083828,
-4.55476045342917));
#34163=CARTESIAN_POINT('Ctrl Pts',(-55.7372274017113,-60.0000736188739,
-4.57968167058906));
#34164=CARTESIAN_POINT('Origin',(-60.,-60.,-6.));
#34165=CARTESIAN_POINT('',(-55.7373026458209,-59.9946120201631,-6.07968167058906));
#34166=CARTESIAN_POINT('',(-55.7367829988534,-60.0000543459286,-5.67031832941095));
#34167=CARTESIAN_POINT('',(-55.737,-60.,-6.));
#34168=CARTESIAN_POINT('Ctrl Pts',(-55.7367829988534,-60.0000543459286,
-5.67031832941095));
#34169=CARTESIAN_POINT('Ctrl Pts',(-55.7373127458066,-59.4158862842898,
-5.63760089747676));
#34170=CARTESIAN_POINT('Ctrl Pts',(-55.8585017631583,-58.8315462413849,
-5.60488346554257));
#34171=CARTESIAN_POINT('Ctrl Pts',(-56.091956403473,-58.296147811699,-5.57216603360838));
#34172=CARTESIAN_POINT('Ctrl Pts',(-56.370041917648,-57.658394167535,-5.53319382097794));
#34173=CARTESIAN_POINT('Ctrl Pts',(-56.8074210959631,-57.0900837660379,
-5.49422160834752));
#34174=CARTESIAN_POINT('Ctrl Pts',(-57.3527858412086,-56.6580726588936,
-5.45524939571708));
#34175=CARTESIAN_POINT('Ctrl Pts',(-57.8981505864541,-56.2260615517493,
-5.41627718308665));
#34176=CARTESIAN_POINT('Ctrl Pts',(-58.5515008986299,-55.9303497389577,
-5.37730497045622));
#34177=CARTESIAN_POINT('Ctrl Pts',(-59.235991157749,-55.8056713421077,-5.33833275782579));
#34178=CARTESIAN_POINT('Ctrl Pts',(-59.9204814168682,-55.6809929452577,
-5.29936054519536));
#34179=CARTESIAN_POINT('Ctrl Pts',(-60.6361116229307,-55.7273479643494,
-5.26038833256493));
#34180=CARTESIAN_POINT('Ctrl Pts',(-61.2987855987603,-55.9392992796723,
-5.2214161199345));
#34181=CARTESIAN_POINT('Ctrl Pts',(-61.9614595745898,-56.1512505949953,
-5.18244390730407));
#34182=CARTESIAN_POINT('Ctrl Pts',(-62.5711773201864,-56.5287982065494,
-5.14347169467364));
#34183=CARTESIAN_POINT('Ctrl Pts',(-63.0562596091439,-57.0275580828228,
-5.10449948204321));
#34184=CARTESIAN_POINT('Ctrl Pts',(-63.5413418981015,-57.5263179590961,
-5.06552726941278));
#34185=CARTESIAN_POINT('Ctrl Pts',(-63.90178873042,-58.1462901000886,-5.02655505678236));
#34186=CARTESIAN_POINT('Ctrl Pts',(-64.0952363394269,-58.8146027140363,
-4.98758284415193));
#34187=CARTESIAN_POINT('Ctrl Pts',(-64.2886839484338,-59.4829153279839,
-4.9486106315215));
#34188=CARTESIAN_POINT('Ctrl Pts',(-64.315132334129,-60.1995684148867,-4.90963841889107));
#34189=CARTESIAN_POINT('Ctrl Pts',(-64.171470427582,-60.880322213531,-4.87066620626064));
#34190=CARTESIAN_POINT('Ctrl Pts',(-64.0278085210349,-61.5610760121754,
-4.83169399363021));
#34191=CARTESIAN_POINT('Ctrl Pts',(-63.7140363222456,-62.2059305225613,
-4.79272178099978));
#34192=CARTESIAN_POINT('Ctrl Pts',(-63.2670370412591,-62.7390872025879,
-4.75374956836935));
#34193=CARTESIAN_POINT('Ctrl Pts',(-62.8200377602726,-63.2722438826145,
-4.71477735573892));
#34194=CARTESIAN_POINT('Ctrl Pts',(-62.2398113970889,-63.6937027322818,
-4.67580514310849));
#34195=CARTESIAN_POINT('Ctrl Pts',(-61.5945598683159,-63.9539233508557,
-4.63683293047806));
#34196=CARTESIAN_POINT('Ctrl Pts',(-60.949308339543,-64.2141439694296,-4.59786071784763));
#34197=CARTESIAN_POINT('Ctrl Pts',(-60.2390316451808,-64.3131263569101,
-4.5588885052172));
#34198=CARTESIAN_POINT('Ctrl Pts',(-59.5472191125019,-64.2392357914097,
-4.51991629258677));
#34199=CARTESIAN_POINT('Ctrl Pts',(-58.855406579823,-64.1653452259092,-4.48094407995634));
#34200=CARTESIAN_POINT('Ctrl Pts',(-58.1820582088273,-63.9185817074278,
-4.44197186732591));
#34201=CARTESIAN_POINT('Ctrl Pts',(-57.6063222395974,-63.5279508797756,
-4.40299965469548));
#34202=CARTESIAN_POINT('Ctrl Pts',(-57.0305862703675,-63.1373200521234,
-4.36402744206505));
#34203=CARTESIAN_POINT('Ctrl Pts',(-56.5524627029033,-62.6028219153003,
-4.32505522943462));
#34204=CARTESIAN_POINT('Ctrl Pts',(-56.2281524310208,-61.9872837657933,
-4.28608301680419));
#34205=CARTESIAN_POINT('Ctrl Pts',(-55.9070375074305,-61.3778103602842,
-4.24749478767311));
#34206=CARTESIAN_POINT('Ctrl Pts',(-55.7367198429653,-60.6888860090946,
-4.20890655854203));
#34207=CARTESIAN_POINT('Ctrl Pts',(-55.7366536901661,-59.9999932304475,
-4.17031832941095));
#34208=CARTESIAN_POINT('Ctrl Pts',(-55.7372274017113,-60.0000736188739,
-4.57968167058906));
#34209=CARTESIAN_POINT('Ctrl Pts',(-55.7370628517358,-60.2510151356077,
-4.5937326660596));
#34210=CARTESIAN_POINT('Ctrl Pts',(-55.7588766922514,-60.5019285941948,
-4.60778366153014));
#34211=CARTESIAN_POINT('Ctrl Pts',(-55.8029386627415,-60.7488728439853,
-4.62183465700068));
#34212=CARTESIAN_POINT('Ctrl Pts',(-55.9251501093579,-61.4338039459045,
-4.66080686963111));
#34213=CARTESIAN_POINT('Ctrl Pts',(-56.2185165013463,-62.0881999100153,
-4.69977908226154));
#34214=CARTESIAN_POINT('Ctrl Pts',(-56.6485487731059,-62.6351299192171,
-4.73875129489197));
#34215=CARTESIAN_POINT('Ctrl Pts',(-57.0785810448654,-63.182059928419,-4.7777235075224));
#34216=CARTESIAN_POINT('Ctrl Pts',(-57.6452791963962,-63.6215239827118,
-4.81669572015283));
#34217=CARTESIAN_POINT('Ctrl Pts',(-58.2820428086401,-63.9018875269744,
-4.85566793278326));
#34218=CARTESIAN_POINT('Ctrl Pts',(-58.9188064208841,-64.1822510712369,
-4.89464014541369));
#34219=CARTESIAN_POINT('Ctrl Pts',(-59.6256354938411,-64.3035141054693,
-4.93361235804412));
#34220=CARTESIAN_POINT('Ctrl Pts',(-60.3194206777223,-64.2513752968827,
-4.97258457067455));
#34221=CARTESIAN_POINT('Ctrl Pts',(-61.0132058616034,-64.1992364882962,
-5.01155678330498));
#34222=CARTESIAN_POINT('Ctrl Pts',(-61.6939471564087,-63.9736958368907,
-5.05052899593541));
#34223=CARTESIAN_POINT('Ctrl Pts',(-62.2816822612956,-63.6013670203114,
-5.08950120856584));
#34224=CARTESIAN_POINT('Ctrl Pts',(-62.8694173661825,-63.2290382037321,
-5.12847342119627));
#34225=CARTESIAN_POINT('Ctrl Pts',(-63.3641462811511,-62.709921221979,-5.1674456338267));
#34226=CARTESIAN_POINT('Ctrl Pts',(-63.707597429373,-62.1048137232406,-5.20641784645713));
#34227=CARTESIAN_POINT('Ctrl Pts',(-64.051048577595,-61.4997062245023,-5.24539005908756));
#34228=CARTESIAN_POINT('Ctrl Pts',(-64.2432219590703,-60.8086082087788,
-5.28436227171798));
#34229=CARTESIAN_POINT('Ctrl Pts',(-64.2617853890068,-60.1132327305904,
-5.32333448434842));
#34230=CARTESIAN_POINT('Ctrl Pts',(-64.2803488189434,-59.4178572524019,
-5.36230669697885));
#34231=CARTESIAN_POINT('Ctrl Pts',(-64.125302297341,-58.7182043117486,-5.40127890960928));
#34232=CARTESIAN_POINT('Ctrl Pts',(-63.8143159491228,-58.0954799012611,
-5.44025112223971));
#34233=CARTESIAN_POINT('Ctrl Pts',(-63.5033296009046,-57.4727554907737,
-5.47922333487014));
#34234=CARTESIAN_POINT('Ctrl Pts',(-63.0364034260706,-56.9269596104521,
-5.51819554750057));
#34235=CARTESIAN_POINT('Ctrl Pts',(-62.4696187992193,-56.5244726304014,
-5.557167760131));
#34236=CARTESIAN_POINT('Ctrl Pts',(-61.902834172368,-56.1219856503507,-5.59613997276143));
#34237=CARTESIAN_POINT('Ctrl Pts',(-61.2361910934994,-55.862807570571,-5.63511218539186));
#34238=CARTESIAN_POINT('Ctrl Pts',(-60.5454488737994,-55.7726030381307,
-5.67408439802229));
#34239=CARTESIAN_POINT('Ctrl Pts',(-59.8547066540995,-55.6823985056904,
-5.71305661065272));
#34240=CARTESIAN_POINT('Ctrl Pts',(-59.1398652935682,-55.7611675205897,
-5.75202882328315));
#34241=CARTESIAN_POINT('Ctrl Pts',(-58.4907658812686,-56.0091161201719,
-5.79100103591358));
#34242=CARTESIAN_POINT('Ctrl Pts',(-57.1925670566693,-56.5050133193363,
-5.86894546117443));
#34243=CARTESIAN_POINT('Ctrl Pts',(-56.1573360249965,-57.6776288572327,
-5.9468898864353));
#34244=CARTESIAN_POINT('Ctrl Pts',(-55.8423908354356,-59.0258082047619,
-6.02483431169616));
#34245=CARTESIAN_POINT('Ctrl Pts',(-55.7685180652509,-59.3420338415045,
-6.04311676466046));
#34246=CARTESIAN_POINT('Ctrl Pts',(-55.7342734351814,-59.667918514758,-6.06139921762476));
#34247=CARTESIAN_POINT('Ctrl Pts',(-55.7373026458209,-59.9946120201631,
-6.07968167058906));
#34248=CARTESIAN_POINT('Origin',(-60.,-60.,-6.));
#34249=CARTESIAN_POINT('',(-55.7371269462215,-59.9999021904687,-7.57968167058906));
#34250=CARTESIAN_POINT('',(-55.7374565106948,-60.0004827185225,-7.17031832941094));
#34251=CARTESIAN_POINT('',(-55.737,-60.,-6.));
#34252=CARTESIAN_POINT('Ctrl Pts',(-55.7374565106948,-60.0004827185225,
-7.17031832941094));
#34253=CARTESIAN_POINT('Ctrl Pts',(-55.7382921058495,-59.5354208239183,
-7.14423966167234));
#34254=CARTESIAN_POINT('Ctrl Pts',(-55.8149029736461,-59.070213340202,-7.11816099393374));
#34255=CARTESIAN_POINT('Ctrl Pts',(-55.9641984444257,-58.6286260986936,
-7.09208232619514));
#34256=CARTESIAN_POINT('Ctrl Pts',(-56.187307036103,-57.9687138653137,-7.05311011356471));
#34257=CARTESIAN_POINT('Ctrl Pts',(-56.572739258111,-57.3615517785553,-7.01413790093428));
#34258=CARTESIAN_POINT('Ctrl Pts',(-57.0811317284725,-56.8879006559434,
-6.97516568830384));
#34259=CARTESIAN_POINT('Ctrl Pts',(-58.0979166691954,-55.9405984107196,
-6.89722126304298));
#34260=CARTESIAN_POINT('Ctrl Pts',(-59.6065426033322,-55.5273400220822,
-6.81927683778213));
#34261=CARTESIAN_POINT('Ctrl Pts',(-60.9556943852598,-55.8380992060676,
-6.74133241252127));
#34262=CARTESIAN_POINT('Ctrl Pts',(-62.3048461671874,-56.148858390053,-6.66338798726041));
#34263=CARTESIAN_POINT('Ctrl Pts',(-63.4945237969059,-57.1836351466612,
-6.58544356199955));
#34264=CARTESIAN_POINT('Ctrl Pts',(-63.9892745582629,-58.4766948843557,
-6.50749913673869));
#34265=CARTESIAN_POINT('Ctrl Pts',(-64.48402531962,-59.7697546220501,-6.42955471147783));
#34266=CARTESIAN_POINT('Ctrl Pts',(-64.2838492126156,-61.3210973408307,
-6.35161028621697));
#34267=CARTESIAN_POINT('Ctrl Pts',(-63.4866149367798,-62.4593638601133,
-6.27366586095611));
#34268=CARTESIAN_POINT('Ctrl Pts',(-63.0879977988619,-63.0284971197546,
-6.23469364832568));
#34269=CARTESIAN_POINT('Ctrl Pts',(-62.5401161187362,-63.4943613295214,
-6.19572143569525));
#34270=CARTESIAN_POINT('Ctrl Pts',(-61.9174955417529,-63.8067796653494,
-6.15674922306482));
#34271=CARTESIAN_POINT('Ctrl Pts',(-61.2948749647697,-64.1191980011775,
-6.11777701043439));
#34272=CARTESIAN_POINT('Ctrl Pts',(-60.597515490929,-64.2781704630668,-6.07880479780396));
#34273=CARTESIAN_POINT('Ctrl Pts',(-59.9025382047836,-64.2624886515656,
-6.03983258517353));
#34274=CARTESIAN_POINT('Ctrl Pts',(-59.2075609186382,-64.2468068400645,
-6.0008603725431));
#34275=CARTESIAN_POINT('Ctrl Pts',(-58.5149658201879,-64.0564707551729,
-5.96188815991268));
#34276=CARTESIAN_POINT('Ctrl Pts',(-57.9084053535882,-63.7150280406438,
-5.92291594728225));
#34277=CARTESIAN_POINT('Ctrl Pts',(-57.3018448869884,-63.3735853261147,
-5.88394373465182));
#34278=CARTESIAN_POINT('Ctrl Pts',(-56.781319052239,-62.8810359819482,-5.84497152202138));
#34279=CARTESIAN_POINT('Ctrl Pts',(-56.4069717968208,-62.2947294084888,
-5.80599930939095));
#34280=CARTESIAN_POINT('Ctrl Pts',(-56.0326245414025,-61.7084228350294,
-5.76702709676052));
#34281=CARTESIAN_POINT('Ctrl Pts',(-55.8044558653154,-61.0283590322772,
-5.7280548841301));
#34282=CARTESIAN_POINT('Ctrl Pts',(-55.7497674522892,-60.3347286874856,
-5.68908267149967));
#34283=CARTESIAN_POINT('Ctrl Pts',(-55.7409903260494,-60.2234056345178,
-5.68282789080343));
#34284=CARTESIAN_POINT('Ctrl Pts',(-55.7366817240644,-60.1117331330244,
-5.67657311010719));
#34285=CARTESIAN_POINT('Ctrl Pts',(-55.7367829988534,-60.0000543459286,
-5.67031832941095));
#34286=CARTESIAN_POINT('Ctrl Pts',(-55.7373026458209,-59.9946120201631,
-6.07968167058906));
#34287=CARTESIAN_POINT('Ctrl Pts',(-55.7471880086661,-61.0607260097358,
-6.13934364288562));
#34288=CARTESIAN_POINT('Ctrl Pts',(-56.1540184553338,-62.1354535990912,
-6.19900561518218));
#34289=CARTESIAN_POINT('Ctrl Pts',(-56.8759755604507,-62.9112256731964,
-6.25866758747873));
#34290=CARTESIAN_POINT('Ctrl Pts',(-57.8191648224755,-63.9247206369396,
-6.33661201273959));
#34291=CARTESIAN_POINT('Ctrl Pts',(-59.3002026939739,-64.4279674072641,
-6.41455643800045));
#34292=CARTESIAN_POINT('Ctrl Pts',(-60.6732080679322,-64.2132805110372,
-6.49250086326132));
#34293=CARTESIAN_POINT('Ctrl Pts',(-61.3597107549114,-64.1059370629238,
-6.53147307589175));
#34294=CARTESIAN_POINT('Ctrl Pts',(-62.0192053175055,-63.8191101981725,
-6.57044528852218));
#34295=CARTESIAN_POINT('Ctrl Pts',(-62.5738278800212,-63.3976182232817,
-6.60941750115261));
#34296=CARTESIAN_POINT('Ctrl Pts',(-63.128450442537,-62.976126248391,-6.64838971378304));
#34297=CARTESIAN_POINT('Ctrl Pts',(-63.5782010049745,-62.4199691633608,
-6.68736192641346));
#34298=CARTESIAN_POINT('Ctrl Pts',(-63.8700858607814,-61.7890620281216,
-6.72633413904389));
#34299=CARTESIAN_POINT('Ctrl Pts',(-64.1619707165883,-61.1581548928825,
-6.76530635167432));
#34300=CARTESIAN_POINT('Ctrl Pts',(-64.2959898657645,-60.4524977074343,
-6.80427856430475));
#34301=CARTESIAN_POINT('Ctrl Pts',(-64.2564570806599,-59.7575622002848,
-6.84325077693518));
#34302=CARTESIAN_POINT('Ctrl Pts',(-64.2169242955553,-59.0626266931353,
-6.88222298956561));
#34303=CARTESIAN_POINT('Ctrl Pts',(-64.0038395761699,-58.3784128642844,
-6.92119520219604));
#34304=CARTESIAN_POINT('Ctrl Pts',(-63.6422173312568,-57.7841730064991,
-6.96016741482647));
#34305=CARTESIAN_POINT('Ctrl Pts',(-63.2805950863436,-57.1899331487137,
-6.9991396274569));
#34306=CARTESIAN_POINT('Ctrl Pts',(-62.7704353159028,-56.6856672619939,
-7.03811184008733));
#34307=CARTESIAN_POINT('Ctrl Pts',(-62.1717193363373,-56.3311916604974,
-7.07708405271776));
#34308=CARTESIAN_POINT('Ctrl Pts',(-61.5730033567719,-55.9767160590009,
-7.11605626534819));
#34309=CARTESIAN_POINT('Ctrl Pts',(-60.8857311680819,-55.7720307427277,
-7.15502847797862));
#34310=CARTESIAN_POINT('Ctrl Pts',(-60.190680876938,-55.7409438651642,-7.19400069060905));
#34311=CARTESIAN_POINT('Ctrl Pts',(-59.495630585794,-55.7098569876007,-7.23297290323948));
#34312=CARTESIAN_POINT('Ctrl Pts',(-58.7928021921962,-55.8523685487467,
-7.27194511586991));
#34313=CARTESIAN_POINT('Ctrl Pts',(-58.1648124824129,-56.1518435245449,
-7.31091732850034));
#34314=CARTESIAN_POINT('Ctrl Pts',(-57.5368227726295,-56.451318500343,-7.34988954113077));
#34315=CARTESIAN_POINT('Ctrl Pts',(-56.9836717466607,-56.9077568907933,
-7.3888617537612));
#34316=CARTESIAN_POINT('Ctrl Pts',(-56.5703777608788,-57.4674529656122,
-7.42783396639163));
#34317=CARTESIAN_POINT('Ctrl Pts',(-56.1570837750969,-58.0271490404312,
-7.46680617902206));
#34318=CARTESIAN_POINT('Ctrl Pts',(-55.8836468295019,-58.6901027996189,
-7.50577839165249));
#34319=CARTESIAN_POINT('Ctrl Pts',(-55.7822086101274,-59.3784126697627,
-7.54475060428292));
#34320=CARTESIAN_POINT('Ctrl Pts',(-55.7519020153531,-59.5840583173523,
-7.55639429305163));
#34321=CARTESIAN_POINT('Ctrl Pts',(-55.7369485277219,-59.7919673252401,
-7.56803798182035));
#34322=CARTESIAN_POINT('Ctrl Pts',(-55.7371269462215,-59.9999021904687,
-7.57968167058906));
#34323=CARTESIAN_POINT('Origin',(-60.,-60.,-6.));
#34324=CARTESIAN_POINT('',(-55.7367869775695,-59.9999237120217,-9.07968167058906));
#34325=CARTESIAN_POINT('',(-55.7373303432786,-59.9999992452069,-8.67031832941095));
#34326=CARTESIAN_POINT('',(-55.737,-60.,-6.));
#34327=CARTESIAN_POINT('',(-63.2233527839579,-57.2101674189746,-10.));
#34328=CARTESIAN_POINT('Ctrl Pts',(-55.7367869775695,-59.9999237120217,
-9.07968167058906));
#34329=CARTESIAN_POINT('Ctrl Pts',(-55.7372968491093,-60.6063764601996,
-9.11364895864637));
#34330=CARTESIAN_POINT('Ctrl Pts',(-55.8681266217369,-61.2130420485546,
-9.14761624670367));
#34331=CARTESIAN_POINT('Ctrl Pts',(-56.1191760941168,-61.7650316055626,
-9.18158353476097));
#34332=CARTESIAN_POINT('Ctrl Pts',(-56.4072165582787,-62.3983542997147,
-9.2205557473914));
#34333=CARTESIAN_POINT('Ctrl Pts',(-56.853514419077,-62.9597013825716,-9.25952796002183));
#34334=CARTESIAN_POINT('Ctrl Pts',(-57.4056092377689,-63.3830862709465,
-9.29850017265226));
#34335=CARTESIAN_POINT('Ctrl Pts',(-57.9577040564609,-63.8064711593214,
-9.33747238528269));
#34336=CARTESIAN_POINT('Ctrl Pts',(-58.6155958330465,-64.0918938532141,
-9.37644459791312));
#34337=CARTESIAN_POINT('Ctrl Pts',(-59.301954238806,-64.205811785771,-9.41541681054355));
#34338=CARTESIAN_POINT('Ctrl Pts',(-59.9883126445655,-64.3197297183279,
-9.45438902317399));
#34339=CARTESIAN_POINT('Ctrl Pts',(-60.7031376794989,-64.2621428895488,
-9.49336123580442));
#34340=CARTESIAN_POINT('Ctrl Pts',(-61.3624026668752,-64.039804899767,-9.53233344843485));
#34341=CARTESIAN_POINT('Ctrl Pts',(-62.0216676542516,-63.8174669099853,
-9.57130566106527));
#34342=CARTESIAN_POINT('Ctrl Pts',(-62.6253725940708,-63.4303777592007,
-9.6102778736957));
#34343=CARTESIAN_POINT('Ctrl Pts',(-63.1025601873701,-62.9240723675456,
-9.64925008632613));
#34344=CARTESIAN_POINT('Ctrl Pts',(-63.5797477806694,-62.4177669758905,
-9.68822229895656));
#34345=CARTESIAN_POINT('Ctrl Pts',(-63.9304180274487,-61.7922453433649,
-9.72719451158699));
#34346=CARTESIAN_POINT('Ctrl Pts',(-64.1133346946325,-61.1209649250503,
-9.76616672421742));
#34347=CARTESIAN_POINT('Ctrl Pts',(-64.2962513618163,-60.4496845067356,
-9.80513893684785));
#34348=CARTESIAN_POINT('Ctrl Pts',(-64.3114144494046,-59.7326453026318,
-9.84411114947828));
#34349=CARTESIAN_POINT('Ctrl Pts',(-64.1570473520141,-59.054316233321,-9.88308336210871));
#34350=CARTESIAN_POINT('Ctrl Pts',(-64.0026802546237,-58.3759871640102,
-9.92205557473914));
#34351=CARTESIAN_POINT('Ctrl Pts',(-63.6787829722545,-57.7363682294924,
-9.96102778736957));
#34352=CARTESIAN_POINT('Ctrl Pts',(-63.2233527839579,-57.2101674189746,
-10.));
#34353=CARTESIAN_POINT('',(-56.7764331763494,-57.2100813324657,-10.));
#34354=CARTESIAN_POINT('Origin',(-60.,-60.,-10.));
#34355=CARTESIAN_POINT('Ctrl Pts',(-56.7764331763494,-57.2100813324657,
-10.));
#34356=CARTESIAN_POINT('Ctrl Pts',(-57.1737624330954,-56.751787072741,-9.96602721186202));
#34357=CARTESIAN_POINT('Ctrl Pts',(-57.669807126483,-56.3786504952751,-9.93205442372405));
#34358=CARTESIAN_POINT('Ctrl Pts',(-58.2209772157099,-56.1255712923699,
-9.89808163558608));
#34359=CARTESIAN_POINT('Ctrl Pts',(-58.8532573166438,-55.8352490359833,
-9.85910942295565));
#34360=CARTESIAN_POINT('Ctrl Pts',(-59.5580810781206,-55.7029193217492,
-9.82013721032522));
#34361=CARTESIAN_POINT('Ctrl Pts',(-60.2526054566513,-55.7441421593256,
-9.78116499769479));
#34362=CARTESIAN_POINT('Ctrl Pts',(-60.947129835182,-55.785364996902,-9.74219278506436));
#34363=CARTESIAN_POINT('Ctrl Pts',(-61.6313548307664,-56.0001403862888,
-9.70322057243393));
#34364=CARTESIAN_POINT('Ctrl Pts',(-62.2248512157896,-56.3632202234726,
-9.6642483598035));
#34365=CARTESIAN_POINT('Ctrl Pts',(-62.8183476008128,-56.7263000606564,
-9.62527614717307));
#34366=CARTESIAN_POINT('Ctrl Pts',(-63.3211153752746,-57.2376843456373,
-9.58630393454265));
#34367=CARTESIAN_POINT('Ctrl Pts',(-63.6740580651529,-57.8372638312712,
-9.54733172191222));
#34368=CARTESIAN_POINT('Ctrl Pts',(-64.0270007550312,-58.4368433169052,
-9.50835950928179));
#34369=CARTESIAN_POINT('Ctrl Pts',(-64.2301183603261,-59.1246180031922,
-9.46938729665136));
#34370=CARTESIAN_POINT('Ctrl Pts',(-64.2595350229124,-59.8197432549321,
-9.43041508402093));
#34371=CARTESIAN_POINT('Ctrl Pts',(-64.2889516854988,-60.514868506672,-9.3914428713905));
#34372=CARTESIAN_POINT('Ctrl Pts',(-64.1446674053766,-61.2173443238648,
-9.35247065876007));
#34373=CARTESIAN_POINT('Ctrl Pts',(-63.8436422372794,-61.8445988100496,
-9.31349844612964));
#34374=CARTESIAN_POINT('Ctrl Pts',(-63.5426170691822,-62.4718532962343,
-9.27452623349921));
#34375=CARTESIAN_POINT('Ctrl Pts',(-63.0848510131098,-63.023886451411,-9.23555402086878));
#34376=CARTESIAN_POINT('Ctrl Pts',(-62.5241518227932,-63.4358097166499,
-9.19658180823835));
#34377=CARTESIAN_POINT('Ctrl Pts',(-61.9634526324765,-63.8477329818888,
-9.15760959560792));
#34378=CARTESIAN_POINT('Ctrl Pts',(-61.2998203079155,-64.1195463571897,
-9.11863738297749));
#34379=CARTESIAN_POINT('Ctrl Pts',(-60.6112612120411,-64.2192997468536,
-9.07966517034706));
#34380=CARTESIAN_POINT('Ctrl Pts',(-59.9227021161667,-64.3190531365174,
-9.04069295771663));
#34381=CARTESIAN_POINT('Ctrl Pts',(-59.209216248979,-64.246746540544,-9.0017207450862));
#34382=CARTESIAN_POINT('Ctrl Pts',(-58.5546698865512,-64.0108791546658,
-8.96274853245577));
#34383=CARTESIAN_POINT('Ctrl Pts',(-57.9001235241234,-63.7750117687875,
-8.92377631982534));
#34384=CARTESIAN_POINT('Ctrl Pts',(-57.3045166664556,-63.3755835930045,
-8.88480410719491));
#34385=CARTESIAN_POINT('Ctrl Pts',(-56.8378596441864,-62.8595452525819,
-8.84583189456448));
#34386=CARTESIAN_POINT('Ctrl Pts',(-56.3712026219172,-62.3435069121593,
-8.80685968193405));
#34387=CARTESIAN_POINT('Ctrl Pts',(-56.0334954350465,-61.7108584070972,
-8.76788746930362));
#34388=CARTESIAN_POINT('Ctrl Pts',(-55.864433621884,-61.0359639683527,-8.72891525667319));
#34389=CARTESIAN_POINT('Ctrl Pts',(-55.7797022872564,-60.6977166405979,
-8.70938294758578));
#34390=CARTESIAN_POINT('Ctrl Pts',(-55.7373324674286,-60.3488576861761,
-8.68985063849836));
#34391=CARTESIAN_POINT('Ctrl Pts',(-55.7373303432786,-59.9999992452069,
-8.67031832941095));
#34392=CARTESIAN_POINT('Origin',(-60.,-60.,-13.3123464956316));
#34393=CARTESIAN_POINT('',(-54.9005857767199,-59.9999919028974,-3.68765350436841));
#34394=CARTESIAN_POINT('',(-54.9008894996693,-60.0001150529132,-3.56234649563159));
#34395=CARTESIAN_POINT('',(-54.901,-60.,-13.3123464956316));
#34396=CARTESIAN_POINT('',(-63.6032183801568,-56.3921449163111,-3.));
#34397=CARTESIAN_POINT('Ctrl Pts',(-54.9008894996694,-60.0001150529132,
-3.56234649563159));
#34398=CARTESIAN_POINT('Ctrl Pts',(-54.9015383135063,-59.326085801412,-3.53078651427611));
#34399=CARTESIAN_POINT('Ctrl Pts',(-55.2021867542944,-57.8191582190388,
-3.4602543202902));
#34400=CARTESIAN_POINT('Ctrl Pts',(-56.6444156037563,-55.8880831676333,
-3.35074991367387));
#34401=CARTESIAN_POINT('Ctrl Pts',(-58.972955243809,-54.7929300280156,-3.23383327578258));
#34402=CARTESIAN_POINT('Ctrl Pts',(-61.543255288011,-54.9220257467759,-3.11691663789129));
#34403=CARTESIAN_POINT('Ctrl Pts',(-63.0142489447553,-55.8039324061734,
-3.03897221263043));
#34404=CARTESIAN_POINT('Ctrl Pts',(-63.6032183801568,-56.3921449163111,
-3.));
#34405=CARTESIAN_POINT('',(-64.9263786176897,-58.683468154111,-3.));
#34406=CARTESIAN_POINT('Origin',(-60.,-60.,-3.));
#34407=CARTESIAN_POINT('Ctrl Pts',(-54.90058577672,-59.9999919028974,-3.68765350436841));
#34408=CARTESIAN_POINT('Ctrl Pts',(-54.9005849893558,-59.9917925604521,
-3.68726952086906));
#34409=CARTESIAN_POINT('Ctrl Pts',(-54.9025709850474,-59.1514054532116,
-3.64791332473929));
#34410=CARTESIAN_POINT('Ctrl Pts',(-55.3285862434613,-57.4808672502626,
-3.56958491597908));
#34411=CARTESIAN_POINT('Ctrl Pts',(-57.0626757333642,-55.5795636292569,
-3.45266827808779));
#34412=CARTESIAN_POINT('Ctrl Pts',(-59.4872942572559,-54.7174568855574,
-3.3357516401965));
#34413=CARTESIAN_POINT('Ctrl Pts',(-62.032451512693,-55.097214824058,-3.21883500230521));
#34414=CARTESIAN_POINT('Ctrl Pts',(-64.0113857967048,-56.5640445520485,
-3.10691778890638));
#34415=CARTESIAN_POINT('Ctrl Pts',(-64.738468572607,-57.9827263087995,-3.03397278813797));
#34416=CARTESIAN_POINT('Ctrl Pts',(-64.9263786176897,-58.683468154111,-3.));
#34417=CARTESIAN_POINT('Origin',(-60.,-60.,-13.3123464956316));
#34418=CARTESIAN_POINT('',(-54.9007404436203,-60.0000650034929,-5.18765350436841));
#34419=CARTESIAN_POINT('',(-54.9012719965578,-60.0000880559789,-5.06234649563159));
#34420=CARTESIAN_POINT('',(-54.901,-60.,-13.3123464956316));
#34421=CARTESIAN_POINT('Ctrl Pts',(-54.9012719965578,-60.0000880559789,
-5.06234649563159));
#34422=CARTESIAN_POINT('Ctrl Pts',(-54.9016210803273,-59.4677293585841,
-5.0374252784717));
#34423=CARTESIAN_POINT('Ctrl Pts',(-55.114536066124,-58.1025886329227,-4.97353184868138));
#34424=CARTESIAN_POINT('Ctrl Pts',(-56.3134109850716,-56.1819888457558,
-4.87066620626063));
#34425=CARTESIAN_POINT('Ctrl Pts',(-58.5427258897122,-54.8966206707426,
-4.75374956836934));
#34426=CARTESIAN_POINT('Ctrl Pts',(-61.1146285526069,-54.8109981670255,
-4.63683293047805));
#34427=CARTESIAN_POINT('Ctrl Pts',(-63.424494989862,-55.9452536147892,-4.51991629258676));
#34428=CARTESIAN_POINT('Ctrl Pts',(-64.9293002326319,-58.0327345315151,
-4.40299965469548));
#34429=CARTESIAN_POINT('Ctrl Pts',(-65.2752818507472,-60.5826980463265,
-4.28608301680418));
#34430=CARTESIAN_POINT('Ctrl Pts',(-64.381102712243,-62.9956755106081,-4.16916637891289));
#34431=CARTESIAN_POINT('Ctrl Pts',(-62.4569756051562,-64.7044030653083,
-4.0522497410216));
#34432=CARTESIAN_POINT('Ctrl Pts',(-59.9552391145712,-65.3071771254814,
-3.93533310313031));
#34433=CARTESIAN_POINT('Ctrl Pts',(-57.4640288862619,-64.6622934850025,
-3.81841646523903));
#34434=CARTESIAN_POINT('Ctrl Pts',(-55.5689898565188,-62.921354421668,-3.70149982734774));
#34435=CARTESIAN_POINT('Ctrl Pts',(-54.9459957256052,-61.1489679675317,
-3.61614317081193));
#34436=CARTESIAN_POINT('Ctrl Pts',(-54.9007371181404,-60.1584187173525,
-3.56975872690654));
#34437=CARTESIAN_POINT('Ctrl Pts',(-54.9008894996694,-60.0001150529132,
-3.56234649563159));
#34438=CARTESIAN_POINT('Ctrl Pts',(-54.9007404436203,-60.0000650034929,
-5.18765350436841));
#34439=CARTESIAN_POINT('Ctrl Pts',(-54.9013740771447,-59.3013380632403,
-5.15493607243422));
#34440=CARTESIAN_POINT('Ctrl Pts',(-55.2189957750169,-57.7698537702076,
-5.0832464278696));
#34441=CARTESIAN_POINT('Ctrl Pts',(-56.7044889980166,-55.8396721524265,
-4.97258457067455));
#34442=CARTESIAN_POINT('Ctrl Pts',(-59.0489177395961,-54.7785641063853,
-4.85566793278326));
#34443=CARTESIAN_POINT('Ctrl Pts',(-61.6168265507944,-54.9449006597622,
-4.73875129489197));
#34444=CARTESIAN_POINT('Ctrl Pts',(-63.8046877645853,-56.2996615825733,
-4.62183465700068));
#34445=CARTESIAN_POINT('Ctrl Pts',(-65.0980856519831,-58.5243188288231,
-4.50491801910939));
#34446=CARTESIAN_POINT('Ctrl Pts',(-65.1929908727149,-61.0958980618402,
-4.3880013812181));
#34447=CARTESIAN_POINT('Ctrl Pts',(-64.0670764169607,-63.4098411642031,
-4.27108474332681));
#34448=CARTESIAN_POINT('Ctrl Pts',(-61.9850396640587,-64.922169576908,-4.15416810543552));
#34449=CARTESIAN_POINT('Ctrl Pts',(-59.4363409557176,-65.2773498680853,
-4.03725146754424));
#34450=CARTESIAN_POINT('Ctrl Pts',(-57.0201528179928,-64.3918838717894,
-3.92033482965294));
#34451=CARTESIAN_POINT('Ctrl Pts',(-55.3101280285781,-62.4802335661766,
-3.803802175261));
#34452=CARTESIAN_POINT('Ctrl Pts',(-54.9006649024818,-60.8239807085089,
-3.72624173349949));
#34453=CARTESIAN_POINT('Ctrl Pts',(-54.90058577672,-59.9999919028974,-3.68765350436841));
#34454=CARTESIAN_POINT('Origin',(-60.,-60.,-13.3123464956316));
#34455=CARTESIAN_POINT('',(-54.9015460351941,-60.0005773825349,-6.68765350436841));
#34456=CARTESIAN_POINT('',(-54.9013619964909,-59.993555404835,-6.56234649563159));
#34457=CARTESIAN_POINT('',(-54.901,-60.,-13.3123464956316));
#34458=CARTESIAN_POINT('Ctrl Pts',(-54.9013619964909,-59.993555404835,-6.56234649563159));
#34459=CARTESIAN_POINT('Ctrl Pts',(-54.8977387393831,-59.6027953335095,
-6.54406404266729));
#34460=CARTESIAN_POINT('Ctrl Pts',(-55.1133264945161,-57.5511818397621,
-6.44783716444213));
#34461=CARTESIAN_POINT('Ctrl Pts',(-57.2611355705387,-55.1183391042526,
-6.31263807358654));
#34462=CARTESIAN_POINT('Ctrl Pts',(-60.6812398138874,-54.7414747298955,
-6.15674922306482));
#34463=CARTESIAN_POINT('Ctrl Pts',(-63.0733672306018,-55.6714881210263,
-6.03983258517353));
#34464=CARTESIAN_POINT('Ctrl Pts',(-64.7488468685178,-57.6299773495695,
-5.92291594728224));
#34465=CARTESIAN_POINT('Ctrl Pts',(-65.3052031061324,-60.1405546503375,
-5.80599930939095));
#34466=CARTESIAN_POINT('Ctrl Pts',(-64.6156238857644,-62.6204341592567,
-5.68908267149966));
#34467=CARTESIAN_POINT('Ctrl Pts',(-62.8403791725874,-64.4831910135561,
-5.57216603360837));
#34468=CARTESIAN_POINT('Ctrl Pts',(-60.3976628726492,-65.2925026120897,
-5.45524939571708));
#34469=CARTESIAN_POINT('Ctrl Pts',(-57.8613353265494,-64.8573722732082,
-5.33833275782579));
#34470=CARTESIAN_POINT('Ctrl Pts',(-55.8278421001908,-63.2804354591061,
-5.2214161199345));
#34471=CARTESIAN_POINT('Ctrl Pts',(-54.9995353787376,-61.4327780915017,
-5.1294206992031));
#34472=CARTESIAN_POINT('Ctrl Pts',(-54.9010751773401,-60.3002407169748,
-5.07639749110213));
#34473=CARTESIAN_POINT('Ctrl Pts',(-54.9012719965578,-60.0000880559789,
-5.06234649563159));
#34474=CARTESIAN_POINT('Ctrl Pts',(-54.9015460351941,-60.0005773825349,
-6.68765350436841));
#34475=CARTESIAN_POINT('Ctrl Pts',(-54.9025454955962,-59.4443140467181,
-6.66157483662981));
#34476=CARTESIAN_POINT('Ctrl Pts',(-55.1311200271658,-58.0563310394583,
-6.59652395626078));
#34477=CARTESIAN_POINT('Ctrl Pts',(-56.8226683737146,-55.391675711492,-6.45352865063088));
#34478=CARTESIAN_POINT('Ctrl Pts',(-61.3338598105922,-54.1559235864261,
-6.25866758747874));
#34479=CARTESIAN_POINT('Ctrl Pts',(-65.6028015656481,-57.869031736986,-6.02483431169615));
#34480=CARTESIAN_POINT('Ctrl Pts',(-65.0042219447148,-62.5079576829526,
-5.82997324854401));
#34481=CARTESIAN_POINT('Ctrl Pts',(-62.382923622443,-64.736849642231,-5.67408439802229));
#34482=CARTESIAN_POINT('Ctrl Pts',(-59.8805760101181,-65.3072934023813,
-5.557167760131));
#34483=CARTESIAN_POINT('Ctrl Pts',(-57.3953244921747,-64.6243069865738,
-5.44025112223971));
#34484=CARTESIAN_POINT('Ctrl Pts',(-55.5275122251888,-62.8568832667251,
-5.32333448434841));
#34485=CARTESIAN_POINT('Ctrl Pts',(-54.9378834983018,-61.0994765924383,
-5.23913527839132));
#34486=CARTESIAN_POINT('Ctrl Pts',(-54.9006193082346,-60.1336446740069,
-5.19390828506465));
#34487=CARTESIAN_POINT('Ctrl Pts',(-54.9007404436203,-60.0000650034929,
-5.18765350436841));
#34488=CARTESIAN_POINT('Origin',(-60.,-60.,-13.3123464956316));
#34489=CARTESIAN_POINT('',(-54.901395125587,-59.9999990971874,-8.18765350436841));
#34490=CARTESIAN_POINT('',(-54.9011518411408,-59.9998830094301,-8.06234649563159));
#34491=CARTESIAN_POINT('',(-54.901,-60.,-13.3123464956316));
#34492=CARTESIAN_POINT('Ctrl Pts',(-54.9011518411408,-59.9998830094301,
-8.06234649563159));
#34493=CARTESIAN_POINT('Ctrl Pts',(-54.9009384336978,-59.7511708635701,
-8.05070280686288));
#34494=CARTESIAN_POINT('Ctrl Pts',(-54.9786898953671,-58.6701368161215,
-8.00008690546374));
#34495=CARTESIAN_POINT('Ctrl Pts',(-55.7305243149913,-56.8472980856346,
-7.91049879143416));
#34496=CARTESIAN_POINT('Ctrl Pts',(-57.7154061456845,-55.2094519541036,
-7.79358215354287));
#34497=CARTESIAN_POINT('Ctrl Pts',(-60.2373779816841,-54.6980751417997,
-7.67666551565158));
#34498=CARTESIAN_POINT('Ctrl Pts',(-62.7035292062656,-55.4325511640916,
-7.55974887776029));
#34499=CARTESIAN_POINT('Ctrl Pts',(-64.5341447372141,-57.2420175654881,
-7.442832239869));
#34500=CARTESIAN_POINT('Ctrl Pts',(-65.2987604896043,-59.6971944221457,
-7.32591560197771));
#34501=CARTESIAN_POINT('Ctrl Pts',(-64.8178571527642,-62.229316863103,-7.20899896408642));
#34502=CARTESIAN_POINT('Ctrl Pts',(-63.2040090754463,-64.2249853898932,
-7.09208232619513));
#34503=CARTESIAN_POINT('Ctrl Pts',(-60.048707386807,-65.597286758288,-6.93619347567342));
#34504=CARTESIAN_POINT('Ctrl Pts',(-56.0355251757418,-64.2336342647843,
-6.75961486548556));
#34505=CARTESIAN_POINT('Ctrl Pts',(-54.9131859385852,-61.2687407749573,
-6.62200846792815));
#34506=CARTESIAN_POINT('Ctrl Pts',(-54.9013619964909,-59.993555404835,-6.56234649563159));
#34507=CARTESIAN_POINT('Ctrl Pts',(-54.901395125587,-59.9999990971874,-8.18765350436841));
#34508=CARTESIAN_POINT('Ctrl Pts',(-54.9013925968981,-59.5847014864836,
-8.1682136008254));
#34509=CARTESIAN_POINT('Ctrl Pts',(-55.0522173125255,-58.3368364086299,
-8.10980148465195));
#34510=CARTESIAN_POINT('Ctrl Pts',(-56.0593765808925,-56.444776458995,-8.01241715584808));
#34511=CARTESIAN_POINT('Ctrl Pts',(-58.1949365065413,-55.009018880156,-7.89550051795679));
#34512=CARTESIAN_POINT('Ctrl Pts',(-60.754850176949,-54.7465903023206,-7.7785838800655));
#34513=CARTESIAN_POINT('Ctrl Pts',(-63.1372997996482,-55.7191702494578,
-7.6616672421742));
#34514=CARTESIAN_POINT('Ctrl Pts',(-64.7822203636214,-57.6981473048777,
-7.54475060428292));
#34515=CARTESIAN_POINT('Ctrl Pts',(-65.3028606509933,-60.2182181776382,
-7.42783396639163));
#34516=CARTESIAN_POINT('Ctrl Pts',(-64.5769288134183,-62.6870882382886,
-7.31091732850035));
#34517=CARTESIAN_POINT('Ctrl Pts',(-62.7748568790513,-64.5240380041187,
-7.19400069060905));
#34518=CARTESIAN_POINT('Ctrl Pts',(-60.3207808627358,-65.2979018325692,
-7.07708405271776));
#34519=CARTESIAN_POINT('Ctrl Pts',(-57.7905711249098,-64.8252826799559,
-6.96016741482647));
#34520=CARTESIAN_POINT('Ctrl Pts',(-55.7813289378715,-63.2204602274652,
-6.84325077693518));
#34521=CARTESIAN_POINT('Ctrl Pts',(-54.9881850222051,-61.3817353652472,
-6.7524128067825));
#34522=CARTESIAN_POINT('Ctrl Pts',(-54.9010518923302,-60.2755993416288,
-6.70054704926024));
#34523=CARTESIAN_POINT('Ctrl Pts',(-54.9015460351941,-60.0005773825349,
-6.68765350436841));
#34524=CARTESIAN_POINT('Origin',(-60.,-60.,-13.3123464956316));
#34525=CARTESIAN_POINT('',(-54.9012106606313,-59.9998804662267,-9.68765350436841));
#34526=CARTESIAN_POINT('',(-54.9007452025866,-59.9999087514893,-9.56234649563159));
#34527=CARTESIAN_POINT('',(-54.901,-60.,-13.3123464956316));
#34528=CARTESIAN_POINT('',(-58.6771150344309,-64.9244061944433,-10.));
#34529=CARTESIAN_POINT('Ctrl Pts',(-58.677115034431,-64.9244061944433,-10.));
#34530=CARTESIAN_POINT('Ctrl Pts',(-57.8732233401272,-64.7084499564018,
-9.96102778736957));
#34531=CARTESIAN_POINT('Ctrl Pts',(-56.3739727010425,-63.8754866332611,
-9.88308336210871));
#34532=CARTESIAN_POINT('Ctrl Pts',(-55.1299740881578,-61.950738551684,-9.77896786356485));
#34533=CARTESIAN_POINT('Ctrl Pts',(-54.9016327839252,-60.5589070089215,
-9.71382457765142));
#34534=CARTESIAN_POINT('Ctrl Pts',(-54.9012106606313,-59.9998804662267,
-9.68765350436841));
#34535=CARTESIAN_POINT('',(-61.3230392926944,-64.9246350552985,-10.));
#34536=CARTESIAN_POINT('Origin',(-60.,-60.,-10.));
#34537=CARTESIAN_POINT('Ctrl Pts',(-61.3230392926944,-64.9246350552985,
-10.));
#34538=CARTESIAN_POINT('Ctrl Pts',(-60.6222240304355,-65.1122710972509,
-9.96602721186203));
#34539=CARTESIAN_POINT('Ctrl Pts',(-59.0300681563555,-65.1919398523856,
-9.89308221109362));
#34540=CARTESIAN_POINT('Ctrl Pts',(-56.7702891895575,-64.2115472965565,
-9.78116499769479));
#34541=CARTESIAN_POINT('Ctrl Pts',(-55.2373851602932,-62.2834824754791,
-9.66925328437662));
#34542=CARTESIAN_POINT('Ctrl Pts',(-54.9013550630092,-60.725290539657,-9.5963137836889));
#34543=CARTESIAN_POINT('Ctrl Pts',(-54.9007452025866,-59.9999087514893,
-9.56234649563159));
#34544=CARTESIAN_POINT('Origin',(60.,60.,-6.));
#34545=CARTESIAN_POINT('',(64.2627725569288,59.999926383973,-4.57968167058906));
#34546=CARTESIAN_POINT('',(64.2633463508187,60.0000067694975,-4.17031832941094));
#34547=CARTESIAN_POINT('',(64.263,60.,-6.));
#34548=CARTESIAN_POINT('',(60.8043894954945,55.8135783132205,-3.));
#34549=CARTESIAN_POINT('Ctrl Pts',(64.2633463508187,60.0000067694975,-4.17031832941094));
#34550=CARTESIAN_POINT('Ctrl Pts',(64.2633470090911,60.0068617993432,-4.16993434591159));
#34551=CARTESIAN_POINT('Ctrl Pts',(64.2633308093496,60.0137168260627,-4.16955036241224));
#34552=CARTESIAN_POINT('Ctrl Pts',(64.2632977324257,60.0205717713411,-4.16916637891289));
#34553=CARTESIAN_POINT('Ctrl Pts',(64.2599406066242,60.7163110033908,-4.13019416628246));
#34554=CARTESIAN_POINT('Ctrl Pts',(64.0827293769352,61.4112112987266,-4.09122195365203));
#34555=CARTESIAN_POINT('Ctrl Pts',(63.7524939144254,62.0235910863766,-4.0522497410216));
#34556=CARTESIAN_POINT('Ctrl Pts',(63.4222584519156,62.6359708740266,-4.01327752839118));
#34557=CARTESIAN_POINT('Ctrl Pts',(62.938998756585,63.1658301539908,-3.97430531576075));
#34558=CARTESIAN_POINT('Ctrl Pts',(62.3595200208981,63.5508866522884,-3.93533310313031));
#34559=CARTESIAN_POINT('Ctrl Pts',(61.7800412852112,63.935943150586,-3.89636089049989));
#34560=CARTESIAN_POINT('Ctrl Pts',(61.104343509168,64.176196867217,-3.85738867786946));
#34561=CARTESIAN_POINT('Ctrl Pts',(60.4118497411081,64.243407855033,-3.81841646523903));
#34562=CARTESIAN_POINT('Ctrl Pts',(59.7193559730481,64.3106188428491,-3.7794442526086));
#34563=CARTESIAN_POINT('Ctrl Pts',(59.0100662129713,64.2047871018501,-3.74047203997816));
#34564=CARTESIAN_POINT('Ctrl Pts',(58.367356741015,63.9383514081819,-3.70149982734773));
#34565=CARTESIAN_POINT('Ctrl Pts',(57.7246472690586,63.6719157145136,-3.6625276147173));
#34566=CARTESIAN_POINT('Ctrl Pts',(57.1485180852227,63.2448760681761,-3.62355540208687));
#34567=CARTESIAN_POINT('Ctrl Pts',(56.7066830620729,62.7074312242854,-3.58458318945645));
#34568=CARTESIAN_POINT('Ctrl Pts',(56.2648480389232,62.1699863803947,-3.54561097682602));
#34569=CARTESIAN_POINT('Ctrl Pts',(55.9573071764596,61.5221363389508,-3.50663876419559));
#34570=CARTESIAN_POINT('Ctrl Pts',(55.8202250347853,60.8400271110314,-3.46766655156516));
#34571=CARTESIAN_POINT('Ctrl Pts',(55.683142893111,60.1579178831119,-3.42869433893473));
#34572=CARTESIAN_POINT('Ctrl Pts',(55.7165194722261,59.441549468717,-3.3897221263043));
#34573=CARTESIAN_POINT('Ctrl Pts',(55.9163990068928,58.775140191943,-3.35074991367387));
#34574=CARTESIAN_POINT('Ctrl Pts',(56.1162785415595,58.108730915169,-3.31177770104344));
#34575=CARTESIAN_POINT('Ctrl Pts',(56.4826610317779,57.4922807760161,-3.27280548841301));
#34576=CARTESIAN_POINT('Ctrl Pts',(56.9725486039278,56.9982300189206,-3.23383327578258));
#34577=CARTESIAN_POINT('Ctrl Pts',(57.4624361760777,56.5041792618252,-3.19486106315215));
#34578=CARTESIAN_POINT('Ctrl Pts',(58.0758288301591,56.1325278867873,-3.15588885052172));
#34579=CARTESIAN_POINT('Ctrl Pts',(58.7404625691261,55.927049222772,-3.11691663789129));
#34580=CARTESIAN_POINT('Ctrl Pts',(59.4050963080931,55.7215705587567,-3.07794442526086));
#34581=CARTESIAN_POINT('Ctrl Pts',(60.1209711319459,55.6822646057641,-3.03897221263043));
#34582=CARTESIAN_POINT('Ctrl Pts',(60.8043894954945,55.8135783132205,-3.));
#34583=CARTESIAN_POINT('',(64.0279238903325,61.3967314318666,-3.));
#34584=CARTESIAN_POINT('Origin',(60.,60.,-3.));
#34585=CARTESIAN_POINT('',(64.2630923348121,59.9999038151513,-3.07968167058906));
#34586=CARTESIAN_POINT('Ctrl Pts',(64.0279238903325,61.3967314318666,-3.));
#34587=CARTESIAN_POINT('Ctrl Pts',(64.1829036615969,60.9485583421562,-3.02656055686302));
#34588=CARTESIAN_POINT('Ctrl Pts',(64.2626358261587,60.4741561725529,-3.05312111372604));
#34589=CARTESIAN_POINT('Ctrl Pts',(64.2630923348121,59.9999038151513,-3.07968167058906));
#34590=CARTESIAN_POINT('',(64.263,60.,-2.));
#34591=CARTESIAN_POINT('',(64.263,60.,-6.));
#34592=CARTESIAN_POINT('Origin',(60.,60.,-2.));
#34593=CARTESIAN_POINT('Ctrl Pts',(64.2630923348121,59.9999038151513,-3.07968167058906));
#34594=CARTESIAN_POINT('Ctrl Pts',(64.2632197322811,59.8675546263191,-3.08709390186401));
#34595=CARTESIAN_POINT('Ctrl Pts',(64.257173175386,59.7352171047975,-3.09450613313896));
#34596=CARTESIAN_POINT('Ctrl Pts',(64.2448651193736,59.6034645637425,-3.10191836441392));
#34597=CARTESIAN_POINT('Ctrl Pts',(64.180151518544,58.9107327999692,-3.14089057704435));
#34598=CARTESIAN_POINT('Ctrl Pts',(63.942340524664,58.2341726576991,-3.17986278967478));
#34599=CARTESIAN_POINT('Ctrl Pts',(63.5593783060224,57.6533083171945,-3.21883500230521));
#34600=CARTESIAN_POINT('Ctrl Pts',(63.1764160873809,57.07244397669,-3.25780721493564));
#34601=CARTESIAN_POINT('Ctrl Pts',(62.6483026439779,56.5872754379511,-3.29677942756607));
#34602=CARTESIAN_POINT('Ctrl Pts',(62.0371180843352,56.2548324073596,-3.3357516401965));
#34603=CARTESIAN_POINT('Ctrl Pts',(61.4259335246925,55.9223893767681,-3.37472385282693));
#34604=CARTESIAN_POINT('Ctrl Pts',(60.7316778488101,55.742671854324,-3.41369606545736));
#34605=CARTESIAN_POINT('Ctrl Pts',(60.0359554314242,55.7368042611768,-3.45266827808779));
#34606=CARTESIAN_POINT('Ctrl Pts',(59.3402330140382,55.7309366680297,-3.49164049071822));
#34607=CARTESIAN_POINT('Ctrl Pts',(58.6430438551486,55.8989190041796,-3.53061270334864));
#34608=CARTESIAN_POINT('Ctrl Pts',(58.0263393924009,56.2210060567882,-3.56958491597907));
#34609=CARTESIAN_POINT('Ctrl Pts',(57.4096349296532,56.5430931093967,-3.6085571286095));
#34610=CARTESIAN_POINT('Ctrl Pts',(56.8734151630474,57.019284878464,-3.64752934123993));
#34611=CARTESIAN_POINT('Ctrl Pts',(56.4807094232938,57.5936075665364,-3.68650155387036));
#34612=CARTESIAN_POINT('Ctrl Pts',(56.0880036835401,58.1679302546087,-3.72547376650079));
#34613=CARTESIAN_POINT('Ctrl Pts',(55.8388119706386,58.8403838616862,-3.76444597913122));
#34614=CARTESIAN_POINT('Ctrl Pts',(55.7624255547685,59.5319252483343,-3.80341819176165));
#34615=CARTESIAN_POINT('Ctrl Pts',(55.6860391388985,60.2234666349825,-3.84239040439208));
#34616=CARTESIAN_POINT('Ctrl Pts',(55.7824580200599,60.9340958012014,-3.88136261702251));
#34617=CARTESIAN_POINT('Ctrl Pts',(56.0403485969429,61.580282158413,-3.92033482965294));
#34618=CARTESIAN_POINT('Ctrl Pts',(56.2982391738259,62.2264685156246,-3.95930704228337));
#34619=CARTESIAN_POINT('Ctrl Pts',(56.7176014464305,62.8082120638289,-3.9982792549138));
#34620=CARTESIAN_POINT('Ctrl Pts',(57.2491417880006,63.2571321784525,-4.03725146754423));
#34621=CARTESIAN_POINT('Ctrl Pts',(57.7806821295708,63.706052293076,-4.07622368017466));
#34622=CARTESIAN_POINT('Ctrl Pts',(58.4244005401064,64.0221489741188,-4.11519589280509));
#34623=CARTESIAN_POINT('Ctrl Pts',(59.1046313521504,64.1682665851206,-4.15416810543553));
#34624=CARTESIAN_POINT('Ctrl Pts',(59.7848621641945,64.3143841961224,-4.19314031806595));
#34625=CARTESIAN_POINT('Ctrl Pts',(60.5016053777469,64.2905227370833,-4.23211253069638));
#34626=CARTESIAN_POINT('Ctrl Pts',(61.1706120551988,64.0994874623445,-4.27108474332681));
#34627=CARTESIAN_POINT('Ctrl Pts',(61.8396187326508,63.9084521876057,-4.31005695595724));
#34628=CARTESIAN_POINT('Ctrl Pts',(62.4608888740024,63.5502430971673,-4.34902916858767));
#34629=CARTESIAN_POINT('Ctrl Pts',(62.9613950657551,63.0669646706093,-4.3880013812181));
#34630=CARTESIAN_POINT('Ctrl Pts',(63.4619012575079,62.5836862440512,-4.42697359384853));
#34631=CARTESIAN_POINT('Ctrl Pts',(63.8416434996618,61.9753384813737,-4.46594580647896));
#34632=CARTESIAN_POINT('Ctrl Pts',(64.0559863710237,61.3134314862707,-4.50491801910939));
#34633=CARTESIAN_POINT('Ctrl Pts',(64.1930503169315,60.8901676567048,-4.52983923626928));
#34634=CARTESIAN_POINT('Ctrl Pts',(64.2624807063128,60.4450028890856,-4.55476045342917));
#34635=CARTESIAN_POINT('Ctrl Pts',(64.2627725569288,59.999926383973,-4.57968167058906));
#34636=CARTESIAN_POINT('Origin',(60.,60.,-6.));
#34637=CARTESIAN_POINT('',(64.2626973799646,60.005388464797,-6.07968167058906));
#34638=CARTESIAN_POINT('',(64.2632169517948,59.999945593479,-5.67031832941094));
#34639=CARTESIAN_POINT('',(64.263,60.,-6.));
#34640=CARTESIAN_POINT('Ctrl Pts',(64.2632169517948,59.999945593479,-5.67031832941094));
#34641=CARTESIAN_POINT('Ctrl Pts',(64.2626872015258,60.5841136575979,-5.63760089747675));
#34642=CARTESIAN_POINT('Ctrl Pts',(64.141498283485,61.1684537725971,-5.60488346554256));
#34643=CARTESIAN_POINT('Ctrl Pts',(63.908043668822,61.7038522263494,-5.57216603360837));
#34644=CARTESIAN_POINT('Ctrl Pts',(63.6299581852027,62.3416058991808,-5.53319382097794));
#34645=CARTESIAN_POINT('Ctrl Pts',(63.1925789329281,62.9099162611984,-5.49422160834751));
#34646=CARTESIAN_POINT('Ctrl Pts',(62.6472141655169,63.3419273614047,-5.45524939571708));
#34647=CARTESIAN_POINT('Ctrl Pts',(62.1018493981057,63.773938461611,-5.41627718308665));
#34648=CARTESIAN_POINT('Ctrl Pts',(61.4484991155579,64.0696503000059,-5.37730497045622));
#34649=CARTESIAN_POINT('Ctrl Pts',(60.764008858737,64.1943287037686,-5.33833275782579));
#34650=CARTESIAN_POINT('Ctrl Pts',(60.0795186019162,64.3190071075312,-5.29936054519536));
#34651=CARTESIAN_POINT('Ctrl Pts',(59.3638883708224,64.2726520766615,-5.26038833256493));
#34652=CARTESIAN_POINT('Ctrl Pts',(58.7012143841293,64.0607007564596,-5.2214161199345));
#34653=CARTESIAN_POINT('Ctrl Pts',(58.0385403974362,63.8487494362578,-5.18244390730407));
#34654=CARTESIAN_POINT('Ctrl Pts',(57.4288226551439,63.4712018267237,-5.14347169467364));
#34655=CARTESIAN_POINT('Ctrl Pts',(56.9437403638198,62.9724419470908,-5.10449948204321));
#34656=CARTESIAN_POINT('Ctrl Pts',(56.4586580724957,62.473682067458,-5.06552726941278));
#34657=CARTESIAN_POINT('Ctrl Pts',(56.09821123214,61.8537099177263,-5.02655505678235));
#34658=CARTESIAN_POINT('Ctrl Pts',(55.9047636201273,61.1853972966568,-4.98758284415192));
#34659=CARTESIAN_POINT('Ctrl Pts',(55.7113160081146,60.5170846755874,-4.94861063152149));
#34660=CARTESIAN_POINT('Ctrl Pts',(55.684867624445,59.8004315831803,-4.90963841889106));
#34661=CARTESIAN_POINT('Ctrl Pts',(55.828529532945,59.1196777783533,-4.87066620626063));
#34662=CARTESIAN_POINT('Ctrl Pts',(55.972191441445,58.4389239735264,-4.8316939936302));
#34663=CARTESIAN_POINT('Ctrl Pts',(56.2859636421146,57.7940694562796,-4.79272178099977));
#34664=CARTESIAN_POINT('Ctrl Pts',(56.7329629271073,57.2609127709619,-4.75374956836934));
#34665=CARTESIAN_POINT('Ctrl Pts',(57.1799622121,56.7277560856442,-4.71477735573891));
#34666=CARTESIAN_POINT('Ctrl Pts',(57.7601885814157,56.3062972322555,-4.67580514310848));
#34667=CARTESIAN_POINT('Ctrl Pts',(58.4054401165192,56.0460766112725,-4.63683293047805));
#34668=CARTESIAN_POINT('Ctrl Pts',(59.0506916516226,55.7858559902895,-4.59786071784762));
#34669=CARTESIAN_POINT('Ctrl Pts',(59.7609683525138,55.6868736017121,-4.55888850521719));
#34670=CARTESIAN_POINT('Ctrl Pts',(60.4527808917702,55.7607641678725,-4.51991629258676));
#34671=CARTESIAN_POINT('Ctrl Pts',(61.1445934310265,55.8346547340329,-4.48094407995633));
#34672=CARTESIAN_POINT('Ctrl Pts',(61.8179418086481,56.0814182549311,-4.4419718673259));
#34673=CARTESIAN_POINT('Ctrl Pts',(62.3936777834231,56.4720490863694,-4.40299965469547));
#34674=CARTESIAN_POINT('Ctrl Pts',(62.969413758198,56.8626799178076,-4.36402744206504));
#34675=CARTESIAN_POINT('Ctrl Pts',(63.4475373301263,57.3971780597858,-4.32505522943461));
#34676=CARTESIAN_POINT('Ctrl Pts',(63.7718476051335,58.0127162151568,-4.28608301680418));
#34677=CARTESIAN_POINT('Ctrl Pts',(64.0929625318178,58.6221896264721,-4.2474947876731));
#34678=CARTESIAN_POINT('Ctrl Pts',(64.263280198064,59.3111139841629,-4.20890655854202));
#34679=CARTESIAN_POINT('Ctrl Pts',(64.2633463508187,60.0000067694975,-4.17031832941094));
#34680=CARTESIAN_POINT('Ctrl Pts',(64.2627725569288,59.999926383973,-4.57968167058906));
#34681=CARTESIAN_POINT('Ctrl Pts',(64.2629371071454,59.7489848702717,-4.5937326660596));
#34682=CARTESIAN_POINT('Ctrl Pts',(64.2411232668863,59.4980714142625,-4.60778366153014));
#34683=CARTESIAN_POINT('Ctrl Pts',(64.1970612964284,59.2511271660237,-4.62183465700068));
#34684=CARTESIAN_POINT('Ctrl Pts',(64.0748498499012,58.5661960684082,-4.66080686963111));
#34685=CARTESIAN_POINT('Ctrl Pts',(63.7814834562769,57.9118001007057,-4.69977908226154));
#34686=CARTESIAN_POINT('Ctrl Pts',(63.351451191029,57.3648701020231,-4.73875129489197));
#34687=CARTESIAN_POINT('Ctrl Pts',(62.9214189257811,56.8179401033406,-4.7777235075224));
#34688=CARTESIAN_POINT('Ctrl Pts',(62.3547207889096,56.378476073678,-4.81669572015283));
#34689=CARTESIAN_POINT('Ctrl Pts',(61.7179571787521,56.09811252218,-4.85566793278326));
#34690=CARTESIAN_POINT('Ctrl Pts',(61.0811935685946,55.8177489706819,-4.89464014541369));
#34691=CARTESIAN_POINT('Ctrl Pts',(60.374364485151,55.6964858973485,-4.93361235804412));
#34692=CARTESIAN_POINT('Ctrl Pts',(59.6805793162926,55.7486247247237,-4.97258457067455));
#34693=CARTESIAN_POINT('Ctrl Pts',(58.9867941474342,55.8007635520988,-5.01155678330498));
#34694=CARTESIAN_POINT('Ctrl Pts',(58.3060528931609,56.0263042801826,-5.05052899593541));
#34695=CARTESIAN_POINT('Ctrl Pts',(57.7183177787476,56.3986330544208,-5.08950120856584));
#34696=CARTESIAN_POINT('Ctrl Pts',(57.1305826643343,56.7709618286591,-5.12847342119627));
#34697=CARTESIAN_POINT('Ctrl Pts',(56.6358536897809,57.2900786490518,-5.16744563382669));
#34698=CARTESIAN_POINT('Ctrl Pts',(56.2924025719534,57.8951862105726,-5.20641784645712));
#34699=CARTESIAN_POINT('Ctrl Pts',(55.9489514541259,58.5002937720934,-5.24539005908756));
#34700=CARTESIAN_POINT('Ctrl Pts',(55.7567781930244,59.1913920747422,-5.28436227171799));
#34701=CARTESIAN_POINT('Ctrl Pts',(55.7382147113452,59.886767398621,-5.32333448434842));
#34702=CARTESIAN_POINT('Ctrl Pts',(55.719651229666,60.5821427224998,-5.36230669697885));
#34703=CARTESIAN_POINT('Ctrl Pts',(55.8746975274092,61.2817950676086,-5.40127890960928));
#34704=CARTESIAN_POINT('Ctrl Pts',(56.1856839431124,61.9045196740408,-5.44025112223971));
#34705=CARTESIAN_POINT('Ctrl Pts',(56.4966703588156,62.527244280473,-5.47922333487014));
#34706=CARTESIAN_POINT('Ctrl Pts',(56.9635968924788,63.0730411482287,-5.51819554750057));
#34707=CARTESIAN_POINT('Ctrl Pts',(57.530381347957,63.475527534543,-5.557167760131));
#34708=CARTESIAN_POINT('Ctrl Pts',(58.0971658034351,63.8780139208573,-5.59613997276143));
#34709=CARTESIAN_POINT('Ctrl Pts',(58.7638081807283,64.1371898257302,-5.63511218539186));
#34710=CARTESIAN_POINT('Ctrl Pts',(59.4545503724775,64.2273943548749,-5.67408439802229));
#34711=CARTESIAN_POINT('Ctrl Pts',(60.1452925642268,64.3175988840196,-5.71305661065272));
#34712=CARTESIAN_POINT('Ctrl Pts',(60.8601345704321,64.2388320374361,-5.75202882328315));
#34713=CARTESIAN_POINT('Ctrl Pts',(61.5092343352991,63.9908846520633,-5.79100103591358));
#34714=CARTESIAN_POINT('Ctrl Pts',(62.8074338650331,63.4949898813177,-5.86894546117444));
#34715=CARTESIAN_POINT('Ctrl Pts',(63.8426644294139,62.322372955415,-5.9468898864353));
#34716=CARTESIAN_POINT('Ctrl Pts',(64.1576093504471,60.9741927827568,-6.02483431169616));
#34717=CARTESIAN_POINT('Ctrl Pts',(64.2314820576467,60.6579669524741,-6.04311676466046));
#34718=CARTESIAN_POINT('Ctrl Pts',(64.2657266356665,60.3320821166483,-6.06139921762476));
#34719=CARTESIAN_POINT('Ctrl Pts',(64.2626973799646,60.005388464797,-6.07968167058906));
#34720=CARTESIAN_POINT('Origin',(60.,60.,-6.));
#34721=CARTESIAN_POINT('',(64.2628730117989,60.0000978162778,-7.57968167058906));
#34722=CARTESIAN_POINT('',(64.2625441198806,59.9995177541909,-7.17031832941094));
#34723=CARTESIAN_POINT('',(64.263,60.,-6.));
#34724=CARTESIAN_POINT('Ctrl Pts',(64.2625441198806,59.9995177541909,-7.17031832941094));
#34725=CARTESIAN_POINT('Ctrl Pts',(64.2617091262571,60.464580224433,-7.14423966167234));
#34726=CARTESIAN_POINT('Ctrl Pts',(64.1850989669132,60.929788399807,-7.11816099393374));
#34727=CARTESIAN_POINT('Ctrl Pts',(64.0358034903878,61.3713756586764,-7.09208232619513));
#34728=CARTESIAN_POINT('Ctrl Pts',(63.8126948901237,62.0312879180006,-7.0531101135647));
#34729=CARTESIAN_POINT('Ctrl Pts',(63.4272610645377,62.6384485248234,-7.01413790093427));
#34730=CARTESIAN_POINT('Ctrl Pts',(62.9188676932756,63.112098827234,-6.97516568830384));
#34731=CARTESIAN_POINT('Ctrl Pts',(61.9020809507514,64.0593994320554,-6.89722126304298));
#34732=CARTESIAN_POINT('Ctrl Pts',(60.3934560255232,64.4726588192284,-6.81927683778212));
#34733=CARTESIAN_POINT('Ctrl Pts',(59.0443048432248,64.1619002172936,-6.74133241252127));
#34734=CARTESIAN_POINT('Ctrl Pts',(57.6951536609264,63.8511416153587,-6.66338798726041));
#34735=CARTESIAN_POINT('Ctrl Pts',(56.5054762215579,62.816365024316,-6.58544356199954));
#34736=CARTESIAN_POINT('Ctrl Pts',(56.0107261197417,61.523305799792,-6.50749913673868));
#34737=CARTESIAN_POINT('Ctrl Pts',(55.5159760179255,60.230246575268,-6.42955471147782));
#34738=CARTESIAN_POINT('Ctrl Pts',(55.7161532536617,58.6789047172628,-6.35161028621697));
#34739=CARTESIAN_POINT('Ctrl Pts',(56.5133856551997,57.5406366409267,-6.27366586095611));
#34740=CARTESIAN_POINT('Ctrl Pts',(56.9120018559687,56.9715026027586,-6.23469364832568));
#34741=CARTESIAN_POINT('Ctrl Pts',(57.4598818481882,56.5056370100079,-6.19572143569525));
#34742=CARTESIAN_POINT('Ctrl Pts',(58.0825024496753,56.1932186620801,-6.15674922306482));
#34743=CARTESIAN_POINT('Ctrl Pts',(58.7051230511624,55.8808003141523,-6.11777701043439));
#34744=CARTESIAN_POINT('Ctrl Pts',(59.4024842619172,55.7218292110476,-6.07880479780396));
#34745=CARTESIAN_POINT('Ctrl Pts',(60.0974620054189,55.7375114038248,-6.03983258517353));
#34746=CARTESIAN_POINT('Ctrl Pts',(60.7924397489205,55.753193596602,-6.0008603725431));
#34747=CARTESIAN_POINT('Ctrl Pts',(61.4850340251691,55.943529085261,-5.96188815991267));
#34748=CARTESIAN_POINT('Ctrl Pts',(62.0915943313093,56.2849716792125,-5.92291594728224));
#34749=CARTESIAN_POINT('Ctrl Pts',(62.6981546374495,56.626414273164,-5.88394373465181));
#34750=CARTESIAN_POINT('Ctrl Pts',(63.2186809734814,57.1189639724079,-5.84497152202138));
#34751=CARTESIAN_POINT('Ctrl Pts',(63.5930283536401,57.7052706411259,-5.80599930939095));
#34752=CARTESIAN_POINT('Ctrl Pts',(63.9673757337987,58.2915773098439,-5.76702709676052));
#34753=CARTESIAN_POINT('Ctrl Pts',(64.1955441580842,58.9716409480359,-5.72805488413009));
#34754=CARTESIAN_POINT('Ctrl Pts',(64.2502325127449,59.6652712589544,-5.68908267149966));
#34755=CARTESIAN_POINT('Ctrl Pts',(64.2590096296175,59.7765943064858,-5.68282789080342));
#34756=CARTESIAN_POINT('Ctrl Pts',(64.2633182272178,59.8882668059091,-5.67657311010718));
#34757=CARTESIAN_POINT('Ctrl Pts',(64.2632169517948,59.999945593479,-5.67031832941094));
#34758=CARTESIAN_POINT('Ctrl Pts',(64.2626973799646,60.005388464797,-6.07968167058906));
#34759=CARTESIAN_POINT('Ctrl Pts',(64.252811870065,58.9392739973195,-6.13934364288562));
#34760=CARTESIAN_POINT('Ctrl Pts',(63.8459813507535,57.8645461017925,-6.19900561518218));
#34761=CARTESIAN_POINT('Ctrl Pts',(63.1240241101926,57.0887733774513,-6.25866758747874));
#34762=CARTESIAN_POINT('Ctrl Pts',(62.1808346712192,56.0752775642175,-6.3366120127396));
#34763=CARTESIAN_POINT('Ctrl Pts',(60.6997965155868,55.5720293571637,-6.41455643800045));
#34764=CARTESIAN_POINT('Ctrl Pts',(59.3267917363085,55.7867187111922,-6.49250086326132));
#34765=CARTESIAN_POINT('Ctrl Pts',(58.6402893466693,55.8940633882065,-6.53147307589175));
#34766=CARTESIAN_POINT('Ctrl Pts',(57.9807953011187,56.1808924554913,-6.57044528852218));
#34767=CARTESIAN_POINT('Ctrl Pts',(57.4261727612217,56.6023844136342,-6.60941750115261));
#34768=CARTESIAN_POINT('Ctrl Pts',(56.8715502213248,57.023876371777,-6.64838971378304));
#34769=CARTESIAN_POINT('Ctrl Pts',(56.4217991870814,57.5800312207779,-6.68736192641346));
#34770=CARTESIAN_POINT('Ctrl Pts',(56.1299141849854,58.210937755608,-6.72633413904389));
#34771=CARTESIAN_POINT('Ctrl Pts',(55.8380291828894,58.841844290438,-6.76530635167432));
#34772=CARTESIAN_POINT('Ctrl Pts',(55.7040102129408,59.5475025110972,-6.80427856430475));
#34773=CARTESIAN_POINT('Ctrl Pts',(55.7435430368397,60.2424382218237,-6.84325077693518));
#34774=CARTESIAN_POINT('Ctrl Pts',(55.7830758607386,60.9373739325502,-6.88222298956561));
#34775=CARTESIAN_POINT('Ctrl Pts',(55.9961604784851,61.6215871333439,-6.92119520219604));
#34776=CARTESIAN_POINT('Ctrl Pts',(56.3577826916297,62.2158268315062,-6.96016741482647));
#34777=CARTESIAN_POINT('Ctrl Pts',(56.7194049047743,62.8100665296684,-6.9991396274569));
#34778=CARTESIAN_POINT('Ctrl Pts',(57.229564713317,63.3143327251992,-7.03811184008733));
#34779=CARTESIAN_POINT('Ctrl Pts',(57.8282806977002,63.6688083962819,-7.07708405271776));
#34780=CARTESIAN_POINT('Ctrl Pts',(58.4269966820833,64.0232840673647,-7.11605626534819));
#34781=CARTESIAN_POINT('Ctrl Pts',(59.114268842307,64.2279692139995,-7.15502847797862));
#34782=CARTESIAN_POINT('Ctrl Pts',(59.8093191206801,64.259056050085,-7.19400069060905));
#34783=CARTESIAN_POINT('Ctrl Pts',(60.5043693990532,64.2901428861706,-7.23297290323948));
#34784=CARTESIAN_POINT('Ctrl Pts',(61.2071977955758,64.147631411707,-7.27194511586991));
#34785=CARTESIAN_POINT('Ctrl Pts',(61.8351875016575,63.8481564596784,-7.31091732850034));
#34786=CARTESIAN_POINT('Ctrl Pts',(62.4631772077392,63.5486815076498,-7.34988954113077));
#34787=CARTESIAN_POINT('Ctrl Pts',(63.0163282233802,63.0922430780563,-7.3888617537612));
#34788=CARTESIAN_POINT('Ctrl Pts',(63.4296222037564,62.5325469979949,-7.42783396639163));
#34789=CARTESIAN_POINT('Ctrl Pts',(63.8429161841327,61.9728509179335,-7.46680617902206));
#34790=CARTESIAN_POINT('Ctrl Pts',(64.1163531292443,61.3098971874042,-7.50577839165249));
#34791=CARTESIAN_POINT('Ctrl Pts',(64.2177913481944,60.6215873296248,-7.54475060428292));
#34792=CARTESIAN_POINT('Ctrl Pts',(64.2480979428419,60.4159416857293,-7.55639429305164));
#34793=CARTESIAN_POINT('Ctrl Pts',(64.2630514303516,60.2080326800812,-7.56803798182035));
#34794=CARTESIAN_POINT('Ctrl Pts',(64.2628730117989,60.0000978162778,-7.57968167058906));
#34795=CARTESIAN_POINT('Origin',(60.,60.,-6.));
#34796=CARTESIAN_POINT('',(64.2632129797225,60.0000762878951,-9.07968167058906));
#34797=CARTESIAN_POINT('',(64.2626696975502,60.0000007546914,-8.67031832941094));
#34798=CARTESIAN_POINT('',(64.263,60.,-6.));
#34799=CARTESIAN_POINT('',(56.7766472160421,62.7898325810254,-10.));
#34800=CARTESIAN_POINT('Ctrl Pts',(64.2632129797225,60.0000762878951,-9.07968167058906));
#34801=CARTESIAN_POINT('Ctrl Pts',(64.2627031079153,59.3936235463162,-9.11364895864636));
#34802=CARTESIAN_POINT('Ctrl Pts',(64.1318733360967,58.7869579650774,-9.14761624670367));
#34803=CARTESIAN_POINT('Ctrl Pts',(63.8808238664535,58.2349684131022,-9.18158353476097));
#34804=CARTESIAN_POINT('Ctrl Pts',(63.5927834054316,57.6016457247243,-9.2205557473914));
#34805=CARTESIAN_POINT('Ctrl Pts',(63.1464855503109,57.0402986448989,-9.25952796002183));
#34806=CARTESIAN_POINT('Ctrl Pts',(62.5943907357823,56.6169137625735,-9.29850017265227));
#34807=CARTESIAN_POINT('Ctrl Pts',(62.0422959212538,56.1935288802482,-9.3374723852827));
#34808=CARTESIAN_POINT('Ctrl Pts',(61.3844041473173,55.908106195423,-9.37644459791312));
#34809=CARTESIAN_POINT('Ctrl Pts',(60.6980457486418,55.7941882630383,-9.41541681054355));
#34810=CARTESIAN_POINT('Ctrl Pts',(60.0116873499663,55.6802703306536,-9.45438902317398));
#34811=CARTESIAN_POINT('Ctrl Pts',(59.2968623265517,55.7378571507094,-9.49336123580441));
#34812=CARTESIAN_POINT('Ctrl Pts',(58.6375973357764,55.9601951486079,-9.53233344843484));
#34813=CARTESIAN_POINT('Ctrl Pts',(57.9783323450012,56.1825331465064,-9.57130566106527));
#34814=CARTESIAN_POINT('Ctrl Pts',(57.3746273868654,56.5696223222476,-9.6102778736957));
#34815=CARTESIAN_POINT('Ctrl Pts',(56.8974397908448,57.0759277155521,-9.64925008632613));
#34816=CARTESIAN_POINT('Ctrl Pts',(56.4202521948243,57.5822331088567,-9.68822229895656));
#34817=CARTESIAN_POINT('Ctrl Pts',(56.069581960919,58.2077547197246,-9.72719451158699));
#34818=CARTESIAN_POINT('Ctrl Pts',(55.8866652329043,58.8790351869383,-9.76616672421742));
#34819=CARTESIAN_POINT('Ctrl Pts',(55.7037485048897,59.550315654152,-9.80513893684785));
#34820=CARTESIAN_POINT('Ctrl Pts',(55.6885852827656,60.2673549777114,-9.84411114947828));
#34821=CARTESIAN_POINT('Ctrl Pts',(55.8429524134795,60.9456840068003,-9.88308336210871));
#34822=CARTESIAN_POINT('Ctrl Pts',(55.9973195441935,61.6240130358892,-9.92205557473914));
#34823=CARTESIAN_POINT('Ctrl Pts',(56.3212170277455,62.2636317705077,-9.96102778736957));
#34824=CARTESIAN_POINT('Ctrl Pts',(56.7766472160421,62.7898325810254,-10.));
#34825=CARTESIAN_POINT('',(63.2235668510161,62.7899187021734,-10.));
#34826=CARTESIAN_POINT('Origin',(60.,60.,-10.));
#34827=CARTESIAN_POINT('Ctrl Pts',(63.2235668510161,62.7899187021734,-10.));
#34828=CARTESIAN_POINT('Ctrl Pts',(62.8262375922137,63.2482129590446,-9.96602721186203));
#34829=CARTESIAN_POINT('Ctrl Pts',(62.3301928947912,63.6213495469796,-9.93205442372405));
#34830=CARTESIAN_POINT('Ctrl Pts',(61.7790228005731,63.8744287531187,-9.89808163558608));
#34831=CARTESIAN_POINT('Ctrl Pts',(61.1467426939136,64.1647510132151,-9.85910942295565));
#34832=CARTESIAN_POINT('Ctrl Pts',(60.4419189254527,64.2970807216377,-9.82013721032522));
#34833=CARTESIAN_POINT('Ctrl Pts',(59.7473945403606,64.2558578814904,-9.78116499769479));
#34834=CARTESIAN_POINT('Ctrl Pts',(59.0528701552686,64.2146350413431,-9.74219278506436));
#34835=CARTESIAN_POINT('Ctrl Pts',(58.3686451535453,63.999859652626,-9.70322057243393));
#34836=CARTESIAN_POINT('Ctrl Pts',(57.7751487629232,63.636779812551,-9.6642483598035));
#34837=CARTESIAN_POINT('Ctrl Pts',(57.1816523723011,63.2736999724761,-9.62527614717307));
#34838=CARTESIAN_POINT('Ctrl Pts',(56.6788845927801,62.7623156810432,-9.58630393454264));
#34839=CARTESIAN_POINT('Ctrl Pts',(56.3259418994758,62.1627361892336,-9.54733172191221));
#34840=CARTESIAN_POINT('Ctrl Pts',(55.9729992061715,61.563156697424,-9.50835950928178));
#34841=CARTESIAN_POINT('Ctrl Pts',(55.769881599084,60.8753820052377,-9.46938729665136));
#34842=CARTESIAN_POINT('Ctrl Pts',(55.7404649362495,60.1802567469978,-9.43041508402093));
#34843=CARTESIAN_POINT('Ctrl Pts',(55.711048273415,59.4851314887579,-9.3914428713905));
#34844=CARTESIAN_POINT('Ctrl Pts',(55.8553325548336,58.7826556644645,-9.35247065876007));
#34845=CARTESIAN_POINT('Ctrl Pts',(56.1563577258025,58.1554011721684,-9.31349844612963));
#34846=CARTESIAN_POINT('Ctrl Pts',(56.4573828967714,57.5281466798722,-9.2745262334992));
#34847=CARTESIAN_POINT('Ctrl Pts',(56.9151489572907,56.9761135195733,-9.23555402086877));
#34848=CARTESIAN_POINT('Ctrl Pts',(57.4758481529971,56.5641902504204,-9.19658180823834));
#34849=CARTESIAN_POINT('Ctrl Pts',(58.0365473487036,56.1522669812675,-9.15760959560791));
#34850=CARTESIAN_POINT('Ctrl Pts',(58.7001796795971,55.8804536032608,-9.11863738297749));
#34851=CARTESIAN_POINT('Ctrl Pts',(59.3887387820797,55.7807002126255,-9.07966517034706));
#34852=CARTESIAN_POINT('Ctrl Pts',(60.0772978845623,55.6809468219902,-9.04069295771663));
#34853=CARTESIAN_POINT('Ctrl Pts',(60.7907837586341,55.7532534187264,-9.00172074508619));
#34854=CARTESIAN_POINT('Ctrl Pts',(61.4453301273351,55.9891208068635,-8.96274853245576));
#34855=CARTESIAN_POINT('Ctrl Pts',(62.0998764960362,56.2249881950005,-8.92377631982533));
#34856=CARTESIAN_POINT('Ctrl Pts',(62.6954833593665,56.6244163745384,-8.88480410719491));
#34857=CARTESIAN_POINT('Ctrl Pts',(63.1621403861375,57.1404547199397,-8.84583189456448));
#34858=CARTESIAN_POINT('Ctrl Pts',(63.6287974129085,57.6564930653411,-8.80685968193405));
#34859=CARTESIAN_POINT('Ctrl Pts',(63.9665046031202,58.2891415766059,-8.76788746930362));
#34860=CARTESIAN_POINT('Ctrl Pts',(64.1355664178555,58.9640360217668,-8.72891525667319));
#34861=CARTESIAN_POINT('Ctrl Pts',(64.2202977532714,59.3022833527375,-8.70938294758577));
#34862=CARTESIAN_POINT('Ctrl Pts',(64.2626675734433,59.6511423104289,-8.68985063849836));
#34863=CARTESIAN_POINT('Ctrl Pts',(64.2626696975502,60.0000007546914,-8.67031832941094));
#34864=CARTESIAN_POINT('Origin',(60.,60.,-13.3123464956316));
#34865=CARTESIAN_POINT('',(65.0994142723023,60.0000080970367,-3.68765350436841));
#34866=CARTESIAN_POINT('',(65.0991104422254,59.9998849527226,-3.56234649563159));
#34867=CARTESIAN_POINT('',(65.099,59.9999999999999,-13.3123464956316));
#34868=CARTESIAN_POINT('',(56.3967816198432,63.607855083689,-3.));
#34869=CARTESIAN_POINT('Ctrl Pts',(65.0991104422254,59.9998849527226,-3.56234649563159));
#34870=CARTESIAN_POINT('Ctrl Pts',(65.098461631149,60.6739141965835,-3.53078651427611));
#34871=CARTESIAN_POINT('Ctrl Pts',(64.7978132036202,62.1808417610638,-3.46025432029021));
#34872=CARTESIAN_POINT('Ctrl Pts',(63.3555842661093,64.1119168678935,-3.35074991367387));
#34873=CARTESIAN_POINT('Ctrl Pts',(61.027044706866,65.2070699669712,-3.23383327578258));
#34874=CARTESIAN_POINT('Ctrl Pts',(58.4567442007043,65.0779746991923,-3.11691663789129));
#34875=CARTESIAN_POINT('Ctrl Pts',(56.9857510552448,64.1960675938266,-3.03897221263043));
#34876=CARTESIAN_POINT('Ctrl Pts',(56.3967816198432,63.6078550836889,-3.));
#34877=CARTESIAN_POINT('',(55.0736213347631,61.3165318688511,-3.));
#34878=CARTESIAN_POINT('Origin',(60.,60.,-3.));
#34879=CARTESIAN_POINT('Ctrl Pts',(65.0994142723023,60.0000080970367,-3.68765350436841));
#34880=CARTESIAN_POINT('Ctrl Pts',(65.0994150596659,60.0082074395616,-3.68726952086906));
#34881=CARTESIAN_POINT('Ctrl Pts',(65.097429063898,60.8485945549625,-3.64791332473928));
#34882=CARTESIAN_POINT('Ctrl Pts',(64.6714138007994,62.5191327746011,-3.56958491597908));
#34883=CARTESIAN_POINT('Ctrl Pts',(62.93732429588,64.4204364118546,-3.45266827808779));
#34884=CARTESIAN_POINT('Ctrl Pts',(60.5127057455321,65.2825431684356,-3.3357516401965));
#34885=CARTESIAN_POINT('Ctrl Pts',(57.967548471337,64.9027852181516,-3.2188350023052));
#34886=CARTESIAN_POINT('Ctrl Pts',(55.988614157022,63.4359554976302,-3.10691778890638));
#34887=CARTESIAN_POINT('Ctrl Pts',(55.2615313835496,62.0172737121676,-3.03397278813797));
#34888=CARTESIAN_POINT('Ctrl Pts',(55.0736213347631,61.3165318688511,-3.));
#34889=CARTESIAN_POINT('Origin',(60.,60.,-13.3123464956316));
#34890=CARTESIAN_POINT('',(65.0992594973497,59.9999349240322,-5.18765350436841));
#34891=CARTESIAN_POINT('',(65.0987279539713,59.9999119474263,-5.06234649563159));
#34892=CARTESIAN_POINT('',(65.099,59.9999999999999,-13.3123464956316));
#34893=CARTESIAN_POINT('Ctrl Pts',(65.0987279539713,59.9999119474263,-5.06234649563159));
#34894=CARTESIAN_POINT('Ctrl Pts',(65.0983788696902,60.5322706383878,-5.0374252784717));
#34895=CARTESIAN_POINT('Ctrl Pts',(64.8854638827286,61.8974113431707,-4.97353184868138));
#34896=CARTESIAN_POINT('Ctrl Pts',(63.6865889794253,63.8180111190031,-4.87066620626063));
#34897=CARTESIAN_POINT('Ctrl Pts',(61.4572740950116,65.1033792767411,-4.75374956836934));
#34898=CARTESIAN_POINT('Ctrl Pts',(58.8853714589078,65.189001781766,-4.63683293047805));
#34899=CARTESIAN_POINT('Ctrl Pts',(56.5755050441849,64.0547463443016,-4.51991629258676));
#34900=CARTESIAN_POINT('Ctrl Pts',(55.0706998168725,61.9672654489506,-4.40299965469547));
#34901=CARTESIAN_POINT('Ctrl Pts',(54.7247182017831,59.4173019594712,-4.28608301680418));
#34902=CARTESIAN_POINT('Ctrl Pts',(55.6188973320329,57.0043245192968,-4.16916637891289));
#34903=CARTESIAN_POINT('Ctrl Pts',(57.5430244185373,55.2955969820173,-4.0522497410216));
#34904=CARTESIAN_POINT('Ctrl Pts',(60.0447608866429,54.6928229271066,-3.93533310313032));
#34905=CARTESIAN_POINT('Ctrl Pts',(62.5359710846191,55.3377065632379,-3.81841646523902));
#34906=CARTESIAN_POINT('Ctrl Pts',(64.4310101049653,57.0786456054826,-3.70149982734774));
#34907=CARTESIAN_POINT('Ctrl Pts',(65.0540042126791,58.8510320510013,-3.61614317081192));
#34908=CARTESIAN_POINT('Ctrl Pts',(65.0992628231061,59.8415812900777,-3.56975872690654));
#34909=CARTESIAN_POINT('Ctrl Pts',(65.0991104422254,59.9998849527226,-3.56234649563159));
#34910=CARTESIAN_POINT('Ctrl Pts',(65.0992594973497,59.9999349240322,-5.18765350436841));
#34911=CARTESIAN_POINT('Ctrl Pts',(65.0986258598593,60.6986618672511,-5.15493607243422));
#34912=CARTESIAN_POINT('Ctrl Pts',(64.7810044222689,62.2301463492343,-5.0832464278696));
#34913=CARTESIAN_POINT('Ctrl Pts',(63.2955109480772,64.1603278329295,-4.97258457067455));
#34914=CARTESIAN_POINT('Ctrl Pts',(60.9510823128121,65.2214359708436,-4.85566793278326));
#34915=CARTESIAN_POINT('Ctrl Pts',(58.3831734117936,65.0550993752034,-4.73875129489197));
#34916=CARTESIAN_POINT('Ctrl Pts',(56.1953122098592,63.7003384596412,-4.62183465700068));
#34917=CARTESIAN_POINT('Ctrl Pts',(54.9019142936214,61.4756811820325,-4.50491801910939));
#34918=CARTESIAN_POINT('Ctrl Pts',(54.8070090801581,58.9041019292639,-4.3880013812181));
#34919=CARTESIAN_POINT('Ctrl Pts',(55.9329235426593,56.5901588022821,-4.27108474332681));
#34920=CARTESIAN_POINT('Ctrl Pts',(58.0149603175651,55.0778303762239,-4.15416810543552));
#34921=CARTESIAN_POINT('Ctrl Pts',(60.5636590493342,54.7226500811105,-4.03725146754424));
#34922=CARTESIAN_POINT('Ctrl Pts',(62.9798472108349,55.6081160860788,-3.92033482965294));
#34923=CARTESIAN_POINT('Ctrl Pts',(64.6898720162157,57.5197664101291,-3.803802175261));
#34924=CARTESIAN_POINT('Ctrl Pts',(65.0993351465935,59.1760192834263,-3.72624173349949));
#34925=CARTESIAN_POINT('Ctrl Pts',(65.0994142723023,60.0000080970367,-3.68765350436841));
#34926=CARTESIAN_POINT('Origin',(60.,60.,-13.3123464956316));
#34927=CARTESIAN_POINT('',(65.0984547190409,59.9994231828803,-6.68765350436841));
#34928=CARTESIAN_POINT('',(65.0986380343512,60.0064451752286,-6.56234649563159));
#34929=CARTESIAN_POINT('',(65.099,59.9999999999999,-13.3123464956316));
#34930=CARTESIAN_POINT('Ctrl Pts',(65.0986380343512,60.0064451752286,-6.56234649563159));
#34931=CARTESIAN_POINT('Ctrl Pts',(65.1022613453585,60.3972054217194,-6.54406404266729));
#34932=CARTESIAN_POINT('Ctrl Pts',(64.8866739179056,62.4488199389438,-6.44783716444213));
#34933=CARTESIAN_POINT('Ctrl Pts',(62.7388658113806,64.8816655541704,-6.31263807358654));
#34934=CARTESIAN_POINT('Ctrl Pts',(59.3187584788532,65.2585195543855,-6.15674922306482));
#34935=CARTESIAN_POINT('Ctrl Pts',(56.9266335796149,64.3285139675122,-6.03983258517353));
#34936=CARTESIAN_POINT('Ctrl Pts',(55.2511526541055,62.3700211957414,-5.92291594728224));
#34937=CARTESIAN_POINT('Ctrl Pts',(54.6947972197688,59.8594460319768,-5.80599930939095));
#34938=CARTESIAN_POINT('Ctrl Pts',(55.3843760081973,57.3795654934784,-5.68908267149966));
#34939=CARTESIAN_POINT('Ctrl Pts',(57.1596209351837,55.5168092181914,-5.57216603360837));
#34940=CARTESIAN_POINT('Ctrl Pts',(59.6023370896801,54.7074973445116,-5.45524939571708));
#34941=CARTESIAN_POINT('Ctrl Pts',(62.138664673409,55.1426278237003,-5.33833275782579));
#34942=CARTESIAN_POINT('Ctrl Pts',(64.1721578471653,56.7195645494213,-5.2214161199345));
#34943=CARTESIAN_POINT('Ctrl Pts',(65.0004645732374,58.5672219271665,-5.1294206992031));
#34944=CARTESIAN_POINT('Ctrl Pts',(65.0989247734775,59.6997592900575,-5.07639749110213));
#34945=CARTESIAN_POINT('Ctrl Pts',(65.0987279539713,59.9999119474263,-5.06234649563159));
#34946=CARTESIAN_POINT('Ctrl Pts',(65.0984547190409,59.9994231828803,-6.68765350436841));
#34947=CARTESIAN_POINT('Ctrl Pts',(65.097455978134,60.5556872072211,-6.66157483662981));
#34948=CARTESIAN_POINT('Ctrl Pts',(64.8688835602887,61.943672278096,-6.59652395626078));
#34949=CARTESIAN_POINT('Ctrl Pts',(63.1773281761085,64.6083211110609,-6.45352865063088));
#34950=CARTESIAN_POINT('Ctrl Pts',(58.6661397561353,65.8440762220129,-6.25866758747874));
#34951=CARTESIAN_POINT('Ctrl Pts',(54.3971986841152,62.1309686655549,-6.02483431169616));
#34952=CARTESIAN_POINT('Ctrl Pts',(54.9957816802558,57.4920452935348,-5.82997324854401));
#34953=CARTESIAN_POINT('Ctrl Pts',(57.6170719268681,55.2631467174745,-5.67408439802229));
#34954=CARTESIAN_POINT('Ctrl Pts',(60.1194257717932,54.6927078330755,-5.557167760131));
#34955=CARTESIAN_POINT('Ctrl Pts',(62.6046743394157,55.3756921094109,-5.44025112223971));
#34956=CARTESIAN_POINT('Ctrl Pts',(64.4724884051625,57.1431171033903,-5.32333448434842));
#34957=CARTESIAN_POINT('Ctrl Pts',(65.062116481349,58.900523352424,-5.23913527839132));
#34958=CARTESIAN_POINT('Ctrl Pts',(65.0993806334936,59.8663552529511,-5.19390828506465));
#34959=CARTESIAN_POINT('Ctrl Pts',(65.0992594973497,59.9999349240322,-5.18765350436841));
#34960=CARTESIAN_POINT('Origin',(60.,60.,-13.3123464956316));
#34961=CARTESIAN_POINT('',(65.0986049232486,60.0000009026908,-8.18765350436841));
#34962=CARTESIAN_POINT('',(65.098848108647,60.0001169986396,-8.06234649563159));
#34963=CARTESIAN_POINT('',(65.099,59.9999999999999,-13.3123464956316));
#34964=CARTESIAN_POINT('Ctrl Pts',(65.098848108647,60.0001169986396,-8.06234649563159));
#34965=CARTESIAN_POINT('Ctrl Pts',(65.0990615161536,60.2488291427947,-8.05070280686288));
#34966=CARTESIAN_POINT('Ctrl Pts',(65.0213100551162,61.3298631785982,-8.00008690546373));
#34967=CARTESIAN_POINT('Ctrl Pts',(64.2694756368211,63.1527018302866,-7.91049879143416));
#34968=CARTESIAN_POINT('Ctrl Pts',(62.2845938431877,64.7905481022763,-7.79358215354287));
#34969=CARTESIAN_POINT('Ctrl Pts',(59.7626219966935,65.301924603536,-7.67666551565158));
#34970=CARTESIAN_POINT('Ctrl Pts',(57.2964708742581,64.5674491899606,-7.55974887776029));
#34971=CARTESIAN_POINT('Ctrl Pts',(55.4658552065881,62.7579816804522,-7.442832239869));
#34972=CARTESIAN_POINT('Ctrl Pts',(54.7012398189108,60.3028070774634,-7.32591560197771));
#34973=CARTESIAN_POINT('Ctrl Pts',(55.1821425126253,57.7706809218396,-7.20899896408643));
#34974=CARTESIAN_POINT('Ctrl Pts',(56.7959922829326,55.7750204186338,-7.09208232619513));
#34975=CARTESIAN_POINT('Ctrl Pts',(59.9512914978166,54.4027085123842,-6.93619347567342));
#34976=CARTESIAN_POINT('Ctrl Pts',(63.9644744788023,55.7663648990069,-6.75961486548557));
#34977=CARTESIAN_POINT('Ctrl Pts',(65.0868139163643,58.7312592334816,-6.62200846792815));
#34978=CARTESIAN_POINT('Ctrl Pts',(65.0986380343512,60.0064451752286,-6.56234649563159));
#34979=CARTESIAN_POINT('Ctrl Pts',(65.0986049232486,60.0000009026908,-8.18765350436841));
#34980=CARTESIAN_POINT('Ctrl Pts',(65.098607451886,60.4152985173152,-8.1682136008254));
#34981=CARTESIAN_POINT('Ctrl Pts',(64.9477827347253,61.6631636070336,-8.10980148465196));
#34982=CARTESIAN_POINT('Ctrl Pts',(63.9406234579031,63.5552235763429,-8.01241715584808));
#34983=CARTESIAN_POINT('Ctrl Pts',(61.8050635087969,64.9909811652868,-7.89550051795679));
#34984=CARTESIAN_POINT('Ctrl Pts',(59.2451498198411,65.2534097530527,-7.7785838800655));
#34985=CARTESIAN_POINT('Ctrl Pts',(56.8627001620859,64.2808297817029,-7.66166724217421));
#34986=CARTESIAN_POINT('Ctrl Pts',(55.2177796069362,62.3018527370191,-7.54475060428292));
#34987=CARTESIAN_POINT('Ctrl Pts',(54.6971392652592,59.7817817811634,-7.42783396639163));
#34988=CARTESIAN_POINT('Ctrl Pts',(55.4230712085558,57.3129118130677,-7.31091732850034));
#34989=CARTESIAN_POINT('Ctrl Pts',(57.2251429658425,55.4759618040439,-7.19400069060905));
#34990=CARTESIAN_POINT('Ctrl Pts',(59.6792193933806,54.7020984074429,-7.07708405271776));
#34991=CARTESIAN_POINT('Ctrl Pts',(62.2094284211809,55.174716747074,-6.96016741482647));
#34992=CARTESIAN_POINT('Ctrl Pts',(64.2186721193591,56.7795408043723,-6.84325077693519));
#34993=CARTESIAN_POINT('Ctrl Pts',(65.0118140711112,58.6182636268587,-6.75241280678249));
#34994=CARTESIAN_POINT('Ctrl Pts',(65.0989485061794,59.7244008833735,-6.70054704926024));
#34995=CARTESIAN_POINT('Ctrl Pts',(65.0984547190409,59.9994231828803,-6.68765350436841));
#34996=CARTESIAN_POINT('Origin',(60.,60.,-13.3123464956316));
#34997=CARTESIAN_POINT('',(65.0987893697715,60.0001196244759,-9.68765350436842));
#34998=CARTESIAN_POINT('',(65.0992547463301,60.0000912484111,-9.56234649563159));
#34999=CARTESIAN_POINT('',(65.099,59.9999999999999,-13.3123464956316));
#35000=CARTESIAN_POINT('',(61.322884965569,55.0755938055567,-10.));
#35001=CARTESIAN_POINT('Ctrl Pts',(61.322884965569,55.0755938055567,-10.));
#35002=CARTESIAN_POINT('Ctrl Pts',(62.1267766598728,55.2915500435982,-9.96102778736957));
#35003=CARTESIAN_POINT('Ctrl Pts',(63.6260271731292,56.1245140078271,-9.88308336210872));
#35004=CARTESIAN_POINT('Ctrl Pts',(64.8700259230263,58.049261551967,-9.77896786356485));
#35005=CARTESIAN_POINT('Ctrl Pts',(65.0983672436226,59.4410930803254,-9.71382457765142));
#35006=CARTESIAN_POINT('Ctrl Pts',(65.0987893697715,60.0001196244759,-9.68765350436842));
#35007=CARTESIAN_POINT('',(58.6769607112098,55.0753649997562,-10.));
#35008=CARTESIAN_POINT('Origin',(60.,60.,-10.));
#35009=CARTESIAN_POINT('Ctrl Pts',(58.6769607112098,55.0753649997562,-10.));
#35010=CARTESIAN_POINT('Ctrl Pts',(59.3777759733541,54.8877289534041,-9.96602721186202));
#35011=CARTESIAN_POINT('Ctrl Pts',(60.9699318229197,54.808060215244,-9.89308221109362));
#35012=CARTESIAN_POINT('Ctrl Pts',(63.2297107806181,55.7884527399271,-9.78116499769479));
#35013=CARTESIAN_POINT('Ctrl Pts',(64.7626147903817,57.7165175505922,-9.66925328437663));
#35014=CARTESIAN_POINT('Ctrl Pts',(65.0986448855876,59.2747094681366,-9.5963137836889));
#35015=CARTESIAN_POINT('Ctrl Pts',(65.0992547463301,60.0000912484111,-9.56234649563159));
#35016=CARTESIAN_POINT('Origin',(-60.,60.,-6.));
#35017=CARTESIAN_POINT('',(-55.7372273834134,59.9999263798756,-4.57968167058906));
#35018=CARTESIAN_POINT('',(-55.7366536686051,60.0000067695234,-4.17031832941094));
#35019=CARTESIAN_POINT('',(-55.737,60.,-6.));
#35020=CARTESIAN_POINT('',(-59.1956105045055,55.8135783132205,-3.));
#35021=CARTESIAN_POINT('Ctrl Pts',(-55.7366536686051,60.0000067695234,-4.17031832941094));
#35022=CARTESIAN_POINT('Ctrl Pts',(-55.7366530103325,60.0068617993376,-4.16993434591159));
#35023=CARTESIAN_POINT('Ctrl Pts',(-55.7366692100737,60.0137168260256,-4.16955036241224));
#35024=CARTESIAN_POINT('Ctrl Pts',(-55.7367022869973,60.0205717712724,-4.16916637891289));
#35025=CARTESIAN_POINT('Ctrl Pts',(-55.74005941276,60.7163110001195,-4.13019416628246));
#35026=CARTESIAN_POINT('Ctrl Pts',(-55.9172706415258,61.4112112921654,-4.09122195365204));
#35027=CARTESIAN_POINT('Ctrl Pts',(-56.2475061025821,62.0235910770971,-4.05224974102161));
#35028=CARTESIAN_POINT('Ctrl Pts',(-56.5777415636384,62.6359708620289,-4.01327752839118));
#35029=CARTESIAN_POINT('Ctrl Pts',(-57.0610012569851,63.1658301398464,-3.97430531576075));
#35030=CARTESIAN_POINT('Ctrl Pts',(-57.6404799899334,63.5508866362206,-3.93533310313031));
#35031=CARTESIAN_POINT('Ctrl Pts',(-58.2199587228817,63.9359431325947,-3.89636089049988));
#35032=CARTESIAN_POINT('Ctrl Pts',(-58.8956564954316,64.1761968475256,-3.85738867786946));
#35033=CARTESIAN_POINT('Ctrl Pts',(-59.5881502605052,64.2434078352681,-3.81841646523903));
#35034=CARTESIAN_POINT('Ctrl Pts',(-60.2806440255789,64.3106188230106,-3.7794442526086));
#35035=CARTESIAN_POINT('Ctrl Pts',(-60.9899337831764,64.2047870835648,-3.74047203997817));
#35036=CARTESIAN_POINT('Ctrl Pts',(-61.6326432518039,63.9383513901597,-3.70149982734774));
#35037=CARTESIAN_POINT('Ctrl Pts',(-62.2753527204313,63.6719156967547,-3.66252761471731));
#35038=CARTESIAN_POINT('Ctrl Pts',(-62.8514819000888,63.2448760493903,-3.62355540208688));
#35039=CARTESIAN_POINT('Ctrl Pts',(-63.2933169215645,62.7074312082618,-3.58458318945645));
#35040=CARTESIAN_POINT('Ctrl Pts',(-63.7351519430401,62.1699863671332,-3.54561097682602));
#35041=CARTESIAN_POINT('Ctrl Pts',(-64.0426928063339,61.5221363322404,-3.50663876419559));
#35042=CARTESIAN_POINT('Ctrl Pts',(-64.1797749455836,60.8400271011362,-3.46766655156516));
#35043=CARTESIAN_POINT('Ctrl Pts',(-64.3168570848332,60.1579178700319,-3.42869433893473));
#35044=CARTESIAN_POINT('Ctrl Pts',(-64.2834805000387,59.4415494427162,-3.3897221263043));
#35045=CARTESIAN_POINT('Ctrl Pts',(-64.0836009653472,58.7751401645266,-3.35074991367387));
#35046=CARTESIAN_POINT('Ctrl Pts',(-63.8837214306558,58.1087308863369,-3.31177770104344));
#35047=CARTESIAN_POINT('Ctrl Pts',(-63.5173389460674,57.4922807572733,-3.27280548841301));
#35048=CARTESIAN_POINT('Ctrl Pts',(-63.0274513684703,56.9982299650024,-3.23383327578258));
#35049=CARTESIAN_POINT('Ctrl Pts',(-62.5375637908732,56.5041791727314,-3.19486106315215));
#35050=CARTESIAN_POINT('Ctrl Pts',(-61.9241711202674,56.1325277172532,-3.15588885052172));
#35051=CARTESIAN_POINT('Ctrl Pts',(-61.2595373895626,55.9270490755113,-3.11691663789129));
#35052=CARTESIAN_POINT('Ctrl Pts',(-60.5949036588578,55.7215704337695,-3.07794442526086));
#35053=CARTESIAN_POINT('Ctrl Pts',(-59.8790288680541,55.6822646057641,-3.03897221263043));
#35054=CARTESIAN_POINT('Ctrl Pts',(-59.1956105045055,55.8135783132205,-3.));
#35055=CARTESIAN_POINT('',(-55.972076043732,61.3967314412509,-3.00000000000001));
#35056=CARTESIAN_POINT('Origin',(-60.,60.,-3.));
#35057=CARTESIAN_POINT('',(-55.7369075951045,59.9999038083371,-3.07968167058906));
#35058=CARTESIAN_POINT('Ctrl Pts',(-55.972076043732,61.3967314412509,-3.00000000000001));
#35059=CARTESIAN_POINT('Ctrl Pts',(-55.8170962766014,60.9485583511405,-3.02656055686302));
#35060=CARTESIAN_POINT('Ctrl Pts',(-55.7373641065468,60.4741561734832,-3.05312111372604));
#35061=CARTESIAN_POINT('Ctrl Pts',(-55.7369075951045,59.9999038083371,-3.07968167058906));
#35062=CARTESIAN_POINT('',(-55.737,60.,-2.));
#35063=CARTESIAN_POINT('',(-55.737,60.,-6.));
#35064=CARTESIAN_POINT('Origin',(-60.,60.,-2.));
#35065=CARTESIAN_POINT('Ctrl Pts',(-55.7369075951045,59.9999038083371,-3.07968167058906));
#35066=CARTESIAN_POINT('Ctrl Pts',(-55.7367801968573,59.8675546173436,-3.08709390186401));
#35067=CARTESIAN_POINT('Ctrl Pts',(-55.7428267531846,59.7352170936848,-3.09450613313896));
#35068=CARTESIAN_POINT('Ctrl Pts',(-55.7551348091079,59.6034645506898,-3.10191836441391));
#35069=CARTESIAN_POINT('Ctrl Pts',(-55.8198484094689,58.9107327767164,-3.14089057704434));
#35070=CARTESIAN_POINT('Ctrl Pts',(-56.0576594161103,58.2341726296972,-3.17986278967477));
#35071=CARTESIAN_POINT('Ctrl Pts',(-56.4406216430255,57.6533082825818,-3.2188350023052));
#35072=CARTESIAN_POINT('Ctrl Pts',(-56.8235838699406,57.0724439354665,-3.25780721493563));
#35073=CARTESIAN_POINT('Ctrl Pts',(-57.3516973171296,56.5872753882551,-3.29677942756606));
#35074=CARTESIAN_POINT('Ctrl Pts',(-57.9628818847596,56.254832352553,-3.33575164019649));
#35075=CARTESIAN_POINT('Ctrl Pts',(-58.5740664523896,55.9223893168508,-3.37472385282692));
#35076=CARTESIAN_POINT('Ctrl Pts',(-59.2683221404606,55.742671792658,-3.41369606545735));
#35077=CARTESIAN_POINT('Ctrl Pts',(-59.9640445684598,55.7368041996945,-3.45266827808778));
#35078=CARTESIAN_POINT('Ctrl Pts',(-60.659766996459,55.730936606731,-3.49164049071821));
#35079=CARTESIAN_POINT('Ctrl Pts',(-61.3569561643863,55.8989189449969,-3.53061270334864));
#35080=CARTESIAN_POINT('Ctrl Pts',(-61.9736606357888,56.2210060021645,-3.56958491597907));
#35081=CARTESIAN_POINT('Ctrl Pts',(-62.5903651071913,56.543093059332,-3.6085571286095));
#35082=CARTESIAN_POINT('Ctrl Pts',(-63.1265848820691,57.0192848354013,-3.64752934123993));
#35083=CARTESIAN_POINT('Ctrl Pts',(-63.5192906276179,57.5936075318196,-3.68650155387036));
#35084=CARTESIAN_POINT('Ctrl Pts',(-63.9119963731668,58.1679302282379,-3.72547376650079));
#35085=CARTESIAN_POINT('Ctrl Pts',(-64.1611880893868,58.8403838450051,-3.76444597913122));
#35086=CARTESIAN_POINT('Ctrl Pts',(-64.2375745063077,59.5319252415894,-3.80341819176165));
#35087=CARTESIAN_POINT('Ctrl Pts',(-64.3139609232287,60.2234666381736,-3.84239040439208));
#35088=CARTESIAN_POINT('Ctrl Pts',(-64.2175420408506,60.9340958145749,-3.88136261702251));
#35089=CARTESIAN_POINT('Ctrl Pts',(-63.9596514602529,61.5802821811732,-3.92033482965294));
#35090=CARTESIAN_POINT('Ctrl Pts',(-63.7017608796552,62.2264685477715,-3.95930704228337));
#35091=CARTESIAN_POINT('Ctrl Pts',(-63.2823986008379,62.8082121045669,-3.9982792549138));
#35092=CARTESIAN_POINT('Ctrl Pts',(-62.7508582516328,63.2571322255563,-4.03725146754423));
#35093=CARTESIAN_POINT('Ctrl Pts',(-62.2193179024276,63.7060523465458,-4.07622368017466));
#35094=CARTESIAN_POINT('Ctrl Pts',(-61.5755994828347,64.0221490317292,-4.11519589280509));
#35095=CARTESIAN_POINT('Ctrl Pts',(-60.8953686608783,64.1682666450633,-4.15416810543552));
#35096=CARTESIAN_POINT('Ctrl Pts',(-60.2151378389219,64.3143842583974,-4.19314031806595));
#35097=CARTESIAN_POINT('Ctrl Pts',(-59.4983946146019,64.290522799882,-4.23211253069638));
#35098=CARTESIAN_POINT('Ctrl Pts',(-58.8293879277002,64.0994875219352,-4.27108474332681));
#35099=CARTESIAN_POINT('Ctrl Pts',(-58.1603812407985,63.9084522439884,-4.31005695595724));
#35100=CARTESIAN_POINT('Ctrl Pts',(-57.539111091315,63.5502431466101,-4.34902916858767));
#35101=CARTESIAN_POINT('Ctrl Pts',(-57.0386048919244,63.0669647139892,-4.3880013812181));
#35102=CARTESIAN_POINT('Ctrl Pts',(-56.5380986925339,62.5836862813682,-4.42697359384853));
#35103=CARTESIAN_POINT('Ctrl Pts',(-56.1583564432364,61.9753385135046,-4.46594580647896));
#35104=CARTESIAN_POINT('Ctrl Pts',(-55.9440135696077,61.313431507019,-4.50491801910939));
#35105=CARTESIAN_POINT('Ctrl Pts',(-55.8069496222504,60.8901676701744,-4.52983923626928));
#35106=CARTESIAN_POINT('Ctrl Pts',(-55.7375192334137,60.4450028927427,-4.55476045342917));
#35107=CARTESIAN_POINT('Ctrl Pts',(-55.7372273834134,59.9999263798756,-4.57968167058906));
#35108=CARTESIAN_POINT('Origin',(-60.,60.,-6.));
#35109=CARTESIAN_POINT('',(-55.7373026574226,60.0053877648092,-6.07968167058906));
#35110=CARTESIAN_POINT('',(-55.7367830248949,59.9999456221449,-5.67031832941094));
#35111=CARTESIAN_POINT('',(-55.737,60.,-6.));
#35112=CARTESIAN_POINT('Ctrl Pts',(-55.7367830248949,59.9999456221449,-5.67031832941094));
#35113=CARTESIAN_POINT('Ctrl Pts',(-55.7373127735992,60.5841136850818,-5.63760089747675));
#35114=CARTESIAN_POINT('Ctrl Pts',(-55.8585017386039,61.1684537659817,-5.60488346554256));
#35115=CARTESIAN_POINT('Ctrl Pts',(-56.0919563653973,61.7038522083462,-5.57216603360837));
#35116=CARTESIAN_POINT('Ctrl Pts',(-56.3700418634662,62.3416058676127,-5.53319382097794));
#35117=CARTESIAN_POINT('Ctrl Pts',(-56.807421080765,62.9099162482909,-5.49422160834751));
#35118=CARTESIAN_POINT('Ctrl Pts',(-57.3527858376896,63.3419273517729,-5.45524939571708));
#35119=CARTESIAN_POINT('Ctrl Pts',(-57.8981505946142,63.7739384552549,-5.41627718308665));
#35120=CARTESIAN_POINT('Ctrl Pts',(-58.5515008911646,64.0696502815408,-5.37730497045622));
#35121=CARTESIAN_POINT('Ctrl Pts',(-59.2359911490654,64.1943286820334,-5.33833275782579));
#35122=CARTESIAN_POINT('Ctrl Pts',(-59.9204814069662,64.319007082526,-5.29936054519536));
#35123=CARTESIAN_POINT('Ctrl Pts',(-60.6361116262173,64.2726520572252,-5.26038833256493));
#35124=CARTESIAN_POINT('Ctrl Pts',(-61.2987856077668,64.0607007393324,-5.2214161199345));
#35125=CARTESIAN_POINT('Ctrl Pts',(-61.9614595893163,63.8487494214396,-5.18244390730407));
#35126=CARTESIAN_POINT('Ctrl Pts',(-62.5711773331643,63.4712018109547,-5.14347169467364));
#35127=CARTESIAN_POINT('Ctrl Pts',(-63.0562596233642,62.9724419329156,-5.10449948204321));
#35128=CARTESIAN_POINT('Ctrl Pts',(-63.5413419135642,62.4736820548765,-5.06552726941278));
#35129=CARTESIAN_POINT('Ctrl Pts',(-63.9017887501161,61.8537099092833,-5.02655505678235));
#35130=CARTESIAN_POINT('Ctrl Pts',(-64.0952363607056,61.1853972915882,-4.98758284415192));
#35131=CARTESIAN_POINT('Ctrl Pts',(-64.2886839712951,60.5170846738932,-4.94861063152149));
#35132=CARTESIAN_POINT('Ctrl Pts',(-64.315132355922,59.8004315840964,-4.90963841889106));
#35133=CARTESIAN_POINT('Ctrl Pts',(-64.1714704483469,59.1196777821999,-4.87066620626063));
#35134=CARTESIAN_POINT('Ctrl Pts',(-64.0278085407718,58.4389239803035,-4.8316939936302));
#35135=CARTESIAN_POINT('Ctrl Pts',(-63.7140363409947,57.7940694663075,-4.79272178099977));
#35136=CARTESIAN_POINT('Ctrl Pts',(-63.267037057901,57.2609127834971,-4.75374956836934));
#35137=CARTESIAN_POINT('Ctrl Pts',(-62.8200377748072,56.7277561006868,-4.71477735573891));
#35138=CARTESIAN_POINT('Ctrl Pts',(-62.239811408397,56.3062972490623,-4.67580514310848));
#35139=CARTESIAN_POINT('Ctrl Pts',(-61.5945598762935,56.0460766292211,-4.63683293047805));
#35140=CARTESIAN_POINT('Ctrl Pts',(-60.9493083441901,55.78585600938,-4.59786071784762));
#35141=CARTESIAN_POINT('Ctrl Pts',(-60.2390316463936,55.6868736213223,-4.55888850521719));
#35142=CARTESIAN_POINT('Ctrl Pts',(-59.5472191102546,55.7607641871698,-4.51991629258676));
#35143=CARTESIAN_POINT('Ctrl Pts',(-58.8554065741155,55.8346547530174,-4.48094407995633));
#35144=CARTESIAN_POINT('Ctrl Pts',(-58.1820581996339,56.0814182727702,-4.4419718673259));
#35145=CARTESIAN_POINT('Ctrl Pts',(-57.6063222274869,56.4720491024142,-4.40299965469547));
#35146=CARTESIAN_POINT('Ctrl Pts',(-57.0305862553399,56.8626799320582,-4.36402744206504));
#35147=CARTESIAN_POINT('Ctrl Pts',(-56.5524626855275,57.3971780715933,-4.32505522943461));
#35148=CARTESIAN_POINT('Ctrl Pts',(-56.2281524120011,58.0127162241851,-4.28608301680418));
#35149=CARTESIAN_POINT('Ctrl Pts',(-55.9070374867832,58.6221896327487,-4.2474947876731));
#35150=CARTESIAN_POINT('Ctrl Pts',(-55.7367198213808,59.3111139873581,-4.20890655854202));
#35151=CARTESIAN_POINT('Ctrl Pts',(-55.7366536686051,60.0000067695234,-4.17031832941094));
#35152=CARTESIAN_POINT('Ctrl Pts',(-55.7372273834134,59.9999263798756,-4.57968167058906));
#35153=CARTESIAN_POINT('Ctrl Pts',(-55.7370628335439,59.7489848618022,-4.5937326660596));
#35154=CARTESIAN_POINT('Ctrl Pts',(-55.7588766741727,59.4980714020751,-4.60778366153014));
#35155=CARTESIAN_POINT('Ctrl Pts',(-55.8029386446782,59.2511271515956,-4.62183465700068));
#35156=CARTESIAN_POINT('Ctrl Pts',(-55.9251500913374,58.5661960477653,-4.66080686963111));
#35157=CARTESIAN_POINT('Ctrl Pts',(-56.2185164826157,57.9118000852124,-4.69977908226154));
#35158=CARTESIAN_POINT('Ctrl Pts',(-56.6485487572492,57.3648700713727,-4.73875129489197));
#35159=CARTESIAN_POINT('Ctrl Pts',(-57.0785810318826,56.817940057533,-4.7777235075224));
#35160=CARTESIAN_POINT('Ctrl Pts',(-57.6452791898711,56.3784759924065,-4.81669572015283));
#35161=CARTESIAN_POINT('Ctrl Pts',(-58.2820428030497,56.0981124513163,-4.85566793278326));
#35162=CARTESIAN_POINT('Ctrl Pts',(-58.9188064162282,55.817748910226,-4.89464014541369));
#35163=CARTESIAN_POINT('Ctrl Pts',(-59.6256354845968,55.696485893172,-4.93361235804411));
#35164=CARTESIAN_POINT('Ctrl Pts',(-60.3194206751,55.7486246935045,-4.97258457067455));
#35165=CARTESIAN_POINT('Ctrl Pts',(-61.0132058656032,55.8007634938371,-5.01155678330497));
#35166=CARTESIAN_POINT('Ctrl Pts',(-61.6939471782411,56.0263041115563,-5.05052899593541));
#35167=CARTESIAN_POINT('Ctrl Pts',(-62.2816822789534,56.3986329467664,-5.08950120856583));
#35168=CARTESIAN_POINT('Ctrl Pts',(-62.8694173796658,56.7709617819764,-5.12847342119627));
#35169=CARTESIAN_POINT('Ctrl Pts',(-63.3641462684527,57.2900788346774,-5.16744563382669));
#35170=CARTESIAN_POINT('Ctrl Pts',(-63.7075974300418,57.8951863058555,-5.20641784645712));
#35171=CARTESIAN_POINT('Ctrl Pts',(-64.051048591631,58.5002937770336,-5.24539005908755));
#35172=CARTESIAN_POINT('Ctrl Pts',(-64.2432220260225,59.1913916666888,-5.28436227171798));
#35173=CARTESIAN_POINT('Ctrl Pts',(-64.2617854331837,59.8867672128279,-5.32333448434841));
#35174=CARTESIAN_POINT('Ctrl Pts',(-64.280348840345,60.5821427589669,-5.36230669697884));
#35175=CARTESIAN_POINT('Ctrl Pts',(-64.1253022202761,61.2817959615897,-5.40127890960927));
#35176=CARTESIAN_POINT('Ctrl Pts',(-63.8143159016832,61.9045202861169,-5.4402511222397));
#35177=CARTESIAN_POINT('Ctrl Pts',(-63.5033295830904,62.5272446106442,-5.47922333487013));
#35178=CARTESIAN_POINT('Ctrl Pts',(-63.0364035659737,63.073040057076,-5.51819554750056));
#35179=CARTESIAN_POINT('Ctrl Pts',(-62.4696188635954,63.4755272987511,-5.55716776013099));
#35180=CARTESIAN_POINT('Ctrl Pts',(-61.9028341612172,63.8780145404261,-5.59613997276142));
#35181=CARTESIAN_POINT('Ctrl Pts',(-61.2361907735773,64.1371935773445,-5.63511218539185));
#35182=CARTESIAN_POINT('Ctrl Pts',(-60.5454485416163,64.2273981110301,-5.67408439802228));
#35183=CARTESIAN_POINT('Ctrl Pts',(-59.8547063096553,64.3176026447156,-5.71305661065271));
#35184=CARTESIAN_POINT('Ctrl Pts',(-59.1398652333731,64.2388326751683,-5.75202882328314));
#35185=CARTESIAN_POINT('Ctrl Pts',(-58.4907659763914,63.9908835405709,-5.79100103591357));
#35186=CARTESIAN_POINT('Ctrl Pts',(-57.1925674624281,63.4949852713762,-5.86894546117443));
#35187=CARTESIAN_POINT('Ctrl Pts',(-56.1573362256669,62.3223703419813,-5.94688988643529));
#35188=CARTESIAN_POINT('Ctrl Pts',(-55.8423909177357,60.9741913581959,-6.02483431169615));
#35189=CARTESIAN_POINT('Ctrl Pts',(-55.7685181197862,60.6579658067722,-6.04311676466045));
#35190=CARTESIAN_POINT('Ctrl Pts',(-55.7342734667231,60.3320812053717,-6.06139921762475));
#35191=CARTESIAN_POINT('Ctrl Pts',(-55.7373026574226,60.0053877648092,-6.07968167058906));
#35192=CARTESIAN_POINT('Origin',(-60.,60.,-6.));
#35193=CARTESIAN_POINT('',(-55.7371269276513,60.000097806567,-7.57968167058905));
#35194=CARTESIAN_POINT('',(-55.7374561790016,59.9995175300878,-7.17031832941094));
#35195=CARTESIAN_POINT('',(-55.737,60.,-6.));
#35196=CARTESIAN_POINT('Ctrl Pts',(-55.7374561790016,59.9995175300878,-7.17031832941094));
#35197=CARTESIAN_POINT('Ctrl Pts',(-55.738291457224,60.4645797279776,-7.14423966167234));
#35198=CARTESIAN_POINT('Ctrl Pts',(-55.8149019517132,60.9297875761441,-7.11816099393373));
#35199=CARTESIAN_POINT('Ctrl Pts',(-55.9641974254798,61.3713748268308,-7.09208232619513));
#35200=CARTESIAN_POINT('Ctrl Pts',(-56.187306021621,62.0312870739269,-7.0531101135647));
#35201=CARTESIAN_POINT('Ctrl Pts',(-56.5727390884561,62.6384483809869,-7.01413790093427));
#35202=CARTESIAN_POINT('Ctrl Pts',(-57.0811320333225,63.1120990715827,-6.97516568830384));
#35203=CARTESIAN_POINT('Ctrl Pts',(-58.0979179230553,64.0594004527741,-6.89722126304298));
#35204=CARTESIAN_POINT('Ctrl Pts',(-59.6065433249131,64.4726593681082,-6.81927683778212));
#35205=CARTESIAN_POINT('Ctrl Pts',(-60.9556947910596,64.1619004906492,-6.74133241252127));
#35206=CARTESIAN_POINT('Ctrl Pts',(-62.3048462572061,63.8511416131902,-6.66338798726041));
#35207=CARTESIAN_POINT('Ctrl Pts',(-63.4945237876413,62.8163649429381,-6.58544356199955));
#35208=CARTESIAN_POINT('Ctrl Pts',(-63.9892742016634,61.5233054754929,-6.50749913673869));
#35209=CARTESIAN_POINT('Ctrl Pts',(-64.4840246156856,60.2302460080477,-6.42955471147783));
#35210=CARTESIAN_POINT('Ctrl Pts',(-64.2838479132947,58.6789037434093,-6.35161028621697));
#35211=CARTESIAN_POINT('Ctrl Pts',(-63.4866146246838,57.5406364040299,-6.27366586095611));
#35212=CARTESIAN_POINT('Ctrl Pts',(-63.0879979803783,56.9715027343402,-6.23469364832568));
#35213=CARTESIAN_POINT('Ctrl Pts',(-62.5401171895178,56.5056377959653,-6.19572143569525));
#35214=CARTESIAN_POINT('Ctrl Pts',(-61.9174965995694,56.1932194538155,-6.15674922306481));
#35215=CARTESIAN_POINT('Ctrl Pts',(-61.2948760096211,55.8808011116656,-6.11777701043439));
#35216=CARTESIAN_POINT('Ctrl Pts',(-60.5975156205848,55.7218293657408,-6.07880479780396));
#35217=CARTESIAN_POINT('Ctrl Pts',(-59.9025380935532,55.7375113780632,-6.03983258517353));
#35218=CARTESIAN_POINT('Ctrl Pts',(-59.2075605665216,55.7531933903855,-6.0008603725431));
#35219=CARTESIAN_POINT('Ctrl Pts',(-58.5149659014947,55.943529160955,-5.96188815991267));
#35220=CARTESIAN_POINT('Ctrl Pts',(-57.9084055195204,56.2849718118835,-5.92291594728224));
#35221=CARTESIAN_POINT('Ctrl Pts',(-57.3018451375461,56.6264144628121,-5.88394373465181));
#35222=CARTESIAN_POINT('Ctrl Pts',(-56.7813190386245,57.1189639940998,-5.84497152202137));
#35223=CARTESIAN_POINT('Ctrl Pts',(-56.4069717174883,57.7052706177407,-5.80599930939095));
#35224=CARTESIAN_POINT('Ctrl Pts',(-56.0326243963522,58.2915772413817,-5.76702709676052));
#35225=CARTESIAN_POINT('Ctrl Pts',(-55.8044558530015,58.9716409573759,-5.72805488413009));
#35226=CARTESIAN_POINT('Ctrl Pts',(-55.7497674707456,59.6652712843004,-5.68908267149966));
#35227=CARTESIAN_POINT('Ctrl Pts',(-55.7409903494441,59.7765943344006,-5.68282789080342));
#35228=CARTESIAN_POINT('Ctrl Pts',(-55.7366817497711,59.888266834801,-5.67657311010718));
#35229=CARTESIAN_POINT('Ctrl Pts',(-55.7367830248949,59.9999456221449,-5.67031832941094));
#35230=CARTESIAN_POINT('Ctrl Pts',(-55.7373026574226,60.0053877648092,-6.07968167058906));
#35231=CARTESIAN_POINT('Ctrl Pts',(-55.7471879551968,58.9392739868406,-6.13934364288561));
#35232=CARTESIAN_POINT('Ctrl Pts',(-56.1540183693135,57.8645465344337,-6.19900561518217));
#35233=CARTESIAN_POINT('Ctrl Pts',(-56.8759754147187,57.0887747469718,-6.25866758747873));
#35234=CARTESIAN_POINT('Ctrl Pts',(-57.8191645987341,56.0752801577091,-6.33661201273959));
#35235=CARTESIAN_POINT('Ctrl Pts',(-59.300202345866,55.5720340173595,-6.41455643800045));
#35236=CARTESIAN_POINT('Ctrl Pts',(-60.6732079819148,55.7867198306422,-6.49250086326131));
#35237=CARTESIAN_POINT('Ctrl Pts',(-61.3597107999392,55.8940627372836,-6.53147307589174));
#35238=CARTESIAN_POINT('Ctrl Pts',(-62.0192055901928,56.180888632333,-6.57044528852217));
#35239=CARTESIAN_POINT('Ctrl Pts',(-62.5738281627304,56.6023806143966,-6.6094175011526));
#35240=CARTESIAN_POINT('Ctrl Pts',(-63.1284507352679,57.0238725964602,-6.64838971378303));
#35241=CARTESIAN_POINT('Ctrl Pts',(-63.5782010900893,57.580030665538,-6.68736192641346));
#35242=CARTESIAN_POINT('Ctrl Pts',(-63.8700858814464,58.2109380653483,-6.72633413904389));
#35243=CARTESIAN_POINT('Ctrl Pts',(-64.1619706728036,58.8418454651586,-6.76530635167432));
#35244=CARTESIAN_POINT('Ctrl Pts',(-64.2959899006966,59.5475021957015,-6.80427856430475));
#35245=CARTESIAN_POINT('Ctrl Pts',(-64.2564571325936,60.2424376135327,-6.84325077693518));
#35246=CARTESIAN_POINT('Ctrl Pts',(-64.2169243644906,60.9373730313639,-6.88222298956561));
#35247=CARTESIAN_POINT('Ctrl Pts',(-64.0038396003916,61.6215871364834,-6.92119520219604));
#35248=CARTESIAN_POINT('Ctrl Pts',(-63.6422173414806,62.2158270645543,-6.96016741482647));
#35249=CARTESIAN_POINT('Ctrl Pts',(-63.2805950825697,62.8100669926251,-6.9991396274569));
#35250=CARTESIAN_POINT('Ctrl Pts',(-62.7704353288467,63.3143327436474,-7.03811184008733));
#35251=CARTESIAN_POINT('Ctrl Pts',(-62.1717193513747,63.6688083145846,-7.07708405271776));
#35252=CARTESIAN_POINT('Ctrl Pts',(-61.5730033739028,64.0232838855219,-7.11605626534819));
#35253=CARTESIAN_POINT('Ctrl Pts',(-60.8857311726819,64.2279692763742,-7.15502847797862));
#35254=CARTESIAN_POINT('Ctrl Pts',(-60.1906808759037,64.2590561721801,-7.19400069060905));
#35255=CARTESIAN_POINT('Ctrl Pts',(-59.4956305791255,64.2901430679861,-7.23297290323948));
#35256=CARTESIAN_POINT('Ctrl Pts',(-58.7928021867899,64.1476314687458,-7.2719451158699));
#35257=CARTESIAN_POINT('Ctrl Pts',(-58.1648124753609,63.8481564824943,-7.31091732850033));
#35258=CARTESIAN_POINT('Ctrl Pts',(-57.536822763932,63.5486814962429,-7.34988954113076));
#35259=CARTESIAN_POINT('Ctrl Pts',(-56.9836717334097,63.0922431229803,-7.38886175376119));
#35260=CARTESIAN_POINT('Ctrl Pts',(-56.5703777452405,62.5325470504499,-7.42783396639163));
#35261=CARTESIAN_POINT('Ctrl Pts',(-56.1570837570713,61.9728509779196,-7.46680617902206));
#35262=CARTESIAN_POINT('Ctrl Pts',(-55.8836468112551,61.3098972061215,-7.50577839165248));
#35263=CARTESIAN_POINT('Ctrl Pts',(-55.782208591691,60.6215873305249,-7.54475060428291));
#35264=CARTESIAN_POINT('Ctrl Pts',(-55.75190199686,60.4159416813061,-7.55639429305163));
#35265=CARTESIAN_POINT('Ctrl Pts',(-55.7369485091749,60.2080326724282,-7.56803798182034));
#35266=CARTESIAN_POINT('Ctrl Pts',(-55.7371269276513,60.000097806567,-7.57968167058905));
#35267=CARTESIAN_POINT('Origin',(-60.,60.,-6.));
#35268=CARTESIAN_POINT('',(-55.7367869586782,60.0000762880139,-9.07968167058905));
#35269=CARTESIAN_POINT('',(-55.7373303217998,60.0000007547395,-8.67031832941094));
#35270=CARTESIAN_POINT('',(-55.737,60.,-6.));
#35271=CARTESIAN_POINT('',(-63.2233527839579,62.7898325810254,-10.));
#35272=CARTESIAN_POINT('Ctrl Pts',(-55.7367869586782,60.0000762880139,-9.07968167058905));
#35273=CARTESIAN_POINT('Ctrl Pts',(-55.7372968301002,59.3936235369182,-9.11364895864636));
#35274=CARTESIAN_POINT('Ctrl Pts',(-55.8681266030866,58.786957945418,-9.14761624670367));
#35275=CARTESIAN_POINT('Ctrl Pts',(-56.1191760766754,58.2349683861818,-9.18158353476097));
#35276=CARTESIAN_POINT('Ctrl Pts',(-56.4072165422244,57.6016456894732,-9.2205557473914));
#35277=CARTESIAN_POINT('Ctrl Pts',(-56.8535144055287,57.0402986052668,-9.25952796002183));
#35278=CARTESIAN_POINT('Ctrl Pts',(-57.4056092260623,56.6169137142176,-9.29850017265226));
#35279=CARTESIAN_POINT('Ctrl Pts',(-57.9577040465959,56.1935288231683,-9.33747238528269));
#35280=CARTESIAN_POINT('Ctrl Pts',(-58.6155958243587,55.9081061252761,-9.37644459791312));
#35281=CARTESIAN_POINT('Ctrl Pts',(-59.3019542332415,55.794188192632,-9.41541681054355));
#35282=CARTESIAN_POINT('Ctrl Pts',(-59.9883126421243,55.6802702599879,-9.45438902317398));
#35283=CARTESIAN_POINT('Ctrl Pts',(-60.7031376821272,55.7378570925918,-9.49336123580441));
#35284=CARTESIAN_POINT('Ctrl Pts',(-61.3624026680008,55.9601950787861,-9.53233344843484));
#35285=CARTESIAN_POINT('Ctrl Pts',(-62.0216676538744,56.1825330649805,-9.57130566106527));
#35286=CARTESIAN_POINT('Ctrl Pts',(-62.6253725856187,56.5696222047652,-9.6102778736957));
#35287=CARTESIAN_POINT('Ctrl Pts',(-63.1025601776872,57.0759275956669,-9.64925008632613));
#35288=CARTESIAN_POINT('Ctrl Pts',(-63.5797477697557,57.5822329865685,-9.68822229895656));
#35289=CARTESIAN_POINT('Ctrl Pts',(-63.9304180221485,58.2077546285871,-9.72719451158699));
#35290=CARTESIAN_POINT('Ctrl Pts',(-64.113334662525,58.8790350253607,-9.76616672421742));
#35291=CARTESIAN_POINT('Ctrl Pts',(-64.2962513029015,59.5503154221343,-9.80513893684785));
#35292=CARTESIAN_POINT('Ctrl Pts',(-64.3114143312618,60.267354573663,-9.84411114947828));
#35293=CARTESIAN_POINT('Ctrl Pts',(-64.1570472486001,60.9456836607563,-9.88308336210871));
#35294=CARTESIAN_POINT('Ctrl Pts',(-64.0026801659383,61.6240127478497,-9.92205557473914));
#35295=CARTESIAN_POINT('Ctrl Pts',(-63.6787829722545,62.2636317705077,-9.96102778736957));
#35296=CARTESIAN_POINT('Ctrl Pts',(-63.2233527839579,62.7898325810254,-10.));
#35297=CARTESIAN_POINT('',(-56.7764331619493,62.7899186857328,-10.));
#35298=CARTESIAN_POINT('Origin',(-60.,60.,-10.));
#35299=CARTESIAN_POINT('Ctrl Pts',(-56.7764331619493,62.7899186857328,-10.));
#35300=CARTESIAN_POINT('Ctrl Pts',(-57.1737624197776,63.2482129439588,-9.96602721186203));
#35301=CARTESIAN_POINT('Ctrl Pts',(-57.6698071152885,63.6213495269443,-9.93205442372406));
#35302=CARTESIAN_POINT('Ctrl Pts',(-58.2209772071418,63.8744287315555,-9.89808163558608));
#35303=CARTESIAN_POINT('Ctrl Pts',(-58.8532573110885,64.1647509898991,-9.85910942295565));
#35304=CARTESIAN_POINT('Ctrl Pts',(-59.5580810762401,64.2970807010714,-9.82013721032522));
#35305=CARTESIAN_POINT('Ctrl Pts',(-60.2526054582228,64.2558578621421,-9.78116499769479));
#35306=CARTESIAN_POINT('Ctrl Pts',(-60.9471298402055,64.2146350232128,-9.74219278506436));
#35307=CARTESIAN_POINT('Ctrl Pts',(-61.6313548390192,63.9998596341819,-9.70322057243393));
#35308=CARTESIAN_POINT('Ctrl Pts',(-62.2248512269878,63.6367797954782,-9.6642483598035));
#35309=CARTESIAN_POINT('Ctrl Pts',(-62.8183476149565,63.2736999567746,-9.62527614717307));
#35310=CARTESIAN_POINT('Ctrl Pts',(-63.32111539208,62.7623156683981,-9.58630393454264));
#35311=CARTESIAN_POINT('Ctrl Pts',(-63.6740580837607,62.1627361795151,-9.54733172191221));
#35312=CARTESIAN_POINT('Ctrl Pts',(-64.0270007754414,61.563156690632,-9.50835950928178));
#35313=CARTESIAN_POINT('Ctrl Pts',(-64.2301183816792,60.8753820012424,-9.46938729665135));
#35314=CARTESIAN_POINT('Ctrl Pts',(-64.2595350443961,60.1802567460833,-9.43041508402092));
#35315=CARTESIAN_POINT('Ctrl Pts',(-64.288951707113,59.4851314909241,-9.39144287139049));
#35316=CARTESIAN_POINT('Ctrl Pts',(-64.1446674263089,58.7826556699956,-9.35247065876007));
#35317=CARTESIAN_POINT('Ctrl Pts',(-63.843642256701,58.1554011805957,-9.31349844612963));
#35318=CARTESIAN_POINT('Ctrl Pts',(-63.5426170870931,57.5281466911958,-9.27452623349921));
#35319=CARTESIAN_POINT('Ctrl Pts',(-63.0848510286812,56.9761135333246,-9.23555402086878));
#35320=CARTESIAN_POINT('Ctrl Pts',(-62.5241518355292,56.5641902660268,-9.19658180823834));
#35321=CARTESIAN_POINT('Ctrl Pts',(-61.9634526423771,56.1522669987289,-9.15760959560791));
#35322=CARTESIAN_POINT('Ctrl Pts',(-61.2998203144848,55.8804536220044,-9.11863738297748));
#35323=CARTESIAN_POINT('Ctrl Pts',(-60.611261215134,55.7807002318295,-9.07966517034705));
#35324=CARTESIAN_POINT('Ctrl Pts',(-59.9227021157832,55.6809468416546,-9.04069295771662));
#35325=CARTESIAN_POINT('Ctrl Pts',(-59.2092162449739,55.7532534380294,-9.0017207450862));
#35326=CARTESIAN_POINT('Ctrl Pts',(-58.554669879246,55.9891208250959,-8.96274853245577));
#35327=CARTESIAN_POINT('Ctrl Pts',(-57.900123513518,56.2249882121624,-8.92377631982534));
#35328=CARTESIAN_POINT('Ctrl Pts',(-57.3045166528713,56.6244163899207,-8.88480410719491));
#35329=CARTESIAN_POINT('Ctrl Pts',(-56.8378596282339,57.1404547329625,-8.84583189456448));
#35330=CARTESIAN_POINT('Ctrl Pts',(-56.3712026035963,57.6564930760043,-8.80685968193405));
#35331=CARTESIAN_POINT('Ctrl Pts',(-56.033495414968,58.2891415843297,-8.76788746930362));
#35332=CARTESIAN_POINT('Ctrl Pts',(-55.8644336009782,58.9640360264496,-8.72891525667319));
#35333=CARTESIAN_POINT('Ctrl Pts',(-55.7797022659359,59.3022833558961,-8.70938294758577));
#35334=CARTESIAN_POINT('Ctrl Pts',(-55.7373324459271,59.6511423120379,-8.68985063849836));
#35335=CARTESIAN_POINT('Ctrl Pts',(-55.7373303217998,60.0000007547395,-8.67031832941094));
#35336=CARTESIAN_POINT('Origin',(-60.,60.,-13.3123464956316));
#35337=CARTESIAN_POINT('',(-54.9005857509307,60.0000080970678,-3.68765350436841));
#35338=CARTESIAN_POINT('',(-54.9008894739474,59.9998849445721,-3.56234649563159));
#35339=CARTESIAN_POINT('',(-54.901,59.9999999999999,-13.3123464956316));
#35340=CARTESIAN_POINT('',(-63.6032183801568,63.607855083689,-3.));
#35341=CARTESIAN_POINT('Ctrl Pts',(-54.9008894739474,59.9998849445721,-3.56234649563159));
#35342=CARTESIAN_POINT('Ctrl Pts',(-54.9015382889875,60.6739141994399,-3.53078651427611));
#35343=CARTESIAN_POINT('Ctrl Pts',(-55.2021867355797,62.1808417896872,-3.46025432029021));
#35344=CARTESIAN_POINT('Ctrl Pts',(-56.644415546233,64.1119168166584,-3.35074991367387));
#35345=CARTESIAN_POINT('Ctrl Pts',(-58.9729552216983,65.2070699739396,-3.23383327578258));
#35346=CARTESIAN_POINT('Ctrl Pts',(-61.5432550625777,65.077974056636,-3.11691663789129));
#35347=CARTESIAN_POINT('Ctrl Pts',(-63.0142489447552,64.1960675938266,-3.03897221263043));
#35348=CARTESIAN_POINT('Ctrl Pts',(-63.6032183801568,63.6078550836889,-3.));
#35349=CARTESIAN_POINT('',(-64.9263786426945,61.3165318579407,-3.));
#35350=CARTESIAN_POINT('Origin',(-60.,60.,-3.));
#35351=CARTESIAN_POINT('Ctrl Pts',(-54.9005857509307,60.0000080970678,-3.68765350436841));
#35352=CARTESIAN_POINT('Ctrl Pts',(-54.9005849635668,60.008207439555,-3.68726952086906));
#35353=CARTESIAN_POINT('Ctrl Pts',(-54.9025709592986,60.8485945510885,-3.64791332473928));
#35354=CARTESIAN_POINT('Ctrl Pts',(-55.3285862201775,62.5191327628181,-3.56958491597908));
#35355=CARTESIAN_POINT('Ctrl Pts',(-57.0626757179785,64.4204363923688,-3.45266827808779));
#35356=CARTESIAN_POINT('Ctrl Pts',(-59.487294255791,65.282543142849,-3.3357516401965));
#35357=CARTESIAN_POINT('Ctrl Pts',(-62.0324515210899,64.9027851981381,-3.21883500230521));
#35358=CARTESIAN_POINT('Ctrl Pts',(-64.0113858210523,63.4359554740898,-3.10691778890637));
#35359=CARTESIAN_POINT('Ctrl Pts',(-64.7384685956641,62.0172737022055,-3.03397278813797));
#35360=CARTESIAN_POINT('Ctrl Pts',(-64.9263786426945,61.3165318579407,-3.));
#35361=CARTESIAN_POINT('Origin',(-60.,60.,-13.3123464956316));
#35362=CARTESIAN_POINT('',(-54.9007404747687,59.9999349583197,-5.18765350436841));
#35363=CARTESIAN_POINT('',(-54.9012719746715,59.9999119425253,-5.06234649563159));
#35364=CARTESIAN_POINT('',(-54.901,59.9999999999999,-13.3123464956316));
#35365=CARTESIAN_POINT('Ctrl Pts',(-54.9012719746715,59.9999119425253,-5.06234649563159));
#35366=CARTESIAN_POINT('Ctrl Pts',(-54.9016210582163,60.5322706427621,-5.0374252784717));
#35367=CARTESIAN_POINT('Ctrl Pts',(-55.1145360435078,61.8974113776361,-4.97353184868138));
#35368=CARTESIAN_POINT('Ctrl Pts',(-56.3134109693639,63.8180111698412,-4.87066620626063));
#35369=CARTESIAN_POINT('Ctrl Pts',(-58.5427258829576,65.1033793524814,-4.75374956836935));
#35370=CARTESIAN_POINT('Ctrl Pts',(-61.1146285576988,65.189001855627,-4.63683293047805));
#35371=CARTESIAN_POINT('Ctrl Pts',(-63.4244950049221,64.0547464033043,-4.51991629258676));
#35372=CARTESIAN_POINT('Ctrl Pts',(-64.9293002545277,61.9672654771257,-4.40299965469547));
#35373=CARTESIAN_POINT('Ctrl Pts',(-65.2752818739828,59.417301951109,-4.28608301680418));
#35374=CARTESIAN_POINT('Ctrl Pts',(-64.3811027318255,57.0043244761643,-4.1691663789129));
#35375=CARTESIAN_POINT('Ctrl Pts',(-62.4569756156385,55.2955969137595,-4.0522497410216));
#35376=CARTESIAN_POINT('Ctrl Pts',(-59.9552391151028,54.6928228512559,-3.93533310313032));
#35377=CARTESIAN_POINT('Ctrl Pts',(-57.4640288733897,55.3377064936621,-3.81841646523903));
#35378=CARTESIAN_POINT('Ctrl Pts',(-55.5689898394584,57.0786455663088,-3.70149982734774));
#35379=CARTESIAN_POINT('Ctrl Pts',(-54.9459956983136,58.8510320242688,-3.61614317081192));
#35380=CARTESIAN_POINT('Ctrl Pts',(-54.9007370921359,59.841581279342,-3.56975872690654));
#35381=CARTESIAN_POINT('Ctrl Pts',(-54.9008894739474,59.9998849445721,-3.56234649563159));
#35382=CARTESIAN_POINT('Ctrl Pts',(-54.9007404747687,59.9999349583197,-5.18765350436841));
#35383=CARTESIAN_POINT('Ctrl Pts',(-54.9013741103876,60.6986619001248,-5.15493607243422));
#35384=CARTESIAN_POINT('Ctrl Pts',(-55.2189956710647,62.2301462927378,-5.0832464278696));
#35385=CARTESIAN_POINT('Ctrl Pts',(-56.7044890264666,64.1603278398107,-4.97258457067455));
#35386=CARTESIAN_POINT('Ctrl Pts',(-59.0489177119773,65.2214359342736,-4.85566793278326));
#35387=CARTESIAN_POINT('Ctrl Pts',(-61.6168265705004,65.0550993586167,-4.73875129489197));
#35388=CARTESIAN_POINT('Ctrl Pts',(-63.8046877780167,63.7003384396424,-4.62183465700068));
#35389=CARTESIAN_POINT('Ctrl Pts',(-65.0980856806054,61.4756811768837,-4.50491801910939));
#35390=CARTESIAN_POINT('Ctrl Pts',(-65.1929908975039,58.9041019334819,-4.3880013812181));
#35391=CARTESIAN_POINT('Ctrl Pts',(-64.067076438205,56.5901588181647,-4.27108474332681));
#35392=CARTESIAN_POINT('Ctrl Pts',(-61.9850396737251,55.0778303984365,-4.15416810543552));
#35393=CARTESIAN_POINT('Ctrl Pts',(-59.4363409530604,54.7226501051879,-4.03725146754423));
#35394=CARTESIAN_POINT('Ctrl Pts',(-57.0201528028271,55.6081161060463,-3.92033482965294));
#35395=CARTESIAN_POINT('Ctrl Pts',(-55.3101280050136,57.5197664213586,-3.803802175261));
#35396=CARTESIAN_POINT('Ctrl Pts',(-54.9006648766645,59.1760192872482,-3.72624173349949));
#35397=CARTESIAN_POINT('Ctrl Pts',(-54.9005857509307,60.0000080970678,-3.68765350436841));
#35398=CARTESIAN_POINT('Origin',(-60.,60.,-13.3123464956316));
#35399=CARTESIAN_POINT('',(-54.901545638454,59.9994229148293,-6.68765350436841));
#35400=CARTESIAN_POINT('',(-54.9013620103677,60.006444337969,-6.56234649563159));
#35401=CARTESIAN_POINT('',(-54.901,59.9999999999999,-13.3123464956316));
#35402=CARTESIAN_POINT('Ctrl Pts',(-54.9013620103677,60.0064443379691,-6.56234649563159));
#35403=CARTESIAN_POINT('Ctrl Pts',(-54.8977387771102,60.3972043317359,-6.54406404266729));
#35404=CARTESIAN_POINT('Ctrl Pts',(-55.1133266770003,62.4488173731316,-6.44783716444213));
#35405=CARTESIAN_POINT('Ctrl Pts',(-57.261136178523,64.881658846174,-6.31263807358654));
#35406=CARTESIAN_POINT('Ctrl Pts',(-60.6812390619036,65.2585277879725,-6.15674922306482));
#35407=CARTESIAN_POINT('Ctrl Pts',(-63.0733675865873,64.3285109623237,-6.03983258517352));
#35408=CARTESIAN_POINT('Ctrl Pts',(-64.7488466585635,62.3700232907153,-5.92291594728224));
#35409=CARTESIAN_POINT('Ctrl Pts',(-65.3052032495076,59.8594450499176,-5.80599930939095));
#35410=CARTESIAN_POINT('Ctrl Pts',(-64.6156238392598,57.3795659933714,-5.68908267149965));
#35411=CARTESIAN_POINT('Ctrl Pts',(-62.8403792200309,55.5168088844888,-5.57216603360837));
#35412=CARTESIAN_POINT('Ctrl Pts',(-60.3976628561038,54.7074974068321,-5.45524939571708));
#35413=CARTESIAN_POINT('Ctrl Pts',(-57.8613353264688,55.1426276840725,-5.33833275782579));
#35414=CARTESIAN_POINT('Ctrl Pts',(-55.8278420769378,56.7195645370492,-5.2214161199345));
#35415=CARTESIAN_POINT('Ctrl Pts',(-54.9995353574893,58.5672219002548,-5.1294206992031));
#35416=CARTESIAN_POINT('Ctrl Pts',(-54.9010751555806,59.6997592799271,-5.07639749110213));
#35417=CARTESIAN_POINT('Ctrl Pts',(-54.9012719746715,59.9999119425253,-5.06234649563159));
#35418=CARTESIAN_POINT('Ctrl Pts',(-54.901545638454,59.9994229148293,-6.68765350436841));
#35419=CARTESIAN_POINT('Ctrl Pts',(-54.9025447197713,60.5556866134078,-6.66157483662981));
#35420=CARTESIAN_POINT('Ctrl Pts',(-55.1311181375491,61.9436707080335,-6.59652395626078));
#35421=CARTESIAN_POINT('Ctrl Pts',(-56.822670191795,64.6083226141335,-6.45352865063088));
#35422=CARTESIAN_POINT('Ctrl Pts',(-61.3338600370175,65.8440763141619,-6.25866758747874));
#35423=CARTESIAN_POINT('Ctrl Pts',(-65.6028014358132,62.1309684734756,-6.02483431169615));
#35424=CARTESIAN_POINT('Ctrl Pts',(-65.0042200345167,57.4920438855145,-5.82997324854401));
#35425=CARTESIAN_POINT('Ctrl Pts',(-62.3829259668669,55.2631484402659,-5.67408439802228));
#35426=CARTESIAN_POINT('Ctrl Pts',(-59.8805750705293,54.692707249224,-5.557167760131));
#35427=CARTESIAN_POINT('Ctrl Pts',(-57.3953251078463,55.3756925371435,-5.44025112223971));
#35428=CARTESIAN_POINT('Ctrl Pts',(-55.5275118929263,57.1431169284426,-5.32333448434842));
#35429=CARTESIAN_POINT('Ctrl Pts',(-54.9378835090541,58.9005233785311,-5.23913527839132));
#35430=CARTESIAN_POINT('Ctrl Pts',(-54.9006193389826,59.8663552875089,-5.19390828506465));
#35431=CARTESIAN_POINT('Ctrl Pts',(-54.9007404747687,59.9999349583197,-5.18765350436841));
#35432=CARTESIAN_POINT('Origin',(-60.,60.,-13.3123464956316));
#35433=CARTESIAN_POINT('',(-54.9013950998961,60.0000009027484,-8.18765350436842));
#35434=CARTESIAN_POINT('',(-54.9011518189288,60.0001169870244,-8.06234649563159));
#35435=CARTESIAN_POINT('',(-54.901,59.9999999999999,-13.3123464956316));
#35436=CARTESIAN_POINT('Ctrl Pts',(-54.9011518189288,60.0001169870244,-8.06234649563159));
#35437=CARTESIAN_POINT('Ctrl Pts',(-54.9009384115137,60.2488291336409,-8.05070280686288));
#35438=CARTESIAN_POINT('Ctrl Pts',(-54.978689873463,61.3298631862382,-8.00008690546373));
#35439=CARTESIAN_POINT('Ctrl Pts',(-55.7305242936952,63.1527019513981,-7.91049879143416));
#35440=CARTESIAN_POINT('Ctrl Pts',(-57.7154061407277,64.7905480212547,-7.79358215354287));
#35441=CARTESIAN_POINT('Ctrl Pts',(-60.237377972198,65.3019249702528,-7.67666551565158));
#35442=CARTESIAN_POINT('Ctrl Pts',(-62.7035292417443,64.5674486803472,-7.55974887776029));
#35443=CARTESIAN_POINT('Ctrl Pts',(-64.5341447127037,62.7579827658769,-7.442832239869));
#35444=CARTESIAN_POINT('Ctrl Pts',(-65.2987606255403,60.3028049178794,-7.32591560197772));
#35445=CARTESIAN_POINT('Ctrl Pts',(-64.8178570062396,57.770684109267,-7.20899896408642));
#35446=CARTESIAN_POINT('Ctrl Pts',(-63.2040096739143,55.7750120514012,-7.09208232619513));
#35447=CARTESIAN_POINT('Ctrl Pts',(-60.0487068960553,54.4027153224711,-6.93619347567341));
#35448=CARTESIAN_POINT('Ctrl Pts',(-56.0355250219872,55.7663661089261,-6.75961486548557));
#35449=CARTESIAN_POINT('Ctrl Pts',(-54.9131858746302,58.7312592209477,-6.62200846792815));
#35450=CARTESIAN_POINT('Ctrl Pts',(-54.9013620103677,60.0064443379691,-6.56234649563159));
#35451=CARTESIAN_POINT('Ctrl Pts',(-54.9013950998961,60.0000009027484,-8.18765350436842));
#35452=CARTESIAN_POINT('Ctrl Pts',(-54.9013925712344,60.4152985155146,-8.1682136008254));
#35453=CARTESIAN_POINT('Ctrl Pts',(-55.0522172876686,61.6631635996099,-8.10980148465195));
#35454=CARTESIAN_POINT('Ctrl Pts',(-56.059376560482,63.5552235595967,-8.01241715584808));
#35455=CARTESIAN_POINT('Ctrl Pts',(-58.1949364984747,64.9909811437472,-7.89550051795679));
#35456=CARTESIAN_POINT('Ctrl Pts',(-60.7548501786328,65.2534097268154,-7.7785838800655));
#35457=CARTESIAN_POINT('Ctrl Pts',(-63.1372998197884,64.2808297669235,-7.66166724217421));
#35458=CARTESIAN_POINT('Ctrl Pts',(-64.7822203790914,62.3018527171852,-7.54475060428292));
#35459=CARTESIAN_POINT('Ctrl Pts',(-65.3028606950879,59.7817818006449,-7.42783396639163));
#35460=CARTESIAN_POINT('Ctrl Pts',(-64.5769288017872,57.3129117888108,-7.31091732850034));
#35461=CARTESIAN_POINT('Ctrl Pts',(-62.7748569607921,55.4759618947992,-7.19400069060905));
#35462=CARTESIAN_POINT('Ctrl Pts',(-60.3207807277454,54.7020982939809,-7.07708405271776));
#35463=CARTESIAN_POINT('Ctrl Pts',(-57.7905713642451,55.1747170180384,-6.96016741482648));
#35464=CARTESIAN_POINT('Ctrl Pts',(-55.7813283808542,56.7795403162521,-6.84325077693518));
#35465=CARTESIAN_POINT('Ctrl Pts',(-54.9881855005153,58.6182641032336,-6.75241280678249));
#35466=CARTESIAN_POINT('Ctrl Pts',(-54.9010516830133,59.7244007763825,-6.70054704926024));
#35467=CARTESIAN_POINT('Ctrl Pts',(-54.901545638454,59.9994229148293,-6.68765350436841));
#35468=CARTESIAN_POINT('Origin',(-60.,60.,-13.3123464956316));
#35469=CARTESIAN_POINT('',(-54.9012106446239,60.0001195814448,-9.68765350436841));
#35470=CARTESIAN_POINT('',(-54.9007451799907,60.0000912485532,-9.56234649563159));
#35471=CARTESIAN_POINT('',(-54.901,59.9999999999999,-13.3123464956316));
#35472=CARTESIAN_POINT('',(-58.677115034431,55.0755938055567,-10.));
#35473=CARTESIAN_POINT('Ctrl Pts',(-58.677115034431,55.0755938055567,-10.));
#35474=CARTESIAN_POINT('Ctrl Pts',(-57.8732233401272,55.2915500435982,-9.96102778736957));
#35475=CARTESIAN_POINT('Ctrl Pts',(-56.3739727673179,56.1245137043432,-9.88308336210872));
#35476=CARTESIAN_POINT('Ctrl Pts',(-55.1299740822569,58.0492615027565,-9.77896786356484));
#35477=CARTESIAN_POINT('Ctrl Pts',(-54.9016327694172,59.4410930379684,-9.71382457765142));
#35478=CARTESIAN_POINT('Ctrl Pts',(-54.9012106446239,60.0001195814448,-9.68765350436841));
#35479=CARTESIAN_POINT('',(-61.3230392943658,55.0753649202911,-10.));
#35480=CARTESIAN_POINT('Origin',(-60.,60.,-10.));
#35481=CARTESIAN_POINT('Ctrl Pts',(-61.3230392943658,55.0753649202911,-10.));
#35482=CARTESIAN_POINT('Ctrl Pts',(-60.6222240320617,54.8877288802907,-9.96602721186203));
#35483=CARTESIAN_POINT('Ctrl Pts',(-59.0300681471914,54.8080601177165,-9.89308221109362));
#35484=CARTESIAN_POINT('Ctrl Pts',(-56.77028917635,55.7884526872829,-9.78116499769479));
#35485=CARTESIAN_POINT('Ctrl Pts',(-55.2373851384779,57.7165175129953,-9.66925328437663));
#35486=CARTESIAN_POINT('Ctrl Pts',(-54.9013550402723,59.2747094568956,-9.5963137836889));
#35487=CARTESIAN_POINT('Ctrl Pts',(-54.9007451799907,60.0000912485532,-9.56234649563159));
#35488=CARTESIAN_POINT('Origin',(-60.,60.,-3.));
#35489=CARTESIAN_POINT('Ctrl Pts',(-59.1956105045055,55.8135783132204,-3.));
#35490=CARTESIAN_POINT('Ctrl Pts',(-59.3195769365686,55.7770540578209,-3.));
#35491=CARTESIAN_POINT('Ctrl Pts',(-59.445059760185,55.7463481720298,-3.));
#35492=CARTESIAN_POINT('Ctrl Pts',(-59.5716383186483,55.7213771363331,-3.));
#35493=CARTESIAN_POINT('Ctrl Pts',(-59.7000945008852,55.6960356886894,-3.));
#35494=CARTESIAN_POINT('Ctrl Pts',(-59.8296798459766,55.6766002514243,-3.));
#35495=CARTESIAN_POINT('Ctrl Pts',(-59.959981179512,55.6630301115702,-3.));
#35496=CARTESIAN_POINT('Ctrl Pts',(-60.0181559866187,55.6569715375939,-3.));
#35497=CARTESIAN_POINT('Ctrl Pts',(-60.0764737978558,55.6520827276688,-3.));
#35498=CARTESIAN_POINT('Ctrl Pts',(-60.1348989470971,55.6483631838136,-3.));
#35499=CARTESIAN_POINT('Ctrl Pts',(-60.1584275152761,55.646865275082,-3.));
#35500=CARTESIAN_POINT('Ctrl Pts',(-60.1819734969942,55.6455570175179,-3.));
#35501=CARTESIAN_POINT('Ctrl Pts',(-60.2055345827709,55.6444384689613,-3.));
#35502=CARTESIAN_POINT('Ctrl Pts',(-60.2289638731321,55.6433261773138,-3.));
#35503=CARTESIAN_POINT('Ctrl Pts',(-60.2523986226803,55.6424019433942,-3.));
#35504=CARTESIAN_POINT('Ctrl Pts',(-60.2758336778232,55.6416654642661,-3.));
#35505=CARTESIAN_POINT('Ctrl Pts',(-60.4095527621665,55.6374631564819,-3.));
#35506=CARTESIAN_POINT('Ctrl Pts',(-60.5433094949031,55.6393683817081,-3.));
#35507=CARTESIAN_POINT('Ctrl Pts',(-60.6766724777373,55.6473288482565,-3.));
#35508=CARTESIAN_POINT('Ctrl Pts',(-60.7846049163009,55.6537713598771,-3.));
#35509=CARTESIAN_POINT('Ctrl Pts',(-60.8922801012417,55.6641808613591,-3.));
#35510=CARTESIAN_POINT('Ctrl Pts',(-60.9994758570612,55.6785535027164,-3.));
#35511=CARTESIAN_POINT('Ctrl Pts',(-61.053073734971,55.685739823395,-3.));
#35512=CARTESIAN_POINT('Ctrl Pts',(-61.1065518155819,55.6939172672668,-3.));
#35513=CARTESIAN_POINT('Ctrl Pts',(-61.159882506232,55.7030874102868,-3.));
#35514=CARTESIAN_POINT('Ctrl Pts',(-61.1872713887428,55.7077968930766,-3.));
#35515=CARTESIAN_POINT('Ctrl Pts',(-61.2146213974502,55.7127682237387,-3.));
#35516=CARTESIAN_POINT('Ctrl Pts',(-61.2419287911558,55.7180017588153,-3.));
#35517=CARTESIAN_POINT('Ctrl Pts',(-61.2615202355303,55.7217565115552,-3.));
#35518=CARTESIAN_POINT('Ctrl Pts',(-61.2810875141073,55.7256458533217,-3.));
#35519=CARTESIAN_POINT('Ctrl Pts',(-61.3006183099631,55.7296674434209,-3.));
#35520=CARTESIAN_POINT('Ctrl Pts',(-61.3068720706772,55.7309551565462,-3.));
#35521=CARTESIAN_POINT('Ctrl Pts',(-61.3131224068267,55.7322564887182,-3.));
#35522=CARTESIAN_POINT('Ctrl Pts',(-61.3193692733847,55.7335714316187,-3.));
#35523=CARTESIAN_POINT('Ctrl Pts',(-61.4494244547665,55.760947578659,-3.));
#35524=CARTESIAN_POINT('Ctrl Pts',(-61.577974912008,55.7942188050333,-3.));
#35525=CARTESIAN_POINT('Ctrl Pts',(-61.704692114971,55.8330909005726,-3.));
#35526=CARTESIAN_POINT('Ctrl Pts',(-61.8336752302035,55.8726580931955,-3.));
#35527=CARTESIAN_POINT('Ctrl Pts',(-61.9607596091681,55.91802834131,-3.));
#35528=CARTESIAN_POINT('Ctrl Pts',(-62.0856036012641,55.9689451560091,-3.));
#35529=CARTESIAN_POINT('Ctrl Pts',(-62.2120507894683,56.0205158238717,-3.));
#35530=CARTESIAN_POINT('Ctrl Pts',(-62.3362004369027,56.0777765786684,-3.));
#35531=CARTESIAN_POINT('Ctrl Pts',(-62.4576916079016,56.1405137039557,-3.));
#35532=CARTESIAN_POINT('Ctrl Pts',(-62.5340614666828,56.1799505235957,-3.));
#35533=CARTESIAN_POINT('Ctrl Pts',(-62.6093806902554,56.2215523381483,-3.));
#35534=CARTESIAN_POINT('Ctrl Pts',(-62.6835563590128,56.2652760862483,-3.));
#35535=CARTESIAN_POINT('Ctrl Pts',(-62.7445595014197,56.3012351288372,-3.));
#35536=CARTESIAN_POINT('Ctrl Pts',(-62.8047891530527,56.3386295207014,-3.));
#35537=CARTESIAN_POINT('Ctrl Pts',(-62.8641916904358,56.3774390056312,-3.));
#35538=CARTESIAN_POINT('Ctrl Pts',(-62.8791980541292,56.3872431195843,-3.));
#35539=CARTESIAN_POINT('Ctrl Pts',(-62.8941498090572,56.3971364251801,-3.));
#35540=CARTESIAN_POINT('Ctrl Pts',(-62.9090367420972,56.4071121284225,-3.));
#35541=CARTESIAN_POINT('Ctrl Pts',(-63.0253590231817,56.485059449973,-3.));
#35542=CARTESIAN_POINT('Ctrl Pts',(-63.1378862566305,56.5681385841153,-3.));
#35543=CARTESIAN_POINT('Ctrl Pts',(-63.2462619950014,56.656078356157,-3.));
#35544=CARTESIAN_POINT('Ctrl Pts',(-63.2693908817498,56.6748459240537,-3.));
#35545=CARTESIAN_POINT('Ctrl Pts',(-63.2923306567195,56.6938350587944,-3.));
#35546=CARTESIAN_POINT('Ctrl Pts',(-63.3150777939445,56.7130434235261,-3.));
#35547=CARTESIAN_POINT('Ctrl Pts',(-63.4206898136458,56.8022253796735,-3.));
#35548=CARTESIAN_POINT('Ctrl Pts',(-63.5221511112837,56.8961292683318,-3.));
#35549=CARTESIAN_POINT('Ctrl Pts',(-63.6192855225016,56.9943655518854,-3.));
#35550=CARTESIAN_POINT('Ctrl Pts',(-63.7175323011257,57.0937268213073,-3.));
#35551=CARTESIAN_POINT('Ctrl Pts',(-63.8113530858956,57.1975207545623,-3.));
#35552=CARTESIAN_POINT('Ctrl Pts',(-63.9005375437739,57.305389517552,-3.));
#35553=CARTESIAN_POINT('Ctrl Pts',(-63.9806728177378,57.4023132762423,-3.));
#35554=CARTESIAN_POINT('Ctrl Pts',(-64.0570647960701,57.5025277837558,-3.));
#35555=CARTESIAN_POINT('Ctrl Pts',(-64.1295362219416,57.6057990786673,-3.));
#35556=CARTESIAN_POINT('Ctrl Pts',(-64.1412822857501,57.6225371406694,-3.));
#35557=CARTESIAN_POINT('Ctrl Pts',(-64.1529253027095,57.6393555477934,-3.));
#35558=CARTESIAN_POINT('Ctrl Pts',(-64.1644644511097,57.6562533540464,-3.));
#35559=CARTESIAN_POINT('Ctrl Pts',(-64.1746328838408,57.6711438988445,-3.));
#35560=CARTESIAN_POINT('Ctrl Pts',(-64.1847153144395,57.6860882798462,-3.));
#35561=CARTESIAN_POINT('Ctrl Pts',(-64.1947109245644,57.7010848983457,-3.));
#35562=CARTESIAN_POINT('Ctrl Pts',(-64.2739894697328,57.8200281226444,-3.));
#35563=CARTESIAN_POINT('Ctrl Pts',(-64.3478189157374,57.9422686542718,-3.));
#35564=CARTESIAN_POINT('Ctrl Pts',(-64.4160215894327,58.0673941364165,-3.));
#35565=CARTESIAN_POINT('Ctrl Pts',(-64.4849569820396,58.193863873883,-3.));
#35566=CARTESIAN_POINT('Ctrl Pts',(-64.5481446301058,58.3232814243193,-3.));
#35567=CARTESIAN_POINT('Ctrl Pts',(-64.6053684730552,58.4552626417141,-3.));
#35568=CARTESIAN_POINT('Ctrl Pts',(-64.6262261154663,58.5033687613929,-3.));
#35569=CARTESIAN_POINT('Ctrl Pts',(-64.6462910856029,58.5518158315677,-3.));
#35570=CARTESIAN_POINT('Ctrl Pts',(-64.665551625707,58.6005863831579,-3.));
#35571=CARTESIAN_POINT('Ctrl Pts',(-64.7181182841506,58.7336929790112,-3.));
#35572=CARTESIAN_POINT('Ctrl Pts',(-64.7646963550687,58.8692073663929,-3.));
#35573=CARTESIAN_POINT('Ctrl Pts',(-64.8052734936232,59.0067151216772,-3.));
#35574=CARTESIAN_POINT('Ctrl Pts',(-64.8290066390675,59.0871419746329,-3.));
#35575=CARTESIAN_POINT('Ctrl Pts',(-64.8506860242825,59.1682512449237,-3.));
#35576=CARTESIAN_POINT('Ctrl Pts',(-64.8703015754152,59.2499631360153,-3.));
#35577=CARTESIAN_POINT('Ctrl Pts',(-64.8777895471377,59.2811555468604,-3.));
#35578=CARTESIAN_POINT('Ctrl Pts',(-64.8849767115593,59.3124357915603,-3.));
#35579=CARTESIAN_POINT('Ctrl Pts',(-64.8918622845764,59.3437994898947,-3.));
#35580=CARTESIAN_POINT('Ctrl Pts',(-64.8973648848784,59.3688637649373,-3.));
#35581=CARTESIAN_POINT('Ctrl Pts',(-64.9026757353232,59.3939859734578,-3.));
#35582=CARTESIAN_POINT('Ctrl Pts',(-64.9077887067164,59.4191347884762,-3.));
#35583=CARTESIAN_POINT('Ctrl Pts',(-64.9369315292006,59.5624775524785,-3.));
#35584=CARTESIAN_POINT('Ctrl Pts',(-64.9596873533747,59.7068444160501,-3.));
#35585=CARTESIAN_POINT('Ctrl Pts',(-64.9761061056319,59.8517783133678,-3.));
#35586=CARTESIAN_POINT('Ctrl Pts',(-64.9926869506057,59.9981430580958,-3.));
#35587=CARTESIAN_POINT('Ctrl Pts',(-65.0028052187048,60.1450868049904,-3.));
#35588=CARTESIAN_POINT('Ctrl Pts',(-65.0064655586371,60.2921650192025,-3.));
#35589=CARTESIAN_POINT('Ctrl Pts',(-65.0101294420625,60.4393856165403,-3.));
#35590=CARTESIAN_POINT('Ctrl Pts',(-65.0073230692564,60.586741719856,-3.));
#35591=CARTESIAN_POINT('Ctrl Pts',(-64.9980014221604,60.7338023037548,-3.));
#35592=CARTESIAN_POINT('Ctrl Pts',(-64.9923757401215,60.8225544391829,-3.));
#35593=CARTESIAN_POINT('Ctrl Pts',(-64.9843760879495,60.9111991744113,-3.));
#35594=CARTESIAN_POINT('Ctrl Pts',(-64.9739833939208,60.9996425419769,-3.));
#35595=CARTESIAN_POINT('Ctrl Pts',(-64.9615316541797,61.1056086939404,-3.));
#35596=CARTESIAN_POINT('Ctrl Pts',(-64.9456450378036,61.2112859258266,-3.));
#35597=CARTESIAN_POINT('Ctrl Pts',(-64.9263786426945,61.3165318579407,-3.));
#35598=CARTESIAN_POINT('Ctrl Pts',(-63.6032183801568,63.6078550836889,-3.));
#35599=CARTESIAN_POINT('Ctrl Pts',(-63.4898427047886,63.7040964640175,-3.));
#35600=CARTESIAN_POINT('Ctrl Pts',(-63.3723224036437,63.7951365693987,-3.));
#35601=CARTESIAN_POINT('Ctrl Pts',(-63.2510558032013,63.8807935742749,-3.));
#35602=CARTESIAN_POINT('Ctrl Pts',(-63.1296781818555,63.9665289990789,-3.));
#35603=CARTESIAN_POINT('Ctrl Pts',(-63.0045466465185,64.04687175851,-3.));
#35604=CARTESIAN_POINT('Ctrl Pts',(-62.8760397174998,64.1215919436791,-3.));
#35605=CARTESIAN_POINT('Ctrl Pts',(-62.819687934894,64.1543576136944,-3.));
#35606=CARTESIAN_POINT('Ctrl Pts',(-62.7626868867519,64.1860414629978,-3.));
#35607=CARTESIAN_POINT('Ctrl Pts',(-62.7050677894913,64.216620998216,-3.));
#35608=CARTESIAN_POINT('Ctrl Pts',(-62.6757305642214,64.2321908137112,-3.));
#35609=CARTESIAN_POINT('Ctrl Pts',(-62.6462331101221,64.2474743135493,-3.));
#35610=CARTESIAN_POINT('Ctrl Pts',(-62.6165795271981,64.2624683312761,-3.));
#35611=CARTESIAN_POINT('Ctrl Pts',(-62.59496584419,64.2733970594164,-3.));
#35612=CARTESIAN_POINT('Ctrl Pts',(-62.5732698259174,64.2841716159096,-3.));
#35613=CARTESIAN_POINT('Ctrl Pts',(-62.5515051394286,64.2947850862267,-3.));
#35614=CARTESIAN_POINT('Ctrl Pts',(-62.4199917799758,64.3589170983083,-3.));
#35615=CARTESIAN_POINT('Ctrl Pts',(-62.2858583448011,64.4172297974733,-3.));
#35616=CARTESIAN_POINT('Ctrl Pts',(-62.1494741073268,64.4695125788851,-3.00000000000001));
#35617=CARTESIAN_POINT('Ctrl Pts',(-62.0315668791431,64.514712214504,-3.00000000000001));
#35618=CARTESIAN_POINT('Ctrl Pts',(-61.9119768383841,64.5554044377229,-3.));
#35619=CARTESIAN_POINT('Ctrl Pts',(-61.7909377316812,64.591421820407,-3.));
#35620=CARTESIAN_POINT('Ctrl Pts',(-61.7304181783297,64.6094305117491,-3.));
#35621=CARTESIAN_POINT('Ctrl Pts',(-61.6695363247516,64.6262700253364,-3.));
#35622=CARTESIAN_POINT('Ctrl Pts',(-61.6083214049011,64.6419165450135,-3.));
#35623=CARTESIAN_POINT('Ctrl Pts',(-61.5794890944997,64.649286077035,-3.));
#35624=CARTESIAN_POINT('Ctrl Pts',(-61.550582897767,64.6563909242344,-3.00000000000001));
#35625=CARTESIAN_POINT('Ctrl Pts',(-61.5216058842317,64.6632284448234,-3.00000000000001));
#35626=CARTESIAN_POINT('Ctrl Pts',(-61.4953410603476,64.6694259873636,-3.00000000000001));
#35627=CARTESIAN_POINT('Ctrl Pts',(-61.469014170971,64.6754046622799,-3.00000000000001));
#35628=CARTESIAN_POINT('Ctrl Pts',(-61.4426540829023,64.6811568975394,-3.00000000000001));
#35629=CARTESIAN_POINT('Ctrl Pts',(-61.4363509969477,64.6825323418542,-3.00000000000001));
#35630=CARTESIAN_POINT('Ctrl Pts',(-61.4300457323711,64.6838949091617,-3.));
#35631=CARTESIAN_POINT('Ctrl Pts',(-61.42373832106,64.6852445838374,-3.));
#35632=CARTESIAN_POINT('Ctrl Pts',(-61.2841863671008,64.7151062384725,-3.));
#35633=CARTESIAN_POINT('Ctrl Pts',(-61.1435842168792,64.738661067728,-3.));
#35634=CARTESIAN_POINT('Ctrl Pts',(-61.0023536947464,64.7559647413526,-3.));
#35635=CARTESIAN_POINT('Ctrl Pts',(-60.8601843546744,64.7733834396827,-3.));
#35636=CARTESIAN_POINT('Ctrl Pts',(-60.7173774438576,64.7844675371285,-3.00000000000001));
#35637=CARTESIAN_POINT('Ctrl Pts',(-60.5743624263688,64.7892212361641,-3.));
#35638=CARTESIAN_POINT('Ctrl Pts',(-60.4327942671285,64.793926842847,-3.));
#35639=CARTESIAN_POINT('Ctrl Pts',(-60.2910214307437,64.7924293018697,-3.));
#35640=CARTESIAN_POINT('Ctrl Pts',(-60.1494714253414,64.7846834160485,-3.));
#35641=CARTESIAN_POINT('Ctrl Pts',(-60.0601034197739,64.7797930286181,-3.));
#35642=CARTESIAN_POINT('Ctrl Pts',(-59.9708244934901,64.7724110370496,-3.));
#35643=CARTESIAN_POINT('Ctrl Pts',(-59.8817465640546,64.7625162762205,-3.));
#35644=CARTESIAN_POINT('Ctrl Pts',(-59.814938116978,64.7550952055987,-3.));
#35645=CARTESIAN_POINT('Ctrl Pts',(-59.7482427964903,64.7462605465847,-3.));
#35646=CARTESIAN_POINT('Ctrl Pts',(-59.6817095175338,64.7360006295818,-3.));
#35647=CARTESIAN_POINT('Ctrl Pts',(-59.6640767189296,64.7332815233984,-3.));
#35648=CARTESIAN_POINT('Ctrl Pts',(-59.6464553105021,64.7304622990051,-3.));
#35649=CARTESIAN_POINT('Ctrl Pts',(-59.6288462227171,64.7275427118551,-3.));
#35650=CARTESIAN_POINT('Ctrl Pts',(-59.6106484511471,64.7245255209203,-3.));
#35651=CARTESIAN_POINT('Ctrl Pts',(-59.5924725145907,64.7214025728485,-3.));
#35652=CARTESIAN_POINT('Ctrl Pts',(-59.5743219713167,64.7181743788859,-3.));
#35653=CARTESIAN_POINT('Ctrl Pts',(-59.437011224799,64.6937527560055,-3.));
#35654=CARTESIAN_POINT('Ctrl Pts',(-59.3011032400431,64.6633037588374,-3.));
#35655=CARTESIAN_POINT('Ctrl Pts',(-59.1669957960977,64.6268298783159,-3.));
#35656=CARTESIAN_POINT('Ctrl Pts',(-59.1418079969122,64.6199794250445,-3.));
#35657=CARTESIAN_POINT('Ctrl Pts',(-59.1166837551122,64.6129162986319,-3.));
#35658=CARTESIAN_POINT('Ctrl Pts',(-59.0916257724331,64.6056403204325,-3.));
#35659=CARTESIAN_POINT('Ctrl Pts',(-58.9576617080805,64.5667417536875,-3.));
#35660=CARTESIAN_POINT('Ctrl Pts',(-58.8255893248946,64.5217632196472,-3.));
#35661=CARTESIAN_POINT('Ctrl Pts',(-58.6957822301981,64.4709134387138,-3.));
#35662=CARTESIAN_POINT('Ctrl Pts',(-58.5664088958796,64.4202335762294,-3.));
#35663=CARTESIAN_POINT('Ctrl Pts',(-58.4392850870446,64.3637211364018,-3.));
#35664=CARTESIAN_POINT('Ctrl Pts',(-58.3148123421965,64.30154212406,-3.));
#35665=CARTESIAN_POINT('Ctrl Pts',(-58.2087252528553,64.2485474669124,-3.));
#35666=CARTESIAN_POINT('Ctrl Pts',(-58.104564199881,64.1914357758367,-3.));
#35667=CARTESIAN_POINT('Ctrl Pts',(-58.0026013403148,64.1302904539437,-3.));
#35668=CARTESIAN_POINT('Ctrl Pts',(-57.9842571522572,64.119289769102,-3.));
#35669=CARTESIAN_POINT('Ctrl Pts',(-57.9659841788218,64.1081584832539,-3.));
#35670=CARTESIAN_POINT('Ctrl Pts',(-57.947784091658,64.096897029522,-3.));
#35671=CARTESIAN_POINT('Ctrl Pts',(-57.9313889544622,64.0867524034388,-3.));
#35672=CARTESIAN_POINT('Ctrl Pts',(-57.9150608170848,64.0765069865091,-3.));
#35673=CARTESIAN_POINT('Ctrl Pts',(-57.8988040840088,64.0661635692336,-3.));
#35674=CARTESIAN_POINT('Ctrl Pts',(-57.7839055897439,63.9930589014656,-3.));
#35675=CARTESIAN_POINT('Ctrl Pts',(-57.6725153265955,63.9150275507377,-3.));
#35676=CARTESIAN_POINT('Ctrl Pts',(-57.5649776150316,63.8322713084228,-3.));
#35677=CARTESIAN_POINT('Ctrl Pts',(-57.4583964036554,63.7502511461319,-3.));
#35678=CARTESIAN_POINT('Ctrl Pts',(-57.3555989638067,63.6635892415037,-3.));
#35679=CARTESIAN_POINT('Ctrl Pts',(-57.2569565386241,63.5724461284644,-3.));
#35680=CARTESIAN_POINT('Ctrl Pts',(-57.2241738685229,63.5421557680923,-3.));
#35681=CARTESIAN_POINT('Ctrl Pts',(-57.1918504478657,63.5113702013341,-3.));
#35682=CARTESIAN_POINT('Ctrl Pts',(-57.160000955263,63.4800945823787,-3.));
#35683=CARTESIAN_POINT('Ctrl Pts',(-57.0634278031584,63.385261514103,-3.));
#35684=CARTESIAN_POINT('Ctrl Pts',(-56.9712084001481,63.285924190182,-3.));
#35685=CARTESIAN_POINT('Ctrl Pts',(-56.883615186019,63.182418835288,-3.));
#35686=CARTESIAN_POINT('Ctrl Pts',(-56.8363964827363,63.1266224052846,-3.));
#35687=CARTESIAN_POINT('Ctrl Pts',(-56.7905229461631,63.0696144344366,-3.));
#35688=CARTESIAN_POINT('Ctrl Pts',(-56.746043369936,63.0114459376167,-3.));
#35689=CARTESIAN_POINT('Ctrl Pts',(-56.7284856436537,62.9884846904095,-3.));
#35690=CARTESIAN_POINT('Ctrl Pts',(-56.7111451693665,62.9653426048408,-3.));
#35691=CARTESIAN_POINT('Ctrl Pts',(-56.6940251437079,62.9420227923607,-3.));
#35692=CARTESIAN_POINT('Ctrl Pts',(-56.6800433710512,62.9229777089597,-3.));
#35693=CARTESIAN_POINT('Ctrl Pts',(-56.6662062873437,62.9038106341118,-3.));
#35694=CARTESIAN_POINT('Ctrl Pts',(-56.6525316070086,62.8845461048891,-3.));
#35695=CARTESIAN_POINT('Ctrl Pts',(-56.5757647893409,62.776399035557,-3.));
#35696=CARTESIAN_POINT('Ctrl Pts',(-56.5040156403888,62.6650546667281,-3.));
#35697=CARTESIAN_POINT('Ctrl Pts',(-56.4374818016433,62.5508627236001,-3.));
#35698=CARTESIAN_POINT('Ctrl Pts',(-56.371191044164,62.4370879805415,-3.));
#35699=CARTESIAN_POINT('Ctrl Pts',(-56.3100772593781,62.3204856755393,-3.));
#35700=CARTESIAN_POINT('Ctrl Pts',(-56.2543835497104,62.2013821593283,-3.));
#35701=CARTESIAN_POINT('Ctrl Pts',(-56.199678842756,62.0843936701357,-3.));
#35702=CARTESIAN_POINT('Ctrl Pts',(-56.1502032662197,61.9649913135364,-3.));
#35703=CARTESIAN_POINT('Ctrl Pts',(-56.106236400397,61.8434762599769,-3.));
#35704=CARTESIAN_POINT('Ctrl Pts',(-56.0839234706096,61.7818080740045,-3.));
#35705=CARTESIAN_POINT('Ctrl Pts',(-56.0630301163055,61.7195956965504,-3.));
#35706=CARTESIAN_POINT('Ctrl Pts',(-56.0435980583969,61.6568785281303,-3.));
#35707=CARTESIAN_POINT('Ctrl Pts',(-56.0170092286204,61.5710628042873,-3.));
#35708=CARTESIAN_POINT('Ctrl Pts',(-55.9931559383444,61.4843017840239,-3.));
#35709=CARTESIAN_POINT('Ctrl Pts',(-55.9720760437321,61.396731441251,-3.));
#35710=CARTESIAN_POINT('Origin',(-60.,60.,-13.3123464956316));
#35711=CARTESIAN_POINT('Ctrl Pts',(-54.9007451799907,60.0000912485532,-9.56234649563159));
#35712=CARTESIAN_POINT('Ctrl Pts',(-54.9006553198669,60.1069729386028,-9.55734157105846));
#35713=CARTESIAN_POINT('Ctrl Pts',(-54.9296017816049,61.0460695450124,-9.51336443385491));
#35714=CARTESIAN_POINT('Ctrl Pts',(-55.4826600663013,62.7859966694522,-9.43041508402092));
#35715=CARTESIAN_POINT('Ctrl Pts',(-57.3241694659746,64.5834554691913,-9.31349844612963));
#35716=CARTESIAN_POINT('Ctrl Pts',(-59.7947368645222,65.3033954038122,-9.19658180823834));
#35717=CARTESIAN_POINT('Ctrl Pts',(-62.3135594152741,64.7765654229855,-9.07966517034706));
#35718=CARTESIAN_POINT('Ctrl Pts',(-64.2884897335979,63.1268180153125,-8.96274853245577));
#35719=CARTESIAN_POINT('Ctrl Pts',(-65.2552436145005,60.7419901177753,-8.84583189456448));
#35720=CARTESIAN_POINT('Ctrl Pts',(-64.9865478950058,58.1827288524753,-8.72891525667319));
#35721=CARTESIAN_POINT('Ctrl Pts',(-63.5455699950673,56.0506873380101,-8.61199861878189));
#35722=CARTESIAN_POINT('Ctrl Pts',(-61.2710678117403,54.8470867175201,-8.49508198089061));
#35723=CARTESIAN_POINT('Ctrl Pts',(-58.6977517313953,54.8548763465959,-8.37816534299932));
#35724=CARTESIAN_POINT('Ctrl Pts',(-56.4305796456292,56.0722332088069,-8.26124870510802));
#35725=CARTESIAN_POINT('Ctrl Pts',(-55.1447571773361,57.9997588942346,-8.15597575598546));
#35726=CARTESIAN_POINT('Ctrl Pts',(-54.901652700544,59.4163727828879,-8.08967501949331));
#35727=CARTESIAN_POINT('Ctrl Pts',(-54.9011518189288,60.0001169870244,-8.06234649563159));
#35728=CARTESIAN_POINT('Ctrl Pts',(-54.9012106446239,60.0001195814448,-9.68765350436841));
#35729=CARTESIAN_POINT('Ctrl Pts',(-54.9010041693968,60.2735579920353,-9.67485236502099));
#35730=CARTESIAN_POINT('Ctrl Pts',(-54.988526949539,61.3793291690848,-9.62307901304313));
#35731=CARTESIAN_POINT('Ctrl Pts',(-55.7768178011049,63.214507276628,-9.53233344843484));
#35732=CARTESIAN_POINT('Ctrl Pts',(-57.7853302019076,64.8232034014141,-9.41541681054356));
#35733=CARTESIAN_POINT('Ctrl Pts',(-60.3144620657417,65.2980444973094,-9.29850017265226));
#35734=CARTESIAN_POINT('Ctrl Pts',(-62.769679003779,64.5273620844534,-9.18158353476097));
#35735=CARTESIAN_POINT('Ctrl Pts',(-64.5737697114167,62.6923525936502,-9.06466689686969));
#35736=CARTESIAN_POINT('Ctrl Pts',(-65.3026202914353,60.2243982367199,-8.94775025897839));
#35737=CARTESIAN_POINT('Ctrl Pts',(-64.7848823971216,57.703691543606,-8.83083362108711));
#35738=CARTESIAN_POINT('Ctrl Pts',(-63.1422721706319,55.7228209792253,-8.71391698319582));
#35739=CARTESIAN_POINT('Ctrl Pts',(-60.7609482860978,54.7474681235472,-8.59700034530452));
#35740=CARTESIAN_POINT('Ctrl Pts',(-58.2007340318709,55.0069271910455,-8.48008370741324));
#35741=CARTESIAN_POINT('Ctrl Pts',(-56.0635071617532,56.4402025452955,-8.36316706952194));
#35742=CARTESIAN_POINT('Ctrl Pts',(-55.0531942753161,58.3328863911516,-8.26569033517368));
#35743=CARTESIAN_POINT('Ctrl Pts',(-54.9013976405776,59.5827292162986,-8.20718581345583));
#35744=CARTESIAN_POINT('Ctrl Pts',(-54.9013950998961,60.0000009027484,-8.18765350436842));
#35745=CARTESIAN_POINT('Ctrl Pts',(-63.2233527839579,62.7898325810254,-10.));
#35746=CARTESIAN_POINT('Ctrl Pts',(-63.6787829722545,62.2636317705077,-9.96102778736957));
#35747=CARTESIAN_POINT('Ctrl Pts',(-64.3265773596221,60.9843937251917,-9.88308336210871));
#35748=CARTESIAN_POINT('Ctrl Pts',(-64.2810882745412,58.8332762706057,-9.76616672421742));
#35749=CARTESIAN_POINT('Ctrl Pts',(-63.229077517363,56.9567113445499,-9.64925008632613));
#35750=CARTESIAN_POINT('Ctrl Pts',(-61.41796272213,55.7954439251957,-9.53233344843485));
#35751=CARTESIAN_POINT('Ctrl Pts',(-59.2734876021215,55.622683427384,-9.41541681054355));
#35752=CARTESIAN_POINT('Ctrl Pts',(-57.2998122688331,56.4789515210604,-9.29850017265226));
#35753=CARTESIAN_POINT('Ctrl Pts',(-55.96091867892,58.1629927736796,-9.18158353476098));
#35754=CARTESIAN_POINT('Ctrl Pts',(-55.5715694755394,60.2788877013121,-9.06466689686968));
#35755=CARTESIAN_POINT('Ctrl Pts',(-56.223294736741,62.3292221615758,-8.94775025897839));
#35756=CARTESIAN_POINT('Ctrl Pts',(-57.7628818265247,63.8319809109948,-8.8308336210871));
#35757=CARTESIAN_POINT('Ctrl Pts',(-59.8283905184268,64.433884017739,-8.71391698319582));
#35758=CARTESIAN_POINT('Ctrl Pts',(-61.9342427509931,63.9934297701877,-8.59700034530453));
#35759=CARTESIAN_POINT('Ctrl Pts',(-63.585375903967,62.6141645811487,-8.48008370741324));
#35760=CARTESIAN_POINT('Ctrl Pts',(-64.393626893237,60.6203380804229,-8.36316706952195));
#35761=CARTESIAN_POINT('Ctrl Pts',(-64.1689848355383,58.4806772108457,-8.24625043163066));
#35762=CARTESIAN_POINT('Ctrl Pts',(-62.9642606175665,56.6981918262281,-8.12933379373937));
#35763=CARTESIAN_POINT('Ctrl Pts',(-61.06267152019,55.6919260005468,-8.01241715584808));
#35764=CARTESIAN_POINT('Ctrl Pts',(-58.9112601747281,55.6984384909861,-7.89550051795679));
#35765=CARTESIAN_POINT('Ctrl Pts',(-57.0157993781756,56.7162051714344,-7.7785838800655));
#35766=CARTESIAN_POINT('Ctrl Pts',(-55.8218913855027,58.5059454961382,-7.66166724217421));
#35767=CARTESIAN_POINT('Ctrl Pts',(-55.610209865439,60.6469434343234,-7.54475060428292));
#35768=CARTESIAN_POINT('Ctrl Pts',(-56.4305207028874,62.6358047497177,-7.42783396639163));
#35769=CARTESIAN_POINT('Ctrl Pts',(-58.0899737944543,64.0051198695055,-7.31091732850034));
#35770=CARTESIAN_POINT('Ctrl Pts',(-60.1984589714611,64.4326546672265,-7.19400069060905));
#35771=CARTESIAN_POINT('Ctrl Pts',(-62.2602755751237,63.8185984946696,-7.07708405271776));
#35772=CARTESIAN_POINT('Ctrl Pts',(-63.7907548362926,62.3058012416029,-6.96016741482647));
#35773=CARTESIAN_POINT('Ctrl Pts',(-64.4300091285896,60.2531589262444,-6.84325077693518));
#35774=CARTESIAN_POINT('Ctrl Pts',(-64.0279514449107,58.1361887346157,-6.72633413904389));
#35775=CARTESIAN_POINT('Ctrl Pts',(-62.6787003804465,56.4677145273824,-6.60941750115261));
#35776=CARTESIAN_POINT('Ctrl Pts',(-60.040721219432,55.3204109471847,-6.45352865063089));
#35777=CARTESIAN_POINT('Ctrl Pts',(-56.3381268516022,56.5785262980586,-6.25866758747874));
#35778=CARTESIAN_POINT('Ctrl Pts',(-55.1221049889056,61.1497554125864,-6.02483431169616));
#35779=CARTESIAN_POINT('Ctrl Pts',(-57.7101830808087,64.0812927360737,-5.82997324854401));
#35780=CARTESIAN_POINT('Ctrl Pts',(-60.5695473859375,64.3963726142629,-5.67408439802229));
#35781=CARTESIAN_POINT('Ctrl Pts',(-62.569477548857,63.6188355035077,-5.557167760131));
#35782=CARTESIAN_POINT('Ctrl Pts',(-63.9702556002071,61.9814491642124,-5.44025112223971));
#35783=CARTESIAN_POINT('Ctrl Pts',(-64.435395460414,59.8824895563441,-5.32333448434842));
#35784=CARTESIAN_POINT('Ctrl Pts',(-63.8588751572395,57.8091958873783,-5.20641784645713));
#35785=CARTESIAN_POINT('Ctrl Pts',(-62.374688490879,56.2518447292755,-5.08950120856584));
#35786=CARTESIAN_POINT('Ctrl Pts',(-60.3324645529654,55.5752228761179,-4.97258457067455));
#35787=CARTESIAN_POINT('Ctrl Pts',(-58.2119773478597,55.93901192728,-4.85566793278326));
#35788=CARTESIAN_POINT('Ctrl Pts',(-56.5118828738941,57.2574041226595,-4.73875129489197));
#35789=CARTESIAN_POINT('Ctrl Pts',(-55.631783700059,59.2205920103183,-4.62183465700068));
#35790=CARTESIAN_POINT('Ctrl Pts',(-55.778614193939,61.366990745641,-4.50491801910939));
#35791=CARTESIAN_POINT('Ctrl Pts',(-56.9178409418314,63.1920340492318,-4.3880013812181));
#35792=CARTESIAN_POINT('Ctrl Pts',(-58.781651390282,64.2666613413666,-4.27108474332681));
#35793=CARTESIAN_POINT('Ctrl Pts',(-60.9318810632418,64.3382457169127,-4.15416810543552));
#35794=CARTESIAN_POINT('Ctrl Pts',(-62.8630363220205,63.3899556613623,-4.03725146754423));
#35795=CARTESIAN_POINT('Ctrl Pts',(-64.1211231584726,61.6447249909761,-3.92033482965295));
#35796=CARTESIAN_POINT('Ctrl Pts',(-64.4103798056068,59.5128374617724,-3.80341819176165));
#35797=CARTESIAN_POINT('Ctrl Pts',(-63.6628046569468,57.4954766114706,-3.68650155387037));
#35798=CARTESIAN_POINT('Ctrl Pts',(-62.0541453323136,56.0669012832628,-3.56958491597908));
#35799=CARTESIAN_POINT('Ctrl Pts',(-59.9625778285317,55.5629542684651,-3.45266827808779));
#35800=CARTESIAN_POINT('Ctrl Pts',(-57.8798107643185,56.1021068410437,-3.3357516401965));
#35801=CARTESIAN_POINT('Ctrl Pts',(-56.2954704227517,57.5576124826779,-3.21883500230521));
#35802=CARTESIAN_POINT('Ctrl Pts',(-55.5820374028276,59.5872929237356,-3.10191836441392));
#35803=CARTESIAN_POINT('Ctrl Pts',(-55.9071888205857,61.7140031265185,-2.98500172652263));
#35804=CARTESIAN_POINT('Ctrl Pts',(-57.1945760881725,63.437752772978,-2.86808508863134));
#35805=CARTESIAN_POINT('Ctrl Pts',(-59.1413430300255,64.3533515000793,-2.75116845074005));
#35806=CARTESIAN_POINT('Ctrl Pts',(-61.2902326596918,64.2454213381917,-2.63425181284876));
#35807=CARTESIAN_POINT('Ctrl Pts',(-62.5200516280627,63.5081067174902,-2.5563073875879));
#35808=CARTESIAN_POINT('Ctrl Pts',(-63.0124573356753,63.0163338344314,-2.51733517495747));
#35809=CARTESIAN_POINT('Ctrl Pts',(-63.4340590883905,62.9722002436837,-10.1608882750142));
#35810=CARTESIAN_POINT('Ctrl Pts',(-63.9192601452004,62.4116023827638,-10.1219160623837));
#35811=CARTESIAN_POINT('Ctrl Pts',(-64.609399994124,61.0487422398731,-10.0439716371229));
#35812=CARTESIAN_POINT('Ctrl Pts',(-64.5609373477695,58.7570090849169,-9.9270549992316));
#35813=CARTESIAN_POINT('Ctrl Pts',(-63.44015804004,56.7577755938301,-9.81013836134031));
#35814=CARTESIAN_POINT('Ctrl Pts',(-61.5106530681853,55.5205976605514,-9.69322172344902));
#35815=CARTESIAN_POINT('Ctrl Pts',(-59.2259964484248,55.336544037697,-9.57630508555773));
#35816=CARTESIAN_POINT('Ctrl Pts',(-57.1233045713387,56.2487852431346,-9.45938844766644));
#35817=CARTESIAN_POINT('Ctrl Pts',(-55.6968892798722,58.0429100431139,-9.34247180977516));
#35818=CARTESIAN_POINT('Ctrl Pts',(-55.2820888344847,60.297118221157,-9.22555517188385));
#35819=CARTESIAN_POINT('Ctrl Pts',(-55.9764165132611,62.4814803308679,-9.10863853399257));
#35820=CARTESIAN_POINT('Ctrl Pts',(-57.616644373008,64.0824724303936,-8.99172189610128));
#35821=CARTESIAN_POINT('Ctrl Pts',(-59.817172633792,64.7237211464301,-8.87480525820999));
#35822=CARTESIAN_POINT('Ctrl Pts',(-62.0606816390868,64.254474987787,-8.7578886203187));
#35823=CARTESIAN_POINT('Ctrl Pts',(-63.8197471805106,62.7850490592033,-8.64097198242742));
#35824=CARTESIAN_POINT('Ctrl Pts',(-64.6808324669915,60.6608887595404,-8.52405534453612));
#35825=CARTESIAN_POINT('Ctrl Pts',(-64.4415058553609,58.3813610913889,-8.40713870664483));
#35826=CARTESIAN_POINT('Ctrl Pts',(-63.1580304100668,56.4823569968221,-8.29022206875354));
#35827=CARTESIAN_POINT('Ctrl Pts',(-61.1321369507068,55.4103129062046,-8.17330543086225));
#35828=CARTESIAN_POINT('Ctrl Pts',(-58.8400906936171,55.4172511095227,-8.05638879297097));
#35829=CARTESIAN_POINT('Ctrl Pts',(-56.8207261339935,56.5015478505586,-7.93947215507967));
#35830=CARTESIAN_POINT('Ctrl Pts',(-55.5487739563277,58.408281131041,-7.82255551718839));
#35831=CARTESIAN_POINT('Ctrl Pts',(-55.3232550955201,60.6892332702054,-7.70563887929709));
#35832=CARTESIAN_POINT('Ctrl Pts',(-56.19718856649,62.8081038169445,-7.58872224140581));
#35833=CARTESIAN_POINT('Ctrl Pts',(-57.9651179098787,64.2669292534219,-7.47180560351451));
#35834=CARTESIAN_POINT('Ctrl Pts',(-60.2114319717067,64.7224114349019,-7.35488896562323));
#35835=CARTESIAN_POINT('Ctrl Pts',(-62.4080267973306,64.0682152232288,-7.23797232773193));
#35836=CARTESIAN_POINT('Ctrl Pts',(-64.038551461763,62.4565284163609,-7.12105568984065));
#35837=CARTESIAN_POINT('Ctrl Pts',(-64.7195929609065,60.2697075901227,-7.00413905194936));
#35838=CARTESIAN_POINT('Ctrl Pts',(-64.291253298687,58.0143538594995,-6.88722241405807));
#35839=CARTESIAN_POINT('Ctrl Pts',(-62.8538034782691,56.2368137020554,-6.77030577616678));
#35840=CARTESIAN_POINT('Ctrl Pts',(-60.0433831116398,55.0145124056135,-6.61441692564506));
#35841=CARTESIAN_POINT('Ctrl Pts',(-56.0987550514566,56.3548690914888,-6.41955586249291));
#35842=CARTESIAN_POINT('Ctrl Pts',(-54.803243449358,61.224913401868,-6.18572258671033));
#35843=CARTESIAN_POINT('Ctrl Pts',(-57.5605007800468,64.3480814394404,-5.99086152355819));
#35844=CARTESIAN_POINT('Ctrl Pts',(-60.6067779445929,64.6837576721661,-5.83497267303646));
#35845=CARTESIAN_POINT('Ctrl Pts',(-62.7374408947671,63.8553939897797,-5.71805603514517));
#35846=CARTESIAN_POINT('Ctrl Pts',(-64.2297859529926,62.1109738730467,-5.60113939725388));
#35847=CARTESIAN_POINT('Ctrl Pts',(-64.7253313901119,59.8748080542019,-5.48422275936259));
#35848=CARTESIAN_POINT('Ctrl Pts',(-64.1111247179129,57.6659859227094,-5.36730612147131));
#35849=CARTESIAN_POINT('Ctrl Pts',(-62.5299187339296,56.0068327810132,-5.25038948358002));
#35850=CARTESIAN_POINT('Ctrl Pts',(-60.3541973206782,55.2859810530227,-5.13347284568872));
#35851=CARTESIAN_POINT('Ctrl Pts',(-58.0950966740627,55.6735505128775,-5.01655620779744));
#35852=CARTESIAN_POINT('Ctrl Pts',(-56.2838692749086,57.0781242607894,-4.89963956990615));
#35853=CARTESIAN_POINT('Ctrl Pts',(-55.3462391831499,59.1696431418083,-4.78272293201486));
#35854=CARTESIAN_POINT('Ctrl Pts',(-55.5026677920415,61.4563491210696,-4.66580629412357));
#35855=CARTESIAN_POINT('Ctrl Pts',(-56.7163642843423,63.400693089435,-4.54888965623228));
#35856=CARTESIAN_POINT('Ctrl Pts',(-58.7020095545072,64.5455673450715,-4.43197301834099));
#35857=CARTESIAN_POINT('Ctrl Pts',(-60.9927968947275,64.6218310964842,-4.3150563804497));
#35858=CARTESIAN_POINT('Ctrl Pts',(-63.0501892163211,63.611552575343,-4.19813974255841));
#35859=CARTESIAN_POINT('Ctrl Pts',(-64.3905155238243,61.7522384863594,-4.08122310466712));
#35860=CARTESIAN_POINT('Ctrl Pts',(-64.6986804950654,59.4809922915512,-3.96430646677583));
#35861=CARTESIAN_POINT('Ctrl Pts',(-63.9022373485731,57.3317592330352,-3.84738982888454));
#35862=CARTESIAN_POINT('Ctrl Pts',(-62.1884220934219,55.8097998267617,-3.73047319099325));
#35863=CARTESIAN_POINT('Ctrl Pts',(-59.960131590722,55.2729104627288,-3.61355655310196));
#35864=CARTESIAN_POINT('Ctrl Pts',(-57.7412168006756,55.8473067252498,-3.49663991521067));
#35865=CARTESIAN_POINT('Ctrl Pts',(-56.0533102283206,57.3979568438882,-3.37972327731939));
#35866=CARTESIAN_POINT('Ctrl Pts',(-55.2932410363222,59.5603148084993,-3.2628066394281));
#35867=CARTESIAN_POINT('Ctrl Pts',(-55.6396471718258,61.8260452419121,-3.1458900015368));
#35868=CARTESIAN_POINT('Ctrl Pts',(-57.0111892408593,63.6624741208715,-3.02897336364552));
#35869=CARTESIAN_POINT('Ctrl Pts',(-59.0852137605831,64.6379243246994,-2.91205672575423));
#35870=CARTESIAN_POINT('Ctrl Pts',(-61.3745734606538,64.5229389110065,-2.79514008786294));
#35871=CARTESIAN_POINT('Ctrl Pts',(-62.6847840669602,63.7374270096023,-2.71719566260208));
#35872=CARTESIAN_POINT('Ctrl Pts',(-63.2093776838358,63.2135075841839,-2.67822344997165));
#35873=CARTESIAN_POINT('Ctrl Pts',(-63.6447653928231,63.154567906342,-10.3217765500284));
#35874=CARTESIAN_POINT('Ctrl Pts',(-64.1597373181463,62.55957299502,-10.2828043373979));
#35875=CARTESIAN_POINT('Ctrl Pts',(-64.8922226286258,61.1130907545544,-10.2048599121371));
#35876=CARTESIAN_POINT('Ctrl Pts',(-64.8407864209977,58.6807418992281,-10.0879432742458));
#35877=CARTESIAN_POINT('Ctrl Pts',(-63.6512385627169,56.5588398431102,-9.97102663635448));
#35878=CARTESIAN_POINT('Ctrl Pts',(-61.6033434142406,55.2457513959071,-9.8541099984632));
#35879=CARTESIAN_POINT('Ctrl Pts',(-59.1785052947282,55.05040464801,-9.73719336057191));
#35880=CARTESIAN_POINT('Ctrl Pts',(-56.9467968738444,56.0186189652088,-9.62027672268061));
#35881=CARTESIAN_POINT('Ctrl Pts',(-55.4328598808243,57.9228273125483,-9.50336008478933));
#35882=CARTESIAN_POINT('Ctrl Pts',(-54.9926081934299,60.315348741002,-9.38644344689803));
#35883=CARTESIAN_POINT('Ctrl Pts',(-55.7295382897812,62.63373850016,-9.26952680900674));
#35884=CARTESIAN_POINT('Ctrl Pts',(-57.4704069194913,64.3329639497925,-9.15261017111546));
#35885=CARTESIAN_POINT('Ctrl Pts',(-59.8059547491571,65.0135582751211,-9.03569353322417));
#35886=CARTESIAN_POINT('Ctrl Pts',(-62.1871205271805,64.5155202053863,-8.91877689533288));
#35887=CARTESIAN_POINT('Ctrl Pts',(-64.0541184570542,62.9559335372579,-8.80186025744159));
#35888=CARTESIAN_POINT('Ctrl Pts',(-64.968038040746,60.7014394386578,-8.6849436195503));
#35889=CARTESIAN_POINT('Ctrl Pts',(-64.7140268751833,58.2820449719321,-8.56802698165901));
#35890=CARTESIAN_POINT('Ctrl Pts',(-63.351800202567,56.2665221674161,-8.45111034376772));
#35891=CARTESIAN_POINT('Ctrl Pts',(-61.2016023812236,55.1286998118624,-8.33419370587643));
#35892=CARTESIAN_POINT('Ctrl Pts',(-58.7689212125062,55.1360637280593,-8.21727706798515));
#35893=CARTESIAN_POINT('Ctrl Pts',(-56.6256528898113,56.2868905296827,-8.10036043009385));
#35894=CARTESIAN_POINT('Ctrl Pts',(-55.2756565271526,58.3106167659438,-7.98344379220257));
#35895=CARTESIAN_POINT('Ctrl Pts',(-55.0363003256012,60.7315231060873,-7.86652715431127));
#35896=CARTESIAN_POINT('Ctrl Pts',(-55.9638564300926,62.9804028841713,-7.74961051641998));
#35897=CARTESIAN_POINT('Ctrl Pts',(-57.8402620253032,64.5287386373382,-7.63269387852869));
#35898=CARTESIAN_POINT('Ctrl Pts',(-60.2244049719524,65.0121682025774,-7.51577724063741));
#35899=CARTESIAN_POINT('Ctrl Pts',(-62.5557780195374,64.317831951788,-7.39886060274611));
#35900=CARTESIAN_POINT('Ctrl Pts',(-64.2863480872334,62.6072555911189,-7.28194396485483));
#35901=CARTESIAN_POINT('Ctrl Pts',(-65.0091767932234,60.2862562540011,-7.16502732696354));
#35902=CARTESIAN_POINT('Ctrl Pts',(-64.5545551524633,57.8925189843833,-7.04811068907224));
#35903=CARTESIAN_POINT('Ctrl Pts',(-63.0289065760917,56.0059128767283,-6.93119405118096));
#35904=CARTESIAN_POINT('Ctrl Pts',(-60.0460450038475,54.7086138640423,-6.77530520065924));
#35905=CARTESIAN_POINT('Ctrl Pts',(-55.8593832513112,56.1312118849188,-6.58044413750709));
#35906=CARTESIAN_POINT('Ctrl Pts',(-54.4843819098103,61.3000713911496,-6.34661086172451));
#35907=CARTESIAN_POINT('Ctrl Pts',(-57.4108184792849,64.6148701428072,-6.15174979857236));
#35908=CARTESIAN_POINT('Ctrl Pts',(-60.6440085032482,64.9711427300693,-5.99586094805064));
#35909=CARTESIAN_POINT('Ctrl Pts',(-62.9054042406772,64.0919524760517,-5.87894431015935));
#35910=CARTESIAN_POINT('Ctrl Pts',(-64.489316305778,62.240498581881,-5.76202767226806));
#35911=CARTESIAN_POINT('Ctrl Pts',(-65.0152673198098,59.8671265520597,-5.64511103437677));
#35912=CARTESIAN_POINT('Ctrl Pts',(-64.3633742785863,57.5227759580404,-5.52819439648548));
#35913=CARTESIAN_POINT('Ctrl Pts',(-62.6851489769803,55.761820832751,-5.41127775859419));
#35914=CARTESIAN_POINT('Ctrl Pts',(-60.375930088391,54.9967392299274,-5.2943611207029));
#35915=CARTESIAN_POINT('Ctrl Pts',(-57.9782160002658,55.408089098475,-5.17744448281162));
#35916=CARTESIAN_POINT('Ctrl Pts',(-56.0558556759232,56.8988443989193,-5.06052784492033));
#35917=CARTESIAN_POINT('Ctrl Pts',(-55.0606946662407,59.1186942732983,-4.94361120702903));
#35918=CARTESIAN_POINT('Ctrl Pts',(-55.226721390144,61.5457074964981,-4.82669456913774));
#35919=CARTESIAN_POINT('Ctrl Pts',(-56.5148876268531,63.609352129638,-4.70977793124646));
#35920=CARTESIAN_POINT('Ctrl Pts',(-58.6223677187324,64.8244733487765,-4.59286129335517));
#35921=CARTESIAN_POINT('Ctrl Pts',(-61.0537127262131,64.9054164760556,-4.47594465546388));
#35922=CARTESIAN_POINT('Ctrl Pts',(-63.2373421106216,63.8331494893237,-4.35902801757258));
#35923=CARTESIAN_POINT('Ctrl Pts',(-64.659907889176,61.8597519817425,-4.2421113796813));
#35924=CARTESIAN_POINT('Ctrl Pts',(-64.9869811845242,59.4491471213301,-4.12519474179001));
#35925=CARTESIAN_POINT('Ctrl Pts',(-64.1416700401993,57.1680418545997,-4.00827810389872));
#35926=CARTESIAN_POINT('Ctrl Pts',(-62.3226988545302,55.5526983702606,-3.89136146600743));
#35927=CARTESIAN_POINT('Ctrl Pts',(-59.9576853529124,54.9828666569923,-3.77444482811614));
#35928=CARTESIAN_POINT('Ctrl Pts',(-57.6026228370326,55.592506609456,-3.65752819022485));
#35929=CARTESIAN_POINT('Ctrl Pts',(-55.8111500338895,57.2383012050985,-3.54061155233356));
#35930=CARTESIAN_POINT('Ctrl Pts',(-55.0044446698169,59.533336693263,-3.42369491444227));
#35931=CARTESIAN_POINT('Ctrl Pts',(-55.3721055230659,61.9380873573058,-3.30677827655098));
#35932=CARTESIAN_POINT('Ctrl Pts',(-56.8278023935462,63.8871954687649,-3.18986163865969));
#35933=CARTESIAN_POINT('Ctrl Pts',(-59.0290844911407,64.9224971493195,-3.0729450007684));
#35934=CARTESIAN_POINT('Ctrl Pts',(-61.4589142616157,64.8004564838213,-2.95602836287711));
#35935=CARTESIAN_POINT('Ctrl Pts',(-62.8495165058577,63.9667473017145,-2.87808393761625));
#35936=CARTESIAN_POINT('Ctrl Pts',(-63.4062980319963,63.4106813339364,-2.83911172498582));
#35937=CARTESIAN_POINT('Ctrl Pts',(-63.8554716972558,63.3369355690004,-10.4826648250425));
#35938=CARTESIAN_POINT('Ctrl Pts',(-64.4002144910922,62.7075436072762,-10.4436926124121));
#35939=CARTESIAN_POINT('Ctrl Pts',(-65.1750452631277,61.1774392692358,-10.3657481871512));
#35940=CARTESIAN_POINT('Ctrl Pts',(-65.120635494226,58.6044747135393,-10.24883154926));
#35941=CARTESIAN_POINT('Ctrl Pts',(-63.8623190853939,56.3599040923904,-10.1319149113687));
#35942=CARTESIAN_POINT('Ctrl Pts',(-61.6960337602958,54.9709051312627,-10.0149982734774));
#35943=CARTESIAN_POINT('Ctrl Pts',(-59.1310141410315,54.764265258323,-9.89808163558608));
#35944=CARTESIAN_POINT('Ctrl Pts',(-56.77028917635,55.7884526872829,-9.78116499769479));
#35945=CARTESIAN_POINT('Ctrl Pts',(-55.1688304817765,57.8027445819827,-9.6642483598035));
#35946=CARTESIAN_POINT('Ctrl Pts',(-54.7031275523752,60.3335792608469,-9.54733172191221));
#35947=CARTESIAN_POINT('Ctrl Pts',(-55.4826600663013,62.7859966694522,-9.43041508402092));
#35948=CARTESIAN_POINT('Ctrl Pts',(-57.3241694659746,64.5834554691913,-9.31349844612963));
#35949=CARTESIAN_POINT('Ctrl Pts',(-59.7947368645222,65.3033954038122,-9.19658180823834));
#35950=CARTESIAN_POINT('Ctrl Pts',(-62.3135594152741,64.7765654229855,-9.07966517034706));
#35951=CARTESIAN_POINT('Ctrl Pts',(-64.2884897335979,63.1268180153125,-8.96274853245577));
#35952=CARTESIAN_POINT('Ctrl Pts',(-65.2552436145005,60.7419901177753,-8.84583189456448));
#35953=CARTESIAN_POINT('Ctrl Pts',(-64.9865478950058,58.1827288524753,-8.72891525667319));
#35954=CARTESIAN_POINT('Ctrl Pts',(-63.5455699950673,56.0506873380101,-8.61199861878189));
#35955=CARTESIAN_POINT('Ctrl Pts',(-61.2710678117403,54.8470867175201,-8.49508198089061));
#35956=CARTESIAN_POINT('Ctrl Pts',(-58.6977517313953,54.8548763465959,-8.37816534299932));
#35957=CARTESIAN_POINT('Ctrl Pts',(-56.4305796456292,56.0722332088069,-8.26124870510802));
#35958=CARTESIAN_POINT('Ctrl Pts',(-55.0025390979776,58.2129524008466,-8.14433206721674));
#35959=CARTESIAN_POINT('Ctrl Pts',(-54.7493455556822,60.7738129419693,-8.02741542932545));
#35960=CARTESIAN_POINT('Ctrl Pts',(-55.7305242936952,63.1527019513981,-7.91049879143416));
#35961=CARTESIAN_POINT('Ctrl Pts',(-57.7154061407277,64.7905480212547,-7.79358215354287));
#35962=CARTESIAN_POINT('Ctrl Pts',(-60.237377972198,65.3019249702528,-7.67666551565158));
#35963=CARTESIAN_POINT('Ctrl Pts',(-62.7035292417443,64.5674486803472,-7.55974887776029));
#35964=CARTESIAN_POINT('Ctrl Pts',(-64.5341447127037,62.7579827658769,-7.442832239869));
#35965=CARTESIAN_POINT('Ctrl Pts',(-65.2987606255403,60.3028049178794,-7.32591560197772));
#35966=CARTESIAN_POINT('Ctrl Pts',(-64.8178570062396,57.770684109267,-7.20899896408642));
#35967=CARTESIAN_POINT('Ctrl Pts',(-63.2040096739143,55.7750120514012,-7.09208232619513));
#35968=CARTESIAN_POINT('Ctrl Pts',(-60.0487068960553,54.4027153224711,-6.93619347567341));
#35969=CARTESIAN_POINT('Ctrl Pts',(-55.6200114511657,55.9075546783489,-6.74133241252127));
#35970=CARTESIAN_POINT('Ctrl Pts',(-54.1655203702626,61.3752293804312,-6.50749913673868));
#35971=CARTESIAN_POINT('Ctrl Pts',(-57.261136178523,64.881658846174,-6.31263807358654));
#35972=CARTESIAN_POINT('Ctrl Pts',(-60.6812390619036,65.2585277879725,-6.15674922306482));
#35973=CARTESIAN_POINT('Ctrl Pts',(-63.0733675865873,64.3285109623237,-6.03983258517352));
#35974=CARTESIAN_POINT('Ctrl Pts',(-64.7488466585635,62.3700232907153,-5.92291594728224));
#35975=CARTESIAN_POINT('Ctrl Pts',(-65.3052032495076,59.8594450499176,-5.80599930939095));
#35976=CARTESIAN_POINT('Ctrl Pts',(-64.6156238392598,57.3795659933714,-5.68908267149965));
#35977=CARTESIAN_POINT('Ctrl Pts',(-62.8403792200309,55.5168088844888,-5.57216603360837));
#35978=CARTESIAN_POINT('Ctrl Pts',(-60.3976628561038,54.7074974068321,-5.45524939571708));
#35979=CARTESIAN_POINT('Ctrl Pts',(-57.8613353264688,55.1426276840725,-5.33833275782579));
#35980=CARTESIAN_POINT('Ctrl Pts',(-55.8278420769378,56.7195645370492,-5.2214161199345));
#35981=CARTESIAN_POINT('Ctrl Pts',(-54.7751501493316,59.0677454047883,-5.10449948204321));
#35982=CARTESIAN_POINT('Ctrl Pts',(-54.9507749882465,61.6350658719267,-4.98758284415192));
#35983=CARTESIAN_POINT('Ctrl Pts',(-56.3134109693639,63.8180111698412,-4.87066620626063));
#35984=CARTESIAN_POINT('Ctrl Pts',(-58.5427258829576,65.1033793524814,-4.75374956836935));
#35985=CARTESIAN_POINT('Ctrl Pts',(-61.1146285576988,65.189001855627,-4.63683293047805));
#35986=CARTESIAN_POINT('Ctrl Pts',(-63.4244950049221,64.0547464033043,-4.51991629258676));
#35987=CARTESIAN_POINT('Ctrl Pts',(-64.9293002545277,61.9672654771257,-4.40299965469547));
#35988=CARTESIAN_POINT('Ctrl Pts',(-65.2752818739828,59.417301951109,-4.28608301680418));
#35989=CARTESIAN_POINT('Ctrl Pts',(-64.3811027318255,57.0043244761643,-4.1691663789129));
#35990=CARTESIAN_POINT('Ctrl Pts',(-62.4569756156385,55.2955969137595,-4.0522497410216));
#35991=CARTESIAN_POINT('Ctrl Pts',(-59.9552391151028,54.6928228512559,-3.93533310313032));
#35992=CARTESIAN_POINT('Ctrl Pts',(-57.4640288733897,55.3377064936621,-3.81841646523903));
#35993=CARTESIAN_POINT('Ctrl Pts',(-55.5689898394584,57.0786455663088,-3.70149982734774));
#35994=CARTESIAN_POINT('Ctrl Pts',(-54.7156483033116,59.5063585780268,-3.58458318945645));
#35995=CARTESIAN_POINT('Ctrl Pts',(-55.104563874306,62.0501294726994,-3.46766655156516));
#35996=CARTESIAN_POINT('Ctrl Pts',(-56.644415546233,64.1119168166584,-3.35074991367387));
#35997=CARTESIAN_POINT('Ctrl Pts',(-58.9729552216983,65.2070699739396,-3.23383327578258));
#35998=CARTESIAN_POINT('Ctrl Pts',(-61.5432550625777,65.077974056636,-3.11691663789129));
#35999=CARTESIAN_POINT('Ctrl Pts',(-63.0142489447552,64.1960675938266,-3.03897221263043));
#36000=CARTESIAN_POINT('Ctrl Pts',(-63.6032183801568,63.6078550836889,-3.));
#36001=CARTESIAN_POINT('Ctrl Pts',(-63.2233527839579,62.7898325810254,-10.));
#36002=CARTESIAN_POINT('Ctrl Pts',(-63.3163082252117,62.7013635452477,-10.));
#36003=CARTESIAN_POINT('Ctrl Pts',(-63.4049730364641,62.6087978162202,-10.));
#36004=CARTESIAN_POINT('Ctrl Pts',(-63.489228887801,62.5125540616361,-10.));
#36005=CARTESIAN_POINT('Ctrl Pts',(-63.5750437123066,62.4145295235377,-10.));
#36006=CARTESIAN_POINT('Ctrl Pts',(-63.6562854342097,62.3126891791932,-10.));
#36007=CARTESIAN_POINT('Ctrl Pts',(-63.7328061009133,62.2074264239704,-10.));
#36008=CARTESIAN_POINT('Ctrl Pts',(-63.8104263008827,62.1006511374799,-10.));
#36009=CARTESIAN_POINT('Ctrl Pts',(-63.8831893713456,61.9903538684369,-10.));
#36010=CARTESIAN_POINT('Ctrl Pts',(-63.9509091476781,61.8769024196434,-10.));
#36011=CARTESIAN_POINT('Ctrl Pts',(-64.0184810129676,61.7636987673289,-10.));
#36012=CARTESIAN_POINT('Ctrl Pts',(-64.0810321009563,61.647354054786,-10.));
#36013=CARTESIAN_POINT('Ctrl Pts',(-64.1383380480206,61.5282002475095,-10.));
#36014=CARTESIAN_POINT('Ctrl Pts',(-64.1498926000478,61.5041753611593,-10.));
#36015=CARTESIAN_POINT('Ctrl Pts',(-64.1612337714855,61.4800361822972,-10.));
#36016=CARTESIAN_POINT('Ctrl Pts',(-64.1723594994649,61.4557853033111,-10.));
#36017=CARTESIAN_POINT('Ctrl Pts',(-64.1825650553464,61.4335401341746,-10.));
#36018=CARTESIAN_POINT('Ctrl Pts',(-64.192591209754,61.4111964786891,-10.));
#36019=CARTESIAN_POINT('Ctrl Pts',(-64.2024244346998,61.3887840242283,-10.));
#36020=CARTESIAN_POINT('Ctrl Pts',(-64.2596369074205,61.2583820506629,-10.));
#36021=CARTESIAN_POINT('Ctrl Pts',(-64.3103965387496,61.1254981286836,-10.));
#36022=CARTESIAN_POINT('Ctrl Pts',(-64.3545197254654,60.9906065311624,-10.));
#36023=CARTESIAN_POINT('Ctrl Pts',(-64.3960228498109,60.8637248809054,-10.));
#36024=CARTESIAN_POINT('Ctrl Pts',(-64.4316548200294,60.7350659665181,-10.));
#36025=CARTESIAN_POINT('Ctrl Pts',(-64.4614760030326,60.6050515502419,-10.));
#36026=CARTESIAN_POINT('Ctrl Pts',(-64.4916766813467,60.4733826100211,-10.));
#36027=CARTESIAN_POINT('Ctrl Pts',(-64.5159179809605,60.3403227556477,-10.));
#36028=CARTESIAN_POINT('Ctrl Pts',(-64.5342155848992,60.2062848307327,-10.));
#36029=CARTESIAN_POINT('Ctrl Pts',(-64.5504250806423,60.0875432085724,-10.));
#36030=CARTESIAN_POINT('Ctrl Pts',(-64.5619694608586,59.9680332992326,-10.));
#36031=CARTESIAN_POINT('Ctrl Pts',(-64.568827180765,59.8480327443896,-10.));
#36032=CARTESIAN_POINT('Ctrl Pts',(-64.5705438281414,59.8179938042673,-10.));
#36033=CARTESIAN_POINT('Ctrl Pts',(-64.5719666480006,59.7879240952274,-10.));
#36034=CARTESIAN_POINT('Ctrl Pts',(-64.5730949929817,59.7578279370814,-10.));
#36035=CARTESIAN_POINT('Ctrl Pts',(-64.5739023538582,59.7362933346079,-10.));
#36036=CARTESIAN_POINT('Ctrl Pts',(-64.5745589112559,59.7147434601342,-10.));
#36037=CARTESIAN_POINT('Ctrl Pts',(-64.5750641121509,59.6932014838883,-10.));
#36038=CARTESIAN_POINT('Ctrl Pts',(-64.5783093817702,59.5548218377918,-10.));
#36039=CARTESIAN_POINT('Ctrl Pts',(-64.5753216210849,59.4165720657667,-10.));
#36040=CARTESIAN_POINT('Ctrl Pts',(-64.5661669353703,59.2788928886624,-10.));
#36041=CARTESIAN_POINT('Ctrl Pts',(-64.5569092713095,59.1396649993025,-10.));
#36042=CARTESIAN_POINT('Ctrl Pts',(-64.5413453776093,59.0010198399725,-10.));
#36043=CARTESIAN_POINT('Ctrl Pts',(-64.5194941179384,58.8633947014968,-10.));
#36044=CARTESIAN_POINT('Ctrl Pts',(-64.5146773775864,58.8330575690879,-10.));
#36045=CARTESIAN_POINT('Ctrl Pts',(-64.5095549335052,58.802769955891,-10.));
#36046=CARTESIAN_POINT('Ctrl Pts',(-64.5041266528052,58.7725364859968,-10.));
#36047=CARTESIAN_POINT('Ctrl Pts',(-64.4796517796898,58.6362207019781,-10.));
#36048=CARTESIAN_POINT('Ctrl Pts',(-64.4489637483093,58.5010054273352,-10.));
#36049=CARTESIAN_POINT('Ctrl Pts',(-64.4122746888345,58.3672428220256,-10.));
#36050=CARTESIAN_POINT('Ctrl Pts',(-64.3910362571152,58.2898108027772,-10.));
#36051=CARTESIAN_POINT('Ctrl Pts',(-64.3677859044126,58.2128655794348,-10.));
#36052=CARTESIAN_POINT('Ctrl Pts',(-64.3425569213142,58.1364765318665,-10.));
#36053=CARTESIAN_POINT('Ctrl Pts',(-64.3288268949054,58.094904359244,-10.));
#36054=CARTESIAN_POINT('Ctrl Pts',(-64.3145107565515,58.0534969305004,-10.));
#36055=CARTESIAN_POINT('Ctrl Pts',(-64.2996131836605,58.0122656222771,-10.));
#36056=CARTESIAN_POINT('Ctrl Pts',(-64.2935454822379,57.995472331894,-10.));
#36057=CARTESIAN_POINT('Ctrl Pts',(-64.2873813217626,57.9787082598248,-10.));
#36058=CARTESIAN_POINT('Ctrl Pts',(-64.281120995717,57.9619741830157,-10.));
#36059=CARTESIAN_POINT('Ctrl Pts',(-64.2745734675927,57.9444724047148,-10.));
#36060=CARTESIAN_POINT('Ctrl Pts',(-64.2679239845411,57.9270121153241,-10.));
#36061=CARTESIAN_POINT('Ctrl Pts',(-64.2611740923314,57.9095963866901,-10.));
#36062=CARTESIAN_POINT('Ctrl Pts',(-64.2098991560052,57.7772994034123,-10.));
#36063=CARTESIAN_POINT('Ctrl Pts',(-64.1528186249486,57.6475317114888,-10.));
#36064=CARTESIAN_POINT('Ctrl Pts',(-64.0902108000695,57.5206511899074,-10.));
#36065=CARTESIAN_POINT('Ctrl Pts',(-64.0269891381023,57.3925266709493,-10.));
#36066=CARTESIAN_POINT('Ctrl Pts',(-63.958131089877,57.2673454677456,-10.));
#36067=CARTESIAN_POINT('Ctrl Pts',(-63.8838698934635,57.1454790252293,-10.));
#36068=CARTESIAN_POINT('Ctrl Pts',(-63.8095390881361,57.0234983509056,-10.));
#36069=CARTESIAN_POINT('Ctrl Pts',(-63.7297947443748,56.9048378848756,-10.));
#36070=CARTESIAN_POINT('Ctrl Pts',(-63.644820966864,56.7898844568111,-10.));
#36071=CARTESIAN_POINT('Ctrl Pts',(-63.6122160516634,56.7457761814837,-10.));
#36072=CARTESIAN_POINT('Ctrl Pts',(-63.5788407066558,56.7022139043511,-10.));
#36073=CARTESIAN_POINT('Ctrl Pts',(-63.5447035113608,56.6592204097588,-10.));
#36074=CARTESIAN_POINT('Ctrl Pts',(-63.4815422486248,56.5796730601769,-10.));
#36075=CARTESIAN_POINT('Ctrl Pts',(-63.4157735403968,56.5020723187067,-10.));
#36076=CARTESIAN_POINT('Ctrl Pts',(-63.3475133873057,56.4265027019109,-10.));
#36077=CARTESIAN_POINT('Ctrl Pts',(-63.3334676224538,56.4109528822957,-10.));
#36078=CARTESIAN_POINT('Ctrl Pts',(-63.3193163336919,56.3954890903373,-10.));
#36079=CARTESIAN_POINT('Ctrl Pts',(-63.3050604789436,56.380112108533,-10.));
#36080=CARTESIAN_POINT('Ctrl Pts',(-63.2906483358829,56.3645665473919,-10.));
#36081=CARTESIAN_POINT('Ctrl Pts',(-63.2761359893981,56.3491169160922,-10.));
#36082=CARTESIAN_POINT('Ctrl Pts',(-63.2615262143732,56.3337653362877,-10.));
#36083=CARTESIAN_POINT('Ctrl Pts',(-63.1618951178549,56.2290755154917,-10.));
#36084=CARTESIAN_POINT('Ctrl Pts',(-63.0577151863935,56.1289202614804,-10.));
#36085=CARTESIAN_POINT('Ctrl Pts',(-62.9493854884616,56.0334960532877,-10.));
#36086=CARTESIAN_POINT('Ctrl Pts',(-62.8507323432671,55.9465956146673,-10.));
#36087=CARTESIAN_POINT('Ctrl Pts',(-62.7486367809699,55.8636187255677,-10.));
#36088=CARTESIAN_POINT('Ctrl Pts',(-62.6433691001371,55.7847332403089,-10.));
#36089=CARTESIAN_POINT('Ctrl Pts',(-62.587860446671,55.7431361705331,-10.));
#36090=CARTESIAN_POINT('Ctrl Pts',(-62.5314693058621,55.7026770787173,-10.));
#36091=CARTESIAN_POINT('Ctrl Pts',(-62.47423249159,55.6633831252636,-10.));
#36092=CARTESIAN_POINT('Ctrl Pts',(-62.4525293449788,55.6484835812623,-10.));
#36093=CARTESIAN_POINT('Ctrl Pts',(-62.4307045902376,55.633751578947,-10.));
#36094=CARTESIAN_POINT('Ctrl Pts',(-62.4087601696795,55.619188673283,-10.));
#36095=CARTESIAN_POINT('Ctrl Pts',(-62.3869959955472,55.6047453839783,-10.));
#36096=CARTESIAN_POINT('Ctrl Pts',(-62.3651201281095,55.5904724631012,-10.));
#36097=CARTESIAN_POINT('Ctrl Pts',(-62.3431409641125,55.5763751194668,-10.));
#36098=CARTESIAN_POINT('Ctrl Pts',(-62.2178093976035,55.4959879781926,-10.));
#36099=CARTESIAN_POINT('Ctrl Pts',(-62.0890600516578,55.4212658232662,-10.));
#36100=CARTESIAN_POINT('Ctrl Pts',(-61.9572867186068,55.3524361931912,-10.));
#36101=CARTESIAN_POINT('Ctrl Pts',(-61.8473201865616,55.2949969864408,-10.));
#36102=CARTESIAN_POINT('Ctrl Pts',(-61.7352467486275,55.2416617648057,-10.));
#36103=CARTESIAN_POINT('Ctrl Pts',(-61.6212758664505,55.1925826499274,-10.));
#36104=CARTESIAN_POINT('Ctrl Pts',(-61.5232159559749,55.1503552536024,-10.));
#36105=CARTESIAN_POINT('Ctrl Pts',(-61.4237510391233,55.1112787685727,-10.));
#36106=CARTESIAN_POINT('Ctrl Pts',(-61.3230392943658,55.0753649202911,-10.));
#36107=CARTESIAN_POINT('Ctrl Pts',(-55.7371269276513,60.000097806567,-7.57968167058905));
#36108=CARTESIAN_POINT('Ctrl Pts',(-55.7375456878641,59.5120606341344,-7.60701019445077));
#36109=CARTESIAN_POINT('Ctrl Pts',(-55.8213219729741,59.0238810226661,-7.63433871831249));
#36110=CARTESIAN_POINT('Ctrl Pts',(-55.9855957976042,58.5644884317184,-7.6616672421742));
#36111=CARTESIAN_POINT('Ctrl Pts',(-56.2198607163937,57.9093653879036,-7.70063945480463));
#36112=CARTESIAN_POINT('Ctrl Pts',(-56.6178300472846,57.312785279669,-7.73961166743506));
#36113=CARTESIAN_POINT('Ctrl Pts',(-57.1327248454888,56.844867445477,-7.77858388006549));
#36114=CARTESIAN_POINT('Ctrl Pts',(-57.6476196436931,56.376949611285,-7.81755609269592));
#36115=CARTESIAN_POINT('Ctrl Pts',(-58.2794399092106,56.0376940511356,-7.85652830532636));
#36116=CARTESIAN_POINT('Ctrl Pts',(-58.9539185995463,55.8669808559876,-7.89550051795679));
#36117=CARTESIAN_POINT('Ctrl Pts',(-59.6283972898821,55.6962676608397,-7.93447273058721));
#36118=CARTESIAN_POINT('Ctrl Pts',(-60.345534405036,55.6940968306933,-7.97344494321764));
#36119=CARTESIAN_POINT('Ctrl Pts',(-61.0210344788425,55.8607223865669,-8.01241715584807));
#36120=CARTESIAN_POINT('Ctrl Pts',(-61.6965345526489,56.0273479424406,-8.0513893684785));
#36121=CARTESIAN_POINT('Ctrl Pts',(-62.3303975851077,56.3627698843344,-8.09036158110893));
#36122=CARTESIAN_POINT('Ctrl Pts',(-62.8481164709991,56.8275617527175,-8.12933379373936));
#36123=CARTESIAN_POINT('Ctrl Pts',(-63.3658353568905,57.2923536211006,-8.16830600636979));
#36124=CARTESIAN_POINT('Ctrl Pts',(-63.7674100962144,57.8865154159731,-8.20727821900022));
#36125=CARTESIAN_POINT('Ctrl Pts',(-64.0056378088262,58.5402064583389,-8.24625043163065));
#36126=CARTESIAN_POINT('Ctrl Pts',(-64.2438655214379,59.1938975007047,-8.28522264426108));
#36127=CARTESIAN_POINT('Ctrl Pts',(-64.3187462073375,59.9071177905638,-8.32419485689151));
#36128=CARTESIAN_POINT('Ctrl Pts',(-64.2214780520756,60.596032352281,-8.36316706952194));
#36129=CARTESIAN_POINT('Ctrl Pts',(-64.1242098968137,61.2849469139981,-8.40213928215237));
#36130=CARTESIAN_POINT('Ctrl Pts',(-63.8547929003903,61.9495557475734,-8.4411114947828));
#36131=CARTESIAN_POINT('Ctrl Pts',(-63.4448955433497,62.5117376958675,-8.48008370741323));
#36132=CARTESIAN_POINT('Ctrl Pts',(-63.034998186309,63.0739196441617,-8.51905592004366));
#36133=CARTESIAN_POINT('Ctrl Pts',(-62.4846204686511,63.5336747071747,-8.55802813267409));
#36134=CARTESIAN_POINT('Ctrl Pts',(-61.8584562377277,63.8369612799398,-8.59700034530452));
#36135=CARTESIAN_POINT('Ctrl Pts',(-61.2322920068043,64.1402478527048,-8.63597255793495));
#36136=CARTESIAN_POINT('Ctrl Pts',(-60.5303412626156,64.2870659352219,-8.67494477056538));
#36137=CARTESIAN_POINT('Ctrl Pts',(-59.8351144418708,64.2601577920231,-8.71391698319581));
#36138=CARTESIAN_POINT('Ctrl Pts',(-59.1398876211261,64.2332496488243,-8.75288919582624));
#36139=CARTESIAN_POINT('Ctrl Pts',(-58.4513847238254,64.0326152799095,-8.79186140845667));
#36140=CARTESIAN_POINT('Ctrl Pts',(-57.8505354268778,63.6818383038823,-8.8308336210871));
#36141=CARTESIAN_POINT('Ctrl Pts',(-57.2496861299302,63.3310613278551,-8.86980583371753));
#36142=CARTESIAN_POINT('Ctrl Pts',(-56.7364904333356,62.8301417447155,-8.90877804634796));
#36143=CARTESIAN_POINT('Ctrl Pts',(-56.3712717081713,62.2379595431017,-8.94775025897839));
#36144=CARTESIAN_POINT('Ctrl Pts',(-56.0060529830071,61.6457773414879,-8.98672247160882));
#36145=CARTESIAN_POINT('Ctrl Pts',(-55.7888112292733,60.9623325214,-9.02569468423925));
#36146=CARTESIAN_POINT('Ctrl Pts',(-55.7450818863031,60.2679609567506,-9.06466689686968));
#36147=CARTESIAN_POINT('Ctrl Pts',(-55.7394660372551,60.1787877466035,-9.0696718214428));
#36148=CARTESIAN_POINT('Ctrl Pts',(-55.7367118314557,60.0894343277631,-9.07467674601593));
#36149=CARTESIAN_POINT('Ctrl Pts',(-55.7367869586782,60.0000762880139,-9.07968167058905));
#36150=CARTESIAN_POINT('Ctrl Pts',(-58.677115034431,55.0755938055567,-10.));
#36151=CARTESIAN_POINT('Ctrl Pts',(-57.8732233401272,55.2915500435982,-9.96102778736957));
#36152=CARTESIAN_POINT('Ctrl Pts',(-56.3739727673179,56.1245137043432,-9.88308336210872));
#36153=CARTESIAN_POINT('Ctrl Pts',(-54.9770227854932,58.2859118105468,-9.76616672421742));
#36154=CARTESIAN_POINT('Ctrl Pts',(-54.7611834123237,60.8500627421559,-9.64925008632613));
#36155=CARTESIAN_POINT('Ctrl Pts',(-55.7768178011049,63.214507276628,-9.53233344843484));
#36156=CARTESIAN_POINT('Ctrl Pts',(-57.7853302019076,64.8232034014141,-9.41541681054356));
#36157=CARTESIAN_POINT('Ctrl Pts',(-60.3144620657417,65.2980444973094,-9.29850017265226));
#36158=CARTESIAN_POINT('Ctrl Pts',(-62.769679003779,64.5273620844534,-9.18158353476097));
#36159=CARTESIAN_POINT('Ctrl Pts',(-64.5737697114167,62.6923525936502,-9.06466689686969));
#36160=CARTESIAN_POINT('Ctrl Pts',(-65.3026202914353,60.2243982367199,-8.94775025897839));
#36161=CARTESIAN_POINT('Ctrl Pts',(-64.7848823971216,57.703691543606,-8.83083362108711));
#36162=CARTESIAN_POINT('Ctrl Pts',(-63.1422721706319,55.7228209792253,-8.71391698319582));
#36163=CARTESIAN_POINT('Ctrl Pts',(-60.7609482860978,54.7474681235472,-8.59700034530452));
#36164=CARTESIAN_POINT('Ctrl Pts',(-58.2007340318709,55.0069271910455,-8.48008370741324));
#36165=CARTESIAN_POINT('Ctrl Pts',(-56.0635071617532,56.4402025452955,-8.36316706952194));
#36166=CARTESIAN_POINT('Ctrl Pts',(-54.8517063490748,58.7103466297086,-8.24625043163066));
#36167=CARTESIAN_POINT('Ctrl Pts',(-54.8502120322186,61.2836744106993,-8.12933379373937));
#36168=CARTESIAN_POINT('Ctrl Pts',(-56.059376560482,63.5552235595967,-8.01241715584808));
#36169=CARTESIAN_POINT('Ctrl Pts',(-58.1949364984747,64.9909811437472,-7.89550051795679));
#36170=CARTESIAN_POINT('Ctrl Pts',(-60.7548501786328,65.2534097268154,-7.7785838800655));
#36171=CARTESIAN_POINT('Ctrl Pts',(-63.1372998197884,64.2808297669235,-7.66166724217421));
#36172=CARTESIAN_POINT('Ctrl Pts',(-64.7822203790914,62.3018527171852,-7.54475060428292));
#36173=CARTESIAN_POINT('Ctrl Pts',(-65.3028606950879,59.7817818006449,-7.42783396639163));
#36174=CARTESIAN_POINT('Ctrl Pts',(-64.5769288017872,57.3129117888108,-7.31091732850034));
#36175=CARTESIAN_POINT('Ctrl Pts',(-62.7748569607921,55.4759618947992,-7.19400069060905));
#36176=CARTESIAN_POINT('Ctrl Pts',(-60.3207807277454,54.7020982939809,-7.07708405271776));
#36177=CARTESIAN_POINT('Ctrl Pts',(-57.7905713642451,55.1747170180384,-6.96016741482648));
#36178=CARTESIAN_POINT('Ctrl Pts',(-55.7813283808542,56.7795403162521,-6.84325077693518));
#36179=CARTESIAN_POINT('Ctrl Pts',(-54.7604821556384,59.1461432117513,-6.72633413904389));
#36180=CARTESIAN_POINT('Ctrl Pts',(-54.9785949323137,61.7034054152601,-6.60941750115261));
#36181=CARTESIAN_POINT('Ctrl Pts',(-56.822670191795,64.6083226141335,-6.45352865063088));
#36182=CARTESIAN_POINT('Ctrl Pts',(-61.3338600370175,65.8440763141619,-6.25866758747874));
#36183=CARTESIAN_POINT('Ctrl Pts',(-65.6028014358132,62.1309684734756,-6.02483431169615));
#36184=CARTESIAN_POINT('Ctrl Pts',(-65.0042200345167,57.4920438855145,-5.82997324854401));
#36185=CARTESIAN_POINT('Ctrl Pts',(-62.3829259668669,55.2631484402659,-5.67408439802228));
#36186=CARTESIAN_POINT('Ctrl Pts',(-59.8805750705293,54.692707249224,-5.557167760131));
#36187=CARTESIAN_POINT('Ctrl Pts',(-57.3953251078463,55.3756925371435,-5.44025112223971));
#36188=CARTESIAN_POINT('Ctrl Pts',(-55.5275118929263,57.1431169284426,-5.32333448434842));
#36189=CARTESIAN_POINT('Ctrl Pts',(-54.7087705821979,59.5834018600784,-5.20641784645713));
#36190=CARTESIAN_POINT('Ctrl Pts',(-55.1350332706562,62.1210494224441,-5.08950120856584));
#36191=CARTESIAN_POINT('Ctrl Pts',(-56.7044890264666,64.1603278398107,-4.97258457067455));
#36192=CARTESIAN_POINT('Ctrl Pts',(-59.0489177119773,65.2214359342736,-4.85566793278326));
#36193=CARTESIAN_POINT('Ctrl Pts',(-61.6168265705004,65.0550993586167,-4.73875129489197));
#36194=CARTESIAN_POINT('Ctrl Pts',(-63.8046877780167,63.7003384396424,-4.62183465700068));
#36195=CARTESIAN_POINT('Ctrl Pts',(-65.0980856806054,61.4756811768837,-4.50491801910939));
#36196=CARTESIAN_POINT('Ctrl Pts',(-65.1929908975039,58.9041019334819,-4.3880013812181));
#36197=CARTESIAN_POINT('Ctrl Pts',(-64.067076438205,56.5901588181647,-4.27108474332681));
#36198=CARTESIAN_POINT('Ctrl Pts',(-61.9850396737251,55.0778303984365,-4.15416810543552));
#36199=CARTESIAN_POINT('Ctrl Pts',(-59.4363409530604,54.7226501051879,-4.03725146754423));
#36200=CARTESIAN_POINT('Ctrl Pts',(-57.0201528028271,55.6081161060463,-3.92033482965294));
#36201=CARTESIAN_POINT('Ctrl Pts',(-55.3044933499955,57.526065446996,-3.80341819176166));
#36202=CARTESIAN_POINT('Ctrl Pts',(-54.6926959629807,60.0256094770039,-3.68650155387036));
#36203=CARTESIAN_POINT('Ctrl Pts',(-55.3285862201775,62.5191327628181,-3.56958491597908));
#36204=CARTESIAN_POINT('Ctrl Pts',(-57.0626757179785,64.4204363923688,-3.45266827808779));
#36205=CARTESIAN_POINT('Ctrl Pts',(-59.487294255791,65.282543142849,-3.3357516401965));
#36206=CARTESIAN_POINT('Ctrl Pts',(-62.0324515210899,64.9027851981381,-3.21883500230521));
#36207=CARTESIAN_POINT('Ctrl Pts',(-64.0997862762435,63.3704311081236,-3.10191836441392));
#36208=CARTESIAN_POINT('Ctrl Pts',(-65.2033407181402,61.045739110996,-2.98500172652263));
#36209=CARTESIAN_POINT('Ctrl Pts',(-65.083574915278,58.4751813271234,-2.86808508863134));
#36210=CARTESIAN_POINT('Ctrl Pts',(-63.7688780194889,56.2631621799769,-2.75116845074005));
#36211=CARTESIAN_POINT('Ctrl Pts',(-61.5678300058233,54.9295585406499,-2.63425181284876));
#36212=CARTESIAN_POINT('Ctrl Pts',(-59.8553056997907,54.8355306649757,-2.5563073875879));
#36213=CARTESIAN_POINT('Ctrl Pts',(-59.0378648750817,54.9925957821044,-2.51733517495747));
#36214=CARTESIAN_POINT('Ctrl Pts',(-58.7494123365958,55.344718704462,-10.1608882750142));
#36215=CARTESIAN_POINT('Ctrl Pts',(-57.9894543192508,55.5488726665669,-10.1219160623837));
#36216=CARTESIAN_POINT('Ctrl Pts',(-56.5721396475246,56.3363138313726,-10.0439716371229));
#36217=CARTESIAN_POINT('Ctrl Pts',(-55.2515347127552,58.3795888535214,-9.92705499923159));
#36218=CARTESIAN_POINT('Ctrl Pts',(-55.0474912287124,60.8036057602351,-9.81013836134031));
#36219=CARTESIAN_POINT('Ctrl Pts',(-56.0076199399737,63.0388304718126,-9.69322172344902));
#36220=CARTESIAN_POINT('Ctrl Pts',(-57.9063646499174,64.5596093605183,-9.57630508555773));
#36221=CARTESIAN_POINT('Ctrl Pts',(-60.2972763242917,65.0084998022875,-9.45938844766644));
#36222=CARTESIAN_POINT('Ctrl Pts',(-62.6183126151303,64.2799361380192,-9.34247180977515));
#36223=CARTESIAN_POINT('Ctrl Pts',(-64.323807530679,62.5452121891074,-9.22555517188386));
#36224=CARTESIAN_POINT('Ctrl Pts',(-65.0128255235959,60.2121345950975,-9.10863853399257));
#36225=CARTESIAN_POINT('Ctrl Pts',(-64.5233826465826,57.8291876454264,-8.99172189610128));
#36226=CARTESIAN_POINT('Ctrl Pts',(-62.9705431038444,55.9565741113013,-8.87480525820999));
#36227=CARTESIAN_POINT('Ctrl Pts',(-60.719361519596,55.0345254974581,-8.7578886203187));
#36228=CARTESIAN_POINT('Ctrl Pts',(-58.2990661459689,55.2798048054984,-8.64097198242741));
#36229=CARTESIAN_POINT('Ctrl Pts',(-56.2786413719103,56.63474988609,-8.52405534453612));
#36230=CARTESIAN_POINT('Ctrl Pts',(-55.1330669748298,58.7808277840241,-8.40713870664484));
#36231=CARTESIAN_POINT('Ctrl Pts',(-55.1316543242409,61.2135200139323,-8.29022206875354));
#36232=CARTESIAN_POINT('Ctrl Pts',(-56.2747365131157,63.360926187836,-8.17330543086225));
#36233=CARTESIAN_POINT('Ctrl Pts',(-58.2935854549548,64.7182178413891,-8.05638879297096));
#36234=CARTESIAN_POINT('Ctrl Pts',(-60.7135966812584,64.9663043772948,-7.93947215507967));
#36235=CARTESIAN_POINT('Ctrl Pts',(-62.9658424981343,64.0468771170479,-7.82255551718839));
#36236=CARTESIAN_POINT('Ctrl Pts',(-64.5208661111355,62.1760536146444,-7.70563887929709));
#36237=CARTESIAN_POINT('Ctrl Pts',(-65.013052788891,59.7937076955695,-7.58872224140581));
#36238=CARTESIAN_POINT('Ctrl Pts',(-64.3267939728473,57.4597644883305,-7.47180560351452));
#36239=CARTESIAN_POINT('Ctrl Pts',(-62.6232075903782,55.7232061816494,-7.35488896562323));
#36240=CARTESIAN_POINT('Ctrl Pts',(-60.3032496635893,54.9916351852819,-7.23797232773194));
#36241=CARTESIAN_POINT('Ctrl Pts',(-57.9113193762403,55.4384247105873,-7.12105568984065));
#36242=CARTESIAN_POINT('Ctrl Pts',(-56.011884010952,56.9555424274904,-7.00413905194936));
#36243=CARTESIAN_POINT('Ctrl Pts',(-55.0468282965736,59.1928075429912,-6.88722241405807));
#36244=CARTESIAN_POINT('Ctrl Pts',(-55.2530209398044,61.610312199129,-6.77030577616678));
#36245=CARTESIAN_POINT('Ctrl Pts',(-56.9963152019055,64.356472074458,-6.61441692564506));
#36246=CARTESIAN_POINT('Ctrl Pts',(-61.260962933602,65.5246903039221,-6.41955586249292));
#36247=CARTESIAN_POINT('Ctrl Pts',(-65.2966013965676,62.0145084065457,-6.18572258671033));
#36248=CARTESIAN_POINT('Ctrl Pts',(-64.7307332103775,57.6291067940397,-5.99086152355819));
#36249=CARTESIAN_POINT('Ctrl Pts',(-62.252696110797,55.5220232460408,-5.83497267303646));
#36250=CARTESIAN_POINT('Ctrl Pts',(-59.8871017908691,54.9827573727547,-5.71805603514517));
#36251=CARTESIAN_POINT('Ctrl Pts',(-57.5376738173867,55.6284166686038,-5.60113939725388));
#36252=CARTESIAN_POINT('Ctrl Pts',(-55.7719389085185,57.2992491274242,-5.48422275936259));
#36253=CARTESIAN_POINT('Ctrl Pts',(-54.9979428246821,59.606169464509,-5.36730612147131));
#36254=CARTESIAN_POINT('Ctrl Pts',(-55.40090972916,62.0051314439409,-5.25038948358002));
#36255=CARTESIAN_POINT('Ctrl Pts',(-56.8845927836657,63.9329607695301,-5.13347284568873));
#36256=CARTESIAN_POINT('Ctrl Pts',(-59.1008955372232,64.9360779921247,-5.01655620779744));
#36257=CARTESIAN_POINT('Ctrl Pts',(-61.5284649954897,64.7788319163859,-4.89963956990615));
#36258=CARTESIAN_POINT('Ctrl Pts',(-63.5967568776818,63.4981103599182,-4.78272293201486));
#36259=CARTESIAN_POINT('Ctrl Pts',(-64.8194689826264,61.3950333724858,-4.66580629412357));
#36260=CARTESIAN_POINT('Ctrl Pts',(-64.9091875118522,58.9639941204211,-4.54888965623228));
#36261=CARTESIAN_POINT('Ctrl Pts',(-63.8448056725426,56.7765108628803,-4.43197301834099));
#36262=CARTESIAN_POINT('Ctrl Pts',(-61.8765547964789,55.3468330647702,-4.3150563804497));
#36263=CARTESIAN_POINT('Ctrl Pts',(-59.4671456182393,55.0110638145468,-4.19813974255841));
#36264=CARTESIAN_POINT('Ctrl Pts',(-57.1830051436022,55.8481380015386,-4.08122310466712));
#36265=CARTESIAN_POINT('Ctrl Pts',(-55.5611086052354,57.6612690350401,-3.96430646677583));
#36266=CARTESIAN_POINT('Ctrl Pts',(-54.9827467033185,60.0242098873605,-3.84738982888454));
#36267=CARTESIAN_POINT('Ctrl Pts',(-55.5838847702156,62.3814590366158,-3.73047319099325));
#36268=CARTESIAN_POINT('Ctrl Pts',(-57.2232041287629,64.1788540674672,-3.61355655310196));
#36269=CARTESIAN_POINT('Ctrl Pts',(-59.5153142598545,64.9938456160515,-3.49663991521067));
#36270=CARTESIAN_POINT('Ctrl Pts',(-61.9213755276512,64.634841913465,-3.37972327731938));
#36271=CARTESIAN_POINT('Ctrl Pts',(-63.8757278774111,63.1862328727577,-3.26280663942809));
#36272=CARTESIAN_POINT('Ctrl Pts',(-64.9189717019694,60.9885881731132,-3.1458900015368));
#36273=CARTESIAN_POINT('Ctrl Pts',(-64.8057512486,58.5585145565491,-3.02897336364551));
#36274=CARTESIAN_POINT('Ctrl Pts',(-63.5629041668189,56.4673849960545,-2.91205672575423));
#36275=CARTESIAN_POINT('Ctrl Pts',(-61.4821461537694,55.2066644476915,-2.79514008786293));
#36276=CARTESIAN_POINT('Ctrl Pts',(-59.8632134225452,55.1177753119051,-2.71719566260207));
#36277=CARTESIAN_POINT('Ctrl Pts',(-59.0904467515563,55.2662566258098,-2.67822344997165));
#36278=CARTESIAN_POINT('Ctrl Pts',(-58.8217096387607,55.6138436033673,-10.3217765500284));
#36279=CARTESIAN_POINT('Ctrl Pts',(-58.1056852983744,55.8061952895356,-10.2828043373979));
#36280=CARTESIAN_POINT('Ctrl Pts',(-56.7703065277313,56.548113958402,-10.2048599121371));
#36281=CARTESIAN_POINT('Ctrl Pts',(-55.5260466400173,58.473265896496,-10.0879432742458));
#36282=CARTESIAN_POINT('Ctrl Pts',(-55.333799045101,60.7571487783143,-9.97102663635449));
#36283=CARTESIAN_POINT('Ctrl Pts',(-56.2384220788426,62.8631536669972,-9.85410999846319));
#36284=CARTESIAN_POINT('Ctrl Pts',(-58.0273990979271,64.2960153196226,-9.73719336057191));
#36285=CARTESIAN_POINT('Ctrl Pts',(-60.2800905828417,64.7189551072656,-9.62027672268061));
#36286=CARTESIAN_POINT('Ctrl Pts',(-62.4669462264816,64.0325101915851,-9.50336008478932));
#36287=CARTESIAN_POINT('Ctrl Pts',(-64.0738453499413,62.3980717845645,-9.38644344689804));
#36288=CARTESIAN_POINT('Ctrl Pts',(-64.7230307557564,60.1998709534751,-9.26952680900674));
#36289=CARTESIAN_POINT('Ctrl Pts',(-64.2618828960438,57.9546837472467,-9.15261017111546));
#36290=CARTESIAN_POINT('Ctrl Pts',(-62.7988140370569,56.1903272433774,-9.03569353322417));
#36291=CARTESIAN_POINT('Ctrl Pts',(-60.6777747530942,55.321582871369,-8.91877689533288));
#36292=CARTESIAN_POINT('Ctrl Pts',(-58.3973982600668,55.5526824199513,-8.80186025744159));
#36293=CARTESIAN_POINT('Ctrl Pts',(-56.4937755820675,56.8292972268845,-8.6849436195503));
#36294=CARTESIAN_POINT('Ctrl Pts',(-55.4144276005848,58.8513089383396,-8.56802698165902));
#36295=CARTESIAN_POINT('Ctrl Pts',(-55.4130966162632,61.1433656171654,-8.45111034376772));
#36296=CARTESIAN_POINT('Ctrl Pts',(-56.4900964657494,63.1666288160754,-8.33419370587643));
#36297=CARTESIAN_POINT('Ctrl Pts',(-58.3922344114348,64.4454545390309,-8.21727706798514));
#36298=CARTESIAN_POINT('Ctrl Pts',(-60.6723431838839,64.6791990277741,-8.10036043009385));
#36299=CARTESIAN_POINT('Ctrl Pts',(-62.7943851764801,63.8129244671722,-7.98344379220257));
#36300=CARTESIAN_POINT('Ctrl Pts',(-64.2595118431797,62.0502545121036,-7.86652715431127));
#36301=CARTESIAN_POINT('Ctrl Pts',(-64.7232448826942,59.805633590494,-7.74961051641999));
#36302=CARTESIAN_POINT('Ctrl Pts',(-64.0766591439074,57.6066171878503,-7.63269387852869));
#36303=CARTESIAN_POINT('Ctrl Pts',(-62.4715582199642,55.9704504684996,-7.5157772406374));
#36304=CARTESIAN_POINT('Ctrl Pts',(-60.2857185994333,55.2811720765829,-7.39886060274612));
#36305=CARTESIAN_POINT('Ctrl Pts',(-58.0320673882356,55.7021324031362,-7.28194396485482));
#36306=CARTESIAN_POINT('Ctrl Pts',(-56.2424396410498,57.1315445387288,-7.16502732696353));
#36307=CARTESIAN_POINT('Ctrl Pts',(-55.3331744375089,59.239471874231,-7.04811068907225));
#36308=CARTESIAN_POINT('Ctrl Pts',(-55.5274469472951,61.5172189829979,-6.93119405118096));
#36309=CARTESIAN_POINT('Ctrl Pts',(-57.1699602120159,64.1046215347825,-6.77530520065924));
#36310=CARTESIAN_POINT('Ctrl Pts',(-61.1880658301865,65.2053042936822,-6.58044413750709));
#36311=CARTESIAN_POINT('Ctrl Pts',(-64.9904013573221,61.8980483396159,-6.34661086172452));
#36312=CARTESIAN_POINT('Ctrl Pts',(-64.4572463862384,57.7661697025649,-6.15174979857236));
#36313=CARTESIAN_POINT('Ctrl Pts',(-62.1224662547272,55.7808980518156,-5.99586094805064));
#36314=CARTESIAN_POINT('Ctrl Pts',(-59.8936285112088,55.2728074962854,-5.87894431015935));
#36315=CARTESIAN_POINT('Ctrl Pts',(-57.6800225269272,55.8811408000641,-5.76202767226806));
#36316=CARTESIAN_POINT('Ctrl Pts',(-56.0163659241107,57.4553813264059,-5.64511103437677));
#36317=CARTESIAN_POINT('Ctrl Pts',(-55.2871150671665,59.6289370689395,-5.52819439648548));
#36318=CARTESIAN_POINT('Ctrl Pts',(-55.6667861876637,61.8892134654378,-5.41127775859419));
#36319=CARTESIAN_POINT('Ctrl Pts',(-57.0646965408647,63.7055936992496,-5.2943611207029));
#36320=CARTESIAN_POINT('Ctrl Pts',(-59.1528733624691,64.6507200499757,-5.17744448281161));
#36321=CARTESIAN_POINT('Ctrl Pts',(-61.440103420479,64.5025644741552,-5.06052784492032));
#36322=CARTESIAN_POINT('Ctrl Pts',(-63.388825977347,63.295882280194,-4.94361120702904));
#36323=CARTESIAN_POINT('Ctrl Pts',(-64.5408522846473,61.3143855680879,-4.82669456913774));
#36324=CARTESIAN_POINT('Ctrl Pts',(-64.6253841262005,59.0238863073603,-4.70977793124646));
#36325=CARTESIAN_POINT('Ctrl Pts',(-63.6225349068801,56.9628629075959,-4.59286129335516));
#36326=CARTESIAN_POINT('Ctrl Pts',(-61.7680699192328,55.615835731104,-4.47594465546388));
#36327=CARTESIAN_POINT('Ctrl Pts',(-59.4979502834182,55.2994775239056,-4.35902801757258));
#36328=CARTESIAN_POINT('Ctrl Pts',(-57.3458574843773,56.0881598970308,-4.2421113796813));
#36329=CARTESIAN_POINT('Ctrl Pts',(-55.8177238604752,57.7964726230843,-4.12519474179001));
#36330=CARTESIAN_POINT('Ctrl Pts',(-55.2727974436564,60.0228102977171,-4.00827810389872));
#36331=CARTESIAN_POINT('Ctrl Pts',(-55.8391833202536,62.2437853104136,-3.89136146600743));
#36332=CARTESIAN_POINT('Ctrl Pts',(-57.3837325395474,63.9372717425656,-3.77444482811614));
#36333=CARTESIAN_POINT('Ctrl Pts',(-59.543334263918,64.7051480892539,-3.65752819022485));
#36334=CARTESIAN_POINT('Ctrl Pts',(-61.8102995342126,64.366898628792,-3.54061155233356));
#36335=CARTESIAN_POINT('Ctrl Pts',(-63.6516694785787,63.0020346373919,-3.42369491444227));
#36336=CARTESIAN_POINT('Ctrl Pts',(-64.6346026857985,60.9314372352304,-3.30677827655098));
#36337=CARTESIAN_POINT('Ctrl Pts',(-64.5279275819221,58.6418477859748,-3.18986163865969));
#36338=CARTESIAN_POINT('Ctrl Pts',(-63.3569303141489,56.6716078121321,-3.0729450007684));
#36339=CARTESIAN_POINT('Ctrl Pts',(-61.3964623017155,55.4837703547332,-2.95602836287711));
#36340=CARTESIAN_POINT('Ctrl Pts',(-59.8711211452996,55.4000199588346,-2.87808393761625));
#36341=CARTESIAN_POINT('Ctrl Pts',(-59.1430286280309,55.5399174695151,-2.83911172498582));
#36342=CARTESIAN_POINT('Ctrl Pts',(-58.8940069409255,55.8829685022727,-10.4826648250425));
#36343=CARTESIAN_POINT('Ctrl Pts',(-58.221916277498,56.0635179125043,-10.4436926124121));
#36344=CARTESIAN_POINT('Ctrl Pts',(-56.9684734079381,56.7599140854314,-10.3657481871512));
#36345=CARTESIAN_POINT('Ctrl Pts',(-55.8005585672793,58.5669429394706,-10.2488315492599));
#36346=CARTESIAN_POINT('Ctrl Pts',(-55.6201068614897,60.7106917963935,-10.1319149113687));
#36347=CARTESIAN_POINT('Ctrl Pts',(-56.4692242177114,62.6874768621819,-10.0149982734774));
#36348=CARTESIAN_POINT('Ctrl Pts',(-58.1484335459369,64.0324212787269,-9.89808163558609));
#36349=CARTESIAN_POINT('Ctrl Pts',(-60.2629048413918,64.4294104122436,-9.78116499769479));
#36350=CARTESIAN_POINT('Ctrl Pts',(-62.3155798378329,63.785084245151,-9.6642483598035));
#36351=CARTESIAN_POINT('Ctrl Pts',(-63.8238831692036,62.2509313800217,-9.54733172191221));
#36352=CARTESIAN_POINT('Ctrl Pts',(-64.433235987917,60.1876073118527,-9.43041508402092));
#36353=CARTESIAN_POINT('Ctrl Pts',(-64.0003831455049,58.080179849067,-9.31349844612964));
#36354=CARTESIAN_POINT('Ctrl Pts',(-62.6270849702694,56.4240803754535,-9.19658180823835));
#36355=CARTESIAN_POINT('Ctrl Pts',(-60.6361879865924,55.6086402452798,-9.07966517034705));
#36356=CARTESIAN_POINT('Ctrl Pts',(-58.4957303741647,55.8255600344042,-8.96274853245577));
#36357=CARTESIAN_POINT('Ctrl Pts',(-56.7089097922247,57.0238445676789,-8.84583189456447));
#36358=CARTESIAN_POINT('Ctrl Pts',(-55.6957882263397,58.921790092655,-8.72891525667319));
#36359=CARTESIAN_POINT('Ctrl Pts',(-55.6945389082855,61.0732112203983,-8.6119986187819));
#36360=CARTESIAN_POINT('Ctrl Pts',(-56.705456418383,62.9723314443147,-8.49508198089061));
#36361=CARTESIAN_POINT('Ctrl Pts',(-58.4908833679148,64.1726912366728,-8.37816534299932));
#36362=CARTESIAN_POINT('Ctrl Pts',(-60.6310896865095,64.3920936782534,-8.26124870510802));
#36363=CARTESIAN_POINT('Ctrl Pts',(-62.622927854826,63.5789718172965,-8.14433206721674));
#36364=CARTESIAN_POINT('Ctrl Pts',(-63.9981575752239,61.9244554095628,-8.02741542932544));
#36365=CARTESIAN_POINT('Ctrl Pts',(-64.4334369764973,59.8175594854186,-7.91049879143416));
#36366=CARTESIAN_POINT('Ctrl Pts',(-63.8265243149675,57.7534698873702,-7.79358215354287));
#36367=CARTESIAN_POINT('Ctrl Pts',(-62.3199088495502,56.2176947553498,-7.67666551565158));
#36368=CARTESIAN_POINT('Ctrl Pts',(-60.2681875352772,55.570708967884,-7.55974887776029));
#36369=CARTESIAN_POINT('Ctrl Pts',(-58.1528154002308,55.965840095685,-7.442832239869));
#36370=CARTESIAN_POINT('Ctrl Pts',(-56.4729952711476,57.3075466499671,-7.32591560197771));
#36371=CARTESIAN_POINT('Ctrl Pts',(-55.6195205784441,59.2861362054709,-7.20899896408642));
#36372=CARTESIAN_POINT('Ctrl Pts',(-55.8018729547859,61.4241257668668,-7.09208232619513));
#36373=CARTESIAN_POINT('Ctrl Pts',(-57.3436052221264,63.8527709951071,-6.93619347567341));
#36374=CARTESIAN_POINT('Ctrl Pts',(-61.115168726771,64.8859182834423,-6.74133241252127));
#36375=CARTESIAN_POINT('Ctrl Pts',(-64.6842013180765,61.7815882726861,-6.50749913673869));
#36376=CARTESIAN_POINT('Ctrl Pts',(-64.1837595620993,57.9032326110901,-6.31263807358654));
#36377=CARTESIAN_POINT('Ctrl Pts',(-61.9922363986573,56.0397728575904,-6.15674922306481));
#36378=CARTESIAN_POINT('Ctrl Pts',(-59.9001552315486,55.562857619816,-6.03983258517353));
#36379=CARTESIAN_POINT('Ctrl Pts',(-57.8223712364677,56.1338649315244,-5.92291594728224));
#36380=CARTESIAN_POINT('Ctrl Pts',(-56.2607929397029,57.6115135253875,-5.80599930939094));
#36381=CARTESIAN_POINT('Ctrl Pts',(-55.5762873096508,59.6517046733701,-5.68908267149966));
#36382=CARTESIAN_POINT('Ctrl Pts',(-55.9326626461674,61.7732954869346,-5.57216603360837));
#36383=CARTESIAN_POINT('Ctrl Pts',(-57.2448002980638,63.4782266289691,-5.45524939571708));
#36384=CARTESIAN_POINT('Ctrl Pts',(-59.2048511877151,64.3653621078267,-5.33833275782579));
#36385=CARTESIAN_POINT('Ctrl Pts',(-61.3517418454684,64.2262970319245,-5.2214161199345));
#36386=CARTESIAN_POINT('Ctrl Pts',(-63.1808950770122,63.0936542004698,-5.10449948204321));
#36387=CARTESIAN_POINT('Ctrl Pts',(-64.2622355866681,61.23373776369,-4.98758284415192));
#36388=CARTESIAN_POINT('Ctrl Pts',(-64.341580740549,59.0837784942996,-4.87066620626063));
#36389=CARTESIAN_POINT('Ctrl Pts',(-63.4002641412175,57.1492149523114,-4.75374956836934));
#36390=CARTESIAN_POINT('Ctrl Pts',(-61.6595850419867,55.8848383974377,-4.63683293047805));
#36391=CARTESIAN_POINT('Ctrl Pts',(-59.5287549485971,55.5878912332645,-4.51991629258676));
#36392=CARTESIAN_POINT('Ctrl Pts',(-57.5087098251523,56.3281817925231,-4.40299965469547));
#36393=CARTESIAN_POINT('Ctrl Pts',(-56.074339115715,57.9316762111284,-4.28608301680419));
#36394=CARTESIAN_POINT('Ctrl Pts',(-55.5628481839942,60.0214107080737,-4.16916637891289));
#36395=CARTESIAN_POINT('Ctrl Pts',(-56.0944818702916,62.1061115842113,-4.05224974102161));
#36396=CARTESIAN_POINT('Ctrl Pts',(-57.5442609503319,63.6956894176639,-3.93533310313031));
#36397=CARTESIAN_POINT('Ctrl Pts',(-59.5713542679814,64.4164505624564,-3.81841646523903));
#36398=CARTESIAN_POINT('Ctrl Pts',(-61.6992235407739,64.0989553441189,-3.70149982734774));
#36399=CARTESIAN_POINT('Ctrl Pts',(-63.4276110797463,62.817836402026,-3.58458318945645));
#36400=CARTESIAN_POINT('Ctrl Pts',(-64.3502336696277,60.8742862973476,-3.46766655156516));
#36401=CARTESIAN_POINT('Ctrl Pts',(-64.2501039152442,58.7251810154005,-3.35074991367387));
#36402=CARTESIAN_POINT('Ctrl Pts',(-63.150956461479,56.8758306282097,-3.23383327578258));
#36403=CARTESIAN_POINT('Ctrl Pts',(-61.3107784496616,55.7608762617749,-3.11691663789129));
#36404=CARTESIAN_POINT('Ctrl Pts',(-59.8790288680541,55.6822646057641,-3.03897221263043));
#36405=CARTESIAN_POINT('Ctrl Pts',(-59.1956105045055,55.8135783132205,-3.));
#36406=CARTESIAN_POINT('Ctrl Pts',(-55.7373303217998,60.0000007547395,-8.67031832941094));
#36407=CARTESIAN_POINT('Ctrl Pts',(-55.7373282077215,60.3472087804744,-8.65087842586793));
#36408=CARTESIAN_POINT('Ctrl Pts',(-55.7792938624899,60.6944162976158,-8.63143852232491));
#36409=CARTESIAN_POINT('Ctrl Pts',(-55.8632333796441,61.0311610697605,-8.6119986187819));
#36410=CARTESIAN_POINT('Ctrl Pts',(-56.0315114116513,61.7062512950371,-8.57302640615147));
#36411=CARTESIAN_POINT('Ctrl Pts',(-56.3684839150172,62.3392913696759,-8.53405419352104));
#36412=CARTESIAN_POINT('Ctrl Pts',(-56.8345413249554,62.8558713723883,-8.49508198089061));
#36413=CARTESIAN_POINT('Ctrl Pts',(-57.3005987348936,63.3724513751007,-8.45610976826018));
#36414=CARTESIAN_POINT('Ctrl Pts',(-57.8957410514042,63.7725713058868,-8.41713755562975));
#36415=CARTESIAN_POINT('Ctrl Pts',(-58.5500132627586,64.0091983448765,-8.37816534299932));
#36416=CARTESIAN_POINT('Ctrl Pts',(-59.204285474113,64.2458253838663,-8.33919313036889));
#36417=CARTESIAN_POINT('Ctrl Pts',(-59.9176875803113,64.3189595310599,-8.30022091773846));
#36418=CARTESIAN_POINT('Ctrl Pts',(-60.6063616614631,64.2200062944972,-8.26124870510803));
#36419=CARTESIAN_POINT('Ctrl Pts',(-61.295035742615,64.1210530579345,-8.2222764924776));
#36420=CARTESIAN_POINT('Ctrl Pts',(-61.9589817987205,63.8500124376155,-8.18330427984717));
#36421=CARTESIAN_POINT('Ctrl Pts',(-62.5201597801729,63.4387393928337,-8.14433206721674));
#36422=CARTESIAN_POINT('Ctrl Pts',(-63.0813377616253,63.027466348052,-8.10535985458631));
#36423=CARTESIAN_POINT('Ctrl Pts',(-63.5397476684246,62.4759608788074,-8.06638764195588));
#36424=CARTESIAN_POINT('Ctrl Pts',(-63.8414991887032,61.8490588234943,-8.02741542932545));
#36425=CARTESIAN_POINT('Ctrl Pts',(-64.1432507089817,61.2221567681814,-7.98844321669502));
#36426=CARTESIAN_POINT('Ctrl Pts',(-64.2883438427395,60.5198581268,-7.94947100406459));
#36427=CARTESIAN_POINT('Ctrl Pts',(-64.2597382993634,59.8246938731012,-7.91049879143416));
#36428=CARTESIAN_POINT('Ctrl Pts',(-64.2311327559874,59.1295296194024,-7.87152657880373));
#36429=CARTESIAN_POINT('Ctrl Pts',(-64.0288285354774,58.4414997533863,-7.8325543661733));
#36430=CARTESIAN_POINT('Ctrl Pts',(-63.6765738476529,57.8415222983748,-7.79358215354287));
#36431=CARTESIAN_POINT('Ctrl Pts',(-63.3243191598284,57.2415448433634,-7.75460994091244));
#36432=CARTESIAN_POINT('Ctrl Pts',(-62.8221140046893,56.7296197993566,-7.71563772828201));
#36433=CARTESIAN_POINT('Ctrl Pts',(-62.229057874741,56.3658263127756,-7.67666551565158));
#36434=CARTESIAN_POINT('Ctrl Pts',(-61.6360017447926,56.0020328261945,-7.63769330302115));
#36435=CARTESIAN_POINT('Ctrl Pts',(-60.9520946400349,55.7863708970392,-7.59872109039072));
#36436=CARTESIAN_POINT('Ctrl Pts',(-60.2575790651483,55.7443951204284,-7.55974887776029));
#36437=CARTESIAN_POINT('Ctrl Pts',(-59.5630634902618,55.7024193438176,-7.52077666512986));
#36438=CARTESIAN_POINT('Ctrl Pts',(-58.8579394452463,55.8341297197513,-7.48180445249943));
#36439=CARTESIAN_POINT('Ctrl Pts',(-58.2254074012247,56.1236026667652,-7.442832239869));
#36440=CARTESIAN_POINT('Ctrl Pts',(-57.5928753572031,56.4130756137791,-7.40386002723857));
#36441=CARTESIAN_POINT('Ctrl Pts',(-57.0329353141753,56.8603111318731,-7.36488781460814));
#36442=CARTESIAN_POINT('Ctrl Pts',(-56.6107195105442,57.4136938168374,-7.32591560197771));
#36443=CARTESIAN_POINT('Ctrl Pts',(-56.1885037069131,57.9670765018017,-7.28694338934728));
#36444=CARTESIAN_POINT('Ctrl Pts',(-55.9040121426786,58.6266063536363,-7.24797117671685));
#36445=CARTESIAN_POINT('Ctrl Pts',(-55.792158423285,59.3127028731196,-7.20899896408642));
#36446=CARTESIAN_POINT('Ctrl Pts',(-55.7551528017157,59.5396906594681,-7.1961054191946));
#36447=CARTESIAN_POINT('Ctrl Pts',(-55.7370432093912,59.7695862933357,-7.18321187430277));
#36448=CARTESIAN_POINT('Ctrl Pts',(-55.7374561790016,59.9995175300878,-7.17031832941094));
#36449=CARTESIAN_POINT('Ctrl Pts',(-58.677115034431,55.0755938055567,-10.));
#36450=CARTESIAN_POINT('Ctrl Pts',(-58.5386376224601,55.1251023467987,-10.));
#36451=CARTESIAN_POINT('Ctrl Pts',(-58.4026668815791,55.1806178076285,-10.));
#36452=CARTESIAN_POINT('Ctrl Pts',(-58.2695272544167,55.2418650197503,-10.));
#36453=CARTESIAN_POINT('Ctrl Pts',(-58.135336471899,55.3035957868918,-10.));
#36454=CARTESIAN_POINT('Ctrl Pts',(-58.0040210293143,55.371149627725,-10.));
#36455=CARTESIAN_POINT('Ctrl Pts',(-57.8759387502434,55.4442909167463,-10.));
#36456=CARTESIAN_POINT('Ctrl Pts',(-57.7488534505964,55.5168628814183,-10.));
#36457=CARTESIAN_POINT('Ctrl Pts',(-57.6249506202847,55.5949361888115,-10.));
#36458=CARTESIAN_POINT('Ctrl Pts',(-57.5046138796569,55.6783182407818,-10.));
#36459=CARTESIAN_POINT('Ctrl Pts',(-57.3858527971248,55.7606085097726,-10.));
#36460=CARTESIAN_POINT('Ctrl Pts',(-57.2705645546623,55.8480699257949,-10.));
#36461=CARTESIAN_POINT('Ctrl Pts',(-57.1591587964671,55.9405462498422,-10.));
#36462=CARTESIAN_POINT('Ctrl Pts',(-57.1274511406442,55.9668663207448,-10.));
#36463=CARTESIAN_POINT('Ctrl Pts',(-57.0960582671108,55.9935927805097,-10.));
#36464=CARTESIAN_POINT('Ctrl Pts',(-57.0649903190273,56.020722374975,-10.));
#36465=CARTESIAN_POINT('Ctrl Pts',(-57.0492520137067,56.0344656012663,-10.));
#36466=CARTESIAN_POINT('Ctrl Pts',(-57.0335970960159,56.048312282282,-10.));
#36467=CARTESIAN_POINT('Ctrl Pts',(-57.018026917309,56.0622620081661,-10.));
#36468=CARTESIAN_POINT('Ctrl Pts',(-57.0026738875857,56.0760171846584,-10.));
#36469=CARTESIAN_POINT('Ctrl Pts',(-56.9874092917288,56.0898671766707,-10.));
#36470=CARTESIAN_POINT('Ctrl Pts',(-56.9722391118383,56.1038067825593,-10.));
#36471=CARTESIAN_POINT('Ctrl Pts',(-56.8611663613498,56.2058695384362,-10.));
#36472=CARTESIAN_POINT('Ctrl Pts',(-56.7550660406813,56.3128091758504,-10.));
#36473=CARTESIAN_POINT('Ctrl Pts',(-56.6543282067119,56.4243834820602,-10.));
#36474=CARTESIAN_POINT('Ctrl Pts',(-56.5578656854931,56.5312225757368,-10.));
#36475=CARTESIAN_POINT('Ctrl Pts',(-56.4663200079077,56.6423122346398,-10.));
#36476=CARTESIAN_POINT('Ctrl Pts',(-56.3798948625733,56.757269687502,-10.));
#36477=CARTESIAN_POINT('Ctrl Pts',(-56.2936201130584,56.8720270930254,-10.));
#36478=CARTESIAN_POINT('Ctrl Pts',(-56.2124477882373,56.9906396027887,-10.));
#36479=CARTESIAN_POINT('Ctrl Pts',(-56.1366282844148,57.1127461598228,-10.));
#36480=CARTESIAN_POINT('Ctrl Pts',(-56.0709511389806,57.2185185495178,-10.));
#36481=CARTESIAN_POINT('Ctrl Pts',(-56.0092911309896,57.3269133050067,-10.));
#36482=CARTESIAN_POINT('Ctrl Pts',(-55.9518427208356,57.4377011839666,-10.));
#36483=CARTESIAN_POINT('Ctrl Pts',(-55.9367455036519,57.4668158046411,-10.));
#36484=CARTESIAN_POINT('Ctrl Pts',(-55.9219393122137,57.4960957081207,-10.));
#36485=CARTESIAN_POINT('Ctrl Pts',(-55.9074280351729,57.525536740701,-10.));
#36486=CARTESIAN_POINT('Ctrl Pts',(-55.8951622011407,57.5504221328239,-10.));
#36487=CARTESIAN_POINT('Ctrl Pts',(-55.8831044077694,57.5754285256612,-10.));
#36488=CARTESIAN_POINT('Ctrl Pts',(-55.8712719981158,57.6005211318673,-10.));
#36489=CARTESIAN_POINT('Ctrl Pts',(-55.8112491801806,57.727809569127,-10.));
#36490=CARTESIAN_POINT('Ctrl Pts',(-55.7569584161731,57.8574378456489,-10.));
#36491=CARTESIAN_POINT('Ctrl Pts',(-55.708587679128,57.9890469247172,-10.));
#36492=CARTESIAN_POINT('Ctrl Pts',(-55.660604700135,58.1196009758233,-10.));
#36493=CARTESIAN_POINT('Ctrl Pts',(-55.6184470131256,58.2521049312923,-10.));
#36494=CARTESIAN_POINT('Ctrl Pts',(-55.5823476675558,58.3862204353038,-10.));
#36495=CARTESIAN_POINT('Ctrl Pts',(-55.5736126976742,58.4186724055459,-10.));
#36496=CARTESIAN_POINT('Ctrl Pts',(-55.5652326786128,58.451218759105,-10.));
#36497=CARTESIAN_POINT('Ctrl Pts',(-55.5572113733907,58.4838547369515,-10.));
#36498=CARTESIAN_POINT('Ctrl Pts',(-55.5237968418714,58.6198071636733,-10.));
#36499=CARTESIAN_POINT('Ctrl Pts',(-55.4966031500819,58.7573154760479,-10.));
#36500=CARTESIAN_POINT('Ctrl Pts',(-55.4756766726658,58.8959462545501,-10.));
#36501=CARTESIAN_POINT('Ctrl Pts',(-55.4642433082102,58.9716883961376,-10.));
#36502=CARTESIAN_POINT('Ctrl Pts',(-55.4546816532845,59.0477654877749,-10.));
#36503=CARTESIAN_POINT('Ctrl Pts',(-55.4470056777547,59.124105191105,-10.));
#36504=CARTESIAN_POINT('Ctrl Pts',(-55.4421350689108,59.1725447454963,-10.));
#36505=CARTESIAN_POINT('Ctrl Pts',(-55.4380237695898,59.2210900052751,-10.));
#36506=CARTESIAN_POINT('Ctrl Pts',(-55.4346762817703,59.269722103547,-10.));
#36507=CARTESIAN_POINT('Ctrl Pts',(-55.4333863538523,59.2884620974328,-10.));
#36508=CARTESIAN_POINT('Ctrl Pts',(-55.4322097104365,59.3072175092192,-10.));
#36509=CARTESIAN_POINT('Ctrl Pts',(-55.4311470975273,59.3259789773854,-10.));
#36510=CARTESIAN_POINT('Ctrl Pts',(-55.4233879220381,59.4629747946461,-10.));
#36511=CARTESIAN_POINT('Ctrl Pts',(-55.4217193407444,59.5999983377396,-10.));
#36512=CARTESIAN_POINT('Ctrl Pts',(-55.4261204589518,59.7366439247398,-10.));
#36513=CARTESIAN_POINT('Ctrl Pts',(-55.4305091604386,59.8729039983356,-10.));
#36514=CARTESIAN_POINT('Ctrl Pts',(-55.4409334940953,60.008789039846,-10.));
#36515=CARTESIAN_POINT('Ctrl Pts',(-55.4574237999011,60.1438893245482,-10.));
#36516=CARTESIAN_POINT('Ctrl Pts',(-55.4736437641814,60.2767747796722,-10.));
#36517=CARTESIAN_POINT('Ctrl Pts',(-55.4957326625335,60.4089016790912,-10.));
#36518=CARTESIAN_POINT('Ctrl Pts',(-55.5237660357119,60.5398620252877,-10.));
#36519=CARTESIAN_POINT('Ctrl Pts',(-55.5366368863635,60.599989325932,-10.));
#36520=CARTESIAN_POINT('Ctrl Pts',(-55.5507614458456,60.6598704056294,-10.));
#36521=CARTESIAN_POINT('Ctrl Pts',(-55.5661502149289,60.7194638770806,-10.));
#36522=CARTESIAN_POINT('Ctrl Pts',(-55.5886111804506,60.8064446421006,-10.));
#36523=CARTESIAN_POINT('Ctrl Pts',(-55.6137651104405,60.8928130396799,-10.));
#36524=CARTESIAN_POINT('Ctrl Pts',(-55.6415741874814,60.9784471096742,-10.));
#36525=CARTESIAN_POINT('Ctrl Pts',(-55.6489435502234,61.0011400068149,-10.));
#36526=CARTESIAN_POINT('Ctrl Pts',(-55.6564994059424,61.023781297052,-10.));
#36527=CARTESIAN_POINT('Ctrl Pts',(-55.6642411296903,61.0463686223145,-10.));
#36528=CARTESIAN_POINT('Ctrl Pts',(-55.6712493359898,61.0668158302424,-10.));
#36529=CARTESIAN_POINT('Ctrl Pts',(-55.6784073088638,61.0872112882693,-10.));
#36530=CARTESIAN_POINT('Ctrl Pts',(-55.6857121883891,61.1075477764851,-10.));
#36531=CARTESIAN_POINT('Ctrl Pts',(-55.7311295763656,61.233987941882,-10.));
#36532=CARTESIAN_POINT('Ctrl Pts',(-55.7822461186853,61.3582207273371,-10.));
#36533=CARTESIAN_POINT('Ctrl Pts',(-55.8388703422329,61.4798690368619,-10.));
#36534=CARTESIAN_POINT('Ctrl Pts',(-55.8863606130665,61.5818944741014,-10.));
#36535=CARTESIAN_POINT('Ctrl Pts',(-55.9377259705942,61.6821017750024,-10.));
#36536=CARTESIAN_POINT('Ctrl Pts',(-55.9928752884837,61.7802503783273,-10.));
#36537=CARTESIAN_POINT('Ctrl Pts',(-56.0250178986502,61.8374542099573,-10.));
#36538=CARTESIAN_POINT('Ctrl Pts',(-56.058446233574,61.8939583886922,-10.));
#36539=CARTESIAN_POINT('Ctrl Pts',(-56.0931449406476,61.9497120817676,-10.));
#36540=CARTESIAN_POINT('Ctrl Pts',(-56.1050647419445,61.9688647534108,-10.));
#36541=CARTESIAN_POINT('Ctrl Pts',(-56.117135878067,61.9879310128291,-10.));
#36542=CARTESIAN_POINT('Ctrl Pts',(-56.1293531064626,62.0069015018125,-10.));
#36543=CARTESIAN_POINT('Ctrl Pts',(-56.2001801628626,62.1168793011676,-10.));
#36544=CARTESIAN_POINT('Ctrl Pts',(-56.2758314901157,62.2235154810087,-10.));
#36545=CARTESIAN_POINT('Ctrl Pts',(-56.3561468922528,62.3264414348563,-10.));
#36546=CARTESIAN_POINT('Ctrl Pts',(-56.4292340916213,62.420104287919,-10.));
#36547=CARTESIAN_POINT('Ctrl Pts',(-56.5061843400653,62.5106946453669,-10.));
#36548=CARTESIAN_POINT('Ctrl Pts',(-56.5869001850835,62.5979052562006,-10.));
#36549=CARTESIAN_POINT('Ctrl Pts',(-56.6479573239608,62.6638753315437,-10.));
#36550=CARTESIAN_POINT('Ctrl Pts',(-56.7111697701537,62.7279108548516,-10.));
#36551=CARTESIAN_POINT('Ctrl Pts',(-56.7764331619493,62.7899186857328,-10.));
#36552=CARTESIAN_POINT('Origin',(-60.,60.,-6.));
#36553=CARTESIAN_POINT('Origin',(60.,60.,-3.));
#36554=CARTESIAN_POINT('Ctrl Pts',(60.8043894954945,55.8135783132204,-3.));
#36555=CARTESIAN_POINT('Ctrl Pts',(60.6804230981971,55.7770540680639,-3.));
#36556=CARTESIAN_POINT('Ctrl Pts',(60.5549403090678,55.7463481935189,-3.));
#36557=CARTESIAN_POINT('Ctrl Pts',(60.4283617848279,55.7213771687008,-3.));
#36558=CARTESIAN_POINT('Ctrl Pts',(60.2999056253408,55.6960357297336,-3.));
#36559=CARTESIAN_POINT('Ctrl Pts',(60.1703203025177,55.6766003018695,-3.));
#36560=CARTESIAN_POINT('Ctrl Pts',(60.040018990912,55.6630301707006,-3.));
#36561=CARTESIAN_POINT('Ctrl Pts',(59.9818442061206,55.6569716019064,-3.));
#36562=CARTESIAN_POINT('Ctrl Pts',(59.9235264171928,55.652082796517,-2.99999999999999));
#36563=CARTESIAN_POINT('Ctrl Pts',(59.8651012902447,55.6483632564226,-2.99999999999999));
#36564=CARTESIAN_POINT('Ctrl Pts',(59.8415724912611,55.6468653339403,-2.99999999999999));
#36565=CARTESIAN_POINT('Ctrl Pts',(59.818026278381,55.6455570663652,-3.));
#36566=CARTESIAN_POINT('Ctrl Pts',(59.7944649611546,55.6444385115308,-3.));
#36567=CARTESIAN_POINT('Ctrl Pts',(59.771035780955,55.6433262297969,-3.));
#36568=CARTESIAN_POINT('Ctrl Pts',(59.7476011418858,55.6424020040368,-3.));
#36569=CARTESIAN_POINT('Ctrl Pts',(59.724166197105,55.6416655312924,-3.));
#36570=CARTESIAN_POINT('Ctrl Pts',(59.5904471279288,55.6374632406199,-3.));
#36571=CARTESIAN_POINT('Ctrl Pts',(59.4566904103623,55.6393684815201,-3.));
#36572=CARTESIAN_POINT('Ctrl Pts',(59.3233274428939,55.647328960846,-3.));
#36573=CARTESIAN_POINT('Ctrl Pts',(59.2153950098277,55.6537714832218,-3.));
#36574=CARTESIAN_POINT('Ctrl Pts',(59.1077198305457,55.6641809940724,-3.));
#36575=CARTESIAN_POINT('Ctrl Pts',(59.0005240806928,55.6785536426348,-3.));
#36576=CARTESIAN_POINT('Ctrl Pts',(58.9469262057664,55.685739966916,-3.));
#36577=CARTESIAN_POINT('Ctrl Pts',(58.8934481282158,55.6939174138492,-3.));
#36578=CARTESIAN_POINT('Ctrl Pts',(58.8401174407215,55.7030875592919,-3.));
#36579=CARTESIAN_POINT('Ctrl Pts',(58.8127285511832,55.7077970448129,-3.));
#36580=CARTESIAN_POINT('Ctrl Pts',(58.7853785354981,55.712768378203,-2.99999999999999));
#36581=CARTESIAN_POINT('Ctrl Pts',(58.7580711348704,55.7180019159915,-2.99999999999999));
#36582=CARTESIAN_POINT('Ctrl Pts',(58.7384796892885,55.7217566699567,-2.99999999999999));
#36583=CARTESIAN_POINT('Ctrl Pts',(58.7189124095391,55.7256460128853,-3.));
#36584=CARTESIAN_POINT('Ctrl Pts',(58.6993816125308,55.7296676040812,-3.));
#36585=CARTESIAN_POINT('Ctrl Pts',(58.693127863238,55.7309553151298,-3.));
#36586=CARTESIAN_POINT('Ctrl Pts',(58.6868775384995,55.7322566451671,-3.));
#36587=CARTESIAN_POINT('Ctrl Pts',(58.6806306833416,55.7335715858747,-3.));
#36588=CARTESIAN_POINT('Ctrl Pts',(58.5505754691102,55.7609477441344,-3.));
#36589=CARTESIAN_POINT('Ctrl Pts',(58.4220249805927,55.794218981014,-3.));
#36590=CARTESIAN_POINT('Ctrl Pts',(58.2953077479336,55.8330910870826,-3.));
#36591=CARTESIAN_POINT('Ctrl Pts',(58.1663246104551,55.8726582879748,-3.));
#36592=CARTESIAN_POINT('Ctrl Pts',(58.0392402106457,55.9180285436651,-3.));
#36593=CARTESIAN_POINT('Ctrl Pts',(57.9143961990582,55.9689453660749,-3.));
#36594=CARTESIAN_POINT('Ctrl Pts',(57.7879490069731,56.0205160352784,-3.));
#36595=CARTESIAN_POINT('Ctrl Pts',(57.6637993564696,56.077776790127,-3.));
#36596=CARTESIAN_POINT('Ctrl Pts',(57.5423081830428,56.1405139151216,-3.));
#36597=CARTESIAN_POINT('Ctrl Pts',(57.465938340702,56.1799507252997,-3.));
#36598=CARTESIAN_POINT('Ctrl Pts',(57.3906191333291,56.2215525292356,-3.));
#36599=CARTESIAN_POINT('Ctrl Pts',(57.3164434804249,56.2652762658272,-3.));
#36600=CARTESIAN_POINT('Ctrl Pts',(57.2554403025305,56.3012353275553,-3.));
#36601=CARTESIAN_POINT('Ctrl Pts',(57.1952106164062,56.3386297402385,-3.));
#36602=CARTESIAN_POINT('Ctrl Pts',(57.1358080455961,56.377439247764,-3.));
#36603=CARTESIAN_POINT('Ctrl Pts',(57.1208016710562,56.3872433689947,-3.));
#36604=CARTESIAN_POINT('Ctrl Pts',(57.1058499054844,56.3971366819327,-3.));
#36605=CARTESIAN_POINT('Ctrl Pts',(57.0909629618782,56.4071123926641,-3.));
#36606=CARTESIAN_POINT('Ctrl Pts',(56.9746406743767,56.4850597217074,-3.));
#36607=CARTESIAN_POINT('Ctrl Pts',(56.8621134355589,56.5681388647664,-3.));
#36608=CARTESIAN_POINT('Ctrl Pts',(56.7537376927601,56.6560786480786,-3.));
#36609=CARTESIAN_POINT('Ctrl Pts',(56.7306089015666,56.6748461400773,-3.));
#36610=CARTESIAN_POINT('Ctrl Pts',(56.7076692206168,56.6938351971782,-3.));
#36611=CARTESIAN_POINT('Ctrl Pts',(56.6849221758314,56.7130434825668,-3.));
#36612=CARTESIAN_POINT('Ctrl Pts',(56.5793101632974,56.8022254266987,-3.));
#36613=CARTESIAN_POINT('Ctrl Pts',(56.47784887195,56.896129304385,-3.));
#36614=CARTESIAN_POINT('Ctrl Pts',(56.380714466223,56.9943655777065,-3.));
#36615=CARTESIAN_POINT('Ctrl Pts',(56.2824676905965,57.093726839364,-3.));
#36616=CARTESIAN_POINT('Ctrl Pts',(56.188646908236,57.1975207658422,-3.));
#36617=CARTESIAN_POINT('Ctrl Pts',(56.0994624522646,57.3053895227055,-3.));
#36618=CARTESIAN_POINT('Ctrl Pts',(56.0193271754091,57.4023132814607,-3.));
#36619=CARTESIAN_POINT('Ctrl Pts',(55.9429351942092,57.5025277899424,-3.));
#36620=CARTESIAN_POINT('Ctrl Pts',(55.8704637655828,57.6057990864436,-3.));
#36621=CARTESIAN_POINT('Ctrl Pts',(55.8587177026021,57.6225371468875,-3.));
#36622=CARTESIAN_POINT('Ctrl Pts',(55.847074686451,57.6393555524523,-3.));
#36623=CARTESIAN_POINT('Ctrl Pts',(55.8355355388399,57.656253357144,-3.));
#36624=CARTESIAN_POINT('Ctrl Pts',(55.8253671008489,57.6711439092871,-3.));
#36625=CARTESIAN_POINT('Ctrl Pts',(55.8152846650618,57.6860882977166,-3.));
#36626=CARTESIAN_POINT('Ctrl Pts',(55.8052890498414,57.7010849236945,-3.));
#36627=CARTESIAN_POINT('Ctrl Pts',(55.7260105077896,57.8200281419958,-3.));
#36628=CARTESIAN_POINT('Ctrl Pts',(55.6521810643325,57.9422686678001,-3.));
#36629=CARTESIAN_POINT('Ctrl Pts',(55.5839783927012,58.0673941439682,-3.));
#36630=CARTESIAN_POINT('Ctrl Pts',(55.515043000026,58.1938638793468,-3.));
#36631=CARTESIAN_POINT('Ctrl Pts',(55.4518553517568,58.323281427723,-3.));
#36632=CARTESIAN_POINT('Ctrl Pts',(55.3946315085702,58.4552626427157,-3.));
#36633=CARTESIAN_POINT('Ctrl Pts',(55.3737738613536,58.5033687724028,-3.));
#36634=CARTESIAN_POINT('Ctrl Pts',(55.3537088867656,58.5518158526946,-3.));
#36635=CARTESIAN_POINT('Ctrl Pts',(55.3344483425769,58.6005864144814,-3.));
#36636=CARTESIAN_POINT('Ctrl Pts',(55.2818816840914,58.7336930100419,-3.));
#36637=CARTESIAN_POINT('Ctrl Pts',(55.235303613332,58.8692073967039,-3.));
#36638=CARTESIAN_POINT('Ctrl Pts',(55.1947264750797,59.0067151509791,-3.));
#36639=CARTESIAN_POINT('Ctrl Pts',(55.1709933297947,59.0871420034035,-3.));
#36640=CARTESIAN_POINT('Ctrl Pts',(55.1493139447911,59.1682512730649,-3.));
#36641=CARTESIAN_POINT('Ctrl Pts',(55.1296983939106,59.2499631634561,-3.));
#36642=CARTESIAN_POINT('Ctrl Pts',(55.1222104222649,59.2811555741154,-3.));
#36643=CARTESIAN_POINT('Ctrl Pts',(55.1150232579274,59.3124358186197,-3.));
#36644=CARTESIAN_POINT('Ctrl Pts',(55.1081376850014,59.3437995167499,-3.));
#36645=CARTESIAN_POINT('Ctrl Pts',(55.1026350847819,59.3688637915852,-3.));
#36646=CARTESIAN_POINT('Ctrl Pts',(55.0973242344235,59.3939859998928,-3.));
#36647=CARTESIAN_POINT('Ctrl Pts',(55.0922112631199,59.4191348146936,-3.));
#36648=CARTESIAN_POINT('Ctrl Pts',(55.0630684411167,59.5624775776013,-3.));
#36649=CARTESIAN_POINT('Ctrl Pts',(55.0403126175449,59.7068444399294,-3.));
#36650=CARTESIAN_POINT('Ctrl Pts',(55.0238938659507,59.851778335995,-3.));
#36651=CARTESIAN_POINT('Ctrl Pts',(55.0073130217029,59.9981430789608,-3.));
#36652=CARTESIAN_POINT('Ctrl Pts',(54.9971947543477,60.1450868240802,-3.));
#36653=CARTESIAN_POINT('Ctrl Pts',(54.9935344151175,60.2921650366492,-3.));
#36654=CARTESIAN_POINT('Ctrl Pts',(54.9898705323877,60.4393856326285,-3.));
#36655=CARTESIAN_POINT('Ctrl Pts',(54.9926769058727,60.5867417347185,-3.));
#36656=CARTESIAN_POINT('Ctrl Pts',(55.0019985535712,60.7338023176659,-3.));
#36657=CARTESIAN_POINT('Ctrl Pts',(55.007624235958,60.8225544522708,-3.));
#36658=CARTESIAN_POINT('Ctrl Pts',(55.0156238884368,60.9111991867765,-3.));
#36659=CARTESIAN_POINT('Ctrl Pts',(55.0260165827179,60.9996425537523,-3.));
#36660=CARTESIAN_POINT('Ctrl Pts',(55.0384683227897,61.1056087052492,-3.));
#36661=CARTESIAN_POINT('Ctrl Pts',(55.054354939434,61.2112859368579,-3.));
#36662=CARTESIAN_POINT('Ctrl Pts',(55.0736213347631,61.3165318688511,-3.));
#36663=CARTESIAN_POINT('Ctrl Pts',(56.3967816198432,63.6078550836889,-3.));
#36664=CARTESIAN_POINT('Ctrl Pts',(56.5101573278891,63.7040964917567,-3.));
#36665=CARTESIAN_POINT('Ctrl Pts',(56.6276776524244,63.7951366320638,-3.));
#36666=CARTESIAN_POINT('Ctrl Pts',(56.7489442704341,63.8807936755053,-3.));
#36667=CARTESIAN_POINT('Ctrl Pts',(56.8703218606103,63.9665291044734,-3.));
#36668=CARTESIAN_POINT('Ctrl Pts',(56.995453355925,64.0468718760484,-3.));
#36669=CARTESIAN_POINT('Ctrl Pts',(57.1239602399913,64.1215920780355,-3.));
#36670=CARTESIAN_POINT('Ctrl Pts',(57.1803120064737,64.1543577575125,-3.));
#36671=CARTESIAN_POINT('Ctrl Pts',(57.2373130376274,64.1860416170387,-3.));
#36672=CARTESIAN_POINT('Ctrl Pts',(57.2949321173609,64.2166211629568,-3.));
#36673=CARTESIAN_POINT('Ctrl Pts',(57.3242693742672,64.2321910054261,-3.));
#36674=CARTESIAN_POINT('Ctrl Pts',(57.3537668603064,64.2474745315704,-3.));
#36675=CARTESIAN_POINT('Ctrl Pts',(57.3834204755002,64.2624685748845,-3.));
#36676=CARTESIAN_POINT('Ctrl Pts',(57.4050341385029,64.2733972996662,-3.));
#36677=CARTESIAN_POINT('Ctrl Pts',(57.4267301365591,64.2841718530121,-3.));
#36678=CARTESIAN_POINT('Ctrl Pts',(57.4484948027175,64.294785320416,-3.));
#36679=CARTESIAN_POINT('Ctrl Pts',(57.5800080989128,64.3589173439526,-3.));
#36680=CARTESIAN_POINT('Ctrl Pts',(57.7141414686933,64.4172300576872,-3.));
#36681=CARTESIAN_POINT('Ctrl Pts',(57.8505256425866,64.4695128536294,-3.));
#36682=CARTESIAN_POINT('Ctrl Pts',(57.968432834675,64.5147125090446,-3.));
#36683=CARTESIAN_POINT('Ctrl Pts',(58.0880228412298,64.5554047505907,-3.));
#36684=CARTESIAN_POINT('Ctrl Pts',(58.2090619180921,64.5914221480058,-3.));
#36685=CARTESIAN_POINT('Ctrl Pts',(58.2695814565233,64.6094308467133,-3.00000000000001));
#36686=CARTESIAN_POINT('Ctrl Pts',(58.3304632962727,64.6262703667664,-3.00000000000001));
#36687=CARTESIAN_POINT('Ctrl Pts',(58.3916782037017,64.6419168917389,-3.00000000000001));
#36688=CARTESIAN_POINT('Ctrl Pts',(58.4205105124408,64.649286427325,-3.00000000000001));
#36689=CARTESIAN_POINT('Ctrl Pts',(58.4494167078449,64.6563912777525,-3.));
#36690=CARTESIAN_POINT('Ctrl Pts',(58.4783937204173,64.6632288012031,-3.));
#36691=CARTESIAN_POINT('Ctrl Pts',(58.5046585351189,64.6694263443763,-3.));
#36692=CARTESIAN_POINT('Ctrl Pts',(58.5309854155718,64.6754050197627,-3.));
#36693=CARTESIAN_POINT('Ctrl Pts',(58.5573454950175,64.6811572553105,-3.));
#36694=CARTESIAN_POINT('Ctrl Pts',(58.5636485802747,64.682532699992,-3.));
#36695=CARTESIAN_POINT('Ctrl Pts',(58.5699538441721,64.6838952676503,-3.00000000000001));
#36696=CARTESIAN_POINT('Ctrl Pts',(58.5762612548222,64.6852449426606,-3.00000000000001));
#36697=CARTESIAN_POINT('Ctrl Pts',(58.7158131526305,64.7151065958105,-3.00000000000001));
#36698=CARTESIAN_POINT('Ctrl Pts',(58.8564152550715,64.7386614193891,-3.));
#36699=CARTESIAN_POINT('Ctrl Pts',(58.9976457358102,64.7559650852701,-3.));
#36700=CARTESIAN_POINT('Ctrl Pts',(59.139815066942,64.7733837798151,-3.));
#36701=CARTESIAN_POINT('Ctrl Pts',(59.2826219755861,64.7844678684638,-3.));
#36702=CARTESIAN_POINT('Ctrl Pts',(59.4256369954039,64.7892215558739,-3.));
#36703=CARTESIAN_POINT('Ctrl Pts',(59.5672051822675,64.7939271518904,-3.));
#36704=CARTESIAN_POINT('Ctrl Pts',(59.7089780507634,64.792429595255,-3.));
#36705=CARTESIAN_POINT('Ctrl Pts',(59.8505280903461,64.784683690889,-3.));
#36706=CARTESIAN_POINT('Ctrl Pts',(59.9398961209693,64.77979329156,-3.));
#36707=CARTESIAN_POINT('Ctrl Pts',(60.0291750731265,64.7724112867483,-3.));
#36708=CARTESIAN_POINT('Ctrl Pts',(60.1182530286222,64.7625165118624,-3.));
#36709=CARTESIAN_POINT('Ctrl Pts',(60.1850614952439,64.7550954306981,-3.));
#36710=CARTESIAN_POINT('Ctrl Pts',(60.2517568353818,64.746260760684,-3.));
#36711=CARTESIAN_POINT('Ctrl Pts',(60.3182901338221,64.7360008324502,-3.));
#36712=CARTESIAN_POINT('Ctrl Pts',(60.335922917866,64.733281726332,-3.));
#36713=CARTESIAN_POINT('Ctrl Pts',(60.3535443117469,64.7304625022116,-3.));
#36714=CARTESIAN_POINT('Ctrl Pts',(60.3711533849972,64.7275429155473,-3.));
#36715=CARTESIAN_POINT('Ctrl Pts',(60.3893511940337,64.7245257164122,-3.));
#36716=CARTESIAN_POINT('Ctrl Pts',(60.4075271680476,64.7214027597405,-3.));
#36717=CARTESIAN_POINT('Ctrl Pts',(60.4256777486191,64.718174556807,-3.));
#36718=CARTESIAN_POINT('Ctrl Pts',(60.5629885227604,64.693752911332,-3.));
#36719=CARTESIAN_POINT('Ctrl Pts',(60.6988965337467,64.6633038922754,-3.));
#36720=CARTESIAN_POINT('Ctrl Pts',(60.8330040002292,64.6268299926211,-3.));
#36721=CARTESIAN_POINT('Ctrl Pts',(60.8581918055621,64.6199795352355,-3.));
#36722=CARTESIAN_POINT('Ctrl Pts',(60.8833160533696,64.6129164047735,-3.));
#36723=CARTESIAN_POINT('Ctrl Pts',(60.9083740419004,64.6056404226031,-3.));
#36724=CARTESIAN_POINT('Ctrl Pts',(61.0423381249251,64.566741838291,-3.00000000000001));
#36725=CARTESIAN_POINT('Ctrl Pts',(61.1744105226846,64.5217632900704,-3.));
#36726=CARTESIAN_POINT('Ctrl Pts',(61.3042176288045,64.4709134975508,-3.));
#36727=CARTESIAN_POINT('Ctrl Pts',(61.4335909730649,64.4202336240844,-3.));
#36728=CARTESIAN_POINT('Ctrl Pts',(61.5607147887615,64.3637211759828,-3.));
#36729=CARTESIAN_POINT('Ctrl Pts',(61.6851875383315,64.3015421572917,-3.));
#36730=CARTESIAN_POINT('Ctrl Pts',(61.7912746295725,64.2485474957939,-3.));
#36731=CARTESIAN_POINT('Ctrl Pts',(61.895435682969,64.1914358019316,-3.));
#36732=CARTESIAN_POINT('Ctrl Pts',(61.9973985420836,64.1302904783211,-3.00000000000001));
#36733=CARTESIAN_POINT('Ctrl Pts',(62.0157427331232,64.1192897913335,-3.00000000000001));
#36734=CARTESIAN_POINT('Ctrl Pts',(62.0340157094886,64.1081585033305,-3.));
#36735=CARTESIAN_POINT('Ctrl Pts',(62.052215799533,64.0968970474319,-3.));
#36736=CARTESIAN_POINT('Ctrl Pts',(62.0686109323645,64.086752423703,-3.));
#36737=CARTESIAN_POINT('Ctrl Pts',(62.0849390653794,64.0765070092133,-3.));
#36738=CARTESIAN_POINT('Ctrl Pts',(62.1011957941185,64.0661635944481,-3.));
#36739=CARTESIAN_POINT('Ctrl Pts',(62.2160942895865,63.9930589241547,-3.));
#36740=CARTESIAN_POINT('Ctrl Pts',(62.3274845529479,63.9150275718819,-3.));
#36741=CARTESIAN_POINT('Ctrl Pts',(62.4350222646538,63.8322713282373,-3.));
#36742=CARTESIAN_POINT('Ctrl Pts',(62.5416034782076,63.7502511630611,-3.));
#36743=CARTESIAN_POINT('Ctrl Pts',(62.6444009200186,63.6635892555824,-3.));
#36744=CARTESIAN_POINT('Ctrl Pts',(62.7430433478219,63.5724461389909,-3.));
#36745=CARTESIAN_POINT('Ctrl Pts',(62.7758260127342,63.5421557830373,-3.));
#36746=CARTESIAN_POINT('Ctrl Pts',(62.808149428445,63.5113702208032,-3.));
#36747=CARTESIAN_POINT('Ctrl Pts',(62.8399989163846,63.4800946064471,-3.));
#36748=CARTESIAN_POINT('Ctrl Pts',(62.9365720682666,63.3852615384508,-3.));
#36749=CARTESIAN_POINT('Ctrl Pts',(63.0287914724018,63.2859242142018,-3.));
#36750=CARTESIAN_POINT('Ctrl Pts',(63.116384688617,63.1824188586198,-3.));
#36751=CARTESIAN_POINT('Ctrl Pts',(63.1636033936845,63.1266224274654,-3.));
#36752=CARTESIAN_POINT('Ctrl Pts',(63.2094769322843,63.0696144553279,-3.));
#36753=CARTESIAN_POINT('Ctrl Pts',(63.2539565107167,63.0114459571216,-3.));
#36754=CARTESIAN_POINT('Ctrl Pts',(63.2715142364304,62.9884847112493,-3.));
#36755=CARTESIAN_POINT('Ctrl Pts',(63.2888547102122,62.9653426270302,-3.));
#36756=CARTESIAN_POINT('Ctrl Pts',(63.3059747354259,62.942022815916,-3.));
#36757=CARTESIAN_POINT('Ctrl Pts',(63.3199565107891,62.9229777294489,-3.));
#36758=CARTESIAN_POINT('Ctrl Pts',(63.3337935971807,62.9038106514913,-3.));
#36759=CARTESIAN_POINT('Ctrl Pts',(63.3474682801689,62.8845461191246,-3.));
#36760=CARTESIAN_POINT('Ctrl Pts',(63.4242351022266,62.7763990469401,-3.));
#36761=CARTESIAN_POINT('Ctrl Pts',(63.4959842559734,62.6650546750512,-3.));
#36762=CARTESIAN_POINT('Ctrl Pts',(63.5625180995312,62.5508627289101,-3.));
#36763=CARTESIAN_POINT('Ctrl Pts',(63.6288088601457,62.4370879856974,-3.));
#36764=CARTESIAN_POINT('Ctrl Pts',(63.6899226483436,62.3204856807288,-3.));
#36765=CARTESIAN_POINT('Ctrl Pts',(63.7456163613347,62.2013821649674,-3.));
#36766=CARTESIAN_POINT('Ctrl Pts',(63.8003210691109,62.0843936814399,-3.));
#36767=CARTESIAN_POINT('Ctrl Pts',(63.8497966468504,61.9649913311224,-3.));
#36768=CARTESIAN_POINT('Ctrl Pts',(63.8937635139461,61.8434762846442,-3.));
#36769=CARTESIAN_POINT('Ctrl Pts',(63.9160764497028,61.7818080875531,-3.));
#36770=CARTESIAN_POINT('Ctrl Pts',(63.9369698093169,61.7195956989266,-3.));
#36771=CARTESIAN_POINT('Ctrl Pts',(63.9564018718053,61.6568785193336,-3.));
#36772=CARTESIAN_POINT('Ctrl Pts',(63.9829907032676,61.5710627949871,-3.));
#36773=CARTESIAN_POINT('Ctrl Pts',(64.0068439948043,61.4843017745449,-3.));
#36774=CARTESIAN_POINT('Ctrl Pts',(64.0279238903325,61.3967314318667,-3.));
#36775=CARTESIAN_POINT('Origin',(60.,60.,-13.3123464956316));
#36776=CARTESIAN_POINT('Ctrl Pts',(65.0992547463301,60.0000912484111,-9.56234649563159));
#36777=CARTESIAN_POINT('Ctrl Pts',(65.0993446065218,60.1069729367835,-9.55734157105847));
#36778=CARTESIAN_POINT('Ctrl Pts',(65.0703981457348,61.0460695286254,-9.51336443385491));
#36779=CARTESIAN_POINT('Ctrl Pts',(64.5173398680237,62.7859966304905,-9.43041508402093));
#36780=CARTESIAN_POINT('Ctrl Pts',(62.6758304956081,64.5834554024384,-9.31349844612963));
#36781=CARTESIAN_POINT('Ctrl Pts',(60.205263132424,65.3033953276082,-9.19658180823835));
#36782=CARTESIAN_POINT('Ctrl Pts',(57.6864406181491,64.7765653538453,-9.07966517034705));
#36783=CARTESIAN_POINT('Ctrl Pts',(55.7115103282802,63.1268179703927,-8.96274853245576));
#36784=CARTESIAN_POINT('Ctrl Pts',(54.7447564613263,60.7419901067622,-8.84583189456447));
#36785=CARTESIAN_POINT('Ctrl Pts',(55.0134521769933,58.1827288792718,-8.72891525667318));
#36786=CARTESIAN_POINT('Ctrl Pts',(56.4544300560118,56.0506873938616,-8.6119986187819));
#36787=CARTESIAN_POINT('Ctrl Pts',(58.7289322067895,54.8470867941934,-8.49508198089061));
#36788=CARTESIAN_POINT('Ctrl Pts',(61.3022482494153,54.8548764161609,-8.37816534299932));
#36789=CARTESIAN_POINT('Ctrl Pts',(63.5694203037008,56.0722332749569,-8.26124870510803));
#36790=CARTESIAN_POINT('Ctrl Pts',(64.8552427510861,57.9997589069056,-8.15597575598545));
#36791=CARTESIAN_POINT('Ctrl Pts',(65.0983472268173,59.4163728002799,-8.08967501949331));
#36792=CARTESIAN_POINT('Ctrl Pts',(65.098848108647,60.0001169986396,-8.06234649563159));
#36793=CARTESIAN_POINT('Ctrl Pts',(65.0987893697715,60.0001196244759,-9.68765350436842));
#36794=CARTESIAN_POINT('Ctrl Pts',(65.0989958456617,60.2735580353962,-9.67485236502099));
#36795=CARTESIAN_POINT('Ctrl Pts',(65.0114730664976,61.3793292170961,-9.62307901304313));
#36796=CARTESIAN_POINT('Ctrl Pts',(64.2231822164303,63.2145072853594,-9.53233344843484));
#36797=CARTESIAN_POINT('Ctrl Pts',(62.2146698080337,64.8232034325914,-9.41541681054355));
#36798=CARTESIAN_POINT('Ctrl Pts',(59.6855379323249,65.2980445186201,-9.29850017265226));
#36799=CARTESIAN_POINT('Ctrl Pts',(57.2303209838473,64.5273621068898,-9.18158353476097));
#36800=CARTESIAN_POINT('Ctrl Pts',(55.4262302676069,62.6923526051193,-9.06466689686969));
#36801=CARTESIAN_POINT('Ctrl Pts',(54.6973796845391,60.2243982381535,-8.94775025897839));
#36802=CARTESIAN_POINT('Ctrl Pts',(55.2151175810578,57.7036915329656,-8.8308336210871));
#36803=CARTESIAN_POINT('Ctrl Pts',(56.8577278151099,55.7228209598733,-8.71391698319582));
#36804=CARTESIAN_POINT('Ctrl Pts',(59.2390517104132,54.7474680995942,-8.59700034530453));
#36805=CARTESIAN_POINT('Ctrl Pts',(61.799265976347,55.0069271683894,-8.48008370741324));
#36806=CARTESIAN_POINT('Ctrl Pts',(63.9364928560947,56.4402025290253,-8.36316706952195));
#36807=CARTESIAN_POINT('Ctrl Pts',(64.9468057472684,58.3328863836753,-8.26569033517367));
#36808=CARTESIAN_POINT('Ctrl Pts',(65.0986023825915,59.5827292143741,-8.20718581345583));
#36809=CARTESIAN_POINT('Ctrl Pts',(65.0986049232486,60.0000009026908,-8.18765350436841));
#36810=CARTESIAN_POINT('Ctrl Pts',(56.7766472160421,62.7898325810254,-10.));
#36811=CARTESIAN_POINT('Ctrl Pts',(56.3212170277455,62.2636317705077,-9.96102778736957));
#36812=CARTESIAN_POINT('Ctrl Pts',(55.6734220606415,60.9843943012708,-9.88308336210871));
#36813=CARTESIAN_POINT('Ctrl Pts',(55.7189117270138,58.8332763305925,-9.76616672421742));
#36814=CARTESIAN_POINT('Ctrl Pts',(56.7709224287295,56.9567114979888,-9.64925008632613));
#36815=CARTESIAN_POINT('Ctrl Pts',(58.582037303137,55.7954439707652,-9.53233344843484));
#36816=CARTESIAN_POINT('Ctrl Pts',(60.7265123733809,55.6226835105978,-9.41541681054355));
#36817=CARTESIAN_POINT('Ctrl Pts',(62.7001876951902,56.4789515650734,-9.29850017265227));
#36818=CARTESIAN_POINT('Ctrl Pts',(64.0390812605523,58.1629928045498,-9.18158353476097));
#36819=CARTESIAN_POINT('Ctrl Pts',(64.4284304613218,60.2788876953404,-9.06466689686969));
#36820=CARTESIAN_POINT('Ctrl Pts',(63.7767052083516,62.329222129002,-8.94775025897839));
#36821=CARTESIAN_POINT('Ctrl Pts',(62.2371181413566,63.8319808551863,-8.8308336210871));
#36822=CARTESIAN_POINT('Ctrl Pts',(60.1716094790201,64.433883954029,-8.71391698319582));
#36823=CARTESIAN_POINT('Ctrl Pts',(58.0657572769503,63.9934297123833,-8.59700034530453));
#36824=CARTESIAN_POINT('Ctrl Pts',(56.414624147766,62.6141645435937,-8.48008370741324));
#36825=CARTESIAN_POINT('Ctrl Pts',(55.6063731701577,60.6203380712154,-8.36316706952195));
#36826=CARTESIAN_POINT('Ctrl Pts',(55.8310152246563,58.4806772332488,-8.24625043163065));
#36827=CARTESIAN_POINT('Ctrl Pts',(57.0357394251379,56.6981918729225,-8.12933379373937));
#36828=CARTESIAN_POINT('Ctrl Pts',(58.9373284953018,55.6919260646492,-8.01241715584808));
#36829=CARTESIAN_POINT('Ctrl Pts',(61.0887398092287,55.6984385491457,-7.89550051795679));
#36830=CARTESIAN_POINT('Ctrl Pts',(62.984200579462,56.7162052267388,-7.7785838800655));
#36831=CARTESIAN_POINT('Ctrl Pts',(64.1781085527216,58.5059455017865,-7.66166724217421));
#36832=CARTESIAN_POINT('Ctrl Pts',(64.3897900743559,60.6469434568749,-7.54475060428292));
#36833=CARTESIAN_POINT('Ctrl Pts',(63.5694792390211,62.6358046484627,-7.42783396639163));
#36834=CARTESIAN_POINT('Ctrl Pts',(61.9100261920983,64.0051199372434,-7.31091732850034));
#36835=CARTESIAN_POINT('Ctrl Pts',(59.8015410025307,64.4326543606342,-7.19400069060905));
#36836=CARTESIAN_POINT('Ctrl Pts',(57.7397245218596,63.8185989207299,-7.07708405271776));
#36837=CARTESIAN_POINT('Ctrl Pts',(56.2092450962316,62.3058003341377,-6.96016741482647));
#36838=CARTESIAN_POINT('Ctrl Pts',(55.5699912429921,60.2531607317565,-6.84325077693518));
#36839=CARTESIAN_POINT('Ctrl Pts',(55.9720481528381,58.1361860697788,-6.72633413904389));
#36840=CARTESIAN_POINT('Ctrl Pts',(57.3213012555681,56.4677215227762,-6.60941750115261));
#36841=CARTESIAN_POINT('Ctrl Pts',(59.9592774377706,55.3204052536368,-6.45352865063088));
#36842=CARTESIAN_POINT('Ctrl Pts',(63.6618728268516,56.5785257712713,-6.25866758747874));
#36843=CARTESIAN_POINT('Ctrl Pts',(64.8778949937948,61.1497560295123,-6.02483431169615));
#36844=CARTESIAN_POINT('Ctrl Pts',(62.2898185828427,64.0812983442691,-5.82997324854401));
#36845=CARTESIAN_POINT('Ctrl Pts',(59.4304505580215,64.3963657306031,-5.67408439802229));
#36846=CARTESIAN_POINT('Ctrl Pts',(57.430523426142,63.6188380159844,-5.557167760131));
#36847=CARTESIAN_POINT('Ctrl Pts',(56.0297438251523,61.9814474127173,-5.44025112223971));
#36848=CARTESIAN_POINT('Ctrl Pts',(55.5646049319228,59.8824903773911,-5.32333448434842));
#36849=CARTESIAN_POINT('Ctrl Pts',(56.1411247152275,57.8091954694446,-5.20641784645712));
#36850=CARTESIAN_POINT('Ctrl Pts',(57.6253116388877,56.2518450082663,-5.08950120856584));
#36851=CARTESIAN_POINT('Ctrl Pts',(59.6675354017074,55.5752228240151,-4.97258457067455));
#36852=CARTESIAN_POINT('Ctrl Pts',(61.7880226520381,55.9390120440154,-4.85566793278326));
#36853=CARTESIAN_POINT('Ctrl Pts',(63.4881170626526,57.2574041330032,-4.73875129489197));
#36854=CARTESIAN_POINT('Ctrl Pts',(64.3682162435255,59.2205920361106,-4.62183465700068));
#36855=CARTESIAN_POINT('Ctrl Pts',(64.2213857418157,61.3669907186962,-4.50491801910939));
#36856=CARTESIAN_POINT('Ctrl Pts',(63.082159015354,63.1920340067288,-4.3880013812181));
#36857=CARTESIAN_POINT('Ctrl Pts',(61.2183485912993,64.2666612780442,-4.27108474332681));
#36858=CARTESIAN_POINT('Ctrl Pts',(59.0681189506421,64.3382456551615,-4.15416810543553));
#36859=CARTESIAN_POINT('Ctrl Pts',(57.1369637190351,63.3899556120333,-4.03725146754423));
#36860=CARTESIAN_POINT('Ctrl Pts',(55.8788769012213,61.6447249674203,-3.92033482965294));
#36861=CARTESIAN_POINT('Ctrl Pts',(55.5896202577371,59.5128374687636,-3.80341819176165));
#36862=CARTESIAN_POINT('Ctrl Pts',(56.3371953964416,57.4954766475313,-3.68650155387037));
#36863=CARTESIAN_POINT('Ctrl Pts',(57.945854696259,56.0669013403294,-3.56958491597907));
#36864=CARTESIAN_POINT('Ctrl Pts',(60.0374221729278,55.5629543318799,-3.45266827808779));
#36865=CARTESIAN_POINT('Ctrl Pts',(62.1201892005749,56.1021068992122,-3.3357516401965));
#36866=CARTESIAN_POINT('Ctrl Pts',(63.7045295307839,57.5576125154289,-3.21883500230521));
#36867=CARTESIAN_POINT('Ctrl Pts',(64.417962512424,59.5872929422394,-3.10191836441392));
#36868=CARTESIAN_POINT('Ctrl Pts',(64.0928111357616,61.7140030980687,-2.98500172652263));
#36869=CARTESIAN_POINT('Ctrl Pts',(62.805423754937,63.4377528158129,-2.86808508863134));
#36870=CARTESIAN_POINT('Ctrl Pts',(60.858656910251,64.3533514942534,-2.75116845074005));
#36871=CARTESIAN_POINT('Ctrl Pts',(58.7097667243778,64.2454218753984,-2.63425181284876));
#36872=CARTESIAN_POINT('Ctrl Pts',(57.4799483719373,63.5081067174902,-2.5563073875879));
#36873=CARTESIAN_POINT('Ctrl Pts',(56.9875426643247,63.0163338344315,-2.51733517495747));
#36874=CARTESIAN_POINT('Ctrl Pts',(56.5659409116095,62.9722002436837,-10.1608882750142));
#36875=CARTESIAN_POINT('Ctrl Pts',(56.0807398547996,62.4116023827639,-10.1219160623837));
#36876=CARTESIAN_POINT('Ctrl Pts',(55.390599388243,61.0487428536097,-10.0439716371229));
#36877=CARTESIAN_POINT('Ctrl Pts',(55.4390626538871,58.7570091488251,-9.9270549992316));
#36878=CARTESIAN_POINT('Ctrl Pts',(56.5598419025287,56.757775757299,-9.8101383613403));
#36879=CARTESIAN_POINT('Ctrl Pts',(58.4893469587335,55.5205977090997,-9.69322172344902));
#36880=CARTESIAN_POINT('Ctrl Pts',(60.7740035254761,55.3365441263504,-9.57630508555772));
#36881=CARTESIAN_POINT('Ctrl Pts',(62.8766953903328,56.2487852900246,-9.45938844766644));
#36882=CARTESIAN_POINT('Ctrl Pts',(64.3031106556436,58.0429100760021,-9.34247180977514));
#36883=CARTESIAN_POINT('Ctrl Pts',(64.7179110982492,60.297118214795,-9.22555517188386));
#36884=CARTESIAN_POINT('Ctrl Pts',(64.0235834282423,62.4814802961648,-9.10863853399257));
#36885=CARTESIAN_POINT('Ctrl Pts',(62.3833555927738,64.0824723709371,-8.99172189610128));
#36886=CARTESIAN_POINT('Ctrl Pts',(60.1828273634881,64.7237210785554,-8.87480525820999));
#36887=CARTESIAN_POINT('Ctrl Pts',(57.9393183906832,64.254474926204,-8.7578886203187));
#36888=CARTESIAN_POINT('Ctrl Pts',(56.1802528746041,62.7850490191933,-8.64097198242741));
#36889=CARTESIAN_POINT('Ctrl Pts',(55.3191676005472,60.660888749731,-8.52405534453612));
#36890=CARTESIAN_POINT('Ctrl Pts',(55.5584942087686,58.3813611152564,-8.40713870664483));
#36891=CARTESIAN_POINT('Ctrl Pts',(56.8419696354292,56.4823570465689,-8.29022206875355));
#36892=CARTESIAN_POINT('Ctrl Pts',(58.8678630657977,55.4103129744973,-8.17330543086225));
#36893=CARTESIAN_POINT('Ctrl Pts',(61.1599092892909,55.4172511714842,-8.05638879297097));
#36894=CARTESIAN_POINT('Ctrl Pts',(63.1792738208749,56.5015479094781,-7.93947215507968));
#36895=CARTESIAN_POINT('Ctrl Pts',(64.4512259778585,58.4082811370585,-7.82255551718838));
#36896=CARTESIAN_POINT('Ctrl Pts',(64.6767448403393,60.6892332942311,-7.7056388792971));
#36897=CARTESIAN_POINT('Ctrl Pts',(63.8028113716211,62.8081037090707,-7.58872224140581));
#36898=CARTESIAN_POINT('Ctrl Pts',(62.0348820757948,64.2669293255877,-7.47180560351452));
#36899=CARTESIAN_POINT('Ctrl Pts',(59.788568000585,64.7224111082681,-7.35488896562323));
#36900=CARTESIAN_POINT('Ctrl Pts',(57.5919733059925,64.0682156771401,-7.23797232773193));
#36901=CARTESIAN_POINT('Ctrl Pts',(55.9614484663504,62.4565274495758,-7.12105568984065));
#36902=CARTESIAN_POINT('Ctrl Pts',(55.280407434965,60.2697095136588,-7.00413905194936));
#36903=CARTESIAN_POINT('Ctrl Pts',(55.7087462727672,58.0143510204657,-6.88722241405807));
#36904=CARTESIAN_POINT('Ctrl Pts',(57.1461982646896,56.2368211547287,-6.77030577616678));
#36905=CARTESIAN_POINT('Ctrl Pts',(59.956615457786,55.014506339886,-6.61441692564507));
#36906=CARTESIAN_POINT('Ctrl Pts',(63.901244605978,56.354868530266,-6.41955586249291));
#36907=CARTESIAN_POINT('Ctrl Pts',(65.1967565322115,61.2249140591216,-6.18572258671033));
#36908=CARTESIAN_POINT('Ctrl Pts',(62.4395009923554,64.3480874142361,-5.99086152355818));
#36909=CARTESIAN_POINT('Ctrl Pts',(59.3932198649654,64.6837503385306,-5.83497267303646));
#36910=CARTESIAN_POINT('Ctrl Pts',(57.2625601439663,63.8553966664936,-5.71805603514517));
#36911=CARTESIAN_POINT('Ctrl Pts',(55.7702134348034,62.1109720070587,-5.60113939725388));
#36912=CARTESIAN_POINT('Ctrl Pts',(55.2746690278715,59.8748089289196,-5.48422275936259));
#36913=CARTESIAN_POINT('Ctrl Pts',(55.8888751462175,57.6659854774559,-5.3673061214713));
#36914=CARTESIAN_POINT('Ctrl Pts',(57.4700814043196,56.0068330782413,-5.25038948358001));
#36915=CARTESIAN_POINT('Ctrl Pts',(59.6458026310317,55.2859809975139,-5.13347284568873));
#36916=CARTESIAN_POINT('Ctrl Pts',(61.9049033258284,55.6735506372437,-5.01655620779744));
#36917=CARTESIAN_POINT('Ctrl Pts',(63.7161306574902,57.0781242718092,-4.89963956990615));
#36918=CARTESIAN_POINT('Ctrl Pts',(64.6537607567468,59.1696431692867,-4.78272293201486));
#36919=CARTESIAN_POINT('Ctrl Pts',(64.4973321395136,61.4563490923634,-4.66580629412357));
#36920=CARTESIAN_POINT('Ctrl Pts',(63.2836356700444,63.4006930441535,-4.54888965623228));
#36921=CARTESIAN_POINT('Ctrl Pts',(61.29799042587,64.5455672776098,-4.43197301834099));
#36922=CARTESIAN_POINT('Ctrl Pts',(59.007203120064,64.6218310306964,-4.3150563804497));
#36923=CARTESIAN_POINT('Ctrl Pts',(56.9498108274184,63.6115525227894,-4.19813974255841));
#36924=CARTESIAN_POINT('Ctrl Pts',(55.6094845397717,61.7522384612638,-4.08122310466712));
#36925=CARTESIAN_POINT('Ctrl Pts',(55.3013195724191,59.4809922989995,-3.96430646677583));
#36926=CARTESIAN_POINT('Ctrl Pts',(56.0977627083054,57.3317592714531,-3.84738982888454));
#36927=CARTESIAN_POINT('Ctrl Pts',(57.8115779370184,55.8097998875587,-3.73047319099325));
#36928=CARTESIAN_POINT('Ctrl Pts',(60.0398684108329,55.2729105302888,-3.61355655310196));
#36929=CARTESIAN_POINT('Ctrl Pts',(62.2587831619229,55.8473067872207,-3.49663991521067));
#36930=CARTESIAN_POINT('Ctrl Pts',(63.9466897221777,57.3979568787802,-3.37972327731938));
#36931=CARTESIAN_POINT('Ctrl Pts',(64.7067588733894,59.5603148282126,-3.26280663942809));
#36932=CARTESIAN_POINT('Ctrl Pts',(64.360352781668,61.8260452116026,-3.14589000153681));
#36933=CARTESIAN_POINT('Ctrl Pts',(62.9888105919944,63.6624741665064,-3.02897336364551));
#36934=CARTESIAN_POINT('Ctrl Pts',(60.9147861757894,64.6379243184927,-2.91205672575423));
#36935=CARTESIAN_POINT('Ctrl Pts',(58.6254258831533,64.5229394833297,-2.79514008786294));
#36936=CARTESIAN_POINT('Ctrl Pts',(57.3152159330398,63.7374270096024,-2.71719566260208));
#36937=CARTESIAN_POINT('Ctrl Pts',(56.7906223161642,63.213507584184,-2.67822344997165));
#36938=CARTESIAN_POINT('Ctrl Pts',(56.3552346071769,63.1545679063421,-10.3217765500284));
#36939=CARTESIAN_POINT('Ctrl Pts',(55.8402626818537,62.55957299502,-10.2828043373979));
#36940=CARTESIAN_POINT('Ctrl Pts',(55.1077767158446,61.1130914059486,-10.2048599121371));
#36941=CARTESIAN_POINT('Ctrl Pts',(55.1592135807605,58.6807419670576,-10.0879432742458));
#36942=CARTESIAN_POINT('Ctrl Pts',(56.3487613763279,56.5588400166092,-9.97102663635448));
#36943=CARTESIAN_POINT('Ctrl Pts',(58.3966566143299,55.2457514474342,-9.8541099984632));
#36944=CARTESIAN_POINT('Ctrl Pts',(60.8214946775714,55.0504047421029,-9.7371933605719));
#36945=CARTESIAN_POINT('Ctrl Pts',(63.0532030854754,56.0186190149759,-9.62027672268062));
#36946=CARTESIAN_POINT('Ctrl Pts',(64.5671400507348,57.9228273474544,-9.50336008478932));
#36947=CARTESIAN_POINT('Ctrl Pts',(65.0073917351767,60.3153487342495,-9.38644344689804));
#36948=CARTESIAN_POINT('Ctrl Pts',(64.270461648133,62.6337384633277,-9.26952680900675));
#36949=CARTESIAN_POINT('Ctrl Pts',(62.529593044191,64.3329638866877,-9.15261017111546));
#36950=CARTESIAN_POINT('Ctrl Pts',(60.194045247956,65.0135582030818,-9.03569353322417));
#36951=CARTESIAN_POINT('Ctrl Pts',(57.8128795044162,64.5155201400246,-8.91877689533288));
#36952=CARTESIAN_POINT('Ctrl Pts',(55.9458816014421,62.9559334947931,-8.80186025744159));
#36953=CARTESIAN_POINT('Ctrl Pts',(55.0319620309368,60.7014394282466,-8.6849436195503));
#36954=CARTESIAN_POINT('Ctrl Pts',(55.285973192881,58.2820449972641,-8.56802698165901));
#36955=CARTESIAN_POINT('Ctrl Pts',(56.6481998457205,56.2665222202153,-8.45111034376772));
#36956=CARTESIAN_POINT('Ctrl Pts',(58.7983976362936,55.1286998843454,-8.33419370587643));
#36957=CARTESIAN_POINT('Ctrl Pts',(61.2310787693531,55.1360637938226,-8.21727706798514));
#36958=CARTESIAN_POINT('Ctrl Pts',(63.3743470622879,56.2868905922175,-8.10036043009385));
#36959=CARTESIAN_POINT('Ctrl Pts',(64.7243434029953,58.3106167723305,-7.98344379220256));
#36960=CARTESIAN_POINT('Ctrl Pts',(64.9636996063227,60.7315231315872,-7.86652715431127));
#36961=CARTESIAN_POINT('Ctrl Pts',(64.0361435042211,62.9804027696786,-7.74961051641998));
#36962=CARTESIAN_POINT('Ctrl Pts',(62.1597379594913,64.528738713932,-7.63269387852869));
#36963=CARTESIAN_POINT('Ctrl Pts',(59.7755949986392,65.0121678559021,-7.5157772406374));
#36964=CARTESIAN_POINT('Ctrl Pts',(57.4442220901253,64.3178324335504,-7.39886060274612));
#36965=CARTESIAN_POINT('Ctrl Pts',(55.7136518364692,62.6072545650141,-7.28194396485483));
#36966=CARTESIAN_POINT('Ctrl Pts',(54.9908236269379,60.2862582955611,-7.16502732696353));
#36967=CARTESIAN_POINT('Ctrl Pts',(55.4454443926962,57.8925159711526,-7.04811068907225));
#36968=CARTESIAN_POINT('Ctrl Pts',(56.9710952738111,56.0059207866812,-6.93119405118096));
#36969=CARTESIAN_POINT('Ctrl Pts',(59.9539534778013,54.7086074261351,-6.77530520065924));
#36970=CARTESIAN_POINT('Ctrl Pts',(64.1406163851045,56.1312112892607,-6.58044413750709));
#36971=CARTESIAN_POINT('Ctrl Pts',(65.5156180706283,61.3000720887308,-6.34661086172451));
#36972=CARTESIAN_POINT('Ctrl Pts',(62.5891834018679,64.6148764842033,-6.15174979857236));
#36973=CARTESIAN_POINT('Ctrl Pts',(59.3559891719093,64.9711349464581,-5.99586094805064));
#36974=CARTESIAN_POINT('Ctrl Pts',(57.0945968617905,64.0919553170029,-5.87894431015935));
#36975=CARTESIAN_POINT('Ctrl Pts',(55.5106830444545,62.2404966014001,-5.76202767226806));
#36976=CARTESIAN_POINT('Ctrl Pts',(54.9847331238201,59.8671274804482,-5.64511103437677));
#36977=CARTESIAN_POINT('Ctrl Pts',(55.6366255772074,57.5227754854671,-5.52819439648548));
#36978=CARTESIAN_POINT('Ctrl Pts',(57.3148511697517,55.7618211482163,-5.41127775859419));
#36979=CARTESIAN_POINT('Ctrl Pts',(59.6240698603559,54.9967391710128,-5.2943611207029));
#36980=CARTESIAN_POINT('Ctrl Pts',(62.0217839996187,55.408089230472,-5.17744448281161));
#36981=CARTESIAN_POINT('Ctrl Pts',(63.9441442523277,56.8988444106153,-5.06052784492032));
#36982=CARTESIAN_POINT('Ctrl Pts',(64.9393052699681,59.1186943024627,-4.94361120702903));
#36983=CARTESIAN_POINT('Ctrl Pts',(64.7732785372114,61.5457074660306,-4.82669456913774));
#36984=CARTESIAN_POINT('Ctrl Pts',(63.4851123247348,63.6093520815783,-4.70977793124645));
#36985=CARTESIAN_POINT('Ctrl Pts',(61.3776322604409,64.8244732771755,-4.59286129335517));
#36986=CARTESIAN_POINT('Ctrl Pts',(58.9462872894859,64.9054164062312,-4.47594465546388));
#36987=CARTESIAN_POINT('Ctrl Pts',(56.7626579358016,63.8331494335455,-4.35902801757259));
#36988=CARTESIAN_POINT('Ctrl Pts',(55.3400921783221,61.8597519551072,-4.2421113796813));
#36989=CARTESIAN_POINT('Ctrl Pts',(55.0130188871011,59.4491471292353,-4.12519474179001));
#36990=CARTESIAN_POINT('Ctrl Pts',(55.8583300201691,57.168041895375,-4.00827810389872));
#36991=CARTESIAN_POINT('Ctrl Pts',(57.6773011777778,55.552698434788,-3.89136146600743));
#36992=CARTESIAN_POINT('Ctrl Pts',(60.0423146487379,54.9828667286977,-3.77444482811614));
#36993=CARTESIAN_POINT('Ctrl Pts',(62.3973771232709,55.5925066752293,-3.65752819022485));
#36994=CARTESIAN_POINT('Ctrl Pts',(64.1888499135715,57.2383012421313,-3.54061155233356));
#36995=CARTESIAN_POINT('Ctrl Pts',(64.9955552343548,59.5333367141859,-3.42369491444227));
#36996=CARTESIAN_POINT('Ctrl Pts',(64.6278944275743,61.9380873251365,-3.30677827655098));
#36997=CARTESIAN_POINT('Ctrl Pts',(63.1721974290518,63.8871955171999,-3.18986163865969));
#36998=CARTESIAN_POINT('Ctrl Pts',(60.9709154413277,64.9224971427319,-3.0729450007684));
#36999=CARTESIAN_POINT('Ctrl Pts',(58.5410850419288,64.800457091261,-2.95602836287711));
#37000=CARTESIAN_POINT('Ctrl Pts',(57.1504834941423,63.9667473017145,-2.87808393761625));
#37001=CARTESIAN_POINT('Ctrl Pts',(56.5937019680037,63.4106813339364,-2.83911172498582));
#37002=CARTESIAN_POINT('Ctrl Pts',(56.1445283027442,63.3369355690004,-10.4826648250425));
#37003=CARTESIAN_POINT('Ctrl Pts',(55.5997855089079,62.7075436072762,-10.4436926124121));
#37004=CARTESIAN_POINT('Ctrl Pts',(54.8249540434462,61.1774399582876,-10.3657481871512));
#37005=CARTESIAN_POINT('Ctrl Pts',(54.8793645076338,58.60447478529,-10.24883154926));
#37006=CARTESIAN_POINT('Ctrl Pts',(56.1376808501272,56.3599042759194,-10.1319149113687));
#37007=CARTESIAN_POINT('Ctrl Pts',(58.3039662699263,54.9709051857687,-10.0149982734774));
#37008=CARTESIAN_POINT('Ctrl Pts',(60.8689858296667,54.7642653578555,-9.89808163558608));
#37009=CARTESIAN_POINT('Ctrl Pts',(63.2297107806181,55.7884527399271,-9.78116499769479));
#37010=CARTESIAN_POINT('Ctrl Pts',(64.831169445826,57.8027446189067,-9.6642483598035));
#37011=CARTESIAN_POINT('Ctrl Pts',(65.2968723721041,60.3335792537041,-9.54733172191222));
#37012=CARTESIAN_POINT('Ctrl Pts',(64.5173398680237,62.7859966304905,-9.43041508402093));
#37013=CARTESIAN_POINT('Ctrl Pts',(62.6758304956081,64.5834554024384,-9.31349844612963));
#37014=CARTESIAN_POINT('Ctrl Pts',(60.205263132424,65.3033953276082,-9.19658180823835));
#37015=CARTESIAN_POINT('Ctrl Pts',(57.6864406181491,64.7765653538453,-9.07966517034705));
#37016=CARTESIAN_POINT('Ctrl Pts',(55.7115103282802,63.1268179703927,-8.96274853245576));
#37017=CARTESIAN_POINT('Ctrl Pts',(54.7447564613263,60.7419901067622,-8.84583189456447));
#37018=CARTESIAN_POINT('Ctrl Pts',(55.0134521769933,58.1827288792718,-8.72891525667318));
#37019=CARTESIAN_POINT('Ctrl Pts',(56.4544300560118,56.0506873938616,-8.6119986187819));
#37020=CARTESIAN_POINT('Ctrl Pts',(58.7289322067895,54.8470867941934,-8.49508198089061));
#37021=CARTESIAN_POINT('Ctrl Pts',(61.3022482494153,54.8548764161609,-8.37816534299932));
#37022=CARTESIAN_POINT('Ctrl Pts',(63.5694203037008,56.0722332749569,-8.26124870510803));
#37023=CARTESIAN_POINT('Ctrl Pts',(64.9974608281321,58.2129524076025,-8.14433206721674));
#37024=CARTESIAN_POINT('Ctrl Pts',(65.250654372306,60.7738129689434,-8.02741542932545));
#37025=CARTESIAN_POINT('Ctrl Pts',(64.2694756368211,63.1527018302866,-7.91049879143416));
#37026=CARTESIAN_POINT('Ctrl Pts',(62.2845938431877,64.7905481022763,-7.79358215354287));
#37027=CARTESIAN_POINT('Ctrl Pts',(59.7626219966935,65.301924603536,-7.67666551565158));
#37028=CARTESIAN_POINT('Ctrl Pts',(57.2964708742581,64.5674491899606,-7.55974887776029));
#37029=CARTESIAN_POINT('Ctrl Pts',(55.4658552065881,62.7579816804522,-7.442832239869));
#37030=CARTESIAN_POINT('Ctrl Pts',(54.7012398189108,60.3028070774634,-7.32591560197771));
#37031=CARTESIAN_POINT('Ctrl Pts',(55.1821425126253,57.7706809218396,-7.20899896408643));
#37032=CARTESIAN_POINT('Ctrl Pts',(56.7959922829326,55.7750204186338,-7.09208232619513));
#37033=CARTESIAN_POINT('Ctrl Pts',(59.9512914978166,54.4027085123842,-6.93619347567342));
#37034=CARTESIAN_POINT('Ctrl Pts',(64.3799881642309,55.9075540482554,-6.74133241252127));
#37035=CARTESIAN_POINT('Ctrl Pts',(65.834479609045,61.37523011834,-6.50749913673868));
#37036=CARTESIAN_POINT('Ctrl Pts',(62.7388658113806,64.8816655541704,-6.31263807358654));
#37037=CARTESIAN_POINT('Ctrl Pts',(59.3187584788532,65.2585195543855,-6.15674922306482));
#37038=CARTESIAN_POINT('Ctrl Pts',(56.9266335796149,64.3285139675122,-6.03983258517353));
#37039=CARTESIAN_POINT('Ctrl Pts',(55.2511526541055,62.3700211957414,-5.92291594728224));
#37040=CARTESIAN_POINT('Ctrl Pts',(54.6947972197688,59.8594460319768,-5.80599930939095));
#37041=CARTESIAN_POINT('Ctrl Pts',(55.3843760081973,57.3795654934784,-5.68908267149966));
#37042=CARTESIAN_POINT('Ctrl Pts',(57.1596209351837,55.5168092181914,-5.57216603360837));
#37043=CARTESIAN_POINT('Ctrl Pts',(59.6023370896801,54.7074973445116,-5.45524939571708));
#37044=CARTESIAN_POINT('Ctrl Pts',(62.138664673409,55.1426278237003,-5.33833275782579));
#37045=CARTESIAN_POINT('Ctrl Pts',(64.1721578471653,56.7195645494213,-5.2214161199345));
#37046=CARTESIAN_POINT('Ctrl Pts',(65.2248497831894,59.0677454356388,-5.10449948204321));
#37047=CARTESIAN_POINT('Ctrl Pts',(65.0492249349093,61.6350658396978,-4.98758284415192));
#37048=CARTESIAN_POINT('Ctrl Pts',(63.6865889794253,63.8180111190031,-4.87066620626063));
#37049=CARTESIAN_POINT('Ctrl Pts',(61.4572740950116,65.1033792767411,-4.75374956836934));
#37050=CARTESIAN_POINT('Ctrl Pts',(58.8853714589078,65.189001781766,-4.63683293047805));
#37051=CARTESIAN_POINT('Ctrl Pts',(56.5755050441849,64.0547463443016,-4.51991629258676));
#37052=CARTESIAN_POINT('Ctrl Pts',(55.0706998168725,61.9672654489506,-4.40299965469547));
#37053=CARTESIAN_POINT('Ctrl Pts',(54.7247182017831,59.4173019594712,-4.28608301680418));
#37054=CARTESIAN_POINT('Ctrl Pts',(55.6188973320329,57.0043245192968,-4.16916637891289));
#37055=CARTESIAN_POINT('Ctrl Pts',(57.5430244185373,55.2955969820173,-4.0522497410216));
#37056=CARTESIAN_POINT('Ctrl Pts',(60.0447608866429,54.6928229271066,-3.93533310313032));
#37057=CARTESIAN_POINT('Ctrl Pts',(62.5359710846191,55.3377065632379,-3.81841646523902));
#37058=CARTESIAN_POINT('Ctrl Pts',(64.4310101049653,57.0786456054826,-3.70149982734774));
#37059=CARTESIAN_POINT('Ctrl Pts',(65.2843515953202,59.5063586001592,-3.58458318945645));
#37060=CARTESIAN_POINT('Ctrl Pts',(64.8954360734807,62.0501294386705,-3.46766655156516));
#37061=CARTESIAN_POINT('Ctrl Pts',(63.3555842661093,64.1119168678935,-3.35074991367387));
#37062=CARTESIAN_POINT('Ctrl Pts',(61.027044706866,65.2070699669712,-3.23383327578258));
#37063=CARTESIAN_POINT('Ctrl Pts',(58.4567442007043,65.0779746991923,-3.11691663789129));
#37064=CARTESIAN_POINT('Ctrl Pts',(56.9857510552448,64.1960675938266,-3.03897221263043));
#37065=CARTESIAN_POINT('Ctrl Pts',(56.3967816198432,63.6078550836889,-3.));
#37066=CARTESIAN_POINT('Ctrl Pts',(56.7766472160421,62.7898325810254,-10.));
#37067=CARTESIAN_POINT('Ctrl Pts',(56.6836916815798,62.7013634565378,-10.));
#37068=CARTESIAN_POINT('Ctrl Pts',(56.5950267759711,62.6087976402809,-10.));
#37069=CARTESIAN_POINT('Ctrl Pts',(56.5107708328057,62.5125537979556,-10.));
#37070=CARTESIAN_POINT('Ctrl Pts',(56.4249559337053,62.414529192119,-10.));
#37071=CARTESIAN_POINT('Ctrl Pts',(56.3437141378064,62.312688781189,-10.));
#37072=CARTESIAN_POINT('Ctrl Pts',(56.2671934014339,62.2074259581361,-10.));
#37073=CARTESIAN_POINT('Ctrl Pts',(56.1895731759036,62.1006506648932,-10.));
#37074=CARTESIAN_POINT('Ctrl Pts',(56.1168100786834,61.9903533919095,-10.));
#37075=CARTESIAN_POINT('Ctrl Pts',(56.0490902779739,61.8769019388278,-10.));
#37076=CARTESIAN_POINT('Ctrl Pts',(55.9815184148182,61.7636983265589,-10.));
#37077=CARTESIAN_POINT('Ctrl Pts',(55.9189673273988,61.6473536561778,-10.));
#37078=CARTESIAN_POINT('Ctrl Pts',(55.8616613826493,61.5281998896676,-10.));
#37079=CARTESIAN_POINT('Ctrl Pts',(55.8501068150877,61.5041749782664,-10.));
#37080=CARTESIAN_POINT('Ctrl Pts',(55.8387656287774,61.4800357739801,-10.));
#37081=CARTESIAN_POINT('Ctrl Pts',(55.8276398866233,61.4557848691785,-10.));
#37082=CARTESIAN_POINT('Ctrl Pts',(55.8174344409603,61.4335399449477,-10.));
#37083=CARTESIAN_POINT('Ctrl Pts',(55.8074083930678,61.4111965365112,-10.));
#37084=CARTESIAN_POINT('Ctrl Pts',(55.7975752706419,61.3887843305408,-10.));
#37085=CARTESIAN_POINT('Ctrl Pts',(55.7403627711479,61.2583823821857,-10.));
#37086=CARTESIAN_POINT('Ctrl Pts',(55.6896031187019,61.1254984802314,-10.));
#37087=CARTESIAN_POINT('Ctrl Pts',(55.645479920562,60.9906068936445,-10.));
#37088=CARTESIAN_POINT('Ctrl Pts',(55.6039768116069,60.863725333575,-10.));
#37089=CARTESIAN_POINT('Ctrl Pts',(55.5683448579499,60.7350665035816,-10.));
#37090=CARTESIAN_POINT('Ctrl Pts',(55.5385236905657,60.6050521672458,-10.));
#37091=CARTESIAN_POINT('Ctrl Pts',(55.5083230209178,60.4733832768034,-10.));
#37092=CARTESIAN_POINT('Ctrl Pts',(55.4840817318274,60.3403234669823,-10.));
#37093=CARTESIAN_POINT('Ctrl Pts',(55.4657841380372,60.2062855830499,-10.));
#37094=CARTESIAN_POINT('Ctrl Pts',(55.4495746406316,60.0875439191587,-10.));
#37095=CARTESIAN_POINT('Ctrl Pts',(55.4380302645887,59.9680339642758,-10.));
#37096=CARTESIAN_POINT('Ctrl Pts',(55.4311725531702,59.8480333617552,-10.));
#37097=CARTESIAN_POINT('Ctrl Pts',(55.429455905751,59.8179943717717,-10.));
#37098=CARTESIAN_POINT('Ctrl Pts',(55.4280330868615,59.7879246126589,-10.));
#37099=CARTESIAN_POINT('Ctrl Pts',(55.4269047438418,59.7578284042711,-10.));
#37100=CARTESIAN_POINT('Ctrl Pts',(55.42609738417,59.7362937605487,-10.));
#37101=CARTESIAN_POINT('Ctrl Pts',(55.4254408285579,59.7147438446829,-10.));
#37102=CARTESIAN_POINT('Ctrl Pts',(55.4249356300217,59.6932018270316,-10.));
#37103=CARTESIAN_POINT('Ctrl Pts',(55.4216903829473,59.5548222301979,-10.));
#37104=CARTESIAN_POINT('Ctrl Pts',(55.4246781614053,59.4165725060038,-10.));
#37105=CARTESIAN_POINT('Ctrl Pts',(55.4338328579124,59.2788933768414,-10.));
#37106=CARTESIAN_POINT('Ctrl Pts',(55.4430905358525,59.139665491367,-10.));
#37107=CARTESIAN_POINT('Ctrl Pts',(55.4586544403344,59.0010203364085,-10.));
#37108=CARTESIAN_POINT('Ctrl Pts',(55.4805057053574,58.8633952047768,-10.));
#37109=CARTESIAN_POINT('Ctrl Pts',(55.485322464481,58.8330579630784,-10.));
#37110=CARTESIAN_POINT('Ctrl Pts',(55.4904449293029,58.8027702410737,-10.));
#37111=CARTESIAN_POINT('Ctrl Pts',(55.4958732326893,58.7725366629253,-10.));
#37112=CARTESIAN_POINT('Ctrl Pts',(55.5203481259231,58.6362208484638,-10.));
#37113=CARTESIAN_POINT('Ctrl Pts',(55.551036175231,58.5010055472366,-10.));
#37114=CARTESIAN_POINT('Ctrl Pts',(55.5877252511952,58.3672429184636,-10.));
#37115=CARTESIAN_POINT('Ctrl Pts',(55.6089636892506,58.2898108973326,-10.));
#37116=CARTESIAN_POINT('Ctrl Pts',(55.6322140471996,58.2128656730071,-10.));
#37117=CARTESIAN_POINT('Ctrl Pts',(55.6574430346149,58.136476625185,-10.));
#37118=CARTESIAN_POINT('Ctrl Pts',(55.6711730594046,58.0949044644403,-10.));
#37119=CARTESIAN_POINT('Ctrl Pts',(55.6854891955254,58.0534970476954,-10.));
#37120=CARTESIAN_POINT('Ctrl Pts',(55.7003867655987,58.0122657515545,-10.));
#37121=CARTESIAN_POINT('Ctrl Pts',(55.7064544678847,57.9954724605263,-10.));
#37122=CARTESIAN_POINT('Ctrl Pts',(55.7126186291905,57.9787083878453,-10.));
#37123=CARTESIAN_POINT('Ctrl Pts',(55.7188789560352,57.9619743104561,-10.));
#37124=CARTESIAN_POINT('Ctrl Pts',(55.7254264843682,57.9444725332243,-10.));
#37125=CARTESIAN_POINT('Ctrl Pts',(55.7320759675732,57.9270122449326,-10.));
#37126=CARTESIAN_POINT('Ctrl Pts',(55.7388258598846,57.9095965174206,-10.));
#37127=CARTESIAN_POINT('Ctrl Pts',(55.7901008092709,57.7772995109641,-10.));
#37128=CARTESIAN_POINT('Ctrl Pts',(55.8471813531683,57.647531798479,-10.));
#37129=CARTESIAN_POINT('Ctrl Pts',(55.9097891914145,57.5206512582104,-10.));
#37130=CARTESIAN_POINT('Ctrl Pts',(55.9730108624179,57.3925267294244,-10.));
#37131=CARTESIAN_POINT('Ctrl Pts',(56.0418689194203,57.2673455178894,-10.));
#37132=CARTESIAN_POINT('Ctrl Pts',(56.1161301251681,57.1454790677295,-10.));
#37133=CARTESIAN_POINT('Ctrl Pts',(56.1904609341748,57.0234983950494,-10.));
#37134=CARTESIAN_POINT('Ctrl Pts',(56.2702052813482,56.9048379308472,-10.));
#37135=CARTESIAN_POINT('Ctrl Pts',(56.3551790628638,56.7898845039161,-10.));
#37136=CARTESIAN_POINT('Ctrl Pts',(56.3877839571239,56.7457762594309,-10.));
#37137=CARTESIAN_POINT('Ctrl Pts',(56.4211592802161,56.7022140122855,-10.));
#37138=CARTESIAN_POINT('Ctrl Pts',(56.4552964526868,56.6592205467288,-10.));
#37139=CARTESIAN_POINT('Ctrl Pts',(56.5184577159342,56.5796731970391,-10.));
#37140=CARTESIAN_POINT('Ctrl Pts',(56.5842264250915,56.502072454838,-10.));
#37141=CARTESIAN_POINT('Ctrl Pts',(56.6524865794293,56.4265028368199,-10.));
#37142=CARTESIAN_POINT('Ctrl Pts',(56.6665323443044,56.4109530172116,-10.));
#37143=CARTESIAN_POINT('Ctrl Pts',(56.6806836330993,56.3954892252364,-10.));
#37144=CARTESIAN_POINT('Ctrl Pts',(56.6949394878897,56.3801122433927,-10.));
#37145=CARTESIAN_POINT('Ctrl Pts',(56.7093516312862,56.3645666818957,-10.));
#37146=CARTESIAN_POINT('Ctrl Pts',(56.7238639781207,56.3491170502204,-10.));
#37147=CARTESIAN_POINT('Ctrl Pts',(56.7384737535074,56.3337654700224,-10.));
#37148=CARTESIAN_POINT('Ctrl Pts',(56.838104851128,56.229075647979,-10.));
#37149=CARTESIAN_POINT('Ctrl Pts',(56.9422847841482,56.1289203917598,-10.));
#37150=CARTESIAN_POINT('Ctrl Pts',(57.0506144838166,56.0334961807761,-10.));
#37151=CARTESIAN_POINT('Ctrl Pts',(57.1492676318998,55.9465957384623,-10.));
#37152=CARTESIAN_POINT('Ctrl Pts',(57.2513631973246,55.8636188452892,-10.));
#37153=CARTESIAN_POINT('Ctrl Pts',(57.3566308813066,55.7847333558599,-10.));
#37154=CARTESIAN_POINT('Ctrl Pts',(57.4121395358538,55.7431362843193,-10.));
#37155=CARTESIAN_POINT('Ctrl Pts',(57.4685306777316,55.7026771906877,-10.));
#37156=CARTESIAN_POINT('Ctrl Pts',(57.5257674930296,55.663383235408,-10.));
#37157=CARTESIAN_POINT('Ctrl Pts',(57.5474706288127,55.648483698415,-10.));
#37158=CARTESIAN_POINT('Ctrl Pts',(57.569295372594,55.6337517029334,-10.));
#37159=CARTESIAN_POINT('Ctrl Pts',(57.5912397820617,55.6191888039281,-10.));
#37160=CARTESIAN_POINT('Ctrl Pts',(57.6130039682011,55.6047455059597,-10.));
#37161=CARTESIAN_POINT('Ctrl Pts',(57.6348798477783,55.590472576591,-10.));
#37162=CARTESIAN_POINT('Ctrl Pts',(57.6568590240097,55.5763752246629,-10.));
#37163=CARTESIAN_POINT('Ctrl Pts',(57.782190594167,55.4959880785018,-10.));
#37164=CARTESIAN_POINT('Ctrl Pts',(57.910939943541,55.4212659189356,-10.));
#37165=CARTESIAN_POINT('Ctrl Pts',(58.0427132794917,55.3524362848689,-10.));
#37166=CARTESIAN_POINT('Ctrl Pts',(58.1526798140915,55.294997074717,-10.));
#37167=CARTESIAN_POINT('Ctrl Pts',(58.2647532542174,55.2416618501413,-10.));
#37168=CARTESIAN_POINT('Ctrl Pts',(58.3787241380444,55.1925827330161,-10.));
#37169=CARTESIAN_POINT('Ctrl Pts',(58.4767840492774,55.1503553350432,-10.));
#37170=CARTESIAN_POINT('Ctrl Pts',(58.5762489664664,55.1112788488363,-10.));
#37171=CARTESIAN_POINT('Ctrl Pts',(58.6769607112098,55.0753649997562,-10.));
#37172=CARTESIAN_POINT('Ctrl Pts',(64.2628730117989,60.0000978162778,-7.57968167058906));
#37173=CARTESIAN_POINT('Ctrl Pts',(64.2624542514066,59.5120606486749,-7.60701019445078));
#37174=CARTESIAN_POINT('Ctrl Pts',(64.1786779666622,59.0238810355797,-7.63433871831249));
#37175=CARTESIAN_POINT('Ctrl Pts',(64.0144041441174,58.56448844846,-7.66166724217421));
#37176=CARTESIAN_POINT('Ctrl Pts',(63.7801392283017,57.909365410104,-7.70063945480464));
#37177=CARTESIAN_POINT('Ctrl Pts',(63.3821699038818,57.3127853184214,-7.73961166743507));
#37178=CARTESIAN_POINT('Ctrl Pts',(62.8672751132997,56.8448674929813,-7.7785838800655));
#37179=CARTESIAN_POINT('Ctrl Pts',(62.3523803227176,56.3769496675411,-7.81755609269593));
#37180=CARTESIAN_POINT('Ctrl Pts',(61.7205600659731,56.0376941083434,-7.85652830532636));
#37181=CARTESIAN_POINT('Ctrl Pts',(61.0460813852798,55.8669809146618,-7.89550051795679));
#37182=CARTESIAN_POINT('Ctrl Pts',(60.3716027045864,55.6962677209802,-7.93447273058722));
#37183=CARTESIAN_POINT('Ctrl Pts',(59.6544655999441,55.6940968928147,-7.97344494321765));
#37184=CARTESIAN_POINT('Ctrl Pts',(58.9789655359289,55.8607224467775,-8.01241715584808));
#37185=CARTESIAN_POINT('Ctrl Pts',(58.3034654719138,56.0273480007403,-8.05138936847851));
#37186=CARTESIAN_POINT('Ctrl Pts',(57.6696024485259,56.3627699368315,-8.09036158110894));
#37187=CARTESIAN_POINT('Ctrl Pts',(57.1518835700849,56.8275617982647,-8.12933379373937));
#37188=CARTESIAN_POINT('Ctrl Pts',(56.634164691644,57.292353659698,-8.1683060063698));
#37189=CARTESIAN_POINT('Ctrl Pts',(56.2325899581502,57.8865154464734,-8.20727821900023));
#37190=CARTESIAN_POINT('Ctrl Pts',(55.9943622489868,58.5402064795222,-8.24625043163065));
#37191=CARTESIAN_POINT('Ctrl Pts',(55.7561345398234,59.193897512571,-8.28522264426108));
#37192=CARTESIAN_POINT('Ctrl Pts',(55.6812538549906,59.9071177918932,-8.32419485689152));
#37193=CARTESIAN_POINT('Ctrl Pts',(55.7785220088422,60.5960323436173,-8.36316706952195));
#37194=CARTESIAN_POINT('Ctrl Pts',(55.8757901626938,61.2849468953415,-8.40213928215238));
#37195=CARTESIAN_POINT('Ctrl Pts',(56.1452071552299,61.9495557194676,-8.44111149478281));
#37196=CARTESIAN_POINT('Ctrl Pts',(56.555104506362,62.5117376596622,-8.48008370741324));
#37197=CARTESIAN_POINT('Ctrl Pts',(56.9650018574941,63.0739195998569,-8.51905592004367));
#37198=CARTESIAN_POINT('Ctrl Pts',(57.5153795672222,63.5336746561201,-8.5580281326741));
#37199=CARTESIAN_POINT('Ctrl Pts',(58.1415437890979,63.836961224526,-8.59700034530453));
#37200=CARTESIAN_POINT('Ctrl Pts',(58.7677080109736,64.1402477929319,-8.63597255793496));
#37201=CARTESIAN_POINT('Ctrl Pts',(59.4696587449968,64.2870658734804,-8.67494477056539));
#37202=CARTESIAN_POINT('Ctrl Pts',(60.1648855557312,64.2601577306143,-8.71391698319582));
#37203=CARTESIAN_POINT('Ctrl Pts',(60.8601123664656,64.2332495877481,-8.75288919582625));
#37204=CARTESIAN_POINT('Ctrl Pts',(61.5486152539111,64.0326152214672,-8.79186140845667));
#37205=CARTESIAN_POINT('Ctrl Pts',(62.149464542133,63.6818382506294,-8.8308336210871));
#37206=CARTESIAN_POINT('Ctrl Pts',(62.750313830355,63.3310612797916,-8.86980583371753));
#37207=CARTESIAN_POINT('Ctrl Pts',(63.2635095193533,62.8301417043968,-8.90877804634796));
#37208=CARTESIAN_POINT('Ctrl Pts',(63.6287282393475,62.2379595110891,-8.94775025897839));
#37209=CARTESIAN_POINT('Ctrl Pts',(63.9939469593417,61.6457773177814,-8.98672247160882));
#37210=CARTESIAN_POINT('Ctrl Pts',(64.2111887103318,60.9623325065609,-9.02569468423925));
#37211=CARTESIAN_POINT('Ctrl Pts',(64.2549180523652,60.2679609524856,-9.06466689686968));
#37212=CARTESIAN_POINT('Ctrl Pts',(64.2605339012929,60.1787877436963,-9.06967182144281));
#37213=CARTESIAN_POINT('Ctrl Pts',(64.2632881070018,60.089434326242,-9.07467674601593));
#37214=CARTESIAN_POINT('Ctrl Pts',(64.2632129797225,60.0000762878951,-9.07968167058906));
#37215=CARTESIAN_POINT('Ctrl Pts',(61.322884965569,55.0755938055567,-10.));
#37216=CARTESIAN_POINT('Ctrl Pts',(62.1267766598728,55.2915500435982,-9.96102778736957));
#37217=CARTESIAN_POINT('Ctrl Pts',(63.6260271731292,56.1245140078271,-9.88308336210872));
#37218=CARTESIAN_POINT('Ctrl Pts',(65.0229772277616,58.2859118284941,-9.76616672421742));
#37219=CARTESIAN_POINT('Ctrl Pts',(65.2388166032808,60.8500628014955,-9.64925008632614));
#37220=CARTESIAN_POINT('Ctrl Pts',(64.2231822164303,63.2145072853594,-9.53233344843484));
#37221=CARTESIAN_POINT('Ctrl Pts',(62.2146698080337,64.8232034325914,-9.41541681054355));
#37222=CARTESIAN_POINT('Ctrl Pts',(59.6855379323249,65.2980445186201,-9.29850017265226));
#37223=CARTESIAN_POINT('Ctrl Pts',(57.2303209838473,64.5273621068898,-9.18158353476097));
#37224=CARTESIAN_POINT('Ctrl Pts',(55.4262302676069,62.6923526051193,-9.06466689686969));
#37225=CARTESIAN_POINT('Ctrl Pts',(54.6973796845391,60.2243982381535,-8.94775025897839));
#37226=CARTESIAN_POINT('Ctrl Pts',(55.2151175810578,57.7036915329656,-8.8308336210871));
#37227=CARTESIAN_POINT('Ctrl Pts',(56.8577278151099,55.7228209598733,-8.71391698319582));
#37228=CARTESIAN_POINT('Ctrl Pts',(59.2390517104132,54.7474680995942,-8.59700034530453));
#37229=CARTESIAN_POINT('Ctrl Pts',(61.799265976347,55.0069271683894,-8.48008370741324));
#37230=CARTESIAN_POINT('Ctrl Pts',(63.9364928560947,56.4402025290253,-8.36316706952195));
#37231=CARTESIAN_POINT('Ctrl Pts',(65.1482936744543,58.7103466239862,-8.24625043163065));
#37232=CARTESIAN_POINT('Ctrl Pts',(65.1497879909792,61.2836744162533,-8.12933379373937));
#37233=CARTESIAN_POINT('Ctrl Pts',(63.9406234579031,63.5552235763429,-8.01241715584808));
#37234=CARTESIAN_POINT('Ctrl Pts',(61.8050635087969,64.9909811652868,-7.89550051795679));
#37235=CARTESIAN_POINT('Ctrl Pts',(59.2451498198411,65.2534097530527,-7.7785838800655));
#37236=CARTESIAN_POINT('Ctrl Pts',(56.8627001620859,64.2808297817029,-7.66166724217421));
#37237=CARTESIAN_POINT('Ctrl Pts',(55.2177796069362,62.3018527370191,-7.54475060428292));
#37238=CARTESIAN_POINT('Ctrl Pts',(54.6971392652592,59.7817817811634,-7.42783396639163));
#37239=CARTESIAN_POINT('Ctrl Pts',(55.4230712085558,57.3129118130677,-7.31091732850034));
#37240=CARTESIAN_POINT('Ctrl Pts',(57.2251429658425,55.4759618040439,-7.19400069060905));
#37241=CARTESIAN_POINT('Ctrl Pts',(59.6792193933806,54.7020984074429,-7.07708405271776));
#37242=CARTESIAN_POINT('Ctrl Pts',(62.2094284211809,55.174716747074,-6.96016741482647));
#37243=CARTESIAN_POINT('Ctrl Pts',(64.2186721193591,56.7795408043723,-6.84325077693519));
#37244=CARTESIAN_POINT('Ctrl Pts',(65.2395171494002,59.1461424584795,-6.72633413904389));
#37245=CARTESIAN_POINT('Ctrl Pts',(65.0214070657763,61.7034072624198,-6.60941750115261));
#37246=CARTESIAN_POINT('Ctrl Pts',(63.1773281761085,64.6083211110609,-6.45352865063088));
#37247=CARTESIAN_POINT('Ctrl Pts',(58.6661397561353,65.8440762220129,-6.25866758747874));
#37248=CARTESIAN_POINT('Ctrl Pts',(54.3971986841152,62.1309686655549,-6.02483431169616));
#37249=CARTESIAN_POINT('Ctrl Pts',(54.9957816802558,57.4920452935348,-5.82997324854401));
#37250=CARTESIAN_POINT('Ctrl Pts',(57.6170719268681,55.2631467174745,-5.67408439802229));
#37251=CARTESIAN_POINT('Ctrl Pts',(60.1194257717932,54.6927078330755,-5.557167760131));
#37252=CARTESIAN_POINT('Ctrl Pts',(62.6046743394157,55.3756921094109,-5.44025112223971));
#37253=CARTESIAN_POINT('Ctrl Pts',(64.4724884051625,57.1431171033903,-5.32333448434842));
#37254=CARTESIAN_POINT('Ctrl Pts',(65.2912292886472,59.5834017558471,-5.20641784645713));
#37255=CARTESIAN_POINT('Ctrl Pts',(64.8649668293915,62.1210494825228,-5.08950120856584));
#37256=CARTESIAN_POINT('Ctrl Pts',(63.2955109480772,64.1603278329295,-4.97258457067455));
#37257=CARTESIAN_POINT('Ctrl Pts',(60.9510823128121,65.2214359708436,-4.85566793278326));
#37258=CARTESIAN_POINT('Ctrl Pts',(58.3831734117936,65.0550993752034,-4.73875129489197));
#37259=CARTESIAN_POINT('Ctrl Pts',(56.1953122098592,63.7003384596412,-4.62183465700068));
#37260=CARTESIAN_POINT('Ctrl Pts',(54.9019142936214,61.4756811820325,-4.50491801910939));
#37261=CARTESIAN_POINT('Ctrl Pts',(54.8070090801581,58.9041019292639,-4.3880013812181));
#37262=CARTESIAN_POINT('Ctrl Pts',(55.9329235426593,56.5901588022821,-4.27108474332681));
#37263=CARTESIAN_POINT('Ctrl Pts',(58.0149603175651,55.0778303762239,-4.15416810543552));
#37264=CARTESIAN_POINT('Ctrl Pts',(60.5636590493342,54.7226500811105,-4.03725146754424));
#37265=CARTESIAN_POINT('Ctrl Pts',(62.9798472108349,55.6081160860788,-3.92033482965294));
#37266=CARTESIAN_POINT('Ctrl Pts',(64.6955066712587,57.5260654357952,-3.80341819176166));
#37267=CARTESIAN_POINT('Ctrl Pts',(65.3073040613093,60.0256094769815,-3.68650155387036));
#37268=CARTESIAN_POINT('Ctrl Pts',(64.6714138007994,62.5191327746011,-3.56958491597908));
#37269=CARTESIAN_POINT('Ctrl Pts',(62.93732429588,64.4204364118546,-3.45266827808779));
#37270=CARTESIAN_POINT('Ctrl Pts',(60.5127057455321,65.2825431684356,-3.3357516401965));
#37271=CARTESIAN_POINT('Ctrl Pts',(57.967548471337,64.9027852181516,-3.2188350023052));
#37272=CARTESIAN_POINT('Ctrl Pts',(55.9002137011895,63.3704311318214,-3.10191836441392));
#37273=CARTESIAN_POINT('Ctrl Pts',(54.7966592622721,61.0457391111864,-2.98500172652262));
#37274=CARTESIAN_POINT('Ctrl Pts',(54.9164250447544,58.4751813736776,-2.86808508863134));
#37275=CARTESIAN_POINT('Ctrl Pts',(56.2311219607459,56.2631621903272,-2.75116845074005));
#37276=CARTESIAN_POINT('Ctrl Pts',(58.4321699151165,54.9295588396458,-2.63425181284876));
#37277=CARTESIAN_POINT('Ctrl Pts',(60.1446943002093,54.8355306649757,-2.5563073875879));
#37278=CARTESIAN_POINT('Ctrl Pts',(60.9621351249183,54.9925957821044,-2.51733517495747));
#37279=CARTESIAN_POINT('Ctrl Pts',(61.2505876634042,55.344718704462,-10.1608882750142));
#37280=CARTESIAN_POINT('Ctrl Pts',(62.0105456807492,55.5488726665669,-10.1219160623837));
#37281=CARTESIAN_POINT('Ctrl Pts',(63.4278602961771,56.3363141182708,-10.0439716371229));
#37282=CARTESIAN_POINT('Ctrl Pts',(64.7484652997752,58.3795888704878,-9.9270549992316));
#37283=CARTESIAN_POINT('Ctrl Pts',(64.9525087860393,60.8036058163318,-9.81013836134031));
#37284=CARTESIAN_POINT('Ctrl Pts',(63.9923800766032,63.0388304800668,-9.69322172344902));
#37285=CARTESIAN_POINT('Ctrl Pts',(62.0936353594806,64.5596093899918,-9.57630508555773));
#37286=CARTESIAN_POINT('Ctrl Pts',(59.7027236738805,65.0084998224335,-9.45938844766644));
#37287=CARTESIAN_POINT('Ctrl Pts',(57.3816873731722,64.2799361592295,-9.34247180977515));
#37288=CARTESIAN_POINT('Ctrl Pts',(55.6761924494909,62.5452121999497,-9.22555517188386));
#37289=CARTESIAN_POINT('Ctrl Pts',(54.9871744536915,60.2121345964527,-9.10863853399257));
#37290=CARTESIAN_POINT('Ctrl Pts',(55.4766173327892,57.8291876353675,-8.99172189610128));
#37291=CARTESIAN_POINT('Ctrl Pts',(57.0294568826766,55.9565740930069,-8.87480525820999));
#37292=CARTESIAN_POINT('Ctrl Pts',(59.2806384771057,55.0345254748142,-8.7578886203187));
#37293=CARTESIAN_POINT('Ctrl Pts',(61.7009338617999,55.2798047840805,-8.64097198242741));
#37294=CARTESIAN_POINT('Ctrl Pts',(63.7213586449621,56.634749870709,-8.52405534453613));
#37295=CARTESIAN_POINT('Ctrl Pts',(64.8669330474135,58.7808277786144,-8.40713870664483));
#37296=CARTESIAN_POINT('Ctrl Pts',(64.8683456976891,61.2135200191828,-8.29022206875355));
#37297=CARTESIAN_POINT('Ctrl Pts',(63.7252635042647,63.3609262036671,-8.17330543086225));
#37298=CARTESIAN_POINT('Ctrl Pts',(61.7064145519195,64.7182178617515,-8.05638879297097));
#37299=CARTESIAN_POINT('Ctrl Pts',(59.2864033172989,64.9663044020981,-7.93947215507967));
#37300=CARTESIAN_POINT('Ctrl Pts',(57.0341574847307,64.0468771310195,-7.82255551718839));
#37301=CARTESIAN_POINT('Ctrl Pts',(55.4791338756556,62.1760536333943,-7.7056388792971));
#37302=CARTESIAN_POINT('Ctrl Pts',(54.9869471736231,59.7937076771527,-7.58872224140581));
#37303=CARTESIAN_POINT('Ctrl Pts',(55.6732060369304,57.4597645112618,-7.47180560351452));
#37304=CARTESIAN_POINT('Ctrl Pts',(57.3767923402659,55.723206095854,-7.35488896562323));
#37305=CARTESIAN_POINT('Ctrl Pts',(59.696750450917,54.9916352925431,-7.23797232773193));
#37306=CARTESIAN_POINT('Ctrl Pts',(62.0886804209124,55.4384244544314,-7.12105568984065));
#37307=CARTESIAN_POINT('Ctrl Pts',(63.988116461924,56.9555428889342,-7.00413905194936));
#37308=CARTESIAN_POINT('Ctrl Pts',(64.9531710464455,59.1928068308866,-6.88722241405807));
#37309=CARTESIAN_POINT('Ctrl Pts',(64.7469809490875,61.6103139453392,-6.77030577616678));
#37310=CARTESIAN_POINT('Ctrl Pts',(63.0036832551942,64.3564706535303,-6.61441692564506));
#37311=CARTESIAN_POINT('Ctrl Pts',(58.7390368708552,65.5246902168091,-6.41955586249291));
#37312=CARTESIAN_POINT('Ctrl Pts',(54.7033987168066,62.0145085881277,-6.18572258671033));
#37313=CARTESIAN_POINT('Ctrl Pts',(55.2692684106804,57.6291081251099,-5.99086152355818));
#37314=CARTESIAN_POINT('Ctrl Pts',(57.747301898048,55.522021617402,-5.83497267303646));
#37315=CARTESIAN_POINT('Ctrl Pts',(60.1128990054194,54.9827579246979,-5.71805603514517));
#37316=CARTESIAN_POINT('Ctrl Pts',(62.462325660083,55.6284162642473,-5.60113939725389));
#37317=CARTESIAN_POINT('Ctrl Pts',(64.2280613732794,57.2992492928108,-5.48422275936259));
#37318=CARTESIAN_POINT('Ctrl Pts',(65.0020570532214,59.6061693659741,-5.36730612147131));
#37319=CARTESIAN_POINT('Ctrl Pts',(64.59909036542,62.0051315007363,-5.25038948358001));
#37320=CARTESIAN_POINT('Ctrl Pts',(63.1154071922693,63.9329607630251,-5.13347284568873));
#37321=CARTESIAN_POINT('Ctrl Pts',(60.8991044862114,64.9360780266961,-5.01655620779744));
#37322=CARTESIAN_POINT('Ctrl Pts',(58.4715349877719,64.7788319320662,-4.89963956990615));
#37323=CARTESIAN_POINT('Ctrl Pts',(56.4032431108567,63.498110378824,-4.78272293201486));
#37324=CARTESIAN_POINT('Ctrl Pts',(55.180530993009,61.3950333773531,-4.66580629412357));
#37325=CARTESIAN_POINT('Ctrl Pts',(55.0908124670305,58.9639941164336,-4.54888965623228));
#37326=CARTESIAN_POINT('Ctrl Pts',(56.1551943093676,56.7765108478657,-4.43197301834099));
#37327=CARTESIAN_POINT('Ctrl Pts',(58.1234451952872,55.3468330437716,-4.3150563804497));
#37328=CARTESIAN_POINT('Ctrl Pts',(60.5328543840245,55.0110637917852,-4.19813974255841));
#37329=CARTESIAN_POINT('Ctrl Pts',(62.8169948693132,55.8481379826623,-4.08122310466712));
#37330=CARTESIAN_POINT('Ctrl Pts',(64.4388914148573,57.6612690244515,-3.96430646677583));
#37331=CARTESIAN_POINT('Ctrl Pts',(65.017253319644,60.0242098873393,-3.84738982888454));
#37332=CARTESIAN_POINT('Ctrl Pts',(64.416115249615,62.3814590477548,-3.73047319099325));
#37333=CARTESIAN_POINT('Ctrl Pts',(62.7767958843382,64.178854085888,-3.61355655310196));
#37334=CARTESIAN_POINT('Ctrl Pts',(60.4846857413964,64.9938456402397,-3.49663991521067));
#37335=CARTESIAN_POINT('Ctrl Pts',(58.0786244651895,64.6348419323848,-3.37972327731938));
#37336=CARTESIAN_POINT('Ctrl Pts',(56.1242721012553,63.1862328951605,-3.26280663942809));
#37337=CARTESIAN_POINT('Ctrl Pts',(55.0810282795134,60.9885881732933,-3.1458900015368));
#37338=CARTESIAN_POINT('Ctrl Pts',(55.1942487136166,58.558514600559,-3.02897336364552));
#37339=CARTESIAN_POINT('Ctrl Pts',(56.437095814496,56.4673850058392,-2.91205672575423));
#37340=CARTESIAN_POINT('Ctrl Pts',(58.5178537714911,55.206664730347,-2.79514008786294));
#37341=CARTESIAN_POINT('Ctrl Pts',(60.1367865774548,55.1177753119051,-2.71719566260207));
#37342=CARTESIAN_POINT('Ctrl Pts',(60.9095532484437,55.2662566258098,-2.67822344997165));
#37343=CARTESIAN_POINT('Ctrl Pts',(61.1782903612393,55.6138436033673,-10.3217765500284));
#37344=CARTESIAN_POINT('Ctrl Pts',(61.8943147016256,55.8061952895356,-10.2828043373979));
#37345=CARTESIAN_POINT('Ctrl Pts',(63.229693419225,56.5481142287144,-10.2048599121371));
#37346=CARTESIAN_POINT('Ctrl Pts',(64.4739533717888,58.4732659124817,-10.0879432742458));
#37347=CARTESIAN_POINT('Ctrl Pts',(64.6662009687979,60.757148831168,-9.97102663635449));
#37348=CARTESIAN_POINT('Ctrl Pts',(63.761577936776,62.8631536747742,-9.85410999846319));
#37349=CARTESIAN_POINT('Ctrl Pts',(61.9726009109276,64.2960153473921,-9.7371933605719));
#37350=CARTESIAN_POINT('Ctrl Pts',(59.7199094154362,64.7189551262469,-9.62027672268062));
#37351=CARTESIAN_POINT('Ctrl Pts',(57.5330537624972,64.0325102115692,-9.50336008478933));
#37352=CARTESIAN_POINT('Ctrl Pts',(55.926154631375,62.3980717947801,-9.38644344689803));
#37353=CARTESIAN_POINT('Ctrl Pts',(55.276969222844,60.199870954752,-9.26952680900675));
#37354=CARTESIAN_POINT('Ctrl Pts',(55.7381170845207,57.9546837377693,-9.15261017111545));
#37355=CARTESIAN_POINT('Ctrl Pts',(57.2011859502433,56.1903272261406,-9.03569353322417));
#37356=CARTESIAN_POINT('Ctrl Pts',(59.3222252437981,55.3215828500341,-8.91877689533288));
#37357=CARTESIAN_POINT('Ctrl Pts',(61.6026017472529,55.5526823997716,-8.80186025744159));
#37358=CARTESIAN_POINT('Ctrl Pts',(63.5062244338295,56.8292972123926,-8.6849436195503));
#37359=CARTESIAN_POINT('Ctrl Pts',(64.5855724203726,58.8513089332426,-8.56802698165901));
#37360=CARTESIAN_POINT('Ctrl Pts',(64.586903404399,61.1433656221122,-8.45111034376773));
#37361=CARTESIAN_POINT('Ctrl Pts',(63.5099035506263,63.1666288309912,-8.33419370587642));
#37362=CARTESIAN_POINT('Ctrl Pts',(61.607765595042,64.4454545582162,-8.21727706798515));
#37363=CARTESIAN_POINT('Ctrl Pts',(59.3276568147568,64.6791990511435,-8.10036043009385));
#37364=CARTESIAN_POINT('Ctrl Pts',(57.2056148073754,63.8129244803361,-7.98344379220256));
#37365=CARTESIAN_POINT('Ctrl Pts',(55.740488144375,62.0502545297695,-7.86652715431127));
#37366=CARTESIAN_POINT('Ctrl Pts',(55.2767550819871,59.8056335731419,-7.74961051641998));
#37367=CARTESIAN_POINT('Ctrl Pts',(55.9233408653051,57.6066172094559,-7.63269387852869));
#37368=CARTESIAN_POINT('Ctrl Pts',(57.5284417146894,55.9704503876641,-7.51577724063741));
#37369=CARTESIAN_POINT('Ctrl Pts',(59.7142815084534,55.2811721776433,-7.39886060274611));
#37370=CARTESIAN_POINT('Ctrl Pts',(61.9679324206439,55.7021321617888,-7.28194396485482));
#37371=CARTESIAN_POINT('Ctrl Pts',(63.757560804489,57.1315449734963,-7.16502732696353));
#37372=CARTESIAN_POINT('Ctrl Pts',(64.6668249434908,59.2394712032937,-7.04811068907225));
#37373=CARTESIAN_POINT('Ctrl Pts',(64.4725548323986,61.5172206282585,-6.93119405118096));
#37374=CARTESIAN_POINT('Ctrl Pts',(62.8300383342798,64.1046201959996,-6.77530520065924));
#37375=CARTESIAN_POINT('Ctrl Pts',(58.8119339855751,65.2053042116052,-6.58044413750709));
#37376=CARTESIAN_POINT('Ctrl Pts',(55.0095987494979,61.8980485107005,-6.34661086172451));
#37377=CARTESIAN_POINT('Ctrl Pts',(55.5427551411051,57.7661709566851,-6.15174979857236));
#37378=CARTESIAN_POINT('Ctrl Pts',(57.8775318692278,55.7808965173295,-5.99586094805064));
#37379=CARTESIAN_POINT('Ctrl Pts',(60.1063722390457,55.2728080163204,-5.87894431015935));
#37380=CARTESIAN_POINT('Ctrl Pts',(62.3199769807503,55.8811404190837,-5.76202767226806));
#37381=CARTESIAN_POINT('Ctrl Pts',(63.9836343413963,57.4553814822313,-5.64511103437677));
#37382=CARTESIAN_POINT('Ctrl Pts',(64.7128848177956,59.628936976101,-5.52819439648548));
#37383=CARTESIAN_POINT('Ctrl Pts',(64.3332139014486,61.8892135189497,-5.41127775859419));
#37384=CARTESIAN_POINT('Ctrl Pts',(62.9353034364615,63.7055936931205,-5.29436112070291));
#37385=CARTESIAN_POINT('Ctrl Pts',(60.8471266596107,64.6507200825485,-5.17744448281161));
#37386=CARTESIAN_POINT('Ctrl Pts',(58.5598965637503,64.502564488929,-5.06052784492033));
#37387=CARTESIAN_POINT('Ctrl Pts',(56.6111740118541,63.2958822980069,-4.94361120702903));
#37388=CARTESIAN_POINT('Ctrl Pts',(55.4591476923966,61.3143855726739,-4.82669456913774));
#37389=CARTESIAN_POINT('Ctrl Pts',(55.374615853903,59.0238863036033,-4.70977793124645));
#37390=CARTESIAN_POINT('Ctrl Pts',(56.3774650760759,56.9628628934493,-4.59286129335516));
#37391=CARTESIAN_POINT('Ctrl Pts',(58.2319300730093,55.6158357113192,-4.47594465546387));
#37392=CARTESIAN_POINT('Ctrl Pts',(60.5020497187147,55.29947750246,-4.35902801757259));
#37393=CARTESIAN_POINT('Ctrl Pts',(62.6541425277914,56.0881598792458,-4.2421113796813));
#37394=CARTESIAN_POINT('Ctrl Pts',(64.1822761584559,57.7964726131078,-4.12519474179001));
#37395=CARTESIAN_POINT('Ctrl Pts',(64.7272025779786,60.0228102976971,-4.00827810389872));
#37396=CARTESIAN_POINT('Ctrl Pts',(64.1608166984306,62.2437853209086,-3.89136146600743));
#37397=CARTESIAN_POINT('Ctrl Pts',(62.6162674727963,63.9372717599215,-3.77444482811614));
#37398=CARTESIAN_POINT('Ctrl Pts',(60.4566657372606,64.7051481120438,-3.65752819022485));
#37399=CARTESIAN_POINT('Ctrl Pts',(58.1897004590421,64.366898646618,-3.54061155233356));
#37400=CARTESIAN_POINT('Ctrl Pts',(56.348330501321,63.0020346584995,-3.42369491444227));
#37401=CARTESIAN_POINT('Ctrl Pts',(55.3653972967547,60.9314372354001,-3.30677827655098));
#37402=CARTESIAN_POINT('Ctrl Pts',(55.4720723824788,58.6418478274405,-3.18986163865969));
#37403=CARTESIAN_POINT('Ctrl Pts',(56.6430696682462,56.6716078213511,-3.0729450007684));
#37404=CARTESIAN_POINT('Ctrl Pts',(58.6035376278658,55.4837706210482,-2.95602836287711));
#37405=CARTESIAN_POINT('Ctrl Pts',(60.1288788547003,55.4000199588346,-2.87808393761625));
#37406=CARTESIAN_POINT('Ctrl Pts',(60.8569713719691,55.5399174695151,-2.83911172498582));
#37407=CARTESIAN_POINT('Ctrl Pts',(61.1059930590745,55.8829685022727,-10.4826648250425));
#37408=CARTESIAN_POINT('Ctrl Pts',(61.778083722502,56.0635179125043,-10.4436926124121));
#37409=CARTESIAN_POINT('Ctrl Pts',(63.031526542273,56.759914339158,-10.3657481871512));
#37410=CARTESIAN_POINT('Ctrl Pts',(64.1994414438023,58.5669429544754,-10.24883154926));
#37411=CARTESIAN_POINT('Ctrl Pts',(64.3798931515564,60.7106918460042,-10.1319149113687));
#37412=CARTESIAN_POINT('Ctrl Pts',(63.5307757969489,62.6874768694816,-10.0149982734774));
#37413=CARTESIAN_POINT('Ctrl Pts',(61.8515664623745,64.0324213047925,-9.89808163558608));
#37414=CARTESIAN_POINT('Ctrl Pts',(59.7370951569918,64.4294104300603,-9.78116499769479));
#37415=CARTESIAN_POINT('Ctrl Pts',(57.6844201518221,63.7850842639089,-9.6642483598035));
#37416=CARTESIAN_POINT('Ctrl Pts',(56.176116813259,62.2509313896104,-9.54733172191221));
#37417=CARTESIAN_POINT('Ctrl Pts',(55.5667639919965,60.1876073130513,-9.43041508402093));
#37418=CARTESIAN_POINT('Ctrl Pts',(55.9996168362521,58.0801798401711,-9.31349844612963));
#37419=CARTESIAN_POINT('Ctrl Pts',(57.37291501781,56.4240803592743,-9.19658180823834));
#37420=CARTESIAN_POINT('Ctrl Pts',(59.3638120104906,55.608640225254,-9.07966517034706));
#37421=CARTESIAN_POINT('Ctrl Pts',(61.5042696327058,55.8255600154627,-8.96274853245576));
#37422=CARTESIAN_POINT('Ctrl Pts',(63.2910902226969,57.0238445540762,-8.84583189456448));
#37423=CARTESIAN_POINT('Ctrl Pts',(64.3042117933318,58.9217900878708,-8.72891525667318));
#37424=CARTESIAN_POINT('Ctrl Pts',(64.3054611111089,61.0732112250417,-8.6119986187819));
#37425=CARTESIAN_POINT('Ctrl Pts',(63.2945435969878,62.9723314583153,-8.4950819808906));
#37426=CARTESIAN_POINT('Ctrl Pts',(61.5091166381646,64.1726912546809,-8.37816534299932));
#37427=CARTESIAN_POINT('Ctrl Pts',(59.3689103122146,64.392093700189,-8.26124870510803));
#37428=CARTESIAN_POINT('Ctrl Pts',(57.3770721300201,63.5789718296528,-8.14433206721674));
#37429=CARTESIAN_POINT('Ctrl Pts',(56.0018424130945,61.9244554261448,-8.02741542932545));
#37430=CARTESIAN_POINT('Ctrl Pts',(55.5665629903511,59.8175594691311,-7.91049879143416));
#37431=CARTESIAN_POINT('Ctrl Pts',(56.1734756936798,57.75346990765,-7.79358215354287));
#37432=CARTESIAN_POINT('Ctrl Pts',(57.6800910891129,56.2176946794742,-7.67666551565158));
#37433=CARTESIAN_POINT('Ctrl Pts',(59.7318125659897,55.5707090627434,-7.55974887776029));
#37434=CARTESIAN_POINT('Ctrl Pts',(61.8471844203754,55.9658398691463,-7.442832239869));
#37435=CARTESIAN_POINT('Ctrl Pts',(63.5270051470539,57.3075470580582,-7.32591560197771));
#37436=CARTESIAN_POINT('Ctrl Pts',(64.380478840536,59.2861355757008,-7.20899896408642));
#37437=CARTESIAN_POINT('Ctrl Pts',(64.1981287157098,61.4241273111779,-7.09208232619514));
#37438=CARTESIAN_POINT('Ctrl Pts',(62.6563934133655,63.8527697384689,-6.93619347567341));
#37439=CARTESIAN_POINT('Ctrl Pts',(58.884831100295,64.8859182064014,-6.74133241252127));
#37440=CARTESIAN_POINT('Ctrl Pts',(55.3157987821893,61.7815884332733,-6.50749913673868));
#37441=CARTESIAN_POINT('Ctrl Pts',(55.8162418715298,57.9032337882602,-6.31263807358654));
#37442=CARTESIAN_POINT('Ctrl Pts',(58.0077618404077,56.0397714172571,-6.15674922306482));
#37443=CARTESIAN_POINT('Ctrl Pts',(60.099845472672,55.5628581079429,-6.03983258517353));
#37444=CARTESIAN_POINT('Ctrl Pts',(62.1776283014177,56.1338645739201,-5.92291594728224));
#37445=CARTESIAN_POINT('Ctrl Pts',(63.7392073095132,57.6115136716518,-5.80599930939095));
#37446=CARTESIAN_POINT('Ctrl Pts',(64.4237125823697,59.651704586228,-5.68908267149966));
#37447=CARTESIAN_POINT('Ctrl Pts',(64.0673374374772,61.7732955371631,-5.57216603360837));
#37448=CARTESIAN_POINT('Ctrl Pts',(62.7551996806536,63.4782266232161,-5.45524939571708));
#37449=CARTESIAN_POINT('Ctrl Pts',(60.79514883301,64.3653621384009,-5.33833275782579));
#37450=CARTESIAN_POINT('Ctrl Pts',(58.6482581397286,64.2262970457918,-5.2214161199345));
#37451=CARTESIAN_POINT('Ctrl Pts',(56.8191049128515,63.0936542171897,-5.10449948204321));
#37452=CARTESIAN_POINT('Ctrl Pts',(55.7377643917842,61.2337377679946,-4.98758284415192));
#37453=CARTESIAN_POINT('Ctrl Pts',(55.6584192407754,59.0837784907731,-4.87066620626063));
#37454=CARTESIAN_POINT('Ctrl Pts',(56.5997358427842,57.1492149390329,-4.75374956836934));
#37455=CARTESIAN_POINT('Ctrl Pts',(58.3404149507315,55.8848383788669,-4.63683293047805));
#37456=CARTESIAN_POINT('Ctrl Pts',(60.4712450534049,55.5878912131347,-4.51991629258676));
#37457=CARTESIAN_POINT('Ctrl Pts',(62.4912901862697,56.3281817758293,-4.40299965469547));
#37458=CARTESIAN_POINT('Ctrl Pts',(63.9256609020545,57.9316762017641,-4.28608301680419));
#37459=CARTESIAN_POINT('Ctrl Pts',(64.4371518363133,60.0214107080549,-4.16916637891289));
#37460=CARTESIAN_POINT('Ctrl Pts',(63.9055181472461,62.1061115940624,-4.0522497410216));
#37461=CARTESIAN_POINT('Ctrl Pts',(62.4557390612544,63.6956894339549,-3.93533310313032));
#37462=CARTESIAN_POINT('Ctrl Pts',(60.4286457331249,64.416450583848,-3.81841646523903));
#37463=CARTESIAN_POINT('Ctrl Pts',(58.3007764528946,64.0989553608512,-3.70149982734773));
#37464=CARTESIAN_POINT('Ctrl Pts',(56.5723889013868,62.8178364218386,-3.58458318945645));
#37465=CARTESIAN_POINT('Ctrl Pts',(55.649766313996,60.8742862975069,-3.46766655156516));
#37466=CARTESIAN_POINT('Ctrl Pts',(55.7498960513411,58.725181054322,-3.35074991367387));
#37467=CARTESIAN_POINT('Ctrl Pts',(56.8490435219964,56.8758306368631,-3.23383327578258));
#37468=CARTESIAN_POINT('Ctrl Pts',(58.6892214842404,55.7608765117494,-3.11691663789129));
#37469=CARTESIAN_POINT('Ctrl Pts',(60.1209711319459,55.6822646057641,-3.03897221263043));
#37470=CARTESIAN_POINT('Ctrl Pts',(60.8043894954945,55.8135783132205,-3.));
#37471=CARTESIAN_POINT('Ctrl Pts',(64.2626696975502,60.0000007546914,-8.67031832941094));
#37472=CARTESIAN_POINT('Ctrl Pts',(64.2626718116082,60.3472087819798,-8.65087842586793));
#37473=CARTESIAN_POINT('Ctrl Pts',(64.2207061566376,60.6944163006858,-8.63143852232491));
#37474=CARTESIAN_POINT('Ctrl Pts',(64.1367666391259,61.0311610743922,-8.6119986187819));
#37475=CARTESIAN_POINT('Ctrl Pts',(63.9684886064019,61.7062513027996,-8.57302640615147));
#37476=CARTESIAN_POINT('Ctrl Pts',(63.6315161016949,62.3392913805575,-8.53405419352104));
#37477=CARTESIAN_POINT('Ctrl Pts',(63.1654586895375,62.8558713854973,-8.49508198089061));
#37478=CARTESIAN_POINT('Ctrl Pts',(62.6994012773801,63.3724513904372,-8.45610976826018));
#37479=CARTESIAN_POINT('Ctrl Pts',(62.1042589577723,63.772571322559,-8.41713755562975));
#37480=CARTESIAN_POINT('Ctrl Pts',(61.4499867436435,64.0091983628713,-8.37816534299932));
#37481=CARTESIAN_POINT('Ctrl Pts',(60.7957145295146,64.2458254031836,-8.33919313036889));
#37482=CARTESIAN_POINT('Ctrl Pts',(60.0823124208646,64.3189595516863,-8.30022091773846));
#37483=CARTESIAN_POINT('Ctrl Pts',(59.3936383361739,64.2200063141816,-8.26124870510803));
#37484=CARTESIAN_POINT('Ctrl Pts',(58.7049642514831,64.1210530766769,-8.2222764924776));
#37485=CARTESIAN_POINT('Ctrl Pts',(58.0410181907516,63.8500124531648,-8.18330427984717));
#37486=CARTESIAN_POINT('Ctrl Pts',(57.4798402075649,63.4387394074908,-8.14433206721674));
#37487=CARTESIAN_POINT('Ctrl Pts',(56.9186622243782,63.0274663618168,-8.10535985458631));
#37488=CARTESIAN_POINT('Ctrl Pts',(56.4602523187364,62.4759608939808,-8.06638764195588));
#37489=CARTESIAN_POINT('Ctrl Pts',(56.1585007954582,61.8490588338939,-8.02741542932545));
#37490=CARTESIAN_POINT('Ctrl Pts',(55.85674927218,61.2221567738069,-7.98844321669502));
#37491=CARTESIAN_POINT('Ctrl Pts',(55.7116561312655,60.519858121469,-7.94947100406459));
#37492=CARTESIAN_POINT('Ctrl Pts',(55.7402616780298,59.8246938683866,-7.91049879143416));
#37493=CARTESIAN_POINT('Ctrl Pts',(55.768867224794,59.1295296153041,-7.87152657880373));
#37494=CARTESIAN_POINT('Ctrl Pts',(55.9711714592369,58.441499761477,-7.8325543661733));
#37495=CARTESIAN_POINT('Ctrl Pts',(56.3234261423639,57.8415222965342,-7.79358215354287));
#37496=CARTESIAN_POINT('Ctrl Pts',(56.6756808254908,57.2415448315914,-7.75460994091244));
#37497=CARTESIAN_POINT('Ctrl Pts',(57.1778859573018,56.7296197555328,-7.71563772828201));
#37498=CARTESIAN_POINT('Ctrl Pts',(57.7709421026868,56.3658262813817,-7.67666551565158));
#37499=CARTESIAN_POINT('Ctrl Pts',(58.3639982480718,56.0020328072306,-7.63769330302115));
#37500=CARTESIAN_POINT('Ctrl Pts',(59.0479054070308,55.786370934987,-7.59872109039072));
#37501=CARTESIAN_POINT('Ctrl Pts',(59.7424209622412,55.7443951332657,-7.55974887776029));
#37502=CARTESIAN_POINT('Ctrl Pts',(60.4369365174516,55.7024193315444,-7.52077666512986));
#37503=CARTESIAN_POINT('Ctrl Pts',(61.1420604689135,55.8341296003453,-7.48180445249943));
#37504=CARTESIAN_POINT('Ctrl Pts',(61.7745925657575,56.1236025995645,-7.442832239869));
#37505=CARTESIAN_POINT('Ctrl Pts',(62.4071246626015,56.4130755987836,-7.40386002723857));
#37506=CARTESIAN_POINT('Ctrl Pts',(62.9670649048277,56.8603113284209,-7.36488781460814));
#37507=CARTESIAN_POINT('Ctrl Pts',(63.3892806415212,57.41369394618,-7.32591560197771));
#37508=CARTESIAN_POINT('Ctrl Pts',(63.8114963782146,57.9670765639391,-7.28694338934728));
#37509=CARTESIAN_POINT('Ctrl Pts',(64.0959876093753,58.6266060698199,-7.24797117671685));
#37510=CARTESIAN_POINT('Ctrl Pts',(64.2078415374846,59.3127027786732,-7.20899896408642));
#37511=CARTESIAN_POINT('Ctrl Pts',(64.2448472281053,59.5396906276728,-7.1961054191946));
#37512=CARTESIAN_POINT('Ctrl Pts',(64.2629569487826,59.7695863827851,-7.18321187430277));
#37513=CARTESIAN_POINT('Ctrl Pts',(64.2625441198806,59.9995177541909,-7.17031832941094));
#37514=CARTESIAN_POINT('Ctrl Pts',(61.322884965569,55.0755938055567,-10.));
#37515=CARTESIAN_POINT('Ctrl Pts',(61.4613623534188,55.1251023381749,-10.));
#37516=CARTESIAN_POINT('Ctrl Pts',(61.5973330701288,55.1806177929913,-10.));
#37517=CARTESIAN_POINT('Ctrl Pts',(61.7304726735596,55.2418650003063,-10.));
#37518=CARTESIAN_POINT('Ctrl Pts',(61.8646634500372,55.3035957708277,-10.));
#37519=CARTESIAN_POINT('Ctrl Pts',(61.9959788862617,55.3711496178193,-10.));
#37520=CARTESIAN_POINT('Ctrl Pts',(62.1240611590226,55.4442909142459,-10.));
#37521=CARTESIAN_POINT('Ctrl Pts',(62.2511464727888,55.5168628979036,-10.));
#37522=CARTESIAN_POINT('Ctrl Pts',(62.3750493162488,55.5949362272756,-10.));
#37523=CARTESIAN_POINT('Ctrl Pts',(62.4953860692366,55.6783183026231,-10.));
#37524=CARTESIAN_POINT('Ctrl Pts',(62.6141471692546,55.7606085983489,-10.));
#37525=CARTESIAN_POINT('Ctrl Pts',(62.7294354281262,55.8480700429306,-10.));
#37526=CARTESIAN_POINT('Ctrl Pts',(62.8408412017621,55.9405463957895,-10.));
#37527=CARTESIAN_POINT('Ctrl Pts',(62.8725488687966,55.9668664805511,-10.));
#37528=CARTESIAN_POINT('Ctrl Pts',(62.9039417533278,55.9935929543698,-10.));
#37529=CARTESIAN_POINT('Ctrl Pts',(62.9350097121908,56.020722563045,-10.));
#37530=CARTESIAN_POINT('Ctrl Pts',(62.9507462780503,56.0344642728092,-10.));
#37531=CARTESIAN_POINT('Ctrl Pts',(62.9663994747131,56.048309414399,-10.));
#37532=CARTESIAN_POINT('Ctrl Pts',(62.9819679512752,56.0622575780891,-10.));
#37533=CARTESIAN_POINT('Ctrl Pts',(62.9973223809954,56.076013972188,-10.));
#37534=CARTESIAN_POINT('Ctrl Pts',(63.0125883643442,56.0898652018544,-10.));
#37535=CARTESIAN_POINT('Ctrl Pts',(63.027759913392,56.1038060602825,-10.));
#37536=CARTESIAN_POINT('Ctrl Pts',(63.1388330059994,56.2058690898602,-10.));
#37537=CARTESIAN_POINT('Ctrl Pts',(63.2449336421493,56.3128090269311,-10.));
#37538=CARTESIAN_POINT('Ctrl Pts',(63.34567176205,56.4243836549341,-10.));
#37539=CARTESIAN_POINT('Ctrl Pts',(63.4421342874271,56.5312227581038,-10.));
#37540=CARTESIAN_POINT('Ctrl Pts',(63.533679969545,56.642312423058,-10.));
#37541=CARTESIAN_POINT('Ctrl Pts',(63.6201051195375,56.7572698794827,-10.));
#37542=CARTESIAN_POINT('Ctrl Pts',(63.706379868931,56.8720272822158,-10.));
#37543=CARTESIAN_POINT('Ctrl Pts',(63.7875521943201,56.9906397862812,-10.));
#37544=CARTESIAN_POINT('Ctrl Pts',(63.8633716991881,57.1127463357118,-10.));
#37545=CARTESIAN_POINT('Ctrl Pts',(63.9290488453146,57.2185187184769,-10.));
#37546=CARTESIAN_POINT('Ctrl Pts',(63.9907088543825,57.3269134655884,-10.));
#37547=CARTESIAN_POINT('Ctrl Pts',(64.0481572658614,57.4377013353837,-10.));
#37548=CARTESIAN_POINT('Ctrl Pts',(64.0632545108638,57.466816006626,-10.));
#37549=CARTESIAN_POINT('Ctrl Pts',(64.0780607290788,57.4960959612206,-10.));
#37550=CARTESIAN_POINT('Ctrl Pts',(64.0925720318306,57.5255370454525,-10.));
#37551=CARTESIAN_POINT('Ctrl Pts',(64.1048378291218,57.5504223626014,-10.));
#37552=CARTESIAN_POINT('Ctrl Pts',(64.1168955869776,57.5754286797017,-10.));
#37553=CARTESIAN_POINT('Ctrl Pts',(64.1287279624461,57.6005212096262,-10.));
#37554=CARTESIAN_POINT('Ctrl Pts',(64.1887507851646,57.7278096378235,-10.));
#37555=CARTESIAN_POINT('Ctrl Pts',(64.2430415539658,57.8574379049107,-10.));
#37556=CARTESIAN_POINT('Ctrl Pts',(64.2914122956066,57.9890469751202,-10.));
#37557=CARTESIAN_POINT('Ctrl Pts',(64.3393952774439,58.1196010127734,-10.));
#37558=CARTESIAN_POINT('Ctrl Pts',(64.381552967519,58.2521049552159,-10.));
#37559=CARTESIAN_POINT('Ctrl Pts',(64.4176523161959,58.3862204475955,-10.));
#37560=CARTESIAN_POINT('Ctrl Pts',(64.426387292412,58.4186724357637,-10.));
#37561=CARTESIAN_POINT('Ctrl Pts',(64.4347673173568,58.4512188074512,-10.));
#37562=CARTESIAN_POINT('Ctrl Pts',(64.442788628001,58.4838548036334,-10.));
#37563=CARTESIAN_POINT('Ctrl Pts',(64.4762031615177,58.6198072229625,-10.));
#37564=CARTESIAN_POINT('Ctrl Pts',(64.5033968549748,58.7573155296226,-10.));
#37565=CARTESIAN_POINT('Ctrl Pts',(64.5243233337952,58.8959463037013,-10.));
#37566=CARTESIAN_POINT('Ctrl Pts',(64.5357566990593,58.9716884431454,-10.));
#37567=CARTESIAN_POINT('Ctrl Pts',(64.5453183547014,59.0477655330272,-10.));
#37568=CARTESIAN_POINT('Ctrl Pts',(64.5529943308661,59.1241052349256,-10.));
#37569=CARTESIAN_POINT('Ctrl Pts',(64.5578649402481,59.1725447897545,-10.));
#37570=CARTESIAN_POINT('Ctrl Pts',(64.5619762400323,59.2210900501072,-10.));
#37571=CARTESIAN_POINT('Ctrl Pts',(64.5653237282423,59.2697221490712,-10.));
#37572=CARTESIAN_POINT('Ctrl Pts',(64.5666136562909,59.2884621429351,-10.));
#37573=CARTESIAN_POINT('Ctrl Pts',(64.5677902998301,59.3072175547175,-10.));
#37574=CARTESIAN_POINT('Ctrl Pts',(64.5688529128554,59.3259790228935,-10.));
#37575=CARTESIAN_POINT('Ctrl Pts',(64.5766120890547,59.4629748378002,-10.));
#37576=CARTESIAN_POINT('Ctrl Pts',(64.57828067089,59.5999983793925,-10.));
#37577=CARTESIAN_POINT('Ctrl Pts',(64.5738795531211,59.736643965364,-10.));
#37578=CARTESIAN_POINT('Ctrl Pts',(64.5694908520678,59.8729040380465,-10.));
#37579=CARTESIAN_POINT('Ctrl Pts',(64.559066518732,60.0087890791135,-10.));
#37580=CARTESIAN_POINT('Ctrl Pts',(64.5425762131985,60.1438893634685,-10.));
#37581=CARTESIAN_POINT('Ctrl Pts',(64.5263562494215,60.2767748163219,-10.));
#37582=CARTESIAN_POINT('Ctrl Pts',(64.504267351696,60.4089017135858,-10.));
#37583=CARTESIAN_POINT('Ctrl Pts',(64.4762339793328,60.5398620574008,-10.));
#37584=CARTESIAN_POINT('Ctrl Pts',(64.4633631283279,60.599989360351,-10.));
#37585=CARTESIAN_POINT('Ctrl Pts',(64.4492385683906,60.6598704422786,-10.));
#37586=CARTESIAN_POINT('Ctrl Pts',(64.4338497987549,60.7194639158437,-10.));
#37587=CARTESIAN_POINT('Ctrl Pts',(64.4113888332848,60.8064446806276,-10.));
#37588=CARTESIAN_POINT('Ctrl Pts',(64.3862349033453,60.8928130777696,-10.));
#37589=CARTESIAN_POINT('Ctrl Pts',(64.3584258263513,60.9784471471686,-10.));
#37590=CARTESIAN_POINT('Ctrl Pts',(64.3510564629766,61.001140046138,-10.));
#37591=CARTESIAN_POINT('Ctrl Pts',(64.343500606592,61.0237813381838,-10.));
#37592=CARTESIAN_POINT('Ctrl Pts',(64.3357588821457,61.0463686652349,-10.));
#37593=CARTESIAN_POINT('Ctrl Pts',(64.328750676373,61.0668158714004,-10.));
#37594=CARTESIAN_POINT('Ctrl Pts',(64.3215927040502,61.0872113276609,-10.));
#37595=CARTESIAN_POINT('Ctrl Pts',(64.3142878250982,61.1075478141133,-10.));
#37596=CARTESIAN_POINT('Ctrl Pts',(64.2688704372543,61.2339879780998,-10.));
#37597=CARTESIAN_POINT('Ctrl Pts',(64.217753895083,61.3582207618557,-10.));
#37598=CARTESIAN_POINT('Ctrl Pts',(64.1611296716898,61.4798690695452,-10.));
#37599=CARTESIAN_POINT('Ctrl Pts',(64.1136394008877,61.5818945054559,-10.));
#37600=CARTESIAN_POINT('Ctrl Pts',(64.0622740433798,61.6821018049246,-10.));
#37601=CARTESIAN_POINT('Ctrl Pts',(64.0071247254933,61.7802504068033,-10.));
#37602=CARTESIAN_POINT('Ctrl Pts',(63.9749821154106,61.8374542374444,-10.));
#37603=CARTESIAN_POINT('Ctrl Pts',(63.9415537805714,61.8939584151892,-10.));
#37604=CARTESIAN_POINT('Ctrl Pts',(63.9068550735822,61.9497121072916,-10.));
#37605=CARTESIAN_POINT('Ctrl Pts',(63.8949352721664,61.9688647788382,-10.));
#37606=CARTESIAN_POINT('Ctrl Pts',(63.8828641359213,61.9879310381597,-10.));
#37607=CARTESIAN_POINT('Ctrl Pts',(63.8706469073994,62.0069015270467,-10.));
#37608=CARTESIAN_POINT('Ctrl Pts',(63.7998198500733,62.1168793261435,-10.));
#37609=CARTESIAN_POINT('Ctrl Pts',(63.7241685217449,62.2235155057234,-10.));
#37610=CARTESIAN_POINT('Ctrl Pts',(63.6438531183809,62.3264414594354,-10.));
#37611=CARTESIAN_POINT('Ctrl Pts',(63.5707659198607,62.4201043098569,-10.));
#37612=CARTESIAN_POINT('Ctrl Pts',(63.4938156723471,62.5106946649326,-10.));
#37613=CARTESIAN_POINT('Ctrl Pts',(63.4130998283308,62.5979052737863,-10.));
#37614=CARTESIAN_POINT('Ctrl Pts',(63.3520426893251,62.6638753485895,-10.));
#37615=CARTESIAN_POINT('Ctrl Pts',(63.2888302429821,62.7279108715258,-10.));
#37616=CARTESIAN_POINT('Ctrl Pts',(63.2235668510161,62.7899187021734,-10.));
#37617=CARTESIAN_POINT('Origin',(60.,60.,-6.));
#37618=CARTESIAN_POINT('Origin',(-60.,-60.,-3.));
#37619=CARTESIAN_POINT('Ctrl Pts',(-59.1956105045055,-64.1864216867795,
-3.));
#37620=CARTESIAN_POINT('Ctrl Pts',(-59.3195769752075,-64.2229459535633,
-3.));
#37621=CARTESIAN_POINT('Ctrl Pts',(-59.4450598371526,-64.2536518518579,
-3.));
#37622=CARTESIAN_POINT('Ctrl Pts',(-59.5716384336509,-64.2786228996525,
-3.));
#37623=CARTESIAN_POINT('Ctrl Pts',(-59.7000946411857,-64.3039643569495,
-3.));
#37624=CARTESIAN_POINT('Ctrl Pts',(-59.8296800110397,-64.3233998046748,
-3.));
#37625=CARTESIAN_POINT('Ctrl Pts',(-59.9599813689613,-64.3369699541931,
-3.));
#37626=CARTESIAN_POINT('Ctrl Pts',(-60.0181562008825,-64.3430285339344,
-3.));
#37627=CARTESIAN_POINT('Ctrl Pts',(-60.0764740369278,-64.3479173489061,
-3.));
#37628=CARTESIAN_POINT('Ctrl Pts',(-60.1348992109591,-64.3516368969462,
-3.));
#37629=CARTESIAN_POINT('Ctrl Pts',(-60.1584275239312,-64.3531347904801,
-3.));
#37630=CARTESIAN_POINT('Ctrl Pts',(-60.1819732500468,-64.3544430369817,
-2.99999999999999));
#37631=CARTESIAN_POINT('Ctrl Pts',(-60.205534079903,-64.3555615786038,-2.99999999999999));
#37632=CARTESIAN_POINT('Ctrl Pts',(-60.2289634916764,-64.3566738812014,
-2.99999999999999));
#37633=CARTESIAN_POINT('Ctrl Pts',(-60.2523983629866,-64.3575981241379,
-3.));
#37634=CARTESIAN_POINT('Ctrl Pts',(-60.2758335397625,-64.3583346103257,
-3.));
#37635=CARTESIAN_POINT('Ctrl Pts',(-60.4095526409971,-64.3625369371117,
-3.));
#37636=CARTESIAN_POINT('Ctrl Pts',(-60.5433093906275,-64.360631729286,-2.99999999999999));
#37637=CARTESIAN_POINT('Ctrl Pts',(-60.6766723905723,-64.3526712769133,
-2.99999999999999));
#37638=CARTESIAN_POINT('Ctrl Pts',(-60.7846048350664,-64.3462287772377,
-3.));
#37639=CARTESIAN_POINT('Ctrl Pts',(-60.8922800261175,-64.3358192861715,
-3.));
#37640=CARTESIAN_POINT('Ctrl Pts',(-60.9994757883914,-64.3214466528355,
-3.));
#37641=CARTESIAN_POINT('Ctrl Pts',(-61.0530736695283,-64.3142603361676,
-3.));
#37642=CARTESIAN_POINT('Ctrl Pts',(-61.1065517534524,-64.3060828957079,
-3.));
#37643=CARTESIAN_POINT('Ctrl Pts',(-61.1598824475224,-64.2969127553923,
-3.));
#37644=CARTESIAN_POINT('Ctrl Pts',(-61.1872713223749,-64.2922032756102,
-3.));
#37645=CARTESIAN_POINT('Ctrl Pts',(-61.2146213234789,-64.2872319479493,
-3.));
#37646=CARTESIAN_POINT('Ctrl Pts',(-61.2419287096427,-64.2819984158526,
-3.));
#37647=CARTESIAN_POINT('Ctrl Pts',(-61.2615201519558,-64.2782436646087,
-3.));
#37648=CARTESIAN_POINT('Ctrl Pts',(-61.2810874285119,-64.2743543242779,
-3.));
#37649=CARTESIAN_POINT('Ctrl Pts',(-61.3006182223717,-64.2703327355513,
-3.));
#37650=CARTESIAN_POINT('Ctrl Pts',(-61.3068719962591,-64.2690450200214,
-3.));
#37651=CARTESIAN_POINT('Ctrl Pts',(-61.3131223455695,-64.2677436853781,
-3.));
#37652=CARTESIAN_POINT('Ctrl Pts',(-61.319369225276,-64.2664287399395,-3.));
#37653=CARTESIAN_POINT('Ctrl Pts',(-61.4494243700941,-64.2390526053768,
-3.));
#37654=CARTESIAN_POINT('Ctrl Pts',(-61.5779747925235,-64.2057813906861,
-3.));
#37655=CARTESIAN_POINT('Ctrl Pts',(-61.7046919624325,-64.1669093068584,
-3.));
#37656=CARTESIAN_POINT('Ctrl Pts',(-61.8336750528799,-64.1273421234386,
-3.));
#37657=CARTESIAN_POINT('Ctrl Pts',(-61.9607594086197,-64.0819718837584,
-3.));
#37658=CARTESIAN_POINT('Ctrl Pts',(-62.0856033789978,-64.0310550776473,
-3.));
#37659=CARTESIAN_POINT('Ctrl Pts',(-62.2120505628986,-63.9794844112669,
-3.));
#37660=CARTESIAN_POINT('Ctrl Pts',(-62.3362002069323,-63.9222236565176,
-3.));
#37661=CARTESIAN_POINT('Ctrl Pts',(-62.4576913752432,-63.8594865308942,
-3.));
#37662=CARTESIAN_POINT('Ctrl Pts',(-62.5340612523311,-63.820049700717,-3.));
#37663=CARTESIAN_POINT('Ctrl Pts',(-62.6093804939423,-63.7784478743419,
-3.));
#37664=CARTESIAN_POINT('Ctrl Pts',(-62.6835561803521,-63.7347241134274,
-3.));
#37665=CARTESIAN_POINT('Ctrl Pts',(-62.7445592832535,-63.6987650921443,
-3.));
#37666=CARTESIAN_POINT('Ctrl Pts',(-62.8047888964893,-63.6613707234564,
-3.));
#37667=CARTESIAN_POINT('Ctrl Pts',(-62.8641913966604,-63.6225612636812,
-3.));
#37668=CARTESIAN_POINT('Ctrl Pts',(-62.8791977478544,-63.6127571581072,
-3.));
#37669=CARTESIAN_POINT('Ctrl Pts',(-62.8941494905117,-63.6028638609676,
-3.));
#37670=CARTESIAN_POINT('Ctrl Pts',(-62.9090364113711,-63.5928881663496,
-3.));
#37671=CARTESIAN_POINT('Ctrl Pts',(-63.0253586853184,-63.5149408531926,
-3.));
#37672=CARTESIAN_POINT('Ctrl Pts',(-63.137885912799,-63.4318617290311,-3.));
#37673=CARTESIAN_POINT('Ctrl Pts',(-63.246261646252,-63.3439219695934,-3.));
#37674=CARTESIAN_POINT('Ctrl Pts',(-63.2693906398052,-63.3251543168699,
-3.));
#37675=CARTESIAN_POINT('Ctrl Pts',(-63.2923305198638,-63.3061650953556,
-3.));
#37676=CARTESIAN_POINT('Ctrl Pts',(-63.3150777604115,-63.2869566419458,
-3.));
#37677=CARTESIAN_POINT('Ctrl Pts',(-63.4206897880943,-63.1977746724228,
-3.));
#37678=CARTESIAN_POINT('Ctrl Pts',(-63.5221510927373,-63.1038707715521,
-3.));
#37679=CARTESIAN_POINT('Ctrl Pts',(-63.6192855100693,-63.0056344766105,
-3.));
#37680=CARTESIAN_POINT('Ctrl Pts',(-63.717532292034,-62.9062731985461,-3.));
#37681=CARTESIAN_POINT('Ctrl Pts',(-63.8113530794893,-62.8024792577487,
-3.));
#37682=CARTESIAN_POINT('Ctrl Pts',(-63.9005375394928,-62.6946104879407,
-3.));
#37683=CARTESIAN_POINT('Ctrl Pts',(-63.9806728102355,-62.5976867293296,
-3.));
#37684=CARTESIAN_POINT('Ctrl Pts',(-64.0570647853735,-62.4974722229016,
-3.));
#37685=CARTESIAN_POINT('Ctrl Pts',(-64.129536208176,-62.3942009297676,-3.));
#37686=CARTESIAN_POINT('Ctrl Pts',(-64.1412822732054,-62.3774628656051,
-3.));
#37687=CARTESIAN_POINT('Ctrl Pts',(-64.1529252913588,-62.3606444563152,
-3.));
#37688=CARTESIAN_POINT('Ctrl Pts',(-64.1644644409263,-62.3437466478903,
-3.));
#37689=CARTESIAN_POINT('Ctrl Pts',(-64.1746328675554,-62.32885611162,-3.));
#37690=CARTESIAN_POINT('Ctrl Pts',(-64.184715292135,-62.3139117392423,-3.));
#37691=CARTESIAN_POINT('Ctrl Pts',(-64.1947108963489,-62.2989151294246,
-3.));
#37692=CARTESIAN_POINT('Ctrl Pts',(-64.2739894449572,-62.1799718984846,
-3.));
#37693=CARTESIAN_POINT('Ctrl Pts',(-64.3478188937706,-62.0577313604119,
-3.));
#37694=CARTESIAN_POINT('Ctrl Pts',(-64.4160215697397,-61.9326058716527,
-3.));
#37695=CARTESIAN_POINT('Ctrl Pts',(-64.4849569622618,-61.8061361318724,
-3.));
#37696=CARTESIAN_POINT('Ctrl Pts',(-64.5481446100938,-61.6767185791534,
-3.));
#37697=CARTESIAN_POINT('Ctrl Pts',(-64.6053684527712,-61.5447373590947,
-3.));
#37698=CARTESIAN_POINT('Ctrl Pts',(-64.6262260898092,-61.4966312506089,
-3.));
#37699=CARTESIAN_POINT('Ctrl Pts',(-64.6462910549685,-61.448184191749,-3.));
#37700=CARTESIAN_POINT('Ctrl Pts',(-64.6655515905053,-61.3994136515623,
-3.));
#37701=CARTESIAN_POINT('Ctrl Pts',(-64.7181182489016,-61.2663070553886,
-3.));
#37702=CARTESIAN_POINT('Ctrl Pts',(-64.764696319996,-61.13079266721,-3.));
#37703=CARTESIAN_POINT('Ctrl Pts',(-64.8052734588863,-60.993284910806,-3.));
#37704=CARTESIAN_POINT('Ctrl Pts',(-64.8290066045075,-60.9128580572618,
-3.));
#37705=CARTESIAN_POINT('Ctrl Pts',(-64.8506859899574,-60.831748786273,-3.));
#37706=CARTESIAN_POINT('Ctrl Pts',(-64.8703015413704,-60.750036894404,-3.));
#37707=CARTESIAN_POINT('Ctrl Pts',(-64.8777895131791,-60.7188444833486,
-3.));
#37708=CARTESIAN_POINT('Ctrl Pts',(-64.8849766776954,-60.6875642384272,
-3.));
#37709=CARTESIAN_POINT('Ctrl Pts',(-64.8918622508146,-60.656200539862,-3.));
#37710=CARTESIAN_POINT('Ctrl Pts',(-64.8973648511838,-60.6311362647006,
-3.));
#37711=CARTESIAN_POINT('Ctrl Pts',(-64.9026757017017,-60.6060140560556,
-3.));
#37712=CARTESIAN_POINT('Ctrl Pts',(-64.9077886731734,-60.5808652409076,
-3.));
#37713=CARTESIAN_POINT('Ctrl Pts',(-64.9369314962056,-60.4375224756745,
-3.));
#37714=CARTESIAN_POINT('Ctrl Pts',(-64.9596873210609,-60.293155610705,-3.));
#37715=CARTESIAN_POINT('Ctrl Pts',(-64.9761060740654,-60.1482217119791,
-3.));
#37716=CARTESIAN_POINT('Ctrl Pts',(-64.9926869198554,-60.0018569652858,
-3.));
#37717=CARTESIAN_POINT('Ctrl Pts',(-65.0028051887902,-59.8549132164108,
-3.));
#37718=CARTESIAN_POINT('Ctrl Pts',(-65.0064655295109,-59.707835000365,-3.));
#37719=CARTESIAN_POINT('Ctrl Pts',(-65.0101294137172,-59.5606144015204,
-3.));
#37720=CARTESIAN_POINT('Ctrl Pts',(-65.0073230416735,-59.4132582968452,
-3.));
#37721=CARTESIAN_POINT('Ctrl Pts',(-64.9980013952553,-59.2661977118922,
-3.));
#37722=CARTESIAN_POINT('Ctrl Pts',(-64.9923757136022,-59.1774455754613,
-3.));
#37723=CARTESIAN_POINT('Ctrl Pts',(-64.9843760617657,-59.0888008393423,
-3.));
#37724=CARTESIAN_POINT('Ctrl Pts',(-64.9739833680071,-59.0003574710342,
-3.));
#37725=CARTESIAN_POINT('Ctrl Pts',(-64.9615316286333,-58.8943913185524,
-3.));
#37726=CARTESIAN_POINT('Ctrl Pts',(-64.945645012555,-58.7887140863586,-3.));
#37727=CARTESIAN_POINT('Ctrl Pts',(-64.9263786176897,-58.683468154111,-3.));
#37728=CARTESIAN_POINT('Ctrl Pts',(-63.6032183801568,-56.3921449163111,
-3.));
#37729=CARTESIAN_POINT('Ctrl Pts',(-63.4898426947805,-56.2959035274869,
-3.));
#37730=CARTESIAN_POINT('Ctrl Pts',(-63.3723223864688,-56.2048634114124,
-3.));
#37731=CARTESIAN_POINT('Ctrl Pts',(-63.251055780641,-56.1192063947302,-3.));
#37732=CARTESIAN_POINT('Ctrl Pts',(-63.129678168823,-56.0334709686467,-3.));
#37733=CARTESIAN_POINT('Ctrl Pts',(-63.0045466457224,-55.9531282054953,
-3.));
#37734=CARTESIAN_POINT('Ctrl Pts',(-62.8760397304487,-55.8784080151765,
-3.));
#37735=CARTESIAN_POINT('Ctrl Pts',(-62.8196879527792,-55.8456423422685,
-3.));
#37736=CARTESIAN_POINT('Ctrl Pts',(-62.762686909838,-55.8139584898394,-3.00000000000001));
#37737=CARTESIAN_POINT('Ctrl Pts',(-62.7050678179436,-55.7833789513493,
-3.00000000000001));
#37738=CARTESIAN_POINT('Ctrl Pts',(-62.6757305829629,-55.7678091275846,
-3.00000000000001));
#37739=CARTESIAN_POINT('Ctrl Pts',(-62.6462331190597,-55.7525256196819,
-3.00000000000001));
#37740=CARTESIAN_POINT('Ctrl Pts',(-62.6165795262305,-55.737531594111,-3.00000000000001));
#37741=CARTESIAN_POINT('Ctrl Pts',(-62.5949658489926,-55.7266028668215,
-3.00000000000001));
#37742=CARTESIAN_POINT('Ctrl Pts',(-62.5732698365523,-55.7158283111196,
-3.));
#37743=CARTESIAN_POINT('Ctrl Pts',(-62.5515051559284,-55.7052148415274,
-3.));
#37744=CARTESIAN_POINT('Ctrl Pts',(-62.4199918158176,-55.6410828259762,
-3.));
#37745=CARTESIAN_POINT('Ctrl Pts',(-62.2858584006406,-55.5827701223888,
-3.));
#37746=CARTESIAN_POINT('Ctrl Pts',(-62.1494741826111,-55.5304873365666,
-3.));
#37747=CARTESIAN_POINT('Ctrl Pts',(-62.0315669656725,-55.4852876950014,
-3.));
#37748=CARTESIAN_POINT('Ctrl Pts',(-61.9119769355875,-55.4445954662697,
-3.00000000000001));
#37749=CARTESIAN_POINT('Ctrl Pts',(-61.7909378382297,-55.4085780791561,
-3.00000000000001));
#37750=CARTESIAN_POINT('Ctrl Pts',(-61.7304182895508,-55.3905693855993,
-3.00000000000001));
#37751=CARTESIAN_POINT('Ctrl Pts',(-61.6695364403128,-55.3737298700684,
-3.00000000000001));
#37752=CARTESIAN_POINT('Ctrl Pts',(-61.6083215243732,-55.3580833488014,
-3.00000000000001));
#37753=CARTESIAN_POINT('Ctrl Pts',(-61.5794892144394,-55.3507138156797,
-3.00000000000001));
#37754=CARTESIAN_POINT('Ctrl Pts',(-61.550583018072,-55.3436089674838,-3.));
#37755=CARTESIAN_POINT('Ctrl Pts',(-61.5216060047899,-55.3367714460112,
-3.));
#37756=CARTESIAN_POINT('Ctrl Pts',(-61.495341183815,-55.3305739033024,-3.));
#37757=CARTESIAN_POINT('Ctrl Pts',(-61.469014297269,-55.3245952282657,-3.00000000000001));
#37758=CARTESIAN_POINT('Ctrl Pts',(-61.4426542119394,-55.3188429929397,
-3.00000000000001));
#37759=CARTESIAN_POINT('Ctrl Pts',(-61.4363511262509,-55.3174675485241,
-3.00000000000001));
#37760=CARTESIAN_POINT('Ctrl Pts',(-61.4300458619349,-55.3161049811205,
-3.00000000000001));
#37761=CARTESIAN_POINT('Ctrl Pts',(-61.423738450879,-55.3147553063535,-3.00000000000001));
#37762=CARTESIAN_POINT('Ctrl Pts',(-61.2841865141129,-55.2848936521691,
-3.00000000000001));
#37763=CARTESIAN_POINT('Ctrl Pts',(-61.1435843785244,-55.2613388246454,
-3.00000000000001));
#37764=CARTESIAN_POINT('Ctrl Pts',(-61.0023538690712,-55.2440351533839,
-3.));
#37765=CARTESIAN_POINT('Ctrl Pts',(-60.8601845317392,-55.2266164562045,
-3.));
#37766=CARTESIAN_POINT('Ctrl Pts',(-60.7173776215922,-55.2155323614428,
-3.));
#37767=CARTESIAN_POINT('Ctrl Pts',(-60.5743626033957,-55.210778665957,-3.));
#37768=CARTESIAN_POINT('Ctrl Pts',(-60.4327944357155,-55.2060730625307,
-3.));
#37769=CARTESIAN_POINT('Ctrl Pts',(-60.2910215895177,-55.2075706082915,
-3.));
#37770=CARTESIAN_POINT('Ctrl Pts',(-60.1494715736686,-55.2153164997798,
-3.));
#37771=CARTESIAN_POINT('Ctrl Pts',(-60.0601035604392,-55.2202068908465,
-3.));
#37772=CARTESIAN_POINT('Ctrl Pts',(-59.9708246262431,-55.2275888864629,
-3.));
#37773=CARTESIAN_POINT('Ctrl Pts',(-59.8817466888378,-55.2374836515892,
-3.));
#37774=CARTESIAN_POINT('Ctrl Pts',(-59.8149382357838,-55.244904725434,-3.));
#37775=CARTESIAN_POINT('Ctrl Pts',(-59.7482429092863,-55.2537393878111,
-3.));
#37776=CARTESIAN_POINT('Ctrl Pts',(-59.6817096243707,-55.2639993082479,
-3.));
#37777=CARTESIAN_POINT('Ctrl Pts',(-59.6640768304109,-55.2667184143816,
-3.));
#37778=CARTESIAN_POINT('Ctrl Pts',(-59.6464554266234,-55.2695376386596,
-3.));
#37779=CARTESIAN_POINT('Ctrl Pts',(-59.6288463434743,-55.272457225627,-3.));
#37780=CARTESIAN_POINT('Ctrl Pts',(-59.6106485602809,-55.2754744190945,
-3.));
#37781=CARTESIAN_POINT('Ctrl Pts',(-59.5924726121038,-55.2785973698234,
-3.));
#37782=CARTESIAN_POINT('Ctrl Pts',(-59.5743220572586,-55.2818255665583,
-3.));
#37783=CARTESIAN_POINT('Ctrl Pts',(-59.4370113023005,-55.3062471963439,
-3.));
#37784=CARTESIAN_POINT('Ctrl Pts',(-59.301103309529,-55.3366962002016,-3.));
#37785=CARTESIAN_POINT('Ctrl Pts',(-59.1669958586959,-55.3731700865706,
-3.));
#37786=CARTESIAN_POINT('Ctrl Pts',(-59.1418080575942,-55.3800205411096,
-3.));
#37787=CARTESIAN_POINT('Ctrl Pts',(-59.116683813921,-55.3870836687706,-3.));
#37788=CARTESIAN_POINT('Ctrl Pts',(-59.0916258294163,-55.3943596481952,
-3.));
#37789=CARTESIAN_POINT('Ctrl Pts',(-58.9576617593453,-55.4332582203163,
-3.));
#37790=CARTESIAN_POINT('Ctrl Pts',(-58.8255893716933,-55.4782367586987,
-3.));
#37791=CARTESIAN_POINT('Ctrl Pts',(-58.6957822734934,-55.5290865431825,
-3.));
#37792=CARTESIAN_POINT('Ctrl Pts',(-58.5664089361555,-55.5797664090204,
-3.));
#37793=CARTESIAN_POINT('Ctrl Pts',(-58.4392851252412,-55.636278851372,-3.));
#37794=CARTESIAN_POINT('Ctrl Pts',(-58.3148123789666,-55.6984578656476,
-3.));
#37795=CARTESIAN_POINT('Ctrl Pts',(-58.2087252890362,-55.7514525241305,
-3.));
#37796=CARTESIAN_POINT('Ctrl Pts',(-58.1045642359244,-55.8085642160639,
-3.));
#37797=CARTESIAN_POINT('Ctrl Pts',(-58.0026013764877,-55.8697095384881,
-3.));
#37798=CARTESIAN_POINT('Ctrl Pts',(-57.984257187675,-55.8807102238922,-3.));
#37799=CARTESIAN_POINT('Ctrl Pts',(-57.9659842134992,-55.8918415103031,
-3.));
#37800=CARTESIAN_POINT('Ctrl Pts',(-57.9477841256088,-55.9031029645992,
-3.));
#37801=CARTESIAN_POINT('Ctrl Pts',(-57.9313889896199,-55.9132475900389,
-3.));
#37802=CARTESIAN_POINT('Ctrl Pts',(-57.9150608534493,-55.9234930063007,
-3.));
#37803=CARTESIAN_POINT('Ctrl Pts',(-57.8988041215737,-55.9338364228883,
-3.));
#37804=CARTESIAN_POINT('Ctrl Pts',(-57.7839056269251,-56.0069410914355,
-3.));
#37805=CARTESIAN_POINT('Ctrl Pts',(-57.6725153636961,-56.0849724426437,
-3.));
#37806=CARTESIAN_POINT('Ctrl Pts',(-57.5649776520738,-56.1677286853735,
-3.));
#37807=CARTESIAN_POINT('Ctrl Pts',(-57.4583964400229,-56.2497488485504,
-3.));
#37808=CARTESIAN_POINT('Ctrl Pts',(-57.3555989995654,-56.3364107540539,
-3.));
#37809=CARTESIAN_POINT('Ctrl Pts',(-57.2569565735731,-56.4275538681827,
-3.));
#37810=CARTESIAN_POINT('Ctrl Pts',(-57.224173905029,-56.4578442272297,-3.));
#37811=CARTESIAN_POINT('Ctrl Pts',(-57.1918504858555,-56.4886297926312,
-3.));
#37812=CARTESIAN_POINT('Ctrl Pts',(-57.1600009946507,-56.5199054102076,
-3.));
#37813=CARTESIAN_POINT('Ctrl Pts',(-57.063427842614,-56.6147384783981,-3.));
#37814=CARTESIAN_POINT('Ctrl Pts',(-56.9712084392596,-56.7140758024186,
-3.));
#37815=CARTESIAN_POINT('Ctrl Pts',(-56.8836152244926,-56.8175811575214,
-3.));
#37816=CARTESIAN_POINT('Ctrl Pts',(-56.8363965206617,-56.8733775878787,
-3.));
#37817=CARTESIAN_POINT('Ctrl Pts',(-56.7905229834664,-56.930385559123,-3.));
#37818=CARTESIAN_POINT('Ctrl Pts',(-56.7460434065629,-56.9885540563686,
-3.));
#37819=CARTESIAN_POINT('Ctrl Pts',(-56.7284856804581,-57.0115153031624,
-3.));
#37820=CARTESIAN_POINT('Ctrl Pts',(-56.711145206329,-57.034657388313,-3.));
#37821=CARTESIAN_POINT('Ctrl Pts',(-56.69402518081,-57.0579772003701,-3.));
#37822=CARTESIAN_POINT('Ctrl Pts',(-56.6800434073205,-57.077022284715,-3.));
#37823=CARTESIAN_POINT('Ctrl Pts',(-56.6662063227873,-57.0961893605202,
-3.));
#37824=CARTESIAN_POINT('Ctrl Pts',(-56.652531641636,-57.1154538907109,-3.));
#37825=CARTESIAN_POINT('Ctrl Pts',(-56.5757648226242,-57.2236009609155,
-3.));
#37826=CARTESIAN_POINT('Ctrl Pts',(-56.5040156722043,-57.33494533068,-3.));
#37827=CARTESIAN_POINT('Ctrl Pts',(-56.4374818319856,-57.4491372747288,
-3.));
#37828=CARTESIAN_POINT('Ctrl Pts',(-56.3711910735432,-57.5629120178389,
-3.));
#37829=CARTESIAN_POINT('Ctrl Pts',(-56.31007728771,-57.6795143228349,-3.));
#37830=CARTESIAN_POINT('Ctrl Pts',(-56.2543835770224,-57.7986178389126,
-3.));
#37831=CARTESIAN_POINT('Ctrl Pts',(-56.1996788698177,-57.9156063263675,
-3.));
#37832=CARTESIAN_POINT('Ctrl Pts',(-56.1502032929139,-58.0350086810399,
-3.));
#37833=CARTESIAN_POINT('Ctrl Pts',(-56.1062364267016,-58.1565237324278,
-3.));
#37834=CARTESIAN_POINT('Ctrl Pts',(-56.0839234950841,-58.2181919218099,
-3.));
#37835=CARTESIAN_POINT('Ctrl Pts',(-56.0630301391519,-58.2804043026903,
-3.));
#37836=CARTESIAN_POINT('Ctrl Pts',(-56.0435980798389,-58.3431214745369,
-3.));
#37837=CARTESIAN_POINT('Ctrl Pts',(-56.0170092495455,-58.4289371985343,
-3.));
#37838=CARTESIAN_POINT('Ctrl Pts',(-55.9931559588827,-58.5156982188528,
-3.));
#37839=CARTESIAN_POINT('Ctrl Pts',(-55.9720760639888,-58.6032685615972,
-3.));
#37840=CARTESIAN_POINT('Origin',(-60.,-60.,-13.3123464956316));
#37841=CARTESIAN_POINT('Ctrl Pts',(-54.9007452025866,-59.9999087514893,
-9.56234649563159));
#37842=CARTESIAN_POINT('Ctrl Pts',(-54.900655342442,-59.8930270619539,-9.55734157105847));
#37843=CARTESIAN_POINT('Ctrl Pts',(-54.9296018038888,-58.9539304600107,
-9.51336443385491));
#37844=CARTESIAN_POINT('Ctrl Pts',(-55.4826600864412,-57.2140033424977,
-9.43041508402093));
#37845=CARTESIAN_POINT('Ctrl Pts',(-57.3241694777564,-55.4165445512788,
-9.31349844612963));
#37846=CARTESIAN_POINT('Ctrl Pts',(-59.7947368654586,-54.6966046195577,
-9.19658180823835));
#37847=CARTESIAN_POINT('Ctrl Pts',(-62.3135594050244,-55.2234345982174,
-9.07966517034706));
#37848=CARTESIAN_POINT('Ctrl Pts',(-64.2884897146217,-56.8731819984634,
-8.96274853245577));
#37849=CARTESIAN_POINT('Ctrl Pts',(-65.2552435912467,-59.2580098856016,
-8.84583189456447));
#37850=CARTESIAN_POINT('Ctrl Pts',(-64.986547872926,-61.817271139308,-8.72891525667319));
#37851=CARTESIAN_POINT('Ctrl Pts',(-63.5455699794028,-63.9493126448601,
-8.6119986187819));
#37852=CARTESIAN_POINT('Ctrl Pts',(-61.2710678060581,-65.1529132589701,
-8.49508198089061));
#37853=CARTESIAN_POINT('Ctrl Pts',(-58.6977517372794,-65.1451236320635,
-8.37816534299932));
#37854=CARTESIAN_POINT('Ctrl Pts',(-56.4305796611695,-63.9277667709211,
-8.26124870510803));
#37855=CARTESIAN_POINT('Ctrl Pts',(-55.1447571992843,-62.0002411018557,
-8.15597575598545));
#37856=CARTESIAN_POINT('Ctrl Pts',(-54.9016527228214,-60.5836272117911,
-8.08967501949331));
#37857=CARTESIAN_POINT('Ctrl Pts',(-54.9011518411408,-59.9998830094301,
-8.06234649563159));
#37858=CARTESIAN_POINT('Ctrl Pts',(-54.9012106606313,-59.9998804662267,
-9.68765350436841));
#37859=CARTESIAN_POINT('Ctrl Pts',(-54.9010041861375,-59.7264420560186,
-9.67485236502099));
#37860=CARTESIAN_POINT('Ctrl Pts',(-54.9885269673505,-58.6206708842071,
-9.62307901304313));
#37861=CARTESIAN_POINT('Ctrl Pts',(-55.7768178205809,-56.785492732961,-9.53233344843484));
#37862=CARTESIAN_POINT('Ctrl Pts',(-57.7853302129478,-55.1767966332062,
-9.41541681054355));
#37863=CARTESIAN_POINT('Ctrl Pts',(-60.3144620635955,-54.7019555263241,
-9.29850017265227));
#37864=CARTESIAN_POINT('Ctrl Pts',(-62.7696789900454,-55.4726379404574,
-9.18158353476098));
#37865=CARTESIAN_POINT('Ctrl Pts',(-64.5737696881318,-57.3076474190762,
-9.06466689686968));
#37866=CARTESIAN_POINT('Ctrl Pts',(-65.3026202647668,-59.7756017648733,
-8.9477502589784));
#37867=CARTESIAN_POINT('Ctrl Pts',(-64.7848823729,-62.2963084445819,-8.8308336210871));
#37868=CARTESIAN_POINT('Ctrl Pts',(-63.1422721548051,-64.2771789992941,
-8.71391698319582));
#37869=CARTESIAN_POINT('Ctrl Pts',(-60.7609482822248,-65.252531849864,-8.59700034530452));
#37870=CARTESIAN_POINT('Ctrl Pts',(-58.2007340409931,-64.9930727838061,
-8.48008370741324));
#37871=CARTESIAN_POINT('Ctrl Pts',(-56.0635071815643,-63.5597974366436,
-8.36316706952195));
#37872=CARTESIAN_POINT('Ctrl Pts',(-55.0531943003858,-61.6671136005503,
-8.26569033517368));
#37873=CARTESIAN_POINT('Ctrl Pts',(-54.9013976662957,-60.4172707815651,
-8.20718581345583));
#37874=CARTESIAN_POINT('Ctrl Pts',(-54.901395125587,-59.9999990971874,-8.18765350436841));
#37875=CARTESIAN_POINT('Ctrl Pts',(-63.2233527839579,-57.2101674189746,
-10.));
#37876=CARTESIAN_POINT('Ctrl Pts',(-63.6787829722545,-57.7363682294924,
-9.96102778736957));
#37877=CARTESIAN_POINT('Ctrl Pts',(-64.3265775369929,-59.0156060985281,
-9.8830833621087));
#37878=CARTESIAN_POINT('Ctrl Pts',(-64.2810882742281,-61.1667237108393,
-9.76616672421743));
#37879=CARTESIAN_POINT('Ctrl Pts',(-63.22907753389,-63.0432886084162,-9.64925008632613));
#37880=CARTESIAN_POINT('Ctrl Pts',(-61.4179627144323,-64.2045560607698,
-9.53233344843485));
#37881=CARTESIAN_POINT('Ctrl Pts',(-59.2734876096321,-64.3773165471069,
-9.41541681054355));
#37882=CARTESIAN_POINT('Ctrl Pts',(-57.2998122798752,-63.5210484654286,
-9.29850017265226));
#37883=CARTESIAN_POINT('Ctrl Pts',(-55.9609186974804,-61.8370072168577,
-9.18158353476097));
#37884=CARTESIAN_POINT('Ctrl Pts',(-55.5715694949038,-59.7211123005161,
-9.06466689686968));
#37885=CARTESIAN_POINT('Ctrl Pts',(-56.2232947535789,-57.6707778484149,
-8.94775025897839));
#37886=CARTESIAN_POINT('Ctrl Pts',(-57.7628818363748,-56.1680191061191,
-8.83083362108711));
#37887=CARTESIAN_POINT('Ctrl Pts',(-59.8283905192097,-55.5661160017993,
-8.71391698319581));
#37888=CARTESIAN_POINT('Ctrl Pts',(-61.9342427424238,-56.0065702475388,
-8.59700034530453));
#37889=CARTESIAN_POINT('Ctrl Pts',(-63.5853758881021,-57.3858354303686,
-8.48008370741323));
#37890=CARTESIAN_POINT('Ctrl Pts',(-64.3936268737958,-59.3796619224004,
-8.36316706952195));
#37891=CARTESIAN_POINT('Ctrl Pts',(-64.1689848170786,-61.5193227822848,
-8.24625043163066));
#37892=CARTESIAN_POINT('Ctrl Pts',(-62.9642606044702,-63.3018081594506,
-8.12933379373937));
#37893=CARTESIAN_POINT('Ctrl Pts',(-61.0626715154394,-64.3080739797979,
-8.01241715584808));
#37894=CARTESIAN_POINT('Ctrl Pts',(-58.9112601796474,-64.3015614911722,
-7.89550051795679));
#37895=CARTESIAN_POINT('Ctrl Pts',(-57.0157993911679,-63.2837948116173,
-7.7785838800655));
#37896=CARTESIAN_POINT('Ctrl Pts',(-55.821891404445,-61.494054502106,-7.66166724217421));
#37897=CARTESIAN_POINT('Ctrl Pts',(-55.6102098839069,-59.3530565588066,
-7.54475060428292));
#37898=CARTESIAN_POINT('Ctrl Pts',(-56.4305207206919,-57.3641952812435,
-7.42783396639163));
#37899=CARTESIAN_POINT('Ctrl Pts',(-58.0899737985984,-55.9948801098928,
-7.31091732850034));
#37900=CARTESIAN_POINT('Ctrl Pts',(-60.1984589793919,-55.5673454264546,
-7.19400069060905));
#37901=CARTESIAN_POINT('Ctrl Pts',(-62.2602755454619,-56.1814013752741,
-7.07708405271777));
#37902=CARTESIAN_POINT('Ctrl Pts',(-63.7907548567845,-57.6941990354335,
-6.96016741482647));
#37903=CARTESIAN_POINT('Ctrl Pts',(-64.4300090149408,-59.7468405219862,
-6.84325077693519));
#37904=CARTESIAN_POINT('Ctrl Pts',(-64.027951567412,-61.8638120783306,-6.72633413904389));
#37905=CARTESIAN_POINT('Ctrl Pts',(-62.6786998800996,-63.5322833334212,
-6.60941750115261));
#37906=CARTESIAN_POINT('Ctrl Pts',(-60.0407216297232,-64.6795907924263,
-6.45352865063089));
#37907=CARTESIAN_POINT('Ctrl Pts',(-56.338126950977,-63.4214738666151,-6.25866758747873));
#37908=CARTESIAN_POINT('Ctrl Pts',(-55.1221049933237,-58.8502443951291,
-6.02483431169616));
#37909=CARTESIAN_POINT('Ctrl Pts',(-57.7101825725057,-55.9187055503882,
-5.829973248544));
#37910=CARTESIAN_POINT('Ctrl Pts',(-60.5695480146307,-55.6036294907912,
-5.67408439802229));
#37911=CARTESIAN_POINT('Ctrl Pts',(-62.5694772512366,-56.3811637301305,
-5.557167760131));
#37912=CARTESIAN_POINT('Ctrl Pts',(-63.9702557757387,-58.0185513710953,
-5.44025112223971));
#37913=CARTESIAN_POINT('Ctrl Pts',(-64.4353953405457,-60.1175101930552,
-5.32333448434842));
#37914=CARTESIAN_POINT('Ctrl Pts',(-63.8588751961196,-62.1908042402258,
-5.20641784645712));
#37915=CARTESIAN_POINT('Ctrl Pts',(-62.374688451214,-63.7481551854853,-5.08950120856584));
#37916=CARTESIAN_POINT('Ctrl Pts',(-60.3324645667982,-64.4247771397016,
-4.97258457067455));
#37917=CARTESIAN_POINT('Ctrl Pts',(-58.211977347927,-64.0609880370046,-4.85566793278326));
#37918=CARTESIAN_POINT('Ctrl Pts',(-56.5118828933347,-62.7425958741262,
-4.73875129489197));
#37919=CARTESIAN_POINT('Ctrl Pts',(-55.6317837173695,-60.7794079817936,
-4.62183465700068));
#37920=CARTESIAN_POINT('Ctrl Pts',(-55.7786142136362,-58.6330092626113,
-4.50491801910939));
#37921=CARTESIAN_POINT('Ctrl Pts',(-56.9178409549638,-56.807965963808,-4.3880013812181));
#37922=CARTESIAN_POINT('Ctrl Pts',(-58.7816513959293,-55.7333386780497,
-4.27108474332682));
#37923=CARTESIAN_POINT('Ctrl Pts',(-60.9318810589847,-55.6617543020258,
-4.15416810543552));
#37924=CARTESIAN_POINT('Ctrl Pts',(-62.8630363094296,-56.6100443537648,
-4.03725146754423));
#37925=CARTESIAN_POINT('Ctrl Pts',(-64.1211231401667,-58.355275016248,-3.92033482965294));
#37926=CARTESIAN_POINT('Ctrl Pts',(-64.4103797861807,-60.4871625360835,
-3.80341819176165));
#37927=CARTESIAN_POINT('Ctrl Pts',(-63.662804640575,-62.5045233774706,-3.68650155387036));
#37928=CARTESIAN_POINT('Ctrl Pts',(-62.0541453235499,-63.933098699237,-3.56958491597908));
#37929=CARTESIAN_POINT('Ctrl Pts',(-59.9625778280873,-64.4370457120861,
-3.45266827808779));
#37930=CARTESIAN_POINT('Ctrl Pts',(-57.8798107750803,-63.897893141119,-3.3357516401965));
#37931=CARTESIAN_POINT('Ctrl Pts',(-56.295470437015,-62.4423875072701,-3.21883500230521));
#37932=CARTESIAN_POINT('Ctrl Pts',(-55.5820374288072,-60.4127070705911,
-3.10191836441392));
#37933=CARTESIAN_POINT('Ctrl Pts',(-55.9071888340358,-58.2859968821596,
-2.98500172652263));
#37934=CARTESIAN_POINT('Ctrl Pts',(-57.1945761362646,-56.5622472138891,
-2.86808508863134));
#37935=CARTESIAN_POINT('Ctrl Pts',(-59.141343048511,-55.6466485015553,-2.75116845074005));
#37936=CARTESIAN_POINT('Ctrl Pts',(-61.2902328481645,-55.7545784974516,
-2.63425181284876));
#37937=CARTESIAN_POINT('Ctrl Pts',(-62.5200516280627,-56.4918932825098,
-2.5563073875879));
#37938=CARTESIAN_POINT('Ctrl Pts',(-63.0124573356753,-56.9836661655686,
-2.51733517495747));
#37939=CARTESIAN_POINT('Ctrl Pts',(-63.4340590883905,-57.0277997563163,
-10.1608882750142));
#37940=CARTESIAN_POINT('Ctrl Pts',(-63.9192601452004,-57.5883976172362,
-10.1219160623837));
#37941=CARTESIAN_POINT('Ctrl Pts',(-64.6094001830892,-58.9512575723235,
-10.0439716371229));
#37942=CARTESIAN_POINT('Ctrl Pts',(-64.5609373474359,-61.2429908953152,
-9.92705499923159));
#37943=CARTESIAN_POINT('Ctrl Pts',(-63.4401580576473,-63.2422243560614,
-9.81013836134031));
#37944=CARTESIAN_POINT('Ctrl Pts',(-61.5106530599844,-64.4794023244967,
-9.69322172344902));
#37945=CARTESIAN_POINT('Ctrl Pts',(-59.2259964564264,-64.6634559351264,
-9.57630508555773));
#37946=CARTESIAN_POINT('Ctrl Pts',(-57.1233045831027,-63.7512147424712,
-9.45938844766644));
#37947=CARTESIAN_POINT('Ctrl Pts',(-55.6968892996459,-61.9570899468048,
-9.34247180977515));
#37948=CARTESIAN_POINT('Ctrl Pts',(-55.2820888551148,-59.7028817807907,
-9.22555517188386));
#37949=CARTESIAN_POINT('Ctrl Pts',(-55.9764165311997,-57.5185196797758,
-9.10863853399257));
#37950=CARTESIAN_POINT('Ctrl Pts',(-57.616644383502,-55.917527587839,-8.99172189610128));
#37951=CARTESIAN_POINT('Ctrl Pts',(-59.817172634626,-55.2762788743854,-8.87480525820999));
#37952=CARTESIAN_POINT('Ctrl Pts',(-62.0606816299573,-55.7455250310983,
-8.75788862031871));
#37953=CARTESIAN_POINT('Ctrl Pts',(-63.8197471636086,-57.2149509530668,
-8.64097198242741));
#37954=CARTESIAN_POINT('Ctrl Pts',(-64.6808324462795,-59.3391112434675,
-8.52405534453613));
#37955=CARTESIAN_POINT('Ctrl Pts',(-64.4415058356944,-61.6186389012925,
-8.40713870664484));
#37956=CARTESIAN_POINT('Ctrl Pts',(-63.1580303961144,-63.5176429879204,
-8.29022206875354));
#37957=CARTESIAN_POINT('Ctrl Pts',(-61.1321369456456,-64.5896870728554,
-8.17330543086226));
#37958=CARTESIAN_POINT('Ctrl Pts',(-58.8400906988581,-64.5827488714692,
-8.05638879297096));
#37959=CARTESIAN_POINT('Ctrl Pts',(-56.8207261478351,-63.4984521313852,
-7.93947215507967));
#37960=CARTESIAN_POINT('Ctrl Pts',(-55.5487739765082,-61.5917188670885,
-7.82255551718839));
#37961=CARTESIAN_POINT('Ctrl Pts',(-55.3232551151952,-59.3107667224756,
-7.7056388792971));
#37962=CARTESIAN_POINT('Ctrl Pts',(-56.1971885854583,-57.1918962160405,
-7.58872224140581));
#37963=CARTESIAN_POINT('Ctrl Pts',(-57.9651179142938,-55.7330707246297,
-7.47180560351452));
#37964=CARTESIAN_POINT('Ctrl Pts',(-60.2114319801559,-55.277588664903,-7.35488896562322));
#37965=CARTESIAN_POINT('Ctrl Pts',(-62.4080267657298,-55.9317846382132,
-7.23797232773194));
#37966=CARTESIAN_POINT('Ctrl Pts',(-64.0385514835944,-57.543471878785,-7.12105568984065));
#37967=CARTESIAN_POINT('Ctrl Pts',(-64.7195928398286,-59.7302918220393,
-7.00413905194936));
#37968=CARTESIAN_POINT('Ctrl Pts',(-64.2912534291961,-61.985647006588,-6.88722241405807));
#37969=CARTESIAN_POINT('Ctrl Pts',(-62.8538029452151,-63.7631840189119,
-6.77030577616678));
#37970=CARTESIAN_POINT('Ctrl Pts',(-60.0433835487511,-64.9854894477136,
-6.61441692564506));
#37971=CARTESIAN_POINT('Ctrl Pts',(-56.0987551573276,-63.6451310839495,
-6.41955586249291));
#37972=CARTESIAN_POINT('Ctrl Pts',(-54.8032434540649,-58.7750863932782,
-6.18572258671033));
#37973=CARTESIAN_POINT('Ctrl Pts',(-57.5605002385166,-55.6519167350097,
-5.99086152355818));
#37974=CARTESIAN_POINT('Ctrl Pts',(-60.606778614383,-55.3162445704927,-5.83497267303647));
#37975=CARTESIAN_POINT('Ctrl Pts',(-62.7374405776916,-56.1446051937624,
-5.71805603514518));
#37976=CARTESIAN_POINT('Ctrl Pts',(-64.2297861399983,-57.8890266972534,
-5.60113939725388));
#37977=CARTESIAN_POINT('Ctrl Pts',(-64.7253312624079,-60.1251916788159,
-5.4842227593626));
#37978=CARTESIAN_POINT('Ctrl Pts',(-64.1111247593346,-62.3340142132361,
-5.3673061214713));
#37979=CARTESIAN_POINT('Ctrl Pts',(-62.5299186916718,-63.9931671281756,
-5.25038948358002));
#37980=CARTESIAN_POINT('Ctrl Pts',(-60.3541973354151,-64.714018963831,-5.13347284568873));
#37981=CARTESIAN_POINT('Ctrl Pts',(-58.0950966741345,-64.3264494490725,
-5.01655620779744));
#37982=CARTESIAN_POINT('Ctrl Pts',(-56.28386929562,-62.9218757357862,-4.89963956990615));
#37983=CARTESIAN_POINT('Ctrl Pts',(-55.3462392015919,-60.8303568497879,
-4.78272293201486));
#37984=CARTESIAN_POINT('Ctrl Pts',(-55.5026678130263,-58.5436508877221,
-4.66580629412357));
#37985=CARTESIAN_POINT('Ctrl Pts',(-56.7163642983331,-56.5993069244573,
-4.54888965623228));
#37986=CARTESIAN_POINT('Ctrl Pts',(-58.7020095605236,-55.454432675614,-4.43197301834099));
#37987=CARTESIAN_POINT('Ctrl Pts',(-60.9927968901921,-55.3781689236924,
-4.3150563804497));
#37988=CARTESIAN_POINT('Ctrl Pts',(-63.050189202907,-56.3884474407729,-4.19813974255841));
#37989=CARTESIAN_POINT('Ctrl Pts',(-64.3905155043218,-58.247761521337,-4.08122310466712));
#37990=CARTESIAN_POINT('Ctrl Pts',(-64.6986804743695,-60.5190077061645,
-3.96430646677583));
#37991=CARTESIAN_POINT('Ctrl Pts',(-63.902237331131,-62.668240755183,-3.84738982888454));
#37992=CARTESIAN_POINT('Ctrl Pts',(-62.1884220840853,-64.1902001545941,
-3.73047319099325));
#37993=CARTESIAN_POINT('Ctrl Pts',(-59.9601315902486,-64.7270895165512,
-3.61355655310196));
#37994=CARTESIAN_POINT('Ctrl Pts',(-57.7412168121408,-64.1526932557469,
-3.49663991521067));
#37995=CARTESIAN_POINT('Ctrl Pts',(-56.0533102435163,-62.6020431454028,
-3.37972327731938));
#37996=CARTESIAN_POINT('Ctrl Pts',(-55.2932410640001,-60.4396851854566,
-3.2628066394281));
#37997=CARTESIAN_POINT('Ctrl Pts',(-55.6396471861552,-58.1739547673332,
-3.1458900015368));
#37998=CARTESIAN_POINT('Ctrl Pts',(-57.0111892920952,-56.3375258651372,
-3.02897336364551));
#37999=CARTESIAN_POINT('Ctrl Pts',(-59.085213780277,-55.362075677042,-2.91205672575423));
#38000=CARTESIAN_POINT('Ctrl Pts',(-61.3745736614467,-55.477060913893,-2.79514008786294));
#38001=CARTESIAN_POINT('Ctrl Pts',(-62.6847840669602,-56.2625729903977,
-2.71719566260208));
#38002=CARTESIAN_POINT('Ctrl Pts',(-63.2093776838358,-56.7864924158161,
-2.67822344997165));
#38003=CARTESIAN_POINT('Ctrl Pts',(-63.6447653928232,-56.845432093658,-10.3217765500284));
#38004=CARTESIAN_POINT('Ctrl Pts',(-64.1597373181463,-57.44042700498,-10.2828043373979));
#38005=CARTESIAN_POINT('Ctrl Pts',(-64.8922228291855,-58.8869090461189,
-10.2048599121371));
#38006=CARTESIAN_POINT('Ctrl Pts',(-64.8407864206437,-61.3192580797911,
-10.0879432742458));
#38007=CARTESIAN_POINT('Ctrl Pts',(-63.6512385814046,-63.4411601037068,
-9.97102663635448));
#38008=CARTESIAN_POINT('Ctrl Pts',(-61.6033434055365,-64.7542485882237,
-9.8541099984632));
#38009=CARTESIAN_POINT('Ctrl Pts',(-59.1785053032208,-64.9495953231459,
-9.73719336057191));
#38010=CARTESIAN_POINT('Ctrl Pts',(-56.9467968863301,-63.9813810195139,
-9.62027672268061));
#38011=CARTESIAN_POINT('Ctrl Pts',(-55.4328599018113,-62.0771726767518,
-9.50336008478933));
#38012=CARTESIAN_POINT('Ctrl Pts',(-54.9926082153259,-59.6846512610652,
-9.38644344689804));
#38013=CARTESIAN_POINT('Ctrl Pts',(-55.7295383088205,-57.3662615111368,
-9.26952680900675));
#38014=CARTESIAN_POINT('Ctrl Pts',(-57.4704069306292,-55.6670360695589,
-9.15261017111546));
#38015=CARTESIAN_POINT('Ctrl Pts',(-59.8059547500423,-54.9864417469716,
-9.03569353322417));
#38016=CARTESIAN_POINT('Ctrl Pts',(-62.1871205174909,-55.4844798146578,
-8.91877689533288));
#38017=CARTESIAN_POINT('Ctrl Pts',(-64.0541184391152,-57.0440664757651,
-8.80186025744159));
#38018=CARTESIAN_POINT('Ctrl Pts',(-64.9680380187631,-59.2985605645345,
-8.6849436195503));
#38019=CARTESIAN_POINT('Ctrl Pts',(-64.7140268543102,-61.7179550203003,
-8.56802698165901));
#38020=CARTESIAN_POINT('Ctrl Pts',(-63.3518001877586,-63.7334778163903,
-8.45111034376772));
#38021=CARTESIAN_POINT('Ctrl Pts',(-61.2016023758519,-64.8713001659127,
-8.33419370587643));
#38022=CARTESIAN_POINT('Ctrl Pts',(-58.7689212180688,-64.8639362517664,
-8.21727706798514));
#38023=CARTESIAN_POINT('Ctrl Pts',(-56.6256529045023,-63.7131094511532,
-8.10036043009385));
#38024=CARTESIAN_POINT('Ctrl Pts',(-55.2756565485713,-61.689383232071,-7.98344379220256));
#38025=CARTESIAN_POINT('Ctrl Pts',(-55.0363003464836,-59.2684768861445,
-7.86652715431127));
#38026=CARTESIAN_POINT('Ctrl Pts',(-55.9638564502248,-57.0195971508376,
-7.74961051641999));
#38027=CARTESIAN_POINT('Ctrl Pts',(-57.8402620299891,-55.4712613393666,
-7.63269387852869));
#38028=CARTESIAN_POINT('Ctrl Pts',(-60.22440498092,-54.9878319033513,-7.51577724063741));
#38029=CARTESIAN_POINT('Ctrl Pts',(-62.5557779859977,-55.6821679011524,
-7.39886060274612));
#38030=CARTESIAN_POINT('Ctrl Pts',(-64.2863481104043,-57.3927447221366,
-7.28194396485483));
#38031=CARTESIAN_POINT('Ctrl Pts',(-65.0091766647164,-59.7137431220925,
-7.16502732696354));
#38032=CARTESIAN_POINT('Ctrl Pts',(-64.5545552909801,-62.1074819348455,
-7.04811068907225));
#38033=CARTESIAN_POINT('Ctrl Pts',(-63.0289060103307,-63.9940847044025,
-6.93119405118096));
#38034=CARTESIAN_POINT('Ctrl Pts',(-60.046045467779,-65.2913881030008,-6.77530520065924));
#38035=CARTESIAN_POINT('Ctrl Pts',(-55.8593833636781,-63.868788301284,-6.58044413750708));
#38036=CARTESIAN_POINT('Ctrl Pts',(-54.484381914806,-58.6999283914272,-6.34661086172452));
#38037=CARTESIAN_POINT('Ctrl Pts',(-57.4108179045277,-55.3851279196312,
-6.15174979857236));
#38038=CARTESIAN_POINT('Ctrl Pts',(-60.6440092141352,-55.0288596501941,
-5.99586094805064));
#38039=CARTESIAN_POINT('Ctrl Pts',(-62.9054039041467,-55.9080466573944,
-5.87894431015935));
#38040=CARTESIAN_POINT('Ctrl Pts',(-64.4893165042581,-57.7595020234115,
-5.76202767226806));
#38041=CARTESIAN_POINT('Ctrl Pts',(-65.0152671842702,-60.1328731645767,
-5.64511103437677));
#38042=CARTESIAN_POINT('Ctrl Pts',(-64.3633743225495,-62.4772241862465,
-5.52819439648548));
#38043=CARTESIAN_POINT('Ctrl Pts',(-62.6851489321296,-64.2381790708658,
-5.41127775859419));
#38044=CARTESIAN_POINT('Ctrl Pts',(-60.3759301040322,-65.0032607879604,
-5.2943611207029));
#38045=CARTESIAN_POINT('Ctrl Pts',(-57.9782160003419,-64.5919108611403,
-5.17744448281161));
#38046=CARTESIAN_POINT('Ctrl Pts',(-56.0558556979054,-63.1011555974462,
-5.06052784492032));
#38047=CARTESIAN_POINT('Ctrl Pts',(-55.0606946858144,-60.8813057177822,
-4.94361120702903));
#38048=CARTESIAN_POINT('Ctrl Pts',(-55.2267214124163,-58.454292512833,-4.82669456913775));
#38049=CARTESIAN_POINT('Ctrl Pts',(-56.5148876417024,-56.3906478851065,
-4.70977793124645));
#38050=CARTESIAN_POINT('Ctrl Pts',(-58.6223677251179,-55.1755266731783,
-4.59286129335517));
#38051=CARTESIAN_POINT('Ctrl Pts',(-61.0537127213995,-55.0945835453589,
-4.47594465546388));
#38052=CARTESIAN_POINT('Ctrl Pts',(-63.2373420963845,-56.1668505277811,
-4.35902801757259));
#38053=CARTESIAN_POINT('Ctrl Pts',(-64.6599078684769,-58.1402480264261,
-4.2421113796813));
#38054=CARTESIAN_POINT('Ctrl Pts',(-64.9869811625584,-60.5508528762455,
-4.12519474179001));
#38055=CARTESIAN_POINT('Ctrl Pts',(-64.141670021687,-62.8319581328956,-4.00827810389872));
#38056=CARTESIAN_POINT('Ctrl Pts',(-62.3226988446208,-64.4473016099512,
-3.89136146600743));
#38057=CARTESIAN_POINT('Ctrl Pts',(-59.9576853524099,-65.0171333210163,
-3.77444482811614));
#38058=CARTESIAN_POINT('Ctrl Pts',(-57.6026228492013,-64.4074933703747,
-3.65752819022485));
#38059=CARTESIAN_POINT('Ctrl Pts',(-55.8111500500176,-62.7616987835354,
-3.54061155233356));
#38060=CARTESIAN_POINT('Ctrl Pts',(-55.0044446991931,-60.466663300322,-3.42369491444227));
#38061=CARTESIAN_POINT('Ctrl Pts',(-55.3721055382745,-58.0619126525068,
-3.30677827655098));
#38062=CARTESIAN_POINT('Ctrl Pts',(-56.8278024479258,-56.1128045163852,
-3.18986163865969));
#38063=CARTESIAN_POINT('Ctrl Pts',(-59.029084512043,-55.0775028525288,-3.0729450007684));
#38064=CARTESIAN_POINT('Ctrl Pts',(-61.4589144747288,-55.1995433303345,
-2.95602836287711));
#38065=CARTESIAN_POINT('Ctrl Pts',(-62.8495165058577,-56.0332526982856,
-2.87808393761625));
#38066=CARTESIAN_POINT('Ctrl Pts',(-63.4062980319963,-56.5893186660636,
-2.83911172498582));
#38067=CARTESIAN_POINT('Ctrl Pts',(-63.8554716972558,-56.6630644309997,
-10.4826648250425));
#38068=CARTESIAN_POINT('Ctrl Pts',(-64.4002144910922,-57.2924563927238,
-10.4436926124121));
#38069=CARTESIAN_POINT('Ctrl Pts',(-65.1750454752818,-58.8225605199143,
-10.3657481871512));
#38070=CARTESIAN_POINT('Ctrl Pts',(-65.1206354938515,-61.3955252642669,
-10.24883154926));
#38071=CARTESIAN_POINT('Ctrl Pts',(-63.8623191051618,-63.6400958513521,
-10.1319149113687));
#38072=CARTESIAN_POINT('Ctrl Pts',(-61.6960337510886,-65.0290948519505,
-10.0149982734774));
#38073=CARTESIAN_POINT('Ctrl Pts',(-59.131014150015,-65.2357347111654,-9.89808163558608));
#38074=CARTESIAN_POINT('Ctrl Pts',(-56.7702891895575,-64.2115472965565,
-9.78116499769479));
#38075=CARTESIAN_POINT('Ctrl Pts',(-55.1688305039767,-62.1972554066989,
-9.6642483598035));
#38076=CARTESIAN_POINT('Ctrl Pts',(-54.703127575537,-59.6664207413398,-9.54733172191222));
#38077=CARTESIAN_POINT('Ctrl Pts',(-55.4826600864412,-57.2140033424977,
-9.43041508402093));
#38078=CARTESIAN_POINT('Ctrl Pts',(-57.3241694777564,-55.4165445512788,
-9.31349844612963));
#38079=CARTESIAN_POINT('Ctrl Pts',(-59.7947368654586,-54.6966046195577,
-9.19658180823835));
#38080=CARTESIAN_POINT('Ctrl Pts',(-62.3135594050244,-55.2234345982174,
-9.07966517034706));
#38081=CARTESIAN_POINT('Ctrl Pts',(-64.2884897146217,-56.8731819984634,
-8.96274853245577));
#38082=CARTESIAN_POINT('Ctrl Pts',(-65.2552435912467,-59.2580098856016,
-8.84583189456447));
#38083=CARTESIAN_POINT('Ctrl Pts',(-64.986547872926,-61.817271139308,-8.72891525667319));
#38084=CARTESIAN_POINT('Ctrl Pts',(-63.5455699794028,-63.9493126448601,
-8.6119986187819));
#38085=CARTESIAN_POINT('Ctrl Pts',(-61.2710678060581,-65.1529132589701,
-8.49508198089061));
#38086=CARTESIAN_POINT('Ctrl Pts',(-58.6977517372794,-65.1451236320635,
-8.37816534299932));
#38087=CARTESIAN_POINT('Ctrl Pts',(-56.4305796611695,-63.9277667709211,
-8.26124870510803));
#38088=CARTESIAN_POINT('Ctrl Pts',(-55.0025391206345,-61.7870475970534,
-8.14433206721674));
#38089=CARTESIAN_POINT('Ctrl Pts',(-54.7493455777719,-59.2261870498135,
-8.02741542932545));
#38090=CARTESIAN_POINT('Ctrl Pts',(-55.7305243149913,-56.8472980856346,
-7.91049879143416));
#38091=CARTESIAN_POINT('Ctrl Pts',(-57.7154061456845,-55.2094519541036,
-7.79358215354287));
#38092=CARTESIAN_POINT('Ctrl Pts',(-60.2373779816841,-54.6980751417997,
-7.67666551565158));
#38093=CARTESIAN_POINT('Ctrl Pts',(-62.7035292062656,-55.4325511640916,
-7.55974887776029));
#38094=CARTESIAN_POINT('Ctrl Pts',(-64.5341447372141,-57.2420175654881,
-7.442832239869));
#38095=CARTESIAN_POINT('Ctrl Pts',(-65.2987604896043,-59.6971944221457,
-7.32591560197771));
#38096=CARTESIAN_POINT('Ctrl Pts',(-64.8178571527642,-62.229316863103,-7.20899896408642));
#38097=CARTESIAN_POINT('Ctrl Pts',(-63.2040090754463,-64.2249853898932,
-7.09208232619513));
#38098=CARTESIAN_POINT('Ctrl Pts',(-60.048707386807,-65.597286758288,-6.93619347567342));
#38099=CARTESIAN_POINT('Ctrl Pts',(-55.6200115700286,-64.0924455186184,
-6.74133241252126));
#38100=CARTESIAN_POINT('Ctrl Pts',(-54.1655203755472,-58.6247703895763,
-6.50749913673869));
#38101=CARTESIAN_POINT('Ctrl Pts',(-57.2611355705387,-55.1183391042526,
-6.31263807358654));
#38102=CARTESIAN_POINT('Ctrl Pts',(-60.6812398138874,-54.7414747298955,
-6.15674922306482));
#38103=CARTESIAN_POINT('Ctrl Pts',(-63.0733672306018,-55.6714881210263,
-6.03983258517353));
#38104=CARTESIAN_POINT('Ctrl Pts',(-64.7488468685178,-57.6299773495695,
-5.92291594728224));
#38105=CARTESIAN_POINT('Ctrl Pts',(-65.3052031061324,-60.1405546503375,
-5.80599930939095));
#38106=CARTESIAN_POINT('Ctrl Pts',(-64.6156238857644,-62.6204341592567,
-5.68908267149966));
#38107=CARTESIAN_POINT('Ctrl Pts',(-62.8403791725874,-64.4831910135561,
-5.57216603360837));
#38108=CARTESIAN_POINT('Ctrl Pts',(-60.3976628726492,-65.2925026120897,
-5.45524939571708));
#38109=CARTESIAN_POINT('Ctrl Pts',(-57.8613353265494,-64.8573722732082,
-5.33833275782579));
#38110=CARTESIAN_POINT('Ctrl Pts',(-55.8278421001908,-63.2804354591061,
-5.2214161199345));
#38111=CARTESIAN_POINT('Ctrl Pts',(-54.7751501700368,-60.9322545857766,
-5.10449948204321));
#38112=CARTESIAN_POINT('Ctrl Pts',(-54.9507750118064,-58.3649341379439,
-4.98758284415192));
#38113=CARTESIAN_POINT('Ctrl Pts',(-56.3134109850716,-56.1819888457558,
-4.87066620626063));
#38114=CARTESIAN_POINT('Ctrl Pts',(-58.5427258897122,-54.8966206707426,
-4.75374956836934));
#38115=CARTESIAN_POINT('Ctrl Pts',(-61.1146285526069,-54.8109981670255,
-4.63683293047805));
#38116=CARTESIAN_POINT('Ctrl Pts',(-63.424494989862,-55.9452536147892,-4.51991629258676));
#38117=CARTESIAN_POINT('Ctrl Pts',(-64.9293002326319,-58.0327345315151,
-4.40299965469548));
#38118=CARTESIAN_POINT('Ctrl Pts',(-65.2752818507472,-60.5826980463265,
-4.28608301680418));
#38119=CARTESIAN_POINT('Ctrl Pts',(-64.381102712243,-62.9956755106081,-4.16916637891289));
#38120=CARTESIAN_POINT('Ctrl Pts',(-62.4569756051562,-64.7044030653083,
-4.0522497410216));
#38121=CARTESIAN_POINT('Ctrl Pts',(-59.9552391145712,-65.3071771254814,
-3.93533310313031));
#38122=CARTESIAN_POINT('Ctrl Pts',(-57.4640288862619,-64.6622934850025,
-3.81841646523903));
#38123=CARTESIAN_POINT('Ctrl Pts',(-55.5689898565188,-62.921354421668,-3.70149982734774));
#38124=CARTESIAN_POINT('Ctrl Pts',(-54.7156483343861,-60.4936414151875,
-3.58458318945645));
#38125=CARTESIAN_POINT('Ctrl Pts',(-55.1045638903938,-57.9498705376805,
-3.46766655156516));
#38126=CARTESIAN_POINT('Ctrl Pts',(-56.6444156037563,-55.8880831676333,
-3.35074991367387));
#38127=CARTESIAN_POINT('Ctrl Pts',(-58.972955243809,-54.7929300280156,-3.23383327578258));
#38128=CARTESIAN_POINT('Ctrl Pts',(-61.543255288011,-54.9220257467759,-3.11691663789129));
#38129=CARTESIAN_POINT('Ctrl Pts',(-63.0142489447553,-55.8039324061734,
-3.03897221263043));
#38130=CARTESIAN_POINT('Ctrl Pts',(-63.6032183801568,-56.3921449163111,
-3.));
#38131=CARTESIAN_POINT('Ctrl Pts',(-63.2233527839579,-57.2101674189746,
-10.));
#38132=CARTESIAN_POINT('Ctrl Pts',(-63.3163082537287,-57.298636481893,-10.));
#38133=CARTESIAN_POINT('Ctrl Pts',(-63.4049730938493,-57.3912022376077,
-10.));
#38134=CARTESIAN_POINT('Ctrl Pts',(-63.4892289732812,-57.487446019035,-10.));
#38135=CARTESIAN_POINT('Ctrl Pts',(-63.575043820607,-57.5854705778544,-10.));
#38136=CARTESIAN_POINT('Ctrl Pts',(-63.6562855651475,-57.6873109425664,
-10.));
#38137=CARTESIAN_POINT('Ctrl Pts',(-63.7328062531653,-57.7925737185367,
-10.));
#38138=CARTESIAN_POINT('Ctrl Pts',(-63.8104264609581,-57.8993490070937,
-10.));
#38139=CARTESIAN_POINT('Ctrl Pts',(-63.8831895396106,-58.0096462773425,
-10.));
#38140=CARTESIAN_POINT('Ctrl Pts',(-63.9509093234047,-58.1230977274475,
-10.));
#38141=CARTESIAN_POINT('Ctrl Pts',(-64.0184811880466,-58.2363013675129,
-10.));
#38142=CARTESIAN_POINT('Ctrl Pts',(-64.0810322758665,-58.3526460671589,
-10.));
#38143=CARTESIAN_POINT('Ctrl Pts',(-64.138338222228,-58.4717998619651,-10.));
#38144=CARTESIAN_POINT('Ctrl Pts',(-64.1498927790088,-58.4958247559796,
-10.));
#38145=CARTESIAN_POINT('Ctrl Pts',(-64.1612339549976,-58.5199639426201,
-10.));
#38146=CARTESIAN_POINT('Ctrl Pts',(-64.1723596873146,-58.5442148295044,
-10.));
#38147=CARTESIAN_POINT('Ctrl Pts',(-64.182565209477,-58.5664599237149,-10.));
#38148=CARTESIAN_POINT('Ctrl Pts',(-64.1925913312984,-58.5888035036185,
-10.));
#38149=CARTESIAN_POINT('Ctrl Pts',(-64.2024245248804,-58.6112158820566,
-10.));
#38150=CARTESIAN_POINT('Ctrl Pts',(-64.2596370057899,-58.7416178478921,
-10.));
#38151=CARTESIAN_POINT('Ctrl Pts',(-64.3103966435791,-58.8745017637267,
-10.));
#38152=CARTESIAN_POINT('Ctrl Pts',(-64.3545198337919,-59.0093933578834,
-10.));
#38153=CARTESIAN_POINT('Ctrl Pts',(-64.3960229534372,-59.1362749805502,
-10.));
#38154=CARTESIAN_POINT('Ctrl Pts',(-64.4316549185973,-59.2649338691195,
-10.));
#38155=CARTESIAN_POINT('Ctrl Pts',(-64.4614760968299,-59.39494826094,-10.));
#38156=CARTESIAN_POINT('Ctrl Pts',(-64.491676772499,-59.5266171859255,-10.));
#38157=CARTESIAN_POINT('Ctrl Pts',(-64.5159180688999,-59.6596770266619,
-10.));
#38158=CARTESIAN_POINT('Ctrl Pts',(-64.5342156697401,-59.7937149390323,
-10.));
#38159=CARTESIAN_POINT('Ctrl Pts',(-64.5504251659969,-59.9124565739497,
-10.));
#38160=CARTESIAN_POINT('Ctrl Pts',(-64.5619695449417,-60.0319664972129,
-10.));
#38161=CARTESIAN_POINT('Ctrl Pts',(-64.5688272622564,-60.1519670666326,
-10.));
#38162=CARTESIAN_POINT('Ctrl Pts',(-64.570543909647,-60.182006022003,-10.));
#38163=CARTESIAN_POINT('Ctrl Pts',(-64.5719667292107,-60.2120757463558,
-10.));
#38164=CARTESIAN_POINT('Ctrl Pts',(-64.5730950735929,-60.2421719198664,
-10.));
#38165=CARTESIAN_POINT('Ctrl Pts',(-64.5739024340997,-60.2637065349035,
-10.));
#38166=CARTESIAN_POINT('Ctrl Pts',(-64.5745589909509,-60.2852564219846,
-10.));
#38167=CARTESIAN_POINT('Ctrl Pts',(-64.5750641911246,-60.3067984108421,
-10.));
#38168=CARTESIAN_POINT('Ctrl Pts',(-64.5783094538577,-60.4451780418628,
-10.));
#38169=CARTESIAN_POINT('Ctrl Pts',(-64.5753216877452,-60.5834277992512,
-10.));
#38170=CARTESIAN_POINT('Ctrl Pts',(-64.5661669987375,-60.721106961686,-10.));
#38171=CARTESIAN_POINT('Ctrl Pts',(-64.5569093304397,-60.8603348498496,
-10.));
#38172=CARTESIAN_POINT('Ctrl Pts',(-64.5413454334492,-60.9989800078359,
-10.));
#38173=CARTESIAN_POINT('Ctrl Pts',(-64.5194941721477,-61.1366051442133,
-10.));
#38174=CARTESIAN_POINT('Ctrl Pts',(-64.5146774260464,-61.1669423101068,
-10.));
#38175=CARTESIAN_POINT('Ctrl Pts',(-64.5095549756123,-61.1972299566409,
-10.));
#38176=CARTESIAN_POINT('Ctrl Pts',(-64.5041266879631,-61.2274634597029,
-10.));
#38177=CARTESIAN_POINT('Ctrl Pts',(-64.4796518086955,-61.3637792530247,
-10.));
#38178=CARTESIAN_POINT('Ctrl Pts',(-64.4489637718321,-61.4989945357919,
-10.));
#38179=CARTESIAN_POINT('Ctrl Pts',(-64.4122747073138,-61.6327571482726,
-10.));
#38180=CARTESIAN_POINT('Ctrl Pts',(-64.3910362736552,-61.7101891680984,
-10.));
#38181=CARTESIAN_POINT('Ctrl Pts',(-64.3677859193463,-61.7871343917435,
-10.));
#38182=CARTESIAN_POINT('Ctrl Pts',(-64.3425569349254,-61.8635234393916,
-10.));
#38183=CARTESIAN_POINT('Ctrl Pts',(-64.3288269090093,-61.9050956083867,
-10.));
#38184=CARTESIAN_POINT('Ctrl Pts',(-64.3145107713356,-61.9465030334659,
-10.));
#38185=CARTESIAN_POINT('Ctrl Pts',(-64.2996131993035,-61.9877343379993,
-10.));
#38186=CARTESIAN_POINT('Ctrl Pts',(-64.2935454976476,-62.0045276284934,
-10.));
#38187=CARTESIAN_POINT('Ctrl Pts',(-64.2873813369501,-62.0212917006638,
-10.));
#38188=CARTESIAN_POINT('Ctrl Pts',(-64.2811210106928,-62.0380257775647,
-10.));
#38189=CARTESIAN_POINT('Ctrl Pts',(-64.2745734824793,-62.0555275556084,
-10.));
#38190=CARTESIAN_POINT('Ctrl Pts',(-64.2679239993545,-62.0729878447327,
-10.));
#38191=CARTESIAN_POINT('Ctrl Pts',(-64.2611741070867,-62.0904035730928,
-10.));
#38192=CARTESIAN_POINT('Ctrl Pts',(-64.2098991667657,-62.2227005634568,
-10.));
#38193=CARTESIAN_POINT('Ctrl Pts',(-64.1528186317814,-62.352468261667,-10.));
#38194=CARTESIAN_POINT('Ctrl Pts',(-64.090210802814,-62.4793487889625,-10.));
#38195=CARTESIAN_POINT('Ctrl Pts',(-64.0269891380834,-62.6074733109243,
-10.));
#38196=CARTESIAN_POINT('Ctrl Pts',(-63.9581310871743,-62.7326545166747,
-10.));
#38197=CARTESIAN_POINT('Ctrl Pts',(-63.8838698879073,-62.8545209615278,
-10.));
#38198=CARTESIAN_POINT('Ctrl Pts',(-63.8095390814517,-62.976501635355,-10.));
#38199=CARTESIAN_POINT('Ctrl Pts',(-63.7297947366439,-63.0951621008321,
-10.));
#38200=CARTESIAN_POINT('Ctrl Pts',(-63.6448209579058,-63.2101155285558,
-10.));
#38201=CARTESIAN_POINT('Ctrl Pts',(-63.6122160490883,-63.2542237944803,
-10.));
#38202=CARTESIAN_POINT('Ctrl Pts',(-63.5788407107611,-63.2977860624708,
-10.));
#38203=CARTESIAN_POINT('Ctrl Pts',(-63.5447035224235,-63.3407795482112,
-10.));
#38204=CARTESIAN_POINT('Ctrl Pts',(-63.481542259528,-63.4203268978285,-10.));
#38205=CARTESIAN_POINT('Ctrl Pts',(-63.415773551013,-63.4979276395244,-10.));
#38206=CARTESIAN_POINT('Ctrl Pts',(-63.3475133975382,-63.573497256696,-10.));
#38207=CARTESIAN_POINT('Ctrl Pts',(-63.3334676325742,-63.589047076425,-10.));
#38208=CARTESIAN_POINT('Ctrl Pts',(-63.3193163436957,-63.6045108685033,
-10.));
#38209=CARTESIAN_POINT('Ctrl Pts',(-63.3050604888266,-63.6198878504331,
-10.));
#38210=CARTESIAN_POINT('Ctrl Pts',(-63.2906483457391,-63.635433411598,-10.));
#38211=CARTESIAN_POINT('Ctrl Pts',(-63.2761359992246,-63.6508830429282,
-10.));
#38212=CARTESIAN_POINT('Ctrl Pts',(-63.2615262241673,-63.66623462277,-10.));
#38213=CARTESIAN_POINT('Ctrl Pts',(-63.1618951272996,-63.7709244439543,
-10.));
#38214=CARTESIAN_POINT('Ctrl Pts',(-63.0577151953492,-63.8710796986466,
-10.));
#38215=CARTESIAN_POINT('Ctrl Pts',(-62.9493854968739,-63.9665039076976,
-10.));
#38216=CARTESIAN_POINT('Ctrl Pts',(-62.8507323508008,-64.0534043474378,
-10.));
#38217=CARTESIAN_POINT('Ctrl Pts',(-62.7486367875531,-64.1363812377739,
-10.));
#38218=CARTESIAN_POINT('Ctrl Pts',(-62.6433691057641,-64.2152667242994,
-10.));
#38219=CARTESIAN_POINT('Ctrl Pts',(-62.5878604519608,-64.256863794618,-10.));
#38220=CARTESIAN_POINT('Ctrl Pts',(-62.5314693108184,-64.297322886992,-10.));
#38221=CARTESIAN_POINT('Ctrl Pts',(-62.4742324962258,-64.3366168410067,
-10.));
#38222=CARTESIAN_POINT('Ctrl Pts',(-62.4525293526399,-64.3515163830604,
-10.));
#38223=CARTESIAN_POINT('Ctrl Pts',(-62.4307046009612,-64.366248383477,-10.));
#38224=CARTESIAN_POINT('Ctrl Pts',(-62.4087601835023,-64.3808112872915,
-10.));
#38225=CARTESIAN_POINT('Ctrl Pts',(-62.3869960059937,-64.3952545790422,
-10.));
#38226=CARTESIAN_POINT('Ctrl Pts',(-62.3651201351428,-64.4095275023171,
-10.));
#38227=CARTESIAN_POINT('Ctrl Pts',(-62.3431409677063,-64.4236248482937,
-10.));
#38228=CARTESIAN_POINT('Ctrl Pts',(-62.2178094000758,-64.5040119910634,
-10.));
#38229=CARTESIAN_POINT('Ctrl Pts',(-62.0890600530759,-64.5787341474093,
-10.));
#38230=CARTESIAN_POINT('Ctrl Pts',(-61.9572867191326,-64.6475637787053,
-10.));
#38231=CARTESIAN_POINT('Ctrl Pts',(-61.8473201863352,-64.7050029864785,
-10.));
#38232=CARTESIAN_POINT('Ctrl Pts',(-61.7352467477612,-64.7583382089978,
-10.));
#38233=CARTESIAN_POINT('Ctrl Pts',(-61.6212758651111,-64.8074173245507,
-10.));
#38234=CARTESIAN_POINT('Ctrl Pts',(-61.5232159544034,-64.8496447213806,
-10.));
#38235=CARTESIAN_POINT('Ctrl Pts',(-61.4237510374481,-64.8887212067715,
-10.));
#38236=CARTESIAN_POINT('Ctrl Pts',(-61.3230392926944,-64.9246350552985,
-10.));
#38237=CARTESIAN_POINT('Ctrl Pts',(-55.7371269462215,-59.9999021904687,
-7.57968167058906));
#38238=CARTESIAN_POINT('Ctrl Pts',(-55.7375457064891,-60.487939361417,-7.60701019445078));
#38239=CARTESIAN_POINT('Ctrl Pts',(-55.8213219914856,-60.9761189733716,
-7.63433871831249));
#38240=CARTESIAN_POINT('Ctrl Pts',(-55.9855958154758,-61.4355115631413,
-7.66166724217421));
#38241=CARTESIAN_POINT('Ctrl Pts',(-56.2198607333526,-62.0906346052765,
-7.70063945480464));
#38242=CARTESIAN_POINT('Ctrl Pts',(-56.6178300622603,-62.6872147084469,
-7.73961166743507));
#38243=CARTESIAN_POINT('Ctrl Pts',(-57.1327248581274,-63.1551325399579,
-7.7785838800655));
#38244=CARTESIAN_POINT('Ctrl Pts',(-57.6476196539944,-63.6230503714689,
-7.81755609269593));
#38245=CARTESIAN_POINT('Ctrl Pts',(-58.2794399168209,-63.9623059313205,
-7.85652830532636));
#38246=CARTESIAN_POINT('Ctrl Pts',(-58.9539186041995,-64.1330191260173,
-7.89550051795679));
#38247=CARTESIAN_POINT('Ctrl Pts',(-59.6283972915781,-64.3037323207141,
-7.93447273058722));
#38248=CARTESIAN_POINT('Ctrl Pts',(-60.3455344035087,-64.305903150256,-7.97344494321765));
#38249=CARTESIAN_POINT('Ctrl Pts',(-61.0210344743125,-64.1392775949691,
-8.01241715584808));
#38250=CARTESIAN_POINT('Ctrl Pts',(-61.6965345451164,-63.9726520396822,
-8.05138936847851));
#38251=CARTESIAN_POINT('Ctrl Pts',(-62.3303975747933,-63.6372300995664,
-8.09036158110894));
#38252=CARTESIAN_POINT('Ctrl Pts',(-62.8481164583998,-63.1724382333142,
-8.12933379373937));
#38253=CARTESIAN_POINT('Ctrl Pts',(-63.3658353420063,-62.707646367062,-8.1683060063698));
#38254=CARTESIAN_POINT('Ctrl Pts',(-63.7674100795425,-62.1134845746734,
-8.20727821900023));
#38255=CARTESIAN_POINT('Ctrl Pts',(-64.0056377910967,-61.459793535165,-8.24625043163066));
#38256=CARTESIAN_POINT('Ctrl Pts',(-64.243865502651,-60.8061024956567,-8.28522264426109));
#38257=CARTESIAN_POINT('Ctrl Pts',(-64.3187461882234,-60.0928822090285,
-8.32419485689152));
#38258=CARTESIAN_POINT('Ctrl Pts',(-64.221478033394,-59.4039676503758,-8.36316706952195));
#38259=CARTESIAN_POINT('Ctrl Pts',(-64.1242098785646,-58.7150530917231,
-8.40213928215238));
#38260=CARTESIAN_POINT('Ctrl Pts',(-63.8547928833333,-58.0504442610459,
-8.4411114947828));
#38261=CARTESIAN_POINT('Ctrl Pts',(-63.4448955281047,-57.4882623152356,
-8.48008370741324));
#38262=CARTESIAN_POINT('Ctrl Pts',(-63.034998172876,-56.9260803694254,-8.51905592004366));
#38263=CARTESIAN_POINT('Ctrl Pts',(-62.4846204576499,-56.4663253084821,
-8.5580281326741));
#38264=CARTESIAN_POINT('Ctrl Pts',(-61.8584562295012,-56.1630387370539,
-8.59700034530453));
#38265=CARTESIAN_POINT('Ctrl Pts',(-61.2322920013524,-55.8597521656257,
-8.63597255793496));
#38266=CARTESIAN_POINT('Ctrl Pts',(-60.530341260281,-55.7129340837125,-8.67494477056539));
#38267=CARTESIAN_POINT('Ctrl Pts',(-59.8351144426062,-55.7398422268092,
-8.71391698319581));
#38268=CARTESIAN_POINT('Ctrl Pts',(-59.1398876249314,-55.7667503699059,
-8.75288919582624));
#38269=CARTESIAN_POINT('Ctrl Pts',(-58.4513847306531,-55.9673847380125,
-8.79186140845667));
#38270=CARTESIAN_POINT('Ctrl Pts',(-57.8505354363813,-56.3181617124484,
-8.8308336210871));
#38271=CARTESIAN_POINT('Ctrl Pts',(-57.2496861421095,-56.6689386868844,
-8.86980583371754));
#38272=CARTESIAN_POINT('Ctrl Pts',(-56.7364904478442,-57.1698582676496,
-8.90877804634796));
#38273=CARTESIAN_POINT('Ctrl Pts',(-56.3712717242657,-57.7620404667158,
-8.94775025897839));
#38274=CARTESIAN_POINT('Ctrl Pts',(-56.0060530006872,-58.354222665782,-8.98672247160882));
#38275=CARTESIAN_POINT('Ctrl Pts',(-55.7888112477955,-59.037667483149,-9.02569468423925));
#38276=CARTESIAN_POINT('Ctrl Pts',(-55.7450819051124,-59.7320390445562,
-9.06466689686969));
#38277=CARTESIAN_POINT('Ctrl Pts',(-55.7394660561013,-59.8212122542869,
-9.06967182144281));
#38278=CARTESIAN_POINT('Ctrl Pts',(-55.7367118503295,-59.9105656727024,
-9.07467674601594));
#38279=CARTESIAN_POINT('Ctrl Pts',(-55.7367869775695,-59.9999237120217,
-9.07968167058906));
#38280=CARTESIAN_POINT('Ctrl Pts',(-58.677115034431,-64.9244061944433,-10.));
#38281=CARTESIAN_POINT('Ctrl Pts',(-57.8732233401272,-64.7084499564018,
-9.96102778736957));
#38282=CARTESIAN_POINT('Ctrl Pts',(-56.3739727010425,-63.8754866332611,
-9.88308336210871));
#38283=CARTESIAN_POINT('Ctrl Pts',(-54.9770228002682,-61.7140882090784,
-9.76616672421742));
#38284=CARTESIAN_POINT('Ctrl Pts',(-54.7611834296551,-59.14993732374,-9.64925008632613));
#38285=CARTESIAN_POINT('Ctrl Pts',(-55.7768178205809,-56.785492732961,-9.53233344843484));
#38286=CARTESIAN_POINT('Ctrl Pts',(-57.7853302129478,-55.1767966332062,
-9.41541681054355));
#38287=CARTESIAN_POINT('Ctrl Pts',(-60.3144620635955,-54.7019555263241,
-9.29850017265227));
#38288=CARTESIAN_POINT('Ctrl Pts',(-62.7696789900454,-55.4726379404574,
-9.18158353476098));
#38289=CARTESIAN_POINT('Ctrl Pts',(-64.5737696881318,-57.3076474190762,
-9.06466689686968));
#38290=CARTESIAN_POINT('Ctrl Pts',(-65.3026202647668,-59.7756017648733,
-8.9477502589784));
#38291=CARTESIAN_POINT('Ctrl Pts',(-64.7848823729,-62.2963084445819,-8.8308336210871));
#38292=CARTESIAN_POINT('Ctrl Pts',(-63.1422721548051,-64.2771789992941,
-8.71391698319582));
#38293=CARTESIAN_POINT('Ctrl Pts',(-60.7609482822248,-65.252531849864,-8.59700034530452));
#38294=CARTESIAN_POINT('Ctrl Pts',(-58.2007340409931,-64.9930727838061,
-8.48008370741324));
#38295=CARTESIAN_POINT('Ctrl Pts',(-56.0635071815643,-63.5597974366436,
-8.36316706952195));
#38296=CARTESIAN_POINT('Ctrl Pts',(-54.8517063751933,-61.2896533639402,
-8.24625043163066));
#38297=CARTESIAN_POINT('Ctrl Pts',(-54.8502120579674,-58.7163255954642,
-8.12933379373937));
#38298=CARTESIAN_POINT('Ctrl Pts',(-56.0593765808925,-56.444776458995,-8.01241715584808));
#38299=CARTESIAN_POINT('Ctrl Pts',(-58.1949365065413,-55.009018880156,-7.89550051795679));
#38300=CARTESIAN_POINT('Ctrl Pts',(-60.754850176949,-54.7465903023206,-7.7785838800655));
#38301=CARTESIAN_POINT('Ctrl Pts',(-63.1372997996482,-55.7191702494578,
-7.6616672421742));
#38302=CARTESIAN_POINT('Ctrl Pts',(-64.7822203636214,-57.6981473048777,
-7.54475060428292));
#38303=CARTESIAN_POINT('Ctrl Pts',(-65.3028606509933,-60.2182181776382,
-7.42783396639163));
#38304=CARTESIAN_POINT('Ctrl Pts',(-64.5769288134183,-62.6870882382886,
-7.31091732850035));
#38305=CARTESIAN_POINT('Ctrl Pts',(-62.7748568790513,-64.5240380041187,
-7.19400069060905));
#38306=CARTESIAN_POINT('Ctrl Pts',(-60.3207808627358,-65.2979018325692,
-7.07708405271776));
#38307=CARTESIAN_POINT('Ctrl Pts',(-57.7905711249098,-64.8252826799559,
-6.96016741482647));
#38308=CARTESIAN_POINT('Ctrl Pts',(-55.7813289378715,-63.2204602274652,
-6.84325077693518));
#38309=CARTESIAN_POINT('Ctrl Pts',(-54.760481380096,-60.8538559480399,-6.72633413904389));
#38310=CARTESIAN_POINT('Ctrl Pts',(-54.9785971562446,-58.2965966407732,
-6.60941750115261));
#38311=CARTESIAN_POINT('Ctrl Pts',(-56.8226683737146,-55.391675711492,-6.45352865063088));
#38312=CARTESIAN_POINT('Ctrl Pts',(-61.3338598105922,-54.1559235864261,
-6.25866758747874));
#38313=CARTESIAN_POINT('Ctrl Pts',(-65.6028015656481,-57.869031736986,-6.02483431169615));
#38314=CARTESIAN_POINT('Ctrl Pts',(-65.0042219447148,-62.5079576829526,
-5.82997324854401));
#38315=CARTESIAN_POINT('Ctrl Pts',(-62.382923622443,-64.736849642231,-5.67408439802229));
#38316=CARTESIAN_POINT('Ctrl Pts',(-59.8805760101181,-65.3072934023813,
-5.557167760131));
#38317=CARTESIAN_POINT('Ctrl Pts',(-57.3953244921747,-64.6243069865738,
-5.44025112223971));
#38318=CARTESIAN_POINT('Ctrl Pts',(-55.5275122251888,-62.8568832667251,
-5.32333448434841));
#38319=CARTESIAN_POINT('Ctrl Pts',(-54.7087704381597,-60.4165980237737,
-5.20641784645713));
#38320=CARTESIAN_POINT('Ctrl Pts',(-55.135033382092,-57.8789506444978,-5.08950120856584));
#38321=CARTESIAN_POINT('Ctrl Pts',(-56.7044889980166,-55.8396721524265,
-4.97258457067455));
#38322=CARTESIAN_POINT('Ctrl Pts',(-59.0489177395961,-54.7785641063853,
-4.85566793278326));
#38323=CARTESIAN_POINT('Ctrl Pts',(-61.6168265507944,-54.9449006597622,
-4.73875129489197));
#38324=CARTESIAN_POINT('Ctrl Pts',(-63.8046877645853,-56.2996615825733,
-4.62183465700068));
#38325=CARTESIAN_POINT('Ctrl Pts',(-65.0980856519831,-58.5243188288231,
-4.50491801910939));
#38326=CARTESIAN_POINT('Ctrl Pts',(-65.1929908727149,-61.0958980618402,
-4.3880013812181));
#38327=CARTESIAN_POINT('Ctrl Pts',(-64.0670764169607,-63.4098411642031,
-4.27108474332681));
#38328=CARTESIAN_POINT('Ctrl Pts',(-61.9850396640587,-64.922169576908,-4.15416810543552));
#38329=CARTESIAN_POINT('Ctrl Pts',(-59.4363409557176,-65.2773498680853,
-4.03725146754424));
#38330=CARTESIAN_POINT('Ctrl Pts',(-57.0201528179928,-64.3918838717894,
-3.92033482965294));
#38331=CARTESIAN_POINT('Ctrl Pts',(-55.3044933735877,-62.4739345405712,
-3.80341819176166));
#38332=CARTESIAN_POINT('Ctrl Pts',(-54.6926959899439,-59.9743905229704,
-3.68650155387037));
#38333=CARTESIAN_POINT('Ctrl Pts',(-55.3285862434613,-57.4808672502626,
-3.56958491597908));
#38334=CARTESIAN_POINT('Ctrl Pts',(-57.0626757333642,-55.5795636292569,
-3.45266827808779));
#38335=CARTESIAN_POINT('Ctrl Pts',(-59.4872942572559,-54.7174568855574,
-3.3357516401965));
#38336=CARTESIAN_POINT('Ctrl Pts',(-62.032451512693,-55.097214824058,-3.21883500230521));
#38337=CARTESIAN_POINT('Ctrl Pts',(-64.0997862511836,-56.6295689181909,
-3.10191836441392));
#38338=CARTESIAN_POINT('Ctrl Pts',(-65.2033406964322,-58.954260889118,-2.98500172652263));
#38339=CARTESIAN_POINT('Ctrl Pts',(-65.0835748708919,-61.5248187245729,
-2.86808508863134));
#38340=CARTESIAN_POINT('Ctrl Pts',(-63.7688779976231,-63.7368378312184,
-2.75116845074005));
#38341=CARTESIAN_POINT('Ctrl Pts',(-61.5678299178988,-65.0704417919735,
-2.63425181284876));
#38342=CARTESIAN_POINT('Ctrl Pts',(-59.8553056997907,-65.1644693350243,
-2.5563073875879));
#38343=CARTESIAN_POINT('Ctrl Pts',(-59.0378648750817,-65.0074042178956,
-2.51733517495747));
#38344=CARTESIAN_POINT('Ctrl Pts',(-58.7494123365958,-64.655281295538,-10.1608882750142));
#38345=CARTESIAN_POINT('Ctrl Pts',(-57.9894543192508,-64.4511273334331,
-10.1219160623837));
#38346=CARTESIAN_POINT('Ctrl Pts',(-56.5721395848712,-63.6636864877811,
-10.0439716371229));
#38347=CARTESIAN_POINT('Ctrl Pts',(-55.2515347267228,-61.6204111650312,
-9.9270549992316));
#38348=CARTESIAN_POINT('Ctrl Pts',(-55.0474912450966,-59.1963943020595,
-9.81013836134031));
#38349=CARTESIAN_POINT('Ctrl Pts',(-56.0076199583853,-56.9611695372523,
-9.69322172344901));
#38350=CARTESIAN_POINT('Ctrl Pts',(-57.9063646603542,-55.4403906722099,
-9.57630508555773));
#38351=CARTESIAN_POINT('Ctrl Pts',(-60.2972763222628,-54.9915002200545,
-9.45938844766644));
#38352=CARTESIAN_POINT('Ctrl Pts',(-62.6183126021472,-55.7200638855301,
-9.34247180977516));
#38353=CARTESIAN_POINT('Ctrl Pts',(-64.3238075086667,-57.4547878229235,
-9.22555517188386));
#38354=CARTESIAN_POINT('Ctrl Pts',(-65.0128254983848,-59.7878654064087,
-9.10863853399257));
#38355=CARTESIAN_POINT('Ctrl Pts',(-64.5233826236848,-62.1708123434071,
-8.99172189610128));
#38356=CARTESIAN_POINT('Ctrl Pts',(-62.9705430888825,-64.043425868392,-8.87480525820999));
#38357=CARTESIAN_POINT('Ctrl Pts',(-60.7193615159347,-64.9654744774063,
-8.7578886203187));
#38358=CARTESIAN_POINT('Ctrl Pts',(-58.2990661545925,-64.7201951707276,
-8.64097198242741));
#38359=CARTESIAN_POINT('Ctrl Pts',(-56.2786413906388,-63.3652500968363,
-8.52405534453612));
#38360=CARTESIAN_POINT('Ctrl Pts',(-55.1330669995209,-61.2191722099718,
-8.40713870664483));
#38361=CARTESIAN_POINT('Ctrl Pts',(-55.1316543485825,-58.7864799918943,
-8.29022206875355));
#38362=CARTESIAN_POINT('Ctrl Pts',(-56.2747365324107,-56.6390738297396,
-8.17330543086225));
#38363=CARTESIAN_POINT('Ctrl Pts',(-58.2935854625805,-55.2817821812078,
-8.05638879297097));
#38364=CARTESIAN_POINT('Ctrl Pts',(-60.7135966796666,-55.033695650249,-7.93947215507967));
#38365=CARTESIAN_POINT('Ctrl Pts',(-62.9658424790948,-55.9531228984382,
-7.82255551718839));
#38366=CARTESIAN_POINT('Ctrl Pts',(-64.520866096511,-57.8239464062127,-7.7056388792971));
#38367=CARTESIAN_POINT('Ctrl Pts',(-65.0130527472063,-60.2062922839005,
-7.5887222414058));
#38368=CARTESIAN_POINT('Ctrl Pts',(-64.3267939838427,-62.5402355372878,
-7.47180560351452));
#38369=CARTESIAN_POINT('Ctrl Pts',(-62.6232075131046,-64.2767937227928,
-7.35488896562323));
#38370=CARTESIAN_POINT('Ctrl Pts',(-60.3032497912023,-65.008364934352,-7.23797232773194));
#38371=CARTESIAN_POINT('Ctrl Pts',(-57.9113191499851,-64.5615750039121,
-7.12105568984065));
#38372=CARTESIAN_POINT('Ctrl Pts',(-56.0118845375275,-63.044458086512,-7.00413905194936));
#38373=CARTESIAN_POINT('Ctrl Pts',(-55.0468275634157,-60.8071916627186,
-6.88722241405807));
#38374=CARTESIAN_POINT('Ctrl Pts',(-55.2530230421947,-58.3896897445395,
-6.77030577616678));
#38375=CARTESIAN_POINT('Ctrl Pts',(-56.9963134831854,-55.6435263426741,
-6.61441692564506));
#38376=CARTESIAN_POINT('Ctrl Pts',(-61.2609627195511,-54.475309602099,-6.41955586249291));
#38377=CARTESIAN_POINT('Ctrl Pts',(-65.2966015193069,-57.9854917924139,
-6.18572258671033));
#38378=CARTESIAN_POINT('Ctrl Pts',(-64.730735016181,-62.3708946887088,-5.99086152355818));
#38379=CARTESIAN_POINT('Ctrl Pts',(-62.2526938944988,-64.47797494125,-5.83497267303646));
#38380=CARTESIAN_POINT('Ctrl Pts',(-59.8871026791081,-65.0172432432395,
-5.71805603514517));
#38381=CARTESIAN_POINT('Ctrl Pts',(-57.5376732353624,-64.371582881143,-5.60113939725389));
#38382=CARTESIAN_POINT('Ctrl Pts',(-55.7719392226224,-62.7007510570773,
-5.48422275936259));
#38383=CARTESIAN_POINT('Ctrl Pts',(-54.9979426885158,-60.3938304256908,
-5.36730612147131));
#38384=CARTESIAN_POINT('Ctrl Pts',(-55.4009098345056,-57.9948686193426,
-5.25038948358002));
#38385=CARTESIAN_POINT('Ctrl Pts',(-56.8845927567705,-56.0670392231313,
-5.13347284568873));
#38386=CARTESIAN_POINT('Ctrl Pts',(-59.1008955633327,-55.0639220463122,
-5.01655620779744));
#38387=CARTESIAN_POINT('Ctrl Pts',(-61.5284649768607,-55.2211681009885,
-4.89963956990615));
#38388=CARTESIAN_POINT('Ctrl Pts',(-63.5967568649845,-56.5018896610834,
-4.78272293201485));
#38389=CARTESIAN_POINT('Ctrl Pts',(-64.8194689555683,-58.6049666329092,
-4.66580629412357));
#38390=CARTESIAN_POINT('Ctrl Pts',(-64.909187488418,-61.0360058751566,-4.54888965623228));
#38391=CARTESIAN_POINT('Ctrl Pts',(-63.8448056524592,-63.2234891204512,
-4.43197301834099));
#38392=CARTESIAN_POINT('Ctrl Pts',(-61.8765547873409,-64.6531669119217,
-4.3150563804497));
#38393=CARTESIAN_POINT('Ctrl Pts',(-59.4671456207512,-64.9889361601871,
-4.19813974255841));
#38394=CARTESIAN_POINT('Ctrl Pts',(-57.1830051579391,-64.1518619775084,
-4.08122310466712));
#38395=CARTESIAN_POINT('Ctrl Pts',(-55.5611086275382,-62.3387309532065,
-3.96430646677583));
#38396=CARTESIAN_POINT('Ctrl Pts',(-54.9827467288082,-59.9757901126153,
-3.84738982888454));
#38397=CARTESIAN_POINT('Ctrl Pts',(-55.5838847922268,-57.61854097575,-3.73047319099325));
#38398=CARTESIAN_POINT('Ctrl Pts',(-57.2232041433078,-55.8211459529767,
-3.61355655310196));
#38399=CARTESIAN_POINT('Ctrl Pts',(-59.5153142612392,-55.0061544108024,
-3.49663991521067));
#38400=CARTESIAN_POINT('Ctrl Pts',(-61.9213755197133,-55.365158107518,-3.37972327731939));
#38401=CARTESIAN_POINT('Ctrl Pts',(-63.8757278537207,-56.8137671521186,
-3.26280663942809));
#38402=CARTESIAN_POINT('Ctrl Pts',(-64.9189716814477,-59.0114118269946,
-3.14589000153681));
#38403=CARTESIAN_POINT('Ctrl Pts',(-64.8057512066397,-61.441485492322,-3.02897336364551));
#38404=CARTESIAN_POINT('Ctrl Pts',(-63.5629041461481,-63.5326150145289,
-2.91205672575423));
#38405=CARTESIAN_POINT('Ctrl Pts',(-61.4821460706501,-64.7933358667535,
-2.79514008786293));
#38406=CARTESIAN_POINT('Ctrl Pts',(-59.8632134225452,-64.8822246880948,
-2.71719566260207));
#38407=CARTESIAN_POINT('Ctrl Pts',(-59.0904467515563,-64.7337433741902,
-2.67822344997165));
#38408=CARTESIAN_POINT('Ctrl Pts',(-58.8217096387607,-64.3861563966327,
-10.3217765500284));
#38409=CARTESIAN_POINT('Ctrl Pts',(-58.1056852983744,-64.1938047104644,
-10.2828043373979));
#38410=CARTESIAN_POINT('Ctrl Pts',(-56.7703064687,-63.4518863423012,-10.2048599121371));
#38411=CARTESIAN_POINT('Ctrl Pts',(-55.5260466531774,-61.5267341209841,
-10.0879432742458));
#38412=CARTESIAN_POINT('Ctrl Pts',(-55.3337990605381,-59.2428512803789,
-9.97102663635449));
#38413=CARTESIAN_POINT('Ctrl Pts',(-56.2384220961897,-57.1368463415437,
-9.85410999846319));
#38414=CARTESIAN_POINT('Ctrl Pts',(-58.0273991077606,-55.7039847112136,
-9.73719336057191));
#38415=CARTESIAN_POINT('Ctrl Pts',(-60.2800905809301,-55.2810449137848,
-9.62027672268061));
#38416=CARTESIAN_POINT('Ctrl Pts',(-62.4669462142492,-55.9674898306028,
-9.50336008478933));
#38417=CARTESIAN_POINT('Ctrl Pts',(-64.0738453292015,-57.6019282267708,
-9.38644344689803));
#38418=CARTESIAN_POINT('Ctrl Pts',(-64.7230307320029,-59.800129047944,-9.26952680900675));
#38419=CARTESIAN_POINT('Ctrl Pts',(-64.2618828744696,-62.0453162422323,
-9.15261017111546));
#38420=CARTESIAN_POINT('Ctrl Pts',(-62.79881402296,-63.8096727374899,-9.03569353322417));
#38421=CARTESIAN_POINT('Ctrl Pts',(-60.6777747496446,-64.6784171049485,
-8.91877689533288));
#38422=CARTESIAN_POINT('Ctrl Pts',(-58.3973982681919,-64.4473175576491,
-8.80186025744159));
#38423=CARTESIAN_POINT('Ctrl Pts',(-56.4937755997133,-63.1707027570288,
-8.6849436195503));
#38424=CARTESIAN_POINT('Ctrl Pts',(-55.4144276238484,-61.1486910560035,
-8.56802698165901));
#38425=CARTESIAN_POINT('Ctrl Pts',(-55.4130966391976,-58.8566343883245,
-8.45111034376773));
#38426=CARTESIAN_POINT('Ctrl Pts',(-56.4900964839289,-56.8333712004842,
-8.33419370587643));
#38427=CARTESIAN_POINT('Ctrl Pts',(-58.3922344186197,-55.5545454822596,
-8.21727706798514));
#38428=CARTESIAN_POINT('Ctrl Pts',(-60.6723431823842,-55.3208009981773,
-8.10036043009385));
#38429=CARTESIAN_POINT('Ctrl Pts',(-62.7943851585413,-56.1870755474186,
-7.98344379220256));
#38430=CARTESIAN_POINT('Ctrl Pts',(-64.2595118294006,-57.9497455075478,
-7.86652715431127));
#38431=CARTESIAN_POINT('Ctrl Pts',(-64.7232448434193,-60.1943663901628,
-7.74961051641998));
#38432=CARTESIAN_POINT('Ctrl Pts',(-64.0766591542672,-62.393382836287,-7.6326938785287));
#38433=CARTESIAN_POINT('Ctrl Pts',(-62.4715581471579,-64.0295494414668,
-7.51577724063741));
#38434=CARTESIAN_POINT('Ctrl Pts',(-60.2857187196689,-64.7188280361349,
-7.39886060274612));
#38435=CARTESIAN_POINT('Ctrl Pts',(-58.0320671750603,-64.2978673278682,
-7.28194396485483));
#38436=CARTESIAN_POINT('Ctrl Pts',(-56.2424401371836,-62.8684559455588,
-7.16502732696354));
#38437=CARTESIAN_POINT('Ctrl Pts',(-55.3331737467353,-60.7605273773972,
-7.04811068907224));
#38438=CARTESIAN_POINT('Ctrl Pts',(-55.5274489281449,-58.4827828483059,
-6.93119405118096));
#38439=CARTESIAN_POINT('Ctrl Pts',(-57.1699585926562,-55.8953769738562,
-6.77530520065923));
#38440=CARTESIAN_POINT('Ctrl Pts',(-61.18806562851,-54.7946956177719,-6.58044413750709));
#38441=CARTESIAN_POINT('Ctrl Pts',(-64.9904014729656,-58.1019518478416,
-6.3466108617245));
#38442=CARTESIAN_POINT('Ctrl Pts',(-64.4572480876472,-62.233831694465,-6.15174979857236));
#38443=CARTESIAN_POINT('Ctrl Pts',(-62.1224641665546,-64.2191002402691,
-5.99586094805064));
#38444=CARTESIAN_POINT('Ctrl Pts',(-59.8936293480983,-64.7271930840978,
-5.87894431015935));
#38445=CARTESIAN_POINT('Ctrl Pts',(-57.68002197855,-64.1188587757121,-5.76202767226806));
#38446=CARTESIAN_POINT('Ctrl Pts',(-56.016366220056,-62.5446188474295,-5.64511103437677));
#38447=CARTESIAN_POINT('Ctrl Pts',(-55.287114938872,-60.3710628276078,-5.52819439648548));
#38448=CARTESIAN_POINT('Ctrl Pts',(-55.6667862869192,-58.1107865941873,
-5.41127775859419));
#38449=CARTESIAN_POINT('Ctrl Pts',(-57.0646965155244,-56.2944062938361,
-5.2943611207029));
#38450=CARTESIAN_POINT('Ctrl Pts',(-59.1528733870691,-55.3492799862391,
-5.17744448281161));
#38451=CARTESIAN_POINT('Ctrl Pts',(-61.440103402927,-55.4974355422148,-5.06052784492032));
#38452=CARTESIAN_POINT('Ctrl Pts',(-63.3888259653837,-56.7041177395935,
-4.94361120702903));
#38453=CARTESIAN_POINT('Ctrl Pts',(-64.5408522591534,-58.6856144369952,
-4.82669456913774));
#38454=CARTESIAN_POINT('Ctrl Pts',(-64.6253841041211,-60.976113688473,-4.70977793124645));
#38455=CARTESIAN_POINT('Ctrl Pts',(-63.6225348879577,-63.0371370766992,
-4.59286129335517));
#38456=CARTESIAN_POINT('Ctrl Pts',(-61.768069910623,-64.3841642469354,-4.47594465546388));
#38457=CARTESIAN_POINT('Ctrl Pts',(-59.4979502857849,-64.7005224522889,
-4.35902801757259));
#38458=CARTESIAN_POINT('Ctrl Pts',(-57.3458574978853,-63.9118400832274,
-4.2421113796813));
#38459=CARTESIAN_POINT('Ctrl Pts',(-55.8177238814887,-62.2035273658419,
-4.12519474179001));
#38460=CARTESIAN_POINT('Ctrl Pts',(-55.2727974676725,-59.97718970226,-4.00827810389872));
#38461=CARTESIAN_POINT('Ctrl Pts',(-55.8391833409923,-57.7562147012374,
-3.89136146600743));
#38462=CARTESIAN_POINT('Ctrl Pts',(-57.3837325532514,-56.0627282766964,
-3.77444482811614));
#38463=CARTESIAN_POINT('Ctrl Pts',(-59.5433342652227,-55.2948519360475,
-3.65752819022485));
#38464=CARTESIAN_POINT('Ctrl Pts',(-61.8102995267335,-55.633101390978,-3.54061155233356));
#38465=CARTESIAN_POINT('Ctrl Pts',(-63.6516694562579,-56.9979653860463,
-3.42369491444227));
#38466=CARTESIAN_POINT('Ctrl Pts',(-64.6346026664633,-59.0685627648711,
-3.30677827655098));
#38467=CARTESIAN_POINT('Ctrl Pts',(-64.5279275423875,-61.358152260071,-3.18986163865969));
#38468=CARTESIAN_POINT('Ctrl Pts',(-63.3569302946731,-63.3283921978395,
-3.0729450007684));
#38469=CARTESIAN_POINT('Ctrl Pts',(-61.3964622234014,-64.5162299415336,
-2.95602836287711));
#38470=CARTESIAN_POINT('Ctrl Pts',(-59.8711211452996,-64.5999800411654,
-2.87808393761625));
#38471=CARTESIAN_POINT('Ctrl Pts',(-59.1430286280309,-64.4600825304849,
-2.83911172498582));
#38472=CARTESIAN_POINT('Ctrl Pts',(-58.8940069409255,-64.1170314977274,
-10.4826648250425));
#38473=CARTESIAN_POINT('Ctrl Pts',(-58.221916277498,-63.9364820874957,-10.4436926124121));
#38474=CARTESIAN_POINT('Ctrl Pts',(-56.9684733525287,-63.2400861968213,
-10.3657481871512));
#38475=CARTESIAN_POINT('Ctrl Pts',(-55.800558579632,-61.4330570769369,-10.2488315492599));
#38476=CARTESIAN_POINT('Ctrl Pts',(-55.6201068759796,-59.2893082586984,
-10.1319149113687));
#38477=CARTESIAN_POINT('Ctrl Pts',(-56.4692242339942,-57.312523145835,-10.0149982734774));
#38478=CARTESIAN_POINT('Ctrl Pts',(-58.1484335551669,-55.9675787502173,
-9.89808163558608));
#38479=CARTESIAN_POINT('Ctrl Pts',(-60.2629048395975,-55.5705896075151,
-9.78116499769479));
#38480=CARTESIAN_POINT('Ctrl Pts',(-62.3155798263509,-56.2149157756756,
-9.6642483598035));
#38481=CARTESIAN_POINT('Ctrl Pts',(-63.8238831497364,-57.7490686306181,
-9.54733172191221));
#38482=CARTESIAN_POINT('Ctrl Pts',(-64.4332359656209,-59.8123926894793,
-9.43041508402093));
#38483=CARTESIAN_POINT('Ctrl Pts',(-64.0003831252545,-61.9198201410576,
-9.31349844612963));
#38484=CARTESIAN_POINT('Ctrl Pts',(-62.6270849570375,-63.5759196065878,
-9.19658180823835));
#38485=CARTESIAN_POINT('Ctrl Pts',(-60.6361879833545,-64.3913597324907,
-9.07966517034706));
#38486=CARTESIAN_POINT('Ctrl Pts',(-58.4957303817913,-64.1744399445706,
-8.96274853245577));
#38487=CARTESIAN_POINT('Ctrl Pts',(-56.7089098087877,-62.9761554172214,
-8.84583189456448));
#38488=CARTESIAN_POINT('Ctrl Pts',(-55.6957882481759,-61.0782099020351,
-8.72891525667319));
#38489=CARTESIAN_POINT('Ctrl Pts',(-55.6945389298127,-58.9267887847546,
-8.6119986187819));
#38490=CARTESIAN_POINT('Ctrl Pts',(-56.7054564354471,-57.0276685712288,
-8.49508198089061));
#38491=CARTESIAN_POINT('Ctrl Pts',(-58.4908833746589,-55.8273087833114,
-8.37816534299932));
#38492=CARTESIAN_POINT('Ctrl Pts',(-60.6310896851017,-55.6079063461057,
-8.26124870510803));
#38493=CARTESIAN_POINT('Ctrl Pts',(-62.6229278379879,-56.421028196399,-8.14433206721674));
#38494=CARTESIAN_POINT('Ctrl Pts',(-63.9981575622902,-58.0755446088829,
-8.02741542932545));
#38495=CARTESIAN_POINT('Ctrl Pts',(-64.4334369396322,-60.1824404964251,
-7.91049879143416));
#38496=CARTESIAN_POINT('Ctrl Pts',(-63.8265243246915,-62.2465301352862,
-7.79358215354287));
#38497=CARTESIAN_POINT('Ctrl Pts',(-62.3199087812112,-63.7823051601408,
-7.67666551565158));
#38498=CARTESIAN_POINT('Ctrl Pts',(-60.2681876481355,-64.4292911379178,
-7.55974887776029));
#38499=CARTESIAN_POINT('Ctrl Pts',(-58.1528152001354,-64.0341596518243,
-7.442832239869));
#38500=CARTESIAN_POINT('Ctrl Pts',(-56.4729957368398,-62.6924538046056,
-7.32591560197771));
#38501=CARTESIAN_POINT('Ctrl Pts',(-55.6195199300548,-60.7138630920758,
-7.20899896408642));
#38502=CARTESIAN_POINT('Ctrl Pts',(-55.8018748140951,-58.5758759520722,
-7.09208232619513));
#38503=CARTESIAN_POINT('Ctrl Pts',(-57.3436037021269,-56.1472276050383,
-6.93619347567341));
#38504=CARTESIAN_POINT('Ctrl Pts',(-61.115168537469,-55.1140816334448,-6.74133241252127));
#38505=CARTESIAN_POINT('Ctrl Pts',(-64.6842014266244,-58.2184119032695,
-6.50749913673868));
#38506=CARTESIAN_POINT('Ctrl Pts',(-64.1837611591134,-62.0967687002211,
-6.31263807358653));
#38507=CARTESIAN_POINT('Ctrl Pts',(-61.9922344386104,-63.9602255392882,
-6.15674922306482));
#38508=CARTESIAN_POINT('Ctrl Pts',(-59.9001560170883,-64.4371429249561,
-6.03983258517352));
#38509=CARTESIAN_POINT('Ctrl Pts',(-57.8223707217377,-63.8661346702813,
-5.92291594728224));
#38510=CARTESIAN_POINT('Ctrl Pts',(-56.2607932174897,-62.3884866377817,
-5.80599930939095));
#38511=CARTESIAN_POINT('Ctrl Pts',(-55.5762871892282,-60.3482952295248,
-5.68908267149966));
#38512=CARTESIAN_POINT('Ctrl Pts',(-55.9326627393328,-58.226704569032,-5.57216603360837));
#38513=CARTESIAN_POINT('Ctrl Pts',(-57.2448002742782,-56.5217733645409,
-5.45524939571708));
#38514=CARTESIAN_POINT('Ctrl Pts',(-59.2048512108057,-55.634637926166,-5.33833275782579));
#38515=CARTESIAN_POINT('Ctrl Pts',(-61.3517418289932,-55.7737029834411,
-5.2214161199345));
#38516=CARTESIAN_POINT('Ctrl Pts',(-63.1808950657829,-56.9063458181036,
-5.10449948204321));
#38517=CARTESIAN_POINT('Ctrl Pts',(-64.2622355627386,-58.7662622410812,
-4.98758284415192));
#38518=CARTESIAN_POINT('Ctrl Pts',(-64.3415807198242,-60.9162215017895,
-4.87066620626063));
#38519=CARTESIAN_POINT('Ctrl Pts',(-63.4002641234563,-62.8507850329473,
-4.75374956836934));
#38520=CARTESIAN_POINT('Ctrl Pts',(-61.6595850339052,-64.1151615819491,
-4.63683293047805));
#38521=CARTESIAN_POINT('Ctrl Pts',(-59.5287549508186,-64.4121087443906,
-4.51991629258676));
#38522=CARTESIAN_POINT('Ctrl Pts',(-57.5087098378316,-63.6718181889464,
-4.40299965469547));
#38523=CARTESIAN_POINT('Ctrl Pts',(-56.0743391354391,-62.0683237784772,
-4.28608301680418));
#38524=CARTESIAN_POINT('Ctrl Pts',(-55.5628482065368,-59.9785892919048,
-4.1691663789129));
#38525=CARTESIAN_POINT('Ctrl Pts',(-56.0944818897578,-57.8938884267248,
-4.0522497410216));
#38526=CARTESIAN_POINT('Ctrl Pts',(-57.5442609631951,-56.3043106004162,
-3.93533310313032));
#38527=CARTESIAN_POINT('Ctrl Pts',(-59.5713542692061,-55.5835494612926,
-3.81841646523903));
#38528=CARTESIAN_POINT('Ctrl Pts',(-61.6992235337538,-55.901044674438,-3.70149982734774));
#38529=CARTESIAN_POINT('Ctrl Pts',(-63.427611058795,-57.1821636199741,-3.58458318945645));
#38530=CARTESIAN_POINT('Ctrl Pts',(-64.3502336514788,-59.1257137027476,
-3.46766655156516));
#38531=CARTESIAN_POINT('Ctrl Pts',(-64.2501038781353,-61.27481902782,-3.35074991367387));
#38532=CARTESIAN_POINT('Ctrl Pts',(-63.1509564431981,-63.12416938115,-3.23383327578258));
#38533=CARTESIAN_POINT('Ctrl Pts',(-61.3107783761527,-64.2391240163136,
-3.11691663789129));
#38534=CARTESIAN_POINT('Ctrl Pts',(-59.8790288680541,-64.3177353942359,
-3.03897221263043));
#38535=CARTESIAN_POINT('Ctrl Pts',(-59.1956105045054,-64.1864216867795,
-3.));
#38536=CARTESIAN_POINT('Ctrl Pts',(-55.7373303432786,-59.9999992452069,
-8.67031832941095));
#38537=CARTESIAN_POINT('Ctrl Pts',(-55.7373282291776,-59.6527912211962,
-8.65087842586793));
#38538=CARTESIAN_POINT('Ctrl Pts',(-55.7792938837216,-59.3055837057915,
-8.63143852232492));
#38539=CARTESIAN_POINT('Ctrl Pts',(-55.863233400479,-58.9688389353804,-8.6119986187819));
#38540=CARTESIAN_POINT('Ctrl Pts',(-56.0315114316909,-58.2937487135794,
-8.57302640615147));
#38541=CARTESIAN_POINT('Ctrl Pts',(-56.368483933569,-57.6607086424041,-8.53405419352104));
#38542=CARTESIAN_POINT('Ctrl Pts',(-56.8345413410433,-57.1441286421636,
-8.49508198089061));
#38543=CARTESIAN_POINT('Ctrl Pts',(-57.3005987485177,-56.627548641923,-8.45610976826018));
#38544=CARTESIAN_POINT('Ctrl Pts',(-57.8957410615883,-56.2274287126172,
-8.41713755562975));
#38545=CARTESIAN_POINT('Ctrl Pts',(-58.5500132698641,-55.9908016750967,
-8.37816534299932));
#38546=CARTESIAN_POINT('Ctrl Pts',(-59.2042854781398,-55.7541746375761,
-8.33919313036889));
#38547=CARTESIAN_POINT('Ctrl Pts',(-59.9176875816208,-55.6810404918409,
-8.30022091773846));
#38548=CARTESIAN_POINT('Ctrl Pts',(-60.6063616588423,-55.7799937273555,
-8.26124870510803));
#38549=CARTESIAN_POINT('Ctrl Pts',(-61.2950357360638,-55.8789469628701,
-8.2222764924776));
#38550=CARTESIAN_POINT('Ctrl Pts',(-61.9589817870259,-56.1499875796345,
-8.18330427984717));
#38551=CARTESIAN_POINT('Ctrl Pts',(-62.5201597665573,-56.5612606234307,
-8.14433206721674));
#38552=CARTESIAN_POINT('Ctrl Pts',(-63.0813377460887,-56.9725336672269,
-8.10535985458631));
#38553=CARTESIAN_POINT('Ctrl Pts',(-63.5397476541895,-57.5240391380549,
-8.06638764195588));
#38554=CARTESIAN_POINT('Ctrl Pts',(-63.8414991711302,-58.1509411880593,
-8.02741542932545));
#38555=CARTESIAN_POINT('Ctrl Pts',(-64.1432506880709,-58.7778432380636,
-7.98844321669502));
#38556=CARTESIAN_POINT('Ctrl Pts',(-64.2883438138515,-59.4801418672444,
-7.94947100406459));
#38557=CARTESIAN_POINT('Ctrl Pts',(-64.2597382742518,-60.1753061216449,
-7.91049879143416));
#38558=CARTESIAN_POINT('Ctrl Pts',(-64.231132734652,-60.8704703760455,-7.87152657880373));
#38559=CARTESIAN_POINT('Ctrl Pts',(-64.0288285296718,-61.5585002556659,
-7.83255436617331));
#38560=CARTESIAN_POINT('Ctrl Pts',(-63.6765738366016,-62.1584776996185,
-7.79358215354288));
#38561=CARTESIAN_POINT('Ctrl Pts',(-63.3243191435314,-62.7584551435711,
-7.75460994091245));
#38562=CARTESIAN_POINT('Ctrl Pts',(-62.8221139623713,-63.2703801518559,
-7.71563772828202));
#38563=CARTESIAN_POINT('Ctrl Pts',(-62.2290578496119,-63.6341736522945,
-7.67666551565159));
#38564=CARTESIAN_POINT('Ctrl Pts',(-61.6360017368526,-63.9979671527331,
-7.63769330302116));
#38565=CARTESIAN_POINT('Ctrl Pts',(-60.952094692494,-64.2136291453254,-7.59872109039073));
#38566=CARTESIAN_POINT('Ctrl Pts',(-60.2575790956481,-64.2556048939393,
-7.5597488777603));
#38567=CARTESIAN_POINT('Ctrl Pts',(-59.5630634988021,-64.2975806425533,
-7.52077666512987));
#38568=CARTESIAN_POINT('Ctrl Pts',(-58.8579393494688,-64.1658701471888,
-7.48180445249944));
#38569=CARTESIAN_POINT('Ctrl Pts',(-58.2254073642528,-63.8763972583034,
-7.44283223986901));
#38570=CARTESIAN_POINT('Ctrl Pts',(-57.5928753790369,-63.5869243694181,
-7.40386002723858));
#38571=CARTESIAN_POINT('Ctrl Pts',(-57.0329355579383,-63.1396890870119,
-7.36488781460815));
#38572=CARTESIAN_POINT('Ctrl Pts',(-56.6107196795916,-62.5863063270538,
-7.32591560197772));
#38573=CARTESIAN_POINT('Ctrl Pts',(-56.1885038012448,-62.0329235670957,
-7.28694338934729));
#38574=CARTESIAN_POINT('Ctrl Pts',(-55.9040118656498,-61.3733933295857,
-7.24797117671686));
#38575=CARTESIAN_POINT('Ctrl Pts',(-55.7921583785257,-60.6872970208302,
-7.20899896408643));
#38576=CARTESIAN_POINT('Ctrl Pts',(-55.7551528338003,-60.4603093041987,
-7.1961054191946));
#38577=CARTESIAN_POINT('Ctrl Pts',(-55.7370433843899,-60.2304138053273,
-7.18321187430277));
#38578=CARTESIAN_POINT('Ctrl Pts',(-55.7374565106948,-60.0004827185225,
-7.17031832941094));
#38579=CARTESIAN_POINT('Ctrl Pts',(-58.677115034431,-64.9244061944433,-10.));
#38580=CARTESIAN_POINT('Ctrl Pts',(-58.5386375956257,-64.8748976436074,
-10.));
#38581=CARTESIAN_POINT('Ctrl Pts',(-58.4026668278543,-64.8193821760874,
-10.));
#38582=CARTESIAN_POINT('Ctrl Pts',(-58.2695271742903,-64.7581349586174,
-10.));
#38583=CARTESIAN_POINT('Ctrl Pts',(-58.1353363850557,-64.6964041952369,
-10.));
#38584=CARTESIAN_POINT('Ctrl Pts',(-58.0040209353978,-64.6288503612551,
-10.));
#38585=CARTESIAN_POINT('Ctrl Pts',(-57.8759386493091,-64.5557090804722,
-10.));
#38586=CARTESIAN_POINT('Ctrl Pts',(-57.7488533653713,-64.4831371369214,
-10.));
#38587=CARTESIAN_POINT('Ctrl Pts',(-57.6249505496883,-64.4050638539788,
-10.));
#38588=CARTESIAN_POINT('Ctrl Pts',(-57.5046138228123,-64.321681828014,-10.));
#38589=CARTESIAN_POINT('Ctrl Pts',(-57.3858527597443,-64.239391588771,-10.));
#38590=CARTESIAN_POINT('Ctrl Pts',(-57.2705645355474,-64.1519302045263,
-10.));
#38591=CARTESIAN_POINT('Ctrl Pts',(-57.1591587945395,-64.059453912537,-10.));
#38592=CARTESIAN_POINT('Ctrl Pts',(-57.1274511512158,-64.0331338570733,
-10.));
#38593=CARTESIAN_POINT('Ctrl Pts',(-57.096058289943,-64.0064074129648,-10.));
#38594=CARTESIAN_POINT('Ctrl Pts',(-57.0649903538766,-63.9792778343301,
-10.));
#38595=CARTESIAN_POINT('Ctrl Pts',(-57.049250105535,-63.9655329140301,-10.));
#38596=CARTESIAN_POINT('Ctrl Pts',(-57.0335932654157,-63.9516845134244,
-10.));
#38597=CARTESIAN_POINT('Ctrl Pts',(-57.0180211853758,-63.9377330425149,
-10.));
#38598=CARTESIAN_POINT('Ctrl Pts',(-57.002669719216,-63.9239792258767,-10.));
#38599=CARTESIAN_POINT('Ctrl Pts',(-56.9874066729589,-63.9101306161073,
-10.));
#38600=CARTESIAN_POINT('Ctrl Pts',(-56.9722380221926,-63.8961924090838,
-10.));
#38601=CARTESIAN_POINT('Ctrl Pts',(-56.8611656542019,-63.7941299591337,
-10.));
#38602=CARTESIAN_POINT('Ctrl Pts',(-56.7550656862477,-63.6871906566774,
-10.));
#38603=CARTESIAN_POINT('Ctrl Pts',(-56.6543281719513,-63.5756167101953,
-10.));
#38604=CARTESIAN_POINT('Ctrl Pts',(-56.5578656553598,-63.4687776270703,
-10.));
#38605=CARTESIAN_POINT('Ctrl Pts',(-56.4663199828182,-63.3576879748886,
-10.));
#38606=CARTESIAN_POINT('Ctrl Pts',(-56.3798948426675,-63.2427305259782,
-10.));
#38607=CARTESIAN_POINT('Ctrl Pts',(-56.2936200930167,-63.127973117336,-10.));
#38608=CARTESIAN_POINT('Ctrl Pts',(-56.2124477688271,-63.009360601218,-10.));
#38609=CARTESIAN_POINT('Ctrl Pts',(-56.1366282661676,-62.8872540357093,
-10.));
#38610=CARTESIAN_POINT('Ctrl Pts',(-56.0709511215055,-62.7814816382945,
-10.));
#38611=CARTESIAN_POINT('Ctrl Pts',(-56.0092911147144,-62.6730868734753,
-10.));
#38612=CARTESIAN_POINT('Ctrl Pts',(-55.9518427060363,-62.5622989843102,
-10.));
#38613=CARTESIAN_POINT('Ctrl Pts',(-55.936745519732,-62.5331844197562,-10.));
#38614=CARTESIAN_POINT('Ctrl Pts',(-55.9219393580168,-62.5039045730043,
-10.));
#38615=CARTESIAN_POINT('Ctrl Pts',(-55.9074281095161,-62.4744635977475,
-10.));
#38616=CARTESIAN_POINT('Ctrl Pts',(-55.8951622346766,-62.4495781223432,
-10.));
#38617=CARTESIAN_POINT('Ctrl Pts',(-55.883104401859,-62.4245716453768,-10.));
#38618=CARTESIAN_POINT('Ctrl Pts',(-55.8712719542368,-62.3994789544369,
-10.));
#38619=CARTESIAN_POINT('Ctrl Pts',(-55.8112491416254,-62.2721905070847,
-10.));
#38620=CARTESIAN_POINT('Ctrl Pts',(-55.7569583829528,-62.1425622200571,
-10.));
#38621=CARTESIAN_POINT('Ctrl Pts',(-55.708587651022,-62.0109531311258,-10.));
#38622=CARTESIAN_POINT('Ctrl Pts',(-55.6606046751908,-61.8803990650351,
-10.));
#38623=CARTESIAN_POINT('Ctrl Pts',(-55.6184469915901,-61.7478950950569,
-10.));
#38624=CARTESIAN_POINT('Ctrl Pts',(-55.5823476494758,-61.6137795780905,
-10.));
#38625=CARTESIAN_POINT('Ctrl Pts',(-55.5736126866464,-61.5813276278073,
-10.));
#38626=CARTESIAN_POINT('Ctrl Pts',(-55.5652326741346,-61.5487812944326,
-10.));
#38627=CARTESIAN_POINT('Ctrl Pts',(-55.5572113749489,-61.5161453370011,
-10.));
#38628=CARTESIAN_POINT('Ctrl Pts',(-55.5237968456527,-61.3801929020576,
-10.));
#38629=CARTESIAN_POINT('Ctrl Pts',(-55.4966031557185,-61.2426845833312,
-10.));
#38630=CARTESIAN_POINT('Ctrl Pts',(-55.4756766798638,-61.1040537999156,
-10.));
#38631=CARTESIAN_POINT('Ctrl Pts',(-55.4642433163067,-61.0283116559445,
-10.));
#38632=CARTESIAN_POINT('Ctrl Pts',(-55.4546816621768,-60.9522345623555,
-10.));
#38633=CARTESIAN_POINT('Ctrl Pts',(-55.4470056873523,-60.8758948574348,
-10.));
#38634=CARTESIAN_POINT('Ctrl Pts',(-55.4421350791058,-60.8274553035258,
-10.));
#38635=CARTESIAN_POINT('Ctrl Pts',(-55.438023780299,-60.7789100443811,-10.));
#38636=CARTESIAN_POINT('Ctrl Pts',(-55.434676292913,-60.730277946875,-10.));
#38637=CARTESIAN_POINT('Ctrl Pts',(-55.4333863651453,-60.7115379530405,
-10.));
#38638=CARTESIAN_POINT('Ctrl Pts',(-55.4322097218707,-60.6927825413258,
-10.));
#38639=CARTESIAN_POINT('Ctrl Pts',(-55.4311471090937,-60.6740210732465,
-10.));
#38640=CARTESIAN_POINT('Ctrl Pts',(-55.4233879343862,-60.5370252533725,
-10.));
#38641=CARTESIAN_POINT('Ctrl Pts',(-55.4217193536866,-60.4000017086151,
-10.));
#38642=CARTESIAN_POINT('Ctrl Pts',(-55.4261204723732,-60.2633561204773,
-10.));
#38643=CARTESIAN_POINT('Ctrl Pts',(-55.4305091743339,-60.1270960458709,
-10.));
#38644=CARTESIAN_POINT('Ctrl Pts',(-55.4409335083392,-59.9912110038732,
-10.));
#38645=CARTESIAN_POINT('Ctrl Pts',(-55.4574238144397,-59.8561107187901,
-10.));
#38646=CARTESIAN_POINT('Ctrl Pts',(-55.4736437792729,-59.7232252611376,
-10.));
#38647=CARTESIAN_POINT('Ctrl Pts',(-55.4957326783158,-59.5910983593183,
-10.));
#38648=CARTESIAN_POINT('Ctrl Pts',(-55.523766052396,-59.4601380104691,-10.));
#38649=CARTESIAN_POINT('Ctrl Pts',(-55.536636902664,-59.4000107123332,-10.));
#38650=CARTESIAN_POINT('Ctrl Pts',(-55.5507614616516,-59.3401296350604,
-10.));
#38651=CARTESIAN_POINT('Ctrl Pts',(-55.5661502301349,-59.2805361659048,
-10.));
#38652=CARTESIAN_POINT('Ctrl Pts',(-55.588611195713,-59.1935554006261,-10.));
#38653=CARTESIAN_POINT('Ctrl Pts',(-55.613765125758,-59.1071870025639,-10.));
#38654=CARTESIAN_POINT('Ctrl Pts',(-55.6415742028502,-59.0215529319106,
-10.));
#38655=CARTESIAN_POINT('Ctrl Pts',(-55.6489435652431,-58.998860035712,-10.));
#38656=CARTESIAN_POINT('Ctrl Pts',(-55.6564994205945,-58.9762187463995,
-10.));
#38657=CARTESIAN_POINT('Ctrl Pts',(-55.6642411439561,-58.9536314220447,
-10.));
#38658=CARTESIAN_POINT('Ctrl Pts',(-55.6712493505471,-58.9331842130678,
-10.));
#38659=CARTESIAN_POINT('Ctrl Pts',(-55.6784073237258,-58.9127887539849,
-10.));
#38660=CARTESIAN_POINT('Ctrl Pts',(-55.6857122035675,-58.8924522647103,
-10.));
#38661=CARTESIAN_POINT('Ctrl Pts',(-55.7311295916962,-58.7660120977842,
-10.));
#38662=CARTESIAN_POINT('Ctrl Pts',(-55.7822461341829,-58.6417793104773,
-10.));
#38663=CARTESIAN_POINT('Ctrl Pts',(-55.8388703579017,-58.5201309989478,
-10.));
#38664=CARTESIAN_POINT('Ctrl Pts',(-55.886360628764,-58.4181055602739,-10.));
#38665=CARTESIAN_POINT('Ctrl Pts',(-55.9377259863045,-58.3178982578221,
-10.));
#38666=CARTESIAN_POINT('Ctrl Pts',(-55.9928753041857,-58.2197496529292,
-10.));
#38667=CARTESIAN_POINT('Ctrl Pts',(-56.0250179144583,-58.1625458201878,
-10.));
#38668=CARTESIAN_POINT('Ctrl Pts',(-56.0584462494898,-58.1060416403406,
-10.));
#38669=CARTESIAN_POINT('Ctrl Pts',(-56.0931449566715,-58.0502879461722,
-10.));
#38670=CARTESIAN_POINT('Ctrl Pts',(-56.105064758014,-58.0311352741399,-10.));
#38671=CARTESIAN_POINT('Ctrl Pts',(-56.1171358941824,-58.0120690143348,
-10.));
#38672=CARTESIAN_POINT('Ctrl Pts',(-56.1293531226239,-57.9930985249683,
-10.));
#38673=CARTESIAN_POINT('Ctrl Pts',(-56.2001801780243,-57.8831207253578,
-10.));
#38674=CARTESIAN_POINT('Ctrl Pts',(-56.2758315041106,-57.7764845452586,
-10.));
#38675=CARTESIAN_POINT('Ctrl Pts',(-56.3561469049115,-57.6735585912939,
-10.));
#38676=CARTESIAN_POINT('Ctrl Pts',(-56.4292341049692,-57.5798957356827,
-10.));
#38677=CARTESIAN_POINT('Ctrl Pts',(-56.5061843541636,-57.489305375963,-9.99999999999999));
#38678=CARTESIAN_POINT('Ctrl Pts',(-56.5869001999823,-57.4020947632679,
-9.99999999999999));
#38679=CARTESIAN_POINT('Ctrl Pts',(-56.6479573387169,-57.3361246873252,
-9.99999999999999));
#38680=CARTESIAN_POINT('Ctrl Pts',(-56.711169784743,-57.2720891636053,-10.));
#38681=CARTESIAN_POINT('Ctrl Pts',(-56.7764331763494,-57.2100813324657,
-10.));
#38682=CARTESIAN_POINT('Origin',(-60.,-60.,-6.));
#38683=CARTESIAN_POINT('Origin',(60.,-60.,-3.));
#38684=CARTESIAN_POINT('Ctrl Pts',(60.8043894954945,-64.1864216867795,-3.));
#38685=CARTESIAN_POINT('Ctrl Pts',(60.6804231397008,-64.2229459197079,-3.));
#38686=CARTESIAN_POINT('Ctrl Pts',(60.5549403917413,-64.2536517808237,-3.));
#38687=CARTESIAN_POINT('Ctrl Pts',(60.4283619083555,-64.2786227926487,-3.));
#38688=CARTESIAN_POINT('Ctrl Pts',(60.2999057760435,-64.3039642212482,-3.));
#38689=CARTESIAN_POINT('Ctrl Pts',(60.1703204798203,-64.3233996378784,-3.));
#38690=CARTESIAN_POINT('Ctrl Pts',(60.0400191944093,-64.3369697586679,-3.));
#38691=CARTESIAN_POINT('Ctrl Pts',(59.9818444362653,-64.3430283212709,-3.));
#38692=CARTESIAN_POINT('Ctrl Pts',(59.9235266739776,-64.3479171212406,-3.));
#38693=CARTESIAN_POINT('Ctrl Pts',(59.8651015736501,-64.3516366568403,-3.));
#38694=CARTESIAN_POINT('Ctrl Pts',(59.8415724972579,-64.3531345958559,-3.));
#38695=CARTESIAN_POINT('Ctrl Pts',(59.8180260065396,-64.3544428754694,-3.));
#38696=CARTESIAN_POINT('Ctrl Pts',(59.7944644111293,-64.3555614378551,-3.));
#38697=CARTESIAN_POINT('Ctrl Pts',(59.7710353638239,-64.3566737076565,-3.));
#38698=CARTESIAN_POINT('Ctrl Pts',(59.7476008580321,-64.3575979236003,-3.));
#38699=CARTESIAN_POINT('Ctrl Pts',(59.7241660463876,-64.3583343886706,-3.));
#38700=CARTESIAN_POINT('Ctrl Pts',(59.590446995345,-64.3625366588587,-3.));
#38701=CARTESIAN_POINT('Ctrl Pts',(59.456690295917,-64.3606313991924,-3.));
#38702=CARTESIAN_POINT('Ctrl Pts',(59.3233273468215,-64.352670904561,-3.));
#38703=CARTESIAN_POINT('Ctrl Pts',(59.2153949205287,-64.346228369315,-3.));
#38704=CARTESIAN_POINT('Ctrl Pts',(59.1077197482123,-64.3358188472649,-3.));
#38705=CARTESIAN_POINT('Ctrl Pts',(59.0005240056913,-64.321446190102,-3.));
#38706=CARTESIAN_POINT('Ctrl Pts',(58.9469261344308,-64.3142598615205,-3.));
#38707=CARTESIAN_POINT('Ctrl Pts',(58.8934480606378,-64.3060824109368,-3.));
#38708=CARTESIAN_POINT('Ctrl Pts',(58.8401173770145,-64.2969122626104,-3.));
#38709=CARTESIAN_POINT('Ctrl Pts',(58.8127284789263,-64.2922027737965,-3.));
#38710=CARTESIAN_POINT('Ctrl Pts',(58.785378454751,-64.2872314371142,-3.));
#38711=CARTESIAN_POINT('Ctrl Pts',(58.7580710457004,-64.2819978960498,-3.));
#38712=CARTESIAN_POINT('Ctrl Pts',(58.7384795978033,-64.2782431404488,-3.));
#38713=CARTESIAN_POINT('Ctrl Pts',(58.7189123157833,-64.274353795948,-3.));
#38714=CARTESIAN_POINT('Ctrl Pts',(58.6993815165312,-64.2703322032461,-3.));
#38715=CARTESIAN_POINT('Ctrl Pts',(58.6931277820086,-64.2690444949044,-3.));
#38716=CARTESIAN_POINT('Ctrl Pts',(58.6868774720263,-64.2677431676485,-3.));
#38717=CARTESIAN_POINT('Ctrl Pts',(58.6806306316105,-64.2664282297966,-3.));
#38718=CARTESIAN_POINT('Ctrl Pts',(58.5505753781477,-64.2390520581277,-3.));
#38719=CARTESIAN_POINT('Ctrl Pts',(58.4220248522783,-64.2057808086917,-3.));
#38720=CARTESIAN_POINT('Ctrl Pts',(58.2953075841536,-64.1669086900382,-3.));
#38721=CARTESIAN_POINT('Ctrl Pts',(58.1663244201018,-64.1273414792585,-3.));
#38722=CARTESIAN_POINT('Ctrl Pts',(58.0392399953926,-64.0819712145089,-3.));
#38723=CARTESIAN_POINT('Ctrl Pts',(57.9143959605215,-64.031054382879,-3.));
#38724=CARTESIAN_POINT('Ctrl Pts',(57.7879487637979,-63.9794837120631,-3.));
#38725=CARTESIAN_POINT('Ctrl Pts',(57.6637991096253,-63.9222229571421,-3.));
#38726=CARTESIAN_POINT('Ctrl Pts',(57.5423079332954,-63.8594858324879,-3.));
#38727=CARTESIAN_POINT('Ctrl Pts',(57.4659381105853,-63.8200490336033,-3.));
#38728=CARTESIAN_POINT('Ctrl Pts',(57.390618922556,-63.7784472423405,-3.));
#38729=CARTESIAN_POINT('Ctrl Pts',(57.3164432885815,-63.7347235194873,-3.));
#38730=CARTESIAN_POINT('Ctrl Pts',(57.2554400683084,-63.6987644349004,-3.));
#38731=CARTESIAN_POINT('Ctrl Pts',(57.1952103409945,-63.6613699973526,-3.));
#38732=CARTESIAN_POINT('Ctrl Pts',(57.1358077302662,-63.6225604628414,-3.));
#38733=CARTESIAN_POINT('Ctrl Pts',(57.1208013426853,-63.6127563328618,-3.));
#38734=CARTESIAN_POINT('Ctrl Pts',(57.1058495643152,-63.6028630110964,-3.));
#38735=CARTESIAN_POINT('Ctrl Pts',(57.090962608004,-63.5928872913616,-3.));
#38736=CARTESIAN_POINT('Ctrl Pts',(56.9746403128356,-63.5149399533527,-3.));
#38737=CARTESIAN_POINT('Ctrl Pts',(56.8621130676035,-63.4318607996292,-3.));
#38738=CARTESIAN_POINT('Ctrl Pts',(56.7537373195155,-63.3439210028432,-3.));
#38739=CARTESIAN_POINT('Ctrl Pts',(56.7306086425202,-63.3251536015493,-3.));
#38740=CARTESIAN_POINT('Ctrl Pts',(56.707669073934,-63.3061646372347,-3.));
#38741=CARTESIAN_POINT('Ctrl Pts',(56.6849221396237,-63.2869564466686,-3.));
#38742=CARTESIAN_POINT('Ctrl Pts',(56.579310135636,-63.1977745168753,-3.));
#38743=CARTESIAN_POINT('Ctrl Pts',(56.4778488517895,-63.1038706522824,-3.));
#38744=CARTESIAN_POINT('Ctrl Pts',(56.3807144526095,-63.0056343911719,-3.));
#38745=CARTESIAN_POINT('Ctrl Pts',(56.2824676805631,-62.9062731387887,-3.));
#38746=CARTESIAN_POINT('Ctrl Pts',(56.1886469010809,-62.8024792204072,-3.));
#38747=CARTESIAN_POINT('Ctrl Pts',(56.099462447388,-62.6946104708653,-3.));
#38748=CARTESIAN_POINT('Ctrl Pts',(56.0193271670832,-62.5976867120404,-3.));
#38749=CARTESIAN_POINT('Ctrl Pts',(55.9429351824628,-62.4974722024114,-3.));
#38750=CARTESIAN_POINT('Ctrl Pts',(55.8704637505503,-62.3942009040218,-3.));
#38751=CARTESIAN_POINT('Ctrl Pts',(55.8587176889594,-62.3774628460112,-3.));
#38752=CARTESIAN_POINT('Ctrl Pts',(55.847074674168,-62.3606444428867,-3.));
#38753=CARTESIAN_POINT('Ctrl Pts',(55.8355355278864,-62.343746640643,-3.));
#38754=CARTESIAN_POINT('Ctrl Pts',(55.8253670832934,-62.3288560792734,-3.));
#38755=CARTESIAN_POINT('Ctrl Pts',(55.8152846409939,-62.3139116815137,-3.));
#38756=CARTESIAN_POINT('Ctrl Pts',(55.8052890193779,-62.2989150461428,-3.));
#38757=CARTESIAN_POINT('Ctrl Pts',(55.7260104810182,-62.179971834986,-3.));
#38758=CARTESIAN_POINT('Ctrl Pts',(55.6521810405761,-62.0577313161164,-3.));
#38759=CARTESIAN_POINT('Ctrl Pts',(55.5839783713857,-61.9326058470642,-3.));
#38760=CARTESIAN_POINT('Ctrl Pts',(55.5150429786189,-61.8061361141837,-3.));
#38761=CARTESIAN_POINT('Ctrl Pts',(55.4518553300978,-61.6767185682717,-3.));
#38762=CARTESIAN_POINT('Ctrl Pts',(55.3946314866188,-61.5447373561503,-3.));
#38763=CARTESIAN_POINT('Ctrl Pts',(55.3737738336291,-61.4966312144404,-3.));
#38764=CARTESIAN_POINT('Ctrl Pts',(55.3537088536932,-61.4481841219945,-3.));
#38765=CARTESIAN_POINT('Ctrl Pts',(55.3344483045972,-61.3994135479579,-3.));
#38766=CARTESIAN_POINT('Ctrl Pts',(55.2818816460659,-61.2663069527623,-3.));
#38767=CARTESIAN_POINT('Ctrl Pts',(55.2353035754996,-61.1307925669745,-3.));
#38768=CARTESIAN_POINT('Ctrl Pts',(55.1947264376106,-60.9932848139183,-3.));
#38769=CARTESIAN_POINT('Ctrl Pts',(55.1709932925155,-60.9128579621302,-3.));
#38770=CARTESIAN_POINT('Ctrl Pts',(55.149313907764,-60.8317486932218,-3.));
#38771=CARTESIAN_POINT('Ctrl Pts',(55.1296983571844,-60.7500368036683,-3.));
#38772=CARTESIAN_POINT('Ctrl Pts',(55.1222103856338,-60.7188443932466,-3.));
#38773=CARTESIAN_POINT('Ctrl Pts',(55.1150232214001,-60.6875641489917,-3.));
#38774=CARTESIAN_POINT('Ctrl Pts',(55.1081376485859,-60.656200451121,-3.));
#38775=CARTESIAN_POINT('Ctrl Pts',(55.1026350484047,-60.6311361762608,-3.));
#38776=CARTESIAN_POINT('Ctrl Pts',(55.0973241980932,-60.6060139679337,-3.));
#38777=CARTESIAN_POINT('Ctrl Pts',(55.0922112268448,-60.5808651531185,-3.));
#38778=CARTESIAN_POINT('Ctrl Pts',(55.0630684054444,-60.4375223915442,-3.));
#38779=CARTESIAN_POINT('Ctrl Pts',(55.0403125826176,-60.293155530728,-3.));
#38780=CARTESIAN_POINT('Ctrl Pts',(55.0238938318386,-60.148221636185,-3.));
#38781=CARTESIAN_POINT('Ctrl Pts',(55.007312988479,-60.0018568953307,-3.));
#38782=CARTESIAN_POINT('Ctrl Pts',(54.997194722033,-59.8549131523385,-3.));
#38783=CARTESIAN_POINT('Ctrl Pts',(54.9935343836614,-59.7078349417394,-3.));
#38784=CARTESIAN_POINT('Ctrl Pts',(54.9898705017823,-59.5606143473797,-3.));
#38785=CARTESIAN_POINT('Ctrl Pts',(54.9926768760983,-59.4132582467513,-3.));
#38786=CARTESIAN_POINT('Ctrl Pts',(55.0019985245375,-59.2661976649384,-3.));
#38787=CARTESIAN_POINT('Ctrl Pts',(55.007624207338,-59.1774455315433,-3.));
#38788=CARTESIAN_POINT('Ctrl Pts',(55.0156238601694,-59.0888007981271,-3.));
#38789=CARTESIAN_POINT('Ctrl Pts',(55.0260165547263,-59.0003574320813,-3.));
#38790=CARTESIAN_POINT('Ctrl Pts',(55.0384682951938,-58.8943912811428,-3.));
#38791=CARTESIAN_POINT('Ctrl Pts',(55.0543549121591,-58.7887140498665,-3.));
#38792=CARTESIAN_POINT('Ctrl Pts',(55.0736213077518,-58.683468118019,-3.));
#38793=CARTESIAN_POINT('Ctrl Pts',(56.3967816198431,-56.3921449163111,-3.));
#38794=CARTESIAN_POINT('Ctrl Pts',(56.5101573174658,-56.2959035170913,-3.));
#38795=CARTESIAN_POINT('Ctrl Pts',(56.6276776345426,-56.2048633879271,-2.99999999999999));
#38796=CARTESIAN_POINT('Ctrl Pts',(56.7489442469526,-56.1192063567908,-2.99999999999999));
#38797=CARTESIAN_POINT('Ctrl Pts',(56.870321847077,-56.0334709291534,-3.));
#38798=CARTESIAN_POINT('Ctrl Pts',(56.9954533551651,-55.9531281614561,-3.));
#38799=CARTESIAN_POINT('Ctrl Pts',(57.1239602535777,-55.8784079648384,-3.));
#38800=CARTESIAN_POINT('Ctrl Pts',(57.1803120252051,-55.8456422883824,-3.));
#38801=CARTESIAN_POINT('Ctrl Pts',(57.2373130617797,-55.81395843212,-3.));
#38802=CARTESIAN_POINT('Ctrl Pts',(57.2949321471059,-55.7833788896179,-3.));
#38803=CARTESIAN_POINT('Ctrl Pts',(57.3242693939211,-55.7678090557547,-3.));
#38804=CARTESIAN_POINT('Ctrl Pts',(57.3537668697723,-55.7525255380034,-3.));
#38805=CARTESIAN_POINT('Ctrl Pts',(57.3834204746729,-55.7375315028531,-3.));
#38806=CARTESIAN_POINT('Ctrl Pts',(57.405034144051,-55.7266027770044,-3.));
#38807=CARTESIAN_POINT('Ctrl Pts',(57.42673014855,-55.7158282226589,-3.));
#38808=CARTESIAN_POINT('Ctrl Pts',(57.4484948211874,-55.70521475433,-3.));
#38809=CARTESIAN_POINT('Ctrl Pts',(57.5800081375807,-55.641082734445,-3.));
#38810=CARTESIAN_POINT('Ctrl Pts',(57.7141415282411,-55.5827700253566,-3.));
#38811=CARTESIAN_POINT('Ctrl Pts',(57.8505257224348,-55.5304872340483,-3.));
#38812=CARTESIAN_POINT('Ctrl Pts',(57.9684329260342,-55.4852875849543,-3.));
#38813=CARTESIAN_POINT('Ctrl Pts',(58.0880229434954,-55.4445953492595,-3.));
#38814=CARTESIAN_POINT('Ctrl Pts',(58.2090620298704,-55.4085779565464,-3.));
#38815=CARTESIAN_POINT('Ctrl Pts',(58.2695815730579,-55.3905692601899,-3.));
#38816=CARTESIAN_POINT('Ctrl Pts',(58.330463417215,-55.3737297422003,-3.));
#38817=CARTESIAN_POINT('Ctrl Pts',(58.3916783286023,-55.3580832189175,-3.));
#38818=CARTESIAN_POINT('Ctrl Pts',(58.4205106378725,-55.3507136844679,-3.));
#38819=CARTESIAN_POINT('Ctrl Pts',(58.4494168337012,-55.3436088350695,-3.));
#38820=CARTESIAN_POINT('Ctrl Pts',(58.4783938465815,-55.3367713125311,-3.));
#38821=CARTESIAN_POINT('Ctrl Pts',(58.5046586640999,-55.3305737695858,-3.));
#38822=CARTESIAN_POINT('Ctrl Pts',(58.5309855472865,-55.3245950943735,-3.));
#38823=CARTESIAN_POINT('Ctrl Pts',(58.5573456293696,-55.3188428589396,-3.));
#38824=CARTESIAN_POINT('Ctrl Pts',(58.5636487149566,-55.3174674143511,-3.));
#38825=CARTESIAN_POINT('Ctrl Pts',(58.5699539791781,-55.316104846781,-3.));
#38826=CARTESIAN_POINT('Ctrl Pts',(58.5762613901465,-55.3147551718543,-3.));
#38827=CARTESIAN_POINT('Ctrl Pts',(58.7158133058752,-55.2848935182244,-3.));
#38828=CARTESIAN_POINT('Ctrl Pts',(58.856415423564,-55.2613386928272,-3.));
#38829=CARTESIAN_POINT('Ctrl Pts',(58.9976459175114,-55.2440350244678,-3.));
#38830=CARTESIAN_POINT('Ctrl Pts',(59.1398152514854,-55.2266163287087,-3.));
#38831=CARTESIAN_POINT('Ctrl Pts',(59.282622160811,-55.2155322372454,-3.));
#38832=CARTESIAN_POINT('Ctrl Pts',(59.4256371798734,-55.2107785461175,-3.));
#38833=CARTESIAN_POINT('Ctrl Pts',(59.5672053579002,-55.2060729466897,-3.));
#38834=CARTESIAN_POINT('Ctrl Pts',(59.7089782161267,-55.2075704983195,-3.));
#38835=CARTESIAN_POINT('Ctrl Pts',(59.8505282447802,-55.2153163967581,-3.));
#38836=CARTESIAN_POINT('Ctrl Pts',(59.9398962674022,-55.2202067922845,-3.));
#38837=CARTESIAN_POINT('Ctrl Pts',(60.0291752112974,-55.2275887928648,-3.));
#38838=CARTESIAN_POINT('Ctrl Pts',(60.1182531584719,-55.2374835632598,-3.));
#38839=CARTESIAN_POINT('Ctrl Pts',(60.1850616188527,-55.2449046410561,-3.));
#38840=CARTESIAN_POINT('Ctrl Pts',(60.2517569527163,-55.2537393075563,-3.));
#38841=CARTESIAN_POINT('Ctrl Pts',(60.3182902449357,-55.2639992322029,-3.));
#38842=CARTESIAN_POINT('Ctrl Pts',(60.3359230334911,-55.2667183383203,-3.));
#38843=CARTESIAN_POINT('Ctrl Pts',(60.3535444318793,-55.2695375625048,-3.));
#38844=CARTESIAN_POINT('Ctrl Pts',(60.3711535096332,-55.2724571492995,-3.));
#38845=CARTESIAN_POINT('Ctrl Pts',(60.3893513068264,-55.2754743458341,-3.));
#38846=CARTESIAN_POINT('Ctrl Pts',(60.4075272689998,-55.2785972997792,-3.));
#38847=CARTESIAN_POINT('Ctrl Pts',(60.4256778377815,-55.2818254998691,-3.));
#38848=CARTESIAN_POINT('Ctrl Pts',(60.5629886030953,-55.3062471381247,-3.));
#38849=CARTESIAN_POINT('Ctrl Pts',(60.6988966057003,-55.3366961501879,-3.));
#38850=CARTESIAN_POINT('Ctrl Pts',(60.8330040649825,-55.3731700437297,-3.));
#38851=CARTESIAN_POINT('Ctrl Pts',(60.8581918683798,-55.3800204998087,-3.));
#38852=CARTESIAN_POINT('Ctrl Pts',(60.8833161142963,-55.3870836289852,-3.));
#38853=CARTESIAN_POINT('Ctrl Pts',(60.9083741009857,-55.3943596098957,-3.));
#38854=CARTESIAN_POINT('Ctrl Pts',(61.0423381780513,-55.4332581886002,-3.));
#38855=CARTESIAN_POINT('Ctrl Pts',(61.1744105711619,-55.4782367322963,-3.));
#38856=CARTESIAN_POINT('Ctrl Pts',(61.3042176736396,-55.529086521121,-3.));
#38857=CARTESIAN_POINT('Ctrl Pts',(61.4335910147022,-55.5797663910742,-3.));
#38858=CARTESIAN_POINT('Ctrl Pts',(61.5607148281865,-55.6362788365258,-3.));
#38859=CARTESIAN_POINT('Ctrl Pts',(61.6851875762294,-55.6984578531799,-3.));
#38860=CARTESIAN_POINT('Ctrl Pts',(61.7912746668737,-55.7514525132937,-3.));
#38861=CARTESIAN_POINT('Ctrl Pts',(61.8954357201455,-55.8085642062721,-3.));
#38862=CARTESIAN_POINT('Ctrl Pts',(61.9973985794147,-55.8697095293407,-3.));
#38863=CARTESIAN_POINT('Ctrl Pts',(62.0157427701011,-55.8807102160024,-3.));
#38864=CARTESIAN_POINT('Ctrl Pts',(62.0340157461252,-55.8918415036851,-3.));
#38865=CARTESIAN_POINT('Ctrl Pts',(62.0522158358394,-55.9031029592681,-3.));
#38866=CARTESIAN_POINT('Ctrl Pts',(62.0686109696278,-55.9132475834889,-3.));
#38867=CARTESIAN_POINT('Ctrl Pts',(62.0849391036014,-55.9234929984919,-3.));
#38868=CARTESIAN_POINT('Ctrl Pts',(62.1011958332953,-55.9338364137878,-3.));
#38869=CARTESIAN_POINT('Ctrl Pts',(62.216094328377,-56.0069410832934,-3.));
#38870=CARTESIAN_POINT('Ctrl Pts',(62.327484591668,-56.0849724350915,-3.));
#38871=CARTESIAN_POINT('Ctrl Pts',(62.4350223033254,-56.1677286783298,-3.));
#38872=CARTESIAN_POINT('Ctrl Pts',(62.5416035161753,-56.2497488425985,-3.));
#38873=CARTESIAN_POINT('Ctrl Pts',(62.6444009573507,-56.3364107491799,-3.));
#38874=CARTESIAN_POINT('Ctrl Pts',(62.7430433843076,-56.4275538646491,-3.));
#38875=CARTESIAN_POINT('Ctrl Pts',(62.7758260507536,-56.4578442219066,-3.));
#38876=CARTESIAN_POINT('Ctrl Pts',(62.8081494679239,-56.4886297854746,-3.));
#38877=CARTESIAN_POINT('Ctrl Pts',(62.839998957236,-56.5199054011849,-3.));
#38878=CARTESIAN_POINT('Ctrl Pts',(62.9365721091775,-56.6147384692591,-3.));
#38879=CARTESIAN_POINT('Ctrl Pts',(63.0287915129428,-56.7140757933899,-3.));
#38880=CARTESIAN_POINT('Ctrl Pts',(63.1163847284822,-56.8175811487369,-3.));
#38881=CARTESIAN_POINT('Ctrl Pts',(63.1636034329842,-56.8733775795267,-3.));
#38882=CARTESIAN_POINT('Ctrl Pts',(63.2094769709409,-56.9303855512555,-3.));
#38883=CARTESIAN_POINT('Ctrl Pts',(63.253956548673,-56.988554049022,-3.));
#38884=CARTESIAN_POINT('Ctrl Pts',(63.2715142745527,-57.0115152952992,-3.));
#38885=CARTESIAN_POINT('Ctrl Pts',(63.2888547484807,-57.0346573799277,-3.));
#38886=CARTESIAN_POINT('Ctrl Pts',(63.3059747738216,-57.0579771914561,-3.));
#38887=CARTESIAN_POINT('Ctrl Pts',(63.3199565484319,-57.0770222770943,-3.));
#38888=CARTESIAN_POINT('Ctrl Pts',(63.3337936340754,-57.0961893542109,-3.));
#38889=CARTESIAN_POINT('Ctrl Pts',(63.3474683163229,-57.1154538857274,-3.));
#38890=CARTESIAN_POINT('Ctrl Pts',(63.42423513697,-57.2236009570091,-3.));
#38891=CARTESIAN_POINT('Ctrl Pts',(63.4959842891767,-57.3349453279282,-3.));
#38892=CARTESIAN_POINT('Ctrl Pts',(63.5625181311883,-57.4491372731137,-3.));
#38893=CARTESIAN_POINT('Ctrl Pts',(63.6288088907953,-57.5629120162892,-3.));
#38894=CARTESIAN_POINT('Ctrl Pts',(63.6899226778965,-57.6795143212801,-3.00000000000001));
#38895=CARTESIAN_POINT('Ctrl Pts',(63.7456163898184,-57.7986178371963,-3.));
#38896=CARTESIAN_POINT('Ctrl Pts',(63.8003210973205,-57.9156063225357,-3.));
#38897=CARTESIAN_POINT('Ctrl Pts',(63.8497966746643,-58.0350086748614,-3.));
#38898=CARTESIAN_POINT('Ctrl Pts',(63.8937635413419,-58.1565237236026,-3.));
#38899=CARTESIAN_POINT('Ctrl Pts',(63.9160764751396,-58.2181919170143,-3.));
#38900=CARTESIAN_POINT('Ctrl Pts',(63.9369698330113,-58.2804043019419,-3.));
#38901=CARTESIAN_POINT('Ctrl Pts',(63.9564018939967,-58.3431214778336,-3.));
#38902=CARTESIAN_POINT('Ctrl Pts',(63.982990724922,-58.4289372020198,-3.));
#38903=CARTESIAN_POINT('Ctrl Pts',(64.0068440160574,-58.5156982224054,-3.));
#38904=CARTESIAN_POINT('Ctrl Pts',(64.0279239112946,-58.6032685651143,-3.));
#38905=CARTESIAN_POINT('Origin',(60.,-60.,-13.3123464956316));
#38906=CARTESIAN_POINT('Ctrl Pts',(65.0992547697949,-59.9999087515425,-9.56234649563159));
#38907=CARTESIAN_POINT('Ctrl Pts',(65.0993446299649,-59.8930270626359,-9.55734157105847));
#38908=CARTESIAN_POINT('Ctrl Pts',(65.0703981688746,-58.9539304661534,-9.51336443385491));
#38909=CARTESIAN_POINT('Ctrl Pts',(64.5173398889406,-57.2140033571025,-9.43041508402093));
#38910=CARTESIAN_POINT('Ctrl Pts',(62.675830507843,-55.416544576301,-9.31349844612964));
#38911=CARTESIAN_POINT('Ctrl Pts',(60.2052631333967,-54.6966046481226,-9.19658180823834));
#38912=CARTESIAN_POINT('Ctrl Pts',(57.6864406075043,-55.2234346241344,-9.07966517034706));
#38913=CARTESIAN_POINT('Ctrl Pts',(55.7115103085732,-56.8731820153015,-8.96274853245577));
#38914=CARTESIAN_POINT('Ctrl Pts',(54.7447564371768,-59.2580098897298,-8.84583189456448));
#38915=CARTESIAN_POINT('Ctrl Pts',(55.0134521540628,-61.8172711292634,-8.72891525667319));
#38916=CARTESIAN_POINT('Ctrl Pts',(56.4544300397442,-63.9493126239243,-8.6119986187819));
#38917=CARTESIAN_POINT('Ctrl Pts',(58.7289322008878,-65.1529132302293,-8.4950819808906));
#38918=CARTESIAN_POINT('Ctrl Pts',(61.3022482555275,-65.145123605987,-8.37816534299932));
#38919=CARTESIAN_POINT('Ctrl Pts',(63.5694203198369,-63.9277667461252,-8.26124870510802));
#38920=CARTESIAN_POINT('Ctrl Pts',(64.8552427738849,-62.0002410971054,-8.15597575598546));
#38921=CARTESIAN_POINT('Ctrl Pts',(65.09834724995,-60.583627205272,-8.08967501949331));
#38922=CARTESIAN_POINT('Ctrl Pts',(65.0988481317111,-59.9998830050765,-8.06234649563159));
#38923=CARTESIAN_POINT('Ctrl Pts',(65.0987893869763,-59.9998803238954,-9.68765350436841));
#38924=CARTESIAN_POINT('Ctrl Pts',(65.0989958636635,-59.7264419125984,-9.67485236502099));
#38925=CARTESIAN_POINT('Ctrl Pts',(65.0114730856874,-58.6206707254151,-9.62307901304313));
#38926=CARTESIAN_POINT('Ctrl Pts',(64.2231822374133,-56.7854927040709,-9.53233344843484));
#38927=CARTESIAN_POINT('Ctrl Pts',(62.2146698199313,-55.1767965300925,-9.41541681054356));
#38928=CARTESIAN_POINT('Ctrl Pts',(59.6855379300098,-54.7019554558395,-9.29850017265226));
#38929=CARTESIAN_POINT('Ctrl Pts',(57.2303209690299,-55.4726378662523,-9.18158353476098));
#38930=CARTESIAN_POINT('Ctrl Pts',(55.4262302424911,-57.3076473811431,-9.06466689686968));
#38931=CARTESIAN_POINT('Ctrl Pts',(54.6973796557714,-59.775601760132,-8.9477502589784));
#38932=CARTESIAN_POINT('Ctrl Pts',(55.2151175549311,-62.2963084797734,-8.8308336210871));
#38933=CARTESIAN_POINT('Ctrl Pts',(56.8577277980376,-64.2771790632985,-8.71391698319582));
#38934=CARTESIAN_POINT('Ctrl Pts',(59.2390517062358,-65.2525319290857,-8.59700034530453));
#38935=CARTESIAN_POINT('Ctrl Pts',(61.7992659861865,-64.9930728587382,-8.48008370741324));
#38936=CARTESIAN_POINT('Ctrl Pts',(63.9364928774652,-63.5597974904555,-8.36316706952195));
#38937=CARTESIAN_POINT('Ctrl Pts',(64.9468057743096,-61.667113625277,-8.26569033517367));
#38938=CARTESIAN_POINT('Ctrl Pts',(65.0986024103333,-60.4172707879301,-8.20718581345583));
#38939=CARTESIAN_POINT('Ctrl Pts',(65.0986049509612,-59.9999990973777,-8.18765350436841));
#38940=CARTESIAN_POINT('Ctrl Pts',(56.7766472160421,-57.2101674189746,-10.));
#38941=CARTESIAN_POINT('Ctrl Pts',(56.3212170277455,-57.7363682294923,-9.96102778736957));
#38942=CARTESIAN_POINT('Ctrl Pts',(55.6734222457032,-59.0156058825944,-9.88308336210871));
#38943=CARTESIAN_POINT('Ctrl Pts',(55.718911726351,-61.1667236883496,-9.76616672421742));
#38944=CARTESIAN_POINT('Ctrl Pts',(56.7709224459031,-63.0432885509004,-9.64925008632614));
#38945=CARTESIAN_POINT('Ctrl Pts',(58.5820372950378,-64.2045560436868,-9.53233344843484));
#38946=CARTESIAN_POINT('Ctrl Pts',(60.7265123811851,-64.3773165159145,-9.41541681054356));
#38947=CARTESIAN_POINT('Ctrl Pts',(62.7001877066388,-63.5210484489301,-9.29850017265226));
#38948=CARTESIAN_POINT('Ctrl Pts',(64.0390812798309,-61.8370072052861,-9.18158353476097));
#38949=CARTESIAN_POINT('Ctrl Pts',(64.4284304814287,-59.7211123027545,-9.06466689686969));
#38950=CARTESIAN_POINT('Ctrl Pts',(63.7767052258391,-57.6707778606252,-8.9477502589784));
#38951=CARTESIAN_POINT('Ctrl Pts',(62.2371181515856,-56.1680191270389,-8.83083362108711));
#38952=CARTESIAN_POINT('Ctrl Pts',(60.1716094798333,-55.5661160256809,-8.71391698319581));
#38953=CARTESIAN_POINT('Ctrl Pts',(58.0657572680508,-56.0065702692067,-8.59700034530453));
#38954=CARTESIAN_POINT('Ctrl Pts',(56.4146241312899,-57.385835444446,-8.48008370741324));
#38955=CARTESIAN_POINT('Ctrl Pts',(55.6063731499676,-59.3796619258518,-8.36316706952194));
#38956=CARTESIAN_POINT('Ctrl Pts',(55.8310152054854,-61.519322773887,-8.24625043163066));
#38957=CARTESIAN_POINT('Ctrl Pts',(57.0357394115374,-63.3018081419473,-8.12933379373937));
#38958=CARTESIAN_POINT('Ctrl Pts',(58.9373284903676,-64.3080739557693,-8.01241715584808));
#38959=CARTESIAN_POINT('Ctrl Pts',(61.0887398143388,-64.301561469371,-7.89550051795679));
#38960=CARTESIAN_POINT('Ctrl Pts',(62.9842005929525,-63.2837947908868,-7.7785838800655));
#38961=CARTESIAN_POINT('Ctrl Pts',(64.1781085723986,-61.4940544999883,-7.66166724217421));
#38962=CARTESIAN_POINT('Ctrl Pts',(64.3897900935251,-59.3530565503543,-7.54475060428292));
#38963=CARTESIAN_POINT('Ctrl Pts',(63.5694792575328,-57.3641953191966,-7.42783396639163));
#38964=CARTESIAN_POINT('Ctrl Pts',(61.9100261963604,-55.9948800845054,-7.31091732850034));
#38965=CARTESIAN_POINT('Ctrl Pts',(59.80154101086,-55.5673455413723,-7.19400069060905));
#38966=CARTESIAN_POINT('Ctrl Pts',(57.7397244908903,-56.1814012155801,-7.07708405271776));
#38967=CARTESIAN_POINT('Ctrl Pts',(56.2092451179269,-57.6941993755668,-6.96016741482647));
#38968=CARTESIAN_POINT('Ctrl Pts',(55.5699911243389,-59.7468398452376,-6.84325077693518));
#38969=CARTESIAN_POINT('Ctrl Pts',(55.9720482818244,-61.8638130771427,-6.7263341390439));
#38970=CARTESIAN_POINT('Ctrl Pts',(57.3213007331271,-63.5322807113462,-6.60941750115261));
#38971=CARTESIAN_POINT('Ctrl Pts',(59.9592778669654,-64.6795929264981,-6.45352865063088));
#38972=CARTESIAN_POINT('Ctrl Pts',(63.6618729284737,-63.4214740641546,-6.25866758747874));
#38973=CARTESIAN_POINT('Ctrl Pts',(64.8778950002124,-58.8502441638021,-6.02483431169615));
#38974=CARTESIAN_POINT('Ctrl Pts',(62.2898180510687,-55.9187034483083,-5.82997324854401));
#38975=CARTESIAN_POINT('Ctrl Pts',(59.4304512147069,-55.6036320709857,-5.67408439802228));
#38976=CARTESIAN_POINT('Ctrl Pts',(57.4305231142087,-56.3811627884273,-5.557167760131));
#38977=CARTESIAN_POINT('Ctrl Pts',(56.0297440088743,-58.0185520275981,-5.4402511222397));
#38978=CARTESIAN_POINT('Ctrl Pts',(55.5646048065108,-60.1175098853142,-5.32333448434842));
#38979=CARTESIAN_POINT('Ctrl Pts',(56.1411247560802,-62.1908043968745,-5.20641784645713));
#38980=CARTESIAN_POINT('Ctrl Pts',(57.6253115974258,-63.7481550809134,-5.08950120856584));
#38981=CARTESIAN_POINT('Ctrl Pts',(59.6675354162127,-64.4247771592285,-4.97258457067455));
#38982=CARTESIAN_POINT('Ctrl Pts',(61.7880226520338,-64.0609879932485,-4.85566793278326));
#38983=CARTESIAN_POINT('Ctrl Pts',(63.4881170828804,-62.7425958702478,-4.73875129489197));
#38984=CARTESIAN_POINT('Ctrl Pts',(64.368216261483,-60.7794079721259,-4.62183465700068));
#38985=CARTESIAN_POINT('Ctrl Pts',(64.2213857622817,-58.6330092727112,-4.50491801910939));
#38986=CARTESIAN_POINT('Ctrl Pts',(63.0821590289871,-56.8079659797403,-4.3880013812181));
#38987=CARTESIAN_POINT('Ctrl Pts',(61.2183485971665,-55.7333387017859,-4.27108474332681));
#38988=CARTESIAN_POINT('Ctrl Pts',(59.0681189462196,-55.6617543251732,-4.15416810543552));
#38989=CARTESIAN_POINT('Ctrl Pts',(57.13696370596,-56.6100443722557,-4.03725146754423));
#38990=CARTESIAN_POINT('Ctrl Pts',(55.8788768822095,-58.3552750250779,-3.92033482965294));
#38991=CARTESIAN_POINT('Ctrl Pts',(55.5896202375636,-60.4871625334629,-3.80341819176165));
#38992=CARTESIAN_POINT('Ctrl Pts',(56.3371953794376,-62.5045233639532,-3.68650155387036));
#38993=CARTESIAN_POINT('Ctrl Pts',(57.9458546871605,-63.9330986778457,-3.56958491597908));
#38994=CARTESIAN_POINT('Ctrl Pts',(60.0374221724598,-64.4370456883152,-3.45266827808778));
#38995=CARTESIAN_POINT('Ctrl Pts',(62.1201892117601,-63.8978931193146,-3.3357516401965));
#38996=CARTESIAN_POINT('Ctrl Pts',(63.7045295455676,-62.4423874949933,-3.2188350023052));
#38997=CARTESIAN_POINT('Ctrl Pts',(64.4179625394253,-60.412707063655,-3.10191836441392));
#38998=CARTESIAN_POINT('Ctrl Pts',(64.0928111495996,-58.285996892823,-2.98500172652263));
#38999=CARTESIAN_POINT('Ctrl Pts',(62.8054238049257,-56.5622471978326,-2.86808508863134));
#39000=CARTESIAN_POINT('Ctrl Pts',(60.8586569290977,-55.6466485037356,-2.75116845074005));
#39001=CARTESIAN_POINT('Ctrl Pts',(58.7097669209642,-55.7545782960891,-2.63425181284876));
#39002=CARTESIAN_POINT('Ctrl Pts',(57.4799483719373,-56.4918932825098,-2.5563073875879));
#39003=CARTESIAN_POINT('Ctrl Pts',(56.9875426643246,-56.9836661655686,-2.51733517495747));
#39004=CARTESIAN_POINT('Ctrl Pts',(56.5659409116095,-57.0277997563163,-10.1608882750142));
#39005=CARTESIAN_POINT('Ctrl Pts',(56.0807398547996,-57.5883976172362,-10.1219160623837));
#39006=CARTESIAN_POINT('Ctrl Pts',(55.3905995854019,-58.9512573422744,-10.0439716371229));
#39007=CARTESIAN_POINT('Ctrl Pts',(55.4390626531811,-61.2429908713554,-9.9270549992316));
#39008=CARTESIAN_POINT('Ctrl Pts',(56.5598419208249,-63.242224294786,-9.81013836134031));
#39009=CARTESIAN_POINT('Ctrl Pts',(58.4893469501049,-64.4794023062971,-9.69322172344902));
#39010=CARTESIAN_POINT('Ctrl Pts',(60.7740035337905,-64.663455901895,-9.57630508555773));
#39011=CARTESIAN_POINT('Ctrl Pts',(62.8766954025297,-63.7512147248943,-9.45938844766644));
#39012=CARTESIAN_POINT('Ctrl Pts',(64.3031106761823,-61.9570899344768,-9.34247180977515));
#39013=CARTESIAN_POINT('Ctrl Pts',(64.7179111196705,-59.7028817831754,-9.22555517188386));
#39014=CARTESIAN_POINT('Ctrl Pts',(64.0235834468729,-57.5185196927843,-9.10863853399257));
#39015=CARTESIAN_POINT('Ctrl Pts',(62.3833556036714,-55.9175276101262,-8.99172189610129));
#39016=CARTESIAN_POINT('Ctrl Pts',(60.1828273643545,-55.2762788998282,-8.87480525820999));
#39017=CARTESIAN_POINT('Ctrl Pts',(57.9393183812019,-55.7455250541826,-8.7578886203187));
#39018=CARTESIAN_POINT('Ctrl Pts',(56.180252857051,-57.2149509680645,-8.64097198242742));
#39019=CARTESIAN_POINT('Ctrl Pts',(55.3191675790373,-59.3391112471445,-8.52405534453612));
#39020=CARTESIAN_POINT('Ctrl Pts',(55.5584941883445,-61.6186388923458,-8.40713870664483));
#39021=CARTESIAN_POINT('Ctrl Pts',(56.8419696209397,-63.5176429692729,-8.29022206875355));
#39022=CARTESIAN_POINT('Ctrl Pts',(58.867863060541,-64.589687047256,-8.17330543086226));
#39023=CARTESIAN_POINT('Ctrl Pts',(61.159909294735,-64.5827488482429,-8.05638879297097));
#39024=CARTESIAN_POINT('Ctrl Pts',(63.1792738352472,-63.4984521092996,-7.93947215507967));
#39025=CARTESIAN_POINT('Ctrl Pts',(64.4512259988217,-61.5917188648323,-7.82255551718839));
#39026=CARTESIAN_POINT('Ctrl Pts',(64.6767448607616,-59.3107667134707,-7.70563887929709));
#39027=CARTESIAN_POINT('Ctrl Pts',(63.8028113913429,-57.1918962564746,-7.58872224140581));
#39028=CARTESIAN_POINT('Ctrl Pts',(62.0348820803355,-55.7330706975828,-7.47180560351451));
#39029=CARTESIAN_POINT('Ctrl Pts',(59.7885680094587,-55.2775887873327,-7.35488896562323));
#39030=CARTESIAN_POINT('Ctrl Pts',(57.5919732729987,-55.9317844680803,-7.23797232773194));
#39031=CARTESIAN_POINT('Ctrl Pts',(55.9614484894639,-57.5434722411524,-7.12105568984065));
#39032=CARTESIAN_POINT('Ctrl Pts',(55.2804073085556,-59.7302911010526,-7.00413905194936));
#39033=CARTESIAN_POINT('Ctrl Pts',(55.7087464101851,-61.9856480706912,-6.88722241405807));
#39034=CARTESIAN_POINT('Ctrl Pts',(57.1461977080973,-63.7631812254352,-6.77030577616678));
#39035=CARTESIAN_POINT('Ctrl Pts',(59.9566159150367,-64.9854917212868,-6.61441692564506));
#39036=CARTESIAN_POINT('Ctrl Pts',(63.901244714243,-63.6451312944018,-6.41955586249291));
#39037=CARTESIAN_POINT('Ctrl Pts',(65.1967565390488,-58.7750861468296,-6.18572258671033));
#39038=CARTESIAN_POINT('Ctrl Pts',(62.4395004258199,-55.6519144955196,-5.99086152355818));
#39039=CARTESIAN_POINT('Ctrl Pts',(59.3932205645775,-55.316247319351,-5.83497267303646));
#39040=CARTESIAN_POINT('Ctrl Pts',(57.2625598116423,-56.1446041905014,-5.71805603514517));
#39041=CARTESIAN_POINT('Ctrl Pts',(55.770213630535,-57.8890273966708,-5.60113939725388));
#39042=CARTESIAN_POINT('Ctrl Pts',(55.2746688942615,-60.1251913509584,-5.48422275936259));
#39043=CARTESIAN_POINT('Ctrl Pts',(55.8888751897406,-62.3340143801247,-5.36730612147131));
#39044=CARTESIAN_POINT('Ctrl Pts',(57.4700813601475,-63.9931670167679,-5.25038948358002));
#39045=CARTESIAN_POINT('Ctrl Pts',(59.6458026464851,-64.7140189846344,-5.13347284568873));
#39046=CARTESIAN_POINT('Ctrl Pts',(61.9049033258238,-64.3264494024561,-5.01655620779743));
#39047=CARTESIAN_POINT('Ctrl Pts',(63.7161306790402,-62.9218757316543,-4.89963956990615));
#39048=CARTESIAN_POINT('Ctrl Pts',(64.6537607758782,-60.8303568394882,-4.78272293201486));
#39049=CARTESIAN_POINT('Ctrl Pts',(64.4973321613174,-58.5436508984823,-4.66580629412357));
#39050=CARTESIAN_POINT('Ctrl Pts',(63.2836356845687,-56.5993069414311,-4.54888965623228));
#39051=CARTESIAN_POINT('Ctrl Pts',(61.2979904321209,-55.4544327009018,-4.43197301834099));
#39052=CARTESIAN_POINT('Ctrl Pts',(59.0072031153524,-55.3781689483529,-4.3150563804497));
#39053=CARTESIAN_POINT('Ctrl Pts',(56.9498108134885,-56.3884474604725,-4.19813974255841));
#39054=CARTESIAN_POINT('Ctrl Pts',(55.6094845195171,-58.2477615307441,-4.08122310466712));
#39055=CARTESIAN_POINT('Ctrl Pts',(55.3013195509269,-60.5190077033726,-3.96430646677583));
#39056=CARTESIAN_POINT('Ctrl Pts',(56.0977626901898,-62.6682407407822,-3.84738982888454));
#39057=CARTESIAN_POINT('Ctrl Pts',(57.8115779273252,-64.1902001318044,-3.73047319099325));
#39058=CARTESIAN_POINT('Ctrl Pts',(60.0398684103342,-64.7270894912265,-3.61355655310196));
#39059=CARTESIAN_POINT('Ctrl Pts',(62.2587831738394,-64.1526932325171,-3.49663991521067));
#39060=CARTESIAN_POINT('Ctrl Pts',(63.9466897379277,-62.6020431323234,-3.37972327731938));
#39061=CARTESIAN_POINT('Ctrl Pts',(64.7067589021557,-60.4396851780671,-3.26280663942809));
#39062=CARTESIAN_POINT('Ctrl Pts',(64.3603527964105,-58.1739547786936,-3.1458900015368));
#39063=CARTESIAN_POINT('Ctrl Pts',(62.9888106452508,-56.3375258480311,-3.02897336364551));
#39064=CARTESIAN_POINT('Ctrl Pts',(60.9147861958681,-55.3620756793649,-2.91205672575422));
#39065=CARTESIAN_POINT('Ctrl Pts',(58.6254260925902,-55.4770606993678,-2.79514008786293));
#39066=CARTESIAN_POINT('Ctrl Pts',(57.3152159330397,-56.2625729903977,-2.71719566260207));
#39067=CARTESIAN_POINT('Ctrl Pts',(56.7906223161641,-56.7864924158161,-2.67822344997164));
#39068=CARTESIAN_POINT('Ctrl Pts',(56.3552346071769,-56.845432093658,-10.3217765500284));
#39069=CARTESIAN_POINT('Ctrl Pts',(55.8402626818537,-57.44042700498,-10.2828043373979));
#39070=CARTESIAN_POINT('Ctrl Pts',(55.1077769251007,-58.8869088019546,-10.2048599121371));
#39071=CARTESIAN_POINT('Ctrl Pts',(55.1592135800111,-61.3192580543611,-10.0879432742458));
#39072=CARTESIAN_POINT('Ctrl Pts',(56.3487613957467,-63.4411600386716,-9.97102663635449));
#39073=CARTESIAN_POINT('Ctrl Pts',(58.3966566051718,-64.7542485689073,-9.85410999846319));
#39074=CARTESIAN_POINT('Ctrl Pts',(60.8214946863959,-64.9495952878756,-9.73719336057191));
#39075=CARTESIAN_POINT('Ctrl Pts',(63.0532030984208,-63.9813810008584,-9.62027672268061));
#39076=CARTESIAN_POINT('Ctrl Pts',(64.5671400725337,-62.0771726636675,-9.50336008478933));
#39077=CARTESIAN_POINT('Ctrl Pts',(65.0073917579124,-59.6846512635963,-9.38644344689803));
#39078=CARTESIAN_POINT('Ctrl Pts',(64.2704616679068,-57.3662615249434,-9.26952680900675));
#39079=CARTESIAN_POINT('Ctrl Pts',(62.5295930557572,-55.6670360932137,-9.15261017111546));
#39080=CARTESIAN_POINT('Ctrl Pts',(60.1940452488756,-54.9864417739754,-9.03569353322417));
#39081=CARTESIAN_POINT('Ctrl Pts',(57.8128794943531,-55.4844798391586,-8.91877689533288));
#39082=CARTESIAN_POINT('Ctrl Pts',(55.9458815828121,-57.044066491683,-8.80186025744159));
#39083=CARTESIAN_POINT('Ctrl Pts',(55.0319620081071,-59.2985605684372,-8.6849436195503));
#39084=CARTESIAN_POINT('Ctrl Pts',(55.2859731712037,-61.7179550108046,-8.56802698165902));
#39085=CARTESIAN_POINT('Ctrl Pts',(56.6481998303419,-63.7334777965986,-8.45111034376772));
#39086=CARTESIAN_POINT('Ctrl Pts',(58.7983976307144,-64.8713001387427,-8.33419370587643));
#39087=CARTESIAN_POINT('Ctrl Pts',(61.2310787751313,-64.863936227115,-8.21727706798515));
#39088=CARTESIAN_POINT('Ctrl Pts',(63.374347077542,-63.7131094277124,-8.10036043009385));
#39089=CARTESIAN_POINT('Ctrl Pts',(64.7243434252448,-61.6893832296763,-7.98344379220257));
#39090=CARTESIAN_POINT('Ctrl Pts',(64.9636996279981,-59.2684768765872,-7.86652715431127));
#39091=CARTESIAN_POINT('Ctrl Pts',(64.0361435251531,-57.0195971937526,-7.74961051641999));
#39092=CARTESIAN_POINT('Ctrl Pts',(62.1597379643106,-55.4712613106602,-7.6326938785287));
#39093=CARTESIAN_POINT('Ctrl Pts',(59.7755950080574,-54.9878320332931,-7.5157772406374));
#39094=CARTESIAN_POINT('Ctrl Pts',(57.4442220551071,-55.6821677205805,-7.39886060274612));
#39095=CARTESIAN_POINT('Ctrl Pts',(55.7136518610009,-57.3927451067379,-7.28194396485483));
#39096=CARTESIAN_POINT('Ctrl Pts',(54.9908234927723,-59.7137423568676,-7.16502732696353));
#39097=CARTESIAN_POINT('Ctrl Pts',(55.4454445385458,-62.1074830642397,-7.04811068907225));
#39098=CARTESIAN_POINT('Ctrl Pts',(56.9710946830675,-63.9940817395243,-6.93119405118096));
#39099=CARTESIAN_POINT('Ctrl Pts',(59.9539539631079,-65.2913905160755,-6.77530520065924));
#39100=CARTESIAN_POINT('Ctrl Pts',(64.1406165000123,-63.8687885246491,-6.58044413750709));
#39101=CARTESIAN_POINT('Ctrl Pts',(65.5156180778851,-58.6999281298572,-6.34661086172451));
#39102=CARTESIAN_POINT('Ctrl Pts',(62.5891828005711,-55.3851255427309,-6.15174979857236));
#39103=CARTESIAN_POINT('Ctrl Pts',(59.355989914448,-55.0288625677164,-5.99586094805064));
#39104=CARTESIAN_POINT('Ctrl Pts',(57.0945965090759,-55.9080455925754,-5.87894431015935));
#39105=CARTESIAN_POINT('Ctrl Pts',(55.5106832521958,-57.7595027657436,-5.76202767226806));
#39106=CARTESIAN_POINT('Ctrl Pts',(54.9847329820121,-60.1328728166025,-5.64511103437677));
#39107=CARTESIAN_POINT('Ctrl Pts',(55.6366256234011,-62.4772243633749,-5.52819439648548));
#39108=CARTESIAN_POINT('Ctrl Pts',(57.3148511228692,-64.2381789526224,-5.41127775859419));
#39109=CARTESIAN_POINT('Ctrl Pts',(59.6240698767575,-65.0032608100402,-5.2943611207029));
#39110=CARTESIAN_POINT('Ctrl Pts',(62.0217839996138,-64.5919108116637,-5.17744448281161));
#39111=CARTESIAN_POINT('Ctrl Pts',(63.9441442752001,-63.1011555930607,-5.06052784492032));
#39112=CARTESIAN_POINT('Ctrl Pts',(64.9393052902734,-60.8813057068506,-4.94361120702903));
#39113=CARTESIAN_POINT('Ctrl Pts',(64.773278560353,-58.4542925242534,-4.82669456913774));
#39114=CARTESIAN_POINT('Ctrl Pts',(63.4851123401503,-56.3906479031218,-4.70977793124645));
#39115=CARTESIAN_POINT('Ctrl Pts',(61.3776322670752,-55.1755267000177,-4.59286129335516));
#39116=CARTESIAN_POINT('Ctrl Pts',(58.9462872844852,-55.0945835715325,-4.47594465546388));
#39117=CARTESIAN_POINT('Ctrl Pts',(56.7626579210171,-56.1668505486894,-4.35902801757258));
#39118=CARTESIAN_POINT('Ctrl Pts',(55.3400921568247,-58.1402480364103,-4.2421113796813));
#39119=CARTESIAN_POINT('Ctrl Pts',(55.0130188642902,-60.5508528732823,-4.12519474179001));
#39120=CARTESIAN_POINT('Ctrl Pts',(55.858330000942,-62.8319581176111,-4.00827810389872));
#39121=CARTESIAN_POINT('Ctrl Pts',(57.6773011674899,-64.4473015857632,-3.89136146600743));
#39122=CARTESIAN_POINT('Ctrl Pts',(60.0423146482087,-65.0171332941376,-3.77444482811614));
#39123=CARTESIAN_POINT('Ctrl Pts',(62.3973771359187,-64.4074933457197,-3.65752819022485));
#39124=CARTESIAN_POINT('Ctrl Pts',(64.1888499302879,-62.7616987696534,-3.54061155233356));
#39125=CARTESIAN_POINT('Ctrl Pts',(64.9955552648861,-60.4666632924791,-3.42369491444227));
#39126=CARTESIAN_POINT('Ctrl Pts',(64.6278944432215,-58.0619126645643,-3.30677827655098));
#39127=CARTESIAN_POINT('Ctrl Pts',(63.1721974855759,-56.1128044982296,-3.18986163865969));
#39128=CARTESIAN_POINT('Ctrl Pts',(60.9709154626384,-55.0775028549942,-3.0729450007684));
#39129=CARTESIAN_POINT('Ctrl Pts',(58.5410852642163,-55.1995431026464,-2.95602836287711));
#39130=CARTESIAN_POINT('Ctrl Pts',(57.1504834941422,-56.0332526982856,-2.87808393761625));
#39131=CARTESIAN_POINT('Ctrl Pts',(56.5937019680036,-56.5893186660636,-2.83911172498582));
#39132=CARTESIAN_POINT('Ctrl Pts',(56.1445283027442,-56.6630644309996,-10.4826648250425));
#39133=CARTESIAN_POINT('Ctrl Pts',(55.5997855089079,-57.2924563927238,-10.4436926124121));
#39134=CARTESIAN_POINT('Ctrl Pts',(54.8249542647996,-58.8225602616346,-10.3657481871512));
#39135=CARTESIAN_POINT('Ctrl Pts',(54.8793645068411,-61.3955252373669,-10.24883154926));
#39136=CARTESIAN_POINT('Ctrl Pts',(56.1376808706685,-63.6400957825572,-10.1319149113687));
#39137=CARTESIAN_POINT('Ctrl Pts',(58.3039662602388,-65.0290948315175,-10.0149982734774));
#39138=CARTESIAN_POINT('Ctrl Pts',(60.8689858390013,-65.2357346738561,-9.89808163558608));
#39139=CARTESIAN_POINT('Ctrl Pts',(63.2297107943118,-64.2115472768226,-9.78116499769479));
#39140=CARTESIAN_POINT('Ctrl Pts',(64.8311694688852,-62.1972553928581,-9.6642483598035));
#39141=CARTESIAN_POINT('Ctrl Pts',(65.2968723961542,-59.6664207440172,-9.54733172191222));
#39142=CARTESIAN_POINT('Ctrl Pts',(64.5173398889406,-57.2140033571025,-9.43041508402093));
#39143=CARTESIAN_POINT('Ctrl Pts',(62.675830507843,-55.416544576301,-9.31349844612964));
#39144=CARTESIAN_POINT('Ctrl Pts',(60.2052631333967,-54.6966046481226,-9.19658180823834));
#39145=CARTESIAN_POINT('Ctrl Pts',(57.6864406075043,-55.2234346241344,-9.07966517034706));
#39146=CARTESIAN_POINT('Ctrl Pts',(55.7115103085732,-56.8731820153015,-8.96274853245577));
#39147=CARTESIAN_POINT('Ctrl Pts',(54.7447564371768,-59.2580098897298,-8.84583189456448));
#39148=CARTESIAN_POINT('Ctrl Pts',(55.0134521540628,-61.8172711292634,-8.72891525667319));
#39149=CARTESIAN_POINT('Ctrl Pts',(56.4544300397442,-63.9493126239243,-8.6119986187819));
#39150=CARTESIAN_POINT('Ctrl Pts',(58.7289322008878,-65.1529132302293,-8.4950819808906));
#39151=CARTESIAN_POINT('Ctrl Pts',(61.3022482555275,-65.145123605987,-8.37816534299932));
#39152=CARTESIAN_POINT('Ctrl Pts',(63.5694203198369,-63.9277667461252,-8.26124870510802));
#39153=CARTESIAN_POINT('Ctrl Pts',(64.9974608516679,-61.7870475945203,-8.14433206721675));
#39154=CARTESIAN_POINT('Ctrl Pts',(65.2506543952345,-59.2261870397036,-8.02741542932544));
#39155=CARTESIAN_POINT('Ctrl Pts',(64.2694756589632,-56.8472981310306,-7.91049879143416));
#39156=CARTESIAN_POINT('Ctrl Pts',(62.2845938482857,-55.2094519237375,-7.79358215354287));
#39157=CARTESIAN_POINT('Ctrl Pts',(59.7626220066562,-54.6980752792535,-7.67666551565158));
#39158=CARTESIAN_POINT('Ctrl Pts',(57.2964708372155,-55.4325509730806,-7.55974887776029));
#39159=CARTESIAN_POINT('Ctrl Pts',(55.4658552325379,-57.2420179723235,-7.442832239869));
#39160=CARTESIAN_POINT('Ctrl Pts',(54.701239676989,-59.6971936126827,-7.32591560197771));
#39161=CARTESIAN_POINT('Ctrl Pts',(55.1821426669066,-62.2293180577881,-7.20899896408642));
#39162=CARTESIAN_POINT('Ctrl Pts',(56.7959916580377,-64.2249822536134,-7.09208232619513));
#39163=CARTESIAN_POINT('Ctrl Pts',(59.9512920111792,-65.5972893108641,-6.93619347567341));
#39164=CARTESIAN_POINT('Ctrl Pts',(64.3799882857817,-64.0924457548965,-6.74133241252127));
#39165=CARTESIAN_POINT('Ctrl Pts',(65.8344796167214,-58.6247701128846,-6.50749913673868));
#39166=CARTESIAN_POINT('Ctrl Pts',(62.7388651753224,-55.1183365899423,-6.31263807358654));
#39167=CARTESIAN_POINT('Ctrl Pts',(59.3187592643186,-54.7414778160817,-6.15674922306481));
#39168=CARTESIAN_POINT('Ctrl Pts',(56.9266332065095,-55.6714869946495,-6.03983258517353));
#39169=CARTESIAN_POINT('Ctrl Pts',(55.2511528738565,-57.6299781348164,-5.92291594728223));
#39170=CARTESIAN_POINT('Ctrl Pts',(54.6947970697628,-60.1405542822466,-5.80599930939095));
#39171=CARTESIAN_POINT('Ctrl Pts',(55.3843760570615,-62.6204343466251,-5.68908267149966));
#39172=CARTESIAN_POINT('Ctrl Pts',(57.159620885591,-64.483190888477,-5.57216603360837));
#39173=CARTESIAN_POINT('Ctrl Pts',(59.6023371070298,-65.292502635446,-5.45524939571708));
#39174=CARTESIAN_POINT('Ctrl Pts',(62.1386646734039,-64.8573722208712,-5.33833275782579));
#39175=CARTESIAN_POINT('Ctrl Pts',(64.1721578713598,-63.2804354544672,-5.2214161199345));
#39176=CARTESIAN_POINT('Ctrl Pts',(65.2248498046685,-60.9322545742129,-5.10449948204321));
#39177=CARTESIAN_POINT('Ctrl Pts',(65.0492249593888,-58.3649341500245,-4.98758284415192));
#39178=CARTESIAN_POINT('Ctrl Pts',(63.6865889957319,-56.1819888648126,-4.87066620626063));
#39179=CARTESIAN_POINT('Ctrl Pts',(61.4572741020296,-54.8966206991336,-4.75374956836934));
#39180=CARTESIAN_POINT('Ctrl Pts',(58.885371453618,-54.8109981947122,-4.63683293047805));
#39181=CARTESIAN_POINT('Ctrl Pts',(56.5755050285457,-55.9452536369063,-4.51991629258676));
#39182=CARTESIAN_POINT('Ctrl Pts',(55.0706997941323,-58.0327345420765,-4.40299965469547));
#39183=CARTESIAN_POINT('Ctrl Pts',(54.7247181776535,-60.582698043192,-4.28608301680418));
#39184=CARTESIAN_POINT('Ctrl Pts',(55.6188973116942,-62.9956754944399,-4.16916637891289));
#39185=CARTESIAN_POINT('Ctrl Pts',(57.5430244076546,-64.704403039722,-4.0522497410216));
#39186=CARTESIAN_POINT('Ctrl Pts',(60.0447608860831,-65.3071770970488,-3.93533310313031));
#39187=CARTESIAN_POINT('Ctrl Pts',(62.5359710979979,-64.6622934589222,-3.81841646523902));
#39188=CARTESIAN_POINT('Ctrl Pts',(64.4310101226481,-62.9213544069835,-3.70149982734774));
#39189=CARTESIAN_POINT('Ctrl Pts',(65.2843516276165,-60.4936414068911,-3.58458318945645));
#39190=CARTESIAN_POINT('Ctrl Pts',(64.8954360900324,-57.949870550435,-3.46766655156515));
#39191=CARTESIAN_POINT('Ctrl Pts',(63.355584325901,-55.888083148428,-3.35074991367387));
#39192=CARTESIAN_POINT('Ctrl Pts',(61.0270447294087,-54.7929300306235,-3.23383327578258));
#39193=CARTESIAN_POINT('Ctrl Pts',(58.4567444358424,-54.9220255059251,-3.11691663789129));
#39194=CARTESIAN_POINT('Ctrl Pts',(56.9857510552447,-55.8039324061735,-3.03897221263043));
#39195=CARTESIAN_POINT('Ctrl Pts',(56.3967816198431,-56.3921449163111,-3.));
#39196=CARTESIAN_POINT('Ctrl Pts',(56.7766472160421,-57.2101674189746,-10.));
#39197=CARTESIAN_POINT('Ctrl Pts',(56.6836917113314,-57.2986365151465,-10.));
#39198=CARTESIAN_POINT('Ctrl Pts',(56.5950268358409,-57.39120230356,-10.));
#39199=CARTESIAN_POINT('Ctrl Pts',(56.5107709219868,-57.4874461178782,-10.));
#39200=CARTESIAN_POINT('Ctrl Pts',(56.4249560467001,-57.5854707020888,-10.));
#39201=CARTESIAN_POINT('Ctrl Pts',(56.3437142744234,-57.68731109176,-10.));
#39202=CARTESIAN_POINT('Ctrl Pts',(56.2671935602913,-57.792573893156,-10.));
#39203=CARTESIAN_POINT('Ctrl Pts',(56.1895733429177,-57.899349184244,-10.));
#39204=CARTESIAN_POINT('Ctrl Pts',(56.1168102542361,-58.00964645597,-10.));
#39205=CARTESIAN_POINT('Ctrl Pts',(56.049090461305,-58.1230979076824,-10.));
#39206=CARTESIAN_POINT('Ctrl Pts',(55.9815185974621,-58.2363015327393,-10.));
#39207=CARTESIAN_POINT('Ctrl Pts',(55.9189675098551,-58.3526462165835,-10.));
#39208=CARTESIAN_POINT('Ctrl Pts',(55.8616615643608,-58.4717999961111,-10.));
#39209=CARTESIAN_POINT('Ctrl Pts',(55.8501070017569,-58.4958248995163,-10.));
#39210=CARTESIAN_POINT('Ctrl Pts',(55.8387658201931,-58.5199640956874,-10.));
#39211=CARTESIAN_POINT('Ctrl Pts',(55.8276400825626,-58.5442149922488,-10.));
#39212=CARTESIAN_POINT('Ctrl Pts',(55.8174346017263,-58.5664599946337,-10.));
#39213=CARTESIAN_POINT('Ctrl Pts',(55.8074085198422,-58.5888034819082,-10.));
#39214=CARTESIAN_POINT('Ctrl Pts',(55.7975753646996,-58.6112157671766,-10.));
#39215=CARTESIAN_POINT('Ctrl Pts',(55.7403628737432,-58.7416177235827,-10.));
#39216=CARTESIAN_POINT('Ctrl Pts',(55.6896032280292,-58.8745016319323,-10.));
#39217=CARTESIAN_POINT('Ctrl Pts',(55.645480033527,-59.0093932220121,-10.));
#39218=CARTESIAN_POINT('Ctrl Pts',(55.6039769196502,-59.1362748108742,-10.));
#39219=CARTESIAN_POINT('Ctrl Pts',(55.5683449606977,-59.2649336678103,-10.));
#39220=CARTESIAN_POINT('Ctrl Pts',(55.5385237883193,-59.394948029667,-10.));
#39221=CARTESIAN_POINT('Ctrl Pts',(55.5083231158982,-59.5266169359948,-10.));
#39222=CARTESIAN_POINT('Ctrl Pts',(55.4840818234416,-59.6596767600327,-10.));
#39223=CARTESIAN_POINT('Ctrl Pts',(55.4657842264052,-59.7937146570425,-10.));
#39224=CARTESIAN_POINT('Ctrl Pts',(55.4495747295253,-59.9124563076013,-10.));
#39225=CARTESIAN_POINT('Ctrl Pts',(55.4380303521448,-60.0319662479349,-10.));
#39226=CARTESIAN_POINT('Ctrl Pts',(55.4311726380116,-60.1519668352251,-10.));
#39227=CARTESIAN_POINT('Ctrl Pts',(55.429455990605,-60.1820058092848,-10.));
#39228=CARTESIAN_POINT('Ctrl Pts',(55.4280331714048,-60.2120755524062,-10.));
#39229=CARTESIAN_POINT('Ctrl Pts',(55.4269048277578,-60.2421717447487,-10.));
#39230=CARTESIAN_POINT('Ctrl Pts',(55.4260974676989,-60.2637063753445,-10.));
#39231=CARTESIAN_POINT('Ctrl Pts',(55.4254409115147,-60.2852562780381,-10.));
#39232=CARTESIAN_POINT('Ctrl Pts',(55.4249357122242,-60.3067982825129,-10.));
#39233=CARTESIAN_POINT('Ctrl Pts',(55.4216904579502,-60.4451778950763,-10.));
#39234=CARTESIAN_POINT('Ctrl Pts',(55.4246782307337,-60.5834276345437,-10.));
#39235=CARTESIAN_POINT('Ctrl Pts',(55.4338329237967,-60.7211067790156,-10.));
#39236=CARTESIAN_POINT('Ctrl Pts',(55.4430905973063,-60.8603346657192,-10.));
#39237=CARTESIAN_POINT('Ctrl Pts',(55.4586544983472,-60.9989798220631,-10.));
#39238=CARTESIAN_POINT('Ctrl Pts',(55.4805057616638,-61.1366049558711,-10.));
#39239=CARTESIAN_POINT('Ctrl Pts',(55.4853225147871,-61.1669421626271,-10.));
#39240=CARTESIAN_POINT('Ctrl Pts',(55.4904449729792,-61.1972298498434,-10.));
#39241=CARTESIAN_POINT('Ctrl Pts',(55.4958732691136,-61.2274633933805,-10.));
#39242=CARTESIAN_POINT('Ctrl Pts',(55.5203481559226,-61.3637791981151,-10.));
#39243=CARTESIAN_POINT('Ctrl Pts',(55.5510361995063,-61.498994490849,-10.));
#39244=CARTESIAN_POINT('Ctrl Pts',(55.5877252702061,-61.6327571121263,-10.));
#39245=CARTESIAN_POINT('Ctrl Pts',(55.6089637062398,-61.7101891326575,-10.));
#39246=CARTESIAN_POINT('Ctrl Pts',(55.6322140625153,-61.7871343566708,-10.));
#39247=CARTESIAN_POINT('Ctrl Pts',(55.6574430485543,-61.8635234044139,-10.));
#39248=CARTESIAN_POINT('Ctrl Pts',(55.6711730738632,-61.9050955689553,-10.));
#39249=CARTESIAN_POINT('Ctrl Pts',(55.6854892106993,-61.9465029895356,-10.));
#39250=CARTESIAN_POINT('Ctrl Pts',(55.7003867816747,-61.9877342895387,-10.));
#39251=CARTESIAN_POINT('Ctrl Pts',(55.7064544836587,-62.0045275802867,-10.));
#39252=CARTESIAN_POINT('Ctrl Pts',(55.712618644672,-62.0212916526985,-10.));
#39253=CARTESIAN_POINT('Ctrl Pts',(55.7188789712335,-62.0380257298289,-10.));
#39254=CARTESIAN_POINT('Ctrl Pts',(55.7254264995218,-62.0555275074623,-10.));
#39255=CARTESIAN_POINT('Ctrl Pts',(55.7320759827005,-62.072987796165,-10.));
#39256=CARTESIAN_POINT('Ctrl Pts',(55.7388258750028,-62.090403524095,-10.));
#39257=CARTESIAN_POINT('Ctrl Pts',(55.7901008202184,-62.2227005231443,-10.));
#39258=CARTESIAN_POINT('Ctrl Pts',(55.8471813600148,-62.3524682290589,-10.));
#39259=CARTESIAN_POINT('Ctrl Pts',(55.9097891939914,-62.4793487633564,-10.));
#39260=CARTESIAN_POINT('Ctrl Pts',(55.9730108621089,-62.6074732890015,-10.));
#39261=CARTESIAN_POINT('Ctrl Pts',(56.0418689163077,-62.7326544978742,-10.));
#39262=CARTESIAN_POINT('Ctrl Pts',(56.1161301190731,-62.8545209455919,-10.));
#39263=CARTESIAN_POINT('Ctrl Pts',(56.1904609269085,-62.9765016188041,-10.));
#39264=CARTESIAN_POINT('Ctrl Pts',(56.2702052729959,-63.0951620835971,-10.));
#39265=CARTESIAN_POINT('Ctrl Pts',(56.3551790532359,-63.2101155108968,-10.));
#39266=CARTESIAN_POINT('Ctrl Pts',(56.3877839542042,-63.2542237652606,-10.));
#39267=CARTESIAN_POINT('Ctrl Pts',(56.4211592843168,-63.2977860220108,-10.));
#39268=CARTESIAN_POINT('Ctrl Pts',(56.455296464099,-63.3407794968677,-10.));
#39269=CARTESIAN_POINT('Ctrl Pts',(56.5184577271862,-63.4203268465255,-10.));
#39270=CARTESIAN_POINT('Ctrl Pts',(56.5842264360496,-63.4979275884953,-10.));
#39271=CARTESIAN_POINT('Ctrl Pts',(56.6524865899918,-63.5734972061251,-10.));
#39272=CARTESIAN_POINT('Ctrl Pts',(56.6665323550258,-63.5890470259194,-10.));
#39273=CARTESIAN_POINT('Ctrl Pts',(56.6806836439788,-63.6045108180711,-10.));
#39274=CARTESIAN_POINT('Ctrl Pts',(56.6949394989269,-63.619887800082,-10.));
#39275=CARTESIAN_POINT('Ctrl Pts',(56.7093516420952,-63.6354333613299,-10.));
#39276=CARTESIAN_POINT('Ctrl Pts',(56.7238639886949,-63.6508829927511,-10.));
#39277=CARTESIAN_POINT('Ctrl Pts',(56.7384737638415,-63.6662345726912,-10.));
#39278=CARTESIAN_POINT('Ctrl Pts',(56.8381048611188,-63.7709243943361,-10.));
#39279=CARTESIAN_POINT('Ctrl Pts',(56.9422847936492,-63.8710796498495,-10.));
#39280=CARTESIAN_POINT('Ctrl Pts',(57.0506144927706,-63.9665038599407,-10.));
#39281=CARTESIAN_POINT('Ctrl Pts',(57.1492676399244,-64.0534043010616,-10.));
#39282=CARTESIAN_POINT('Ctrl Pts',(57.2513632043421,-64.1363811929212,-10.));
#39283=CARTESIAN_POINT('Ctrl Pts',(57.3566308873088,-64.2152666810068,-10.));
#39284=CARTESIAN_POINT('Ctrl Pts',(57.4121395415194,-64.2568637519878,-10.));
#39285=CARTESIAN_POINT('Ctrl Pts',(57.4685306830645,-64.2973228450431,-10.));
#39286=CARTESIAN_POINT('Ctrl Pts',(57.5257674980437,-64.336616799743,-10.));
#39287=CARTESIAN_POINT('Ctrl Pts',(57.547470637647,-64.3515163392217,-10.));
#39288=CARTESIAN_POINT('Ctrl Pts',(57.5692953852945,-64.3662483371277,-10.));
#39289=CARTESIAN_POINT('Ctrl Pts',(57.5912397986742,-64.3808112384959,-10.));
#39290=CARTESIAN_POINT('Ctrl Pts',(57.6130039806025,-64.3952545334383,-10.));
#39291=CARTESIAN_POINT('Ctrl Pts',(57.6348798559218,-64.4095274598417,-10.));
#39292=CARTESIAN_POINT('Ctrl Pts',(57.6568590278616,-64.4236248088739,-10.));
#39293=CARTESIAN_POINT('Ctrl Pts',(57.7821905968559,-64.5040119534721,-10.));
#39294=CARTESIAN_POINT('Ctrl Pts',(57.9109399451369,-64.5787341115543,-10.));
#39295=CARTESIAN_POINT('Ctrl Pts',(58.0427132801631,-64.6475637443441,-10.));
#39296=CARTESIAN_POINT('Ctrl Pts',(58.1526798139151,-64.7050029533904,-10.));
#39297=CARTESIAN_POINT('Ctrl Pts',(58.2647532533075,-64.7583381770103,-10.));
#39298=CARTESIAN_POINT('Ctrl Pts',(58.3787241365729,-64.8074172934041,-10.));
#39299=CARTESIAN_POINT('Ctrl Pts',(58.4767840475646,-64.8496446908518,-10.));
#39300=CARTESIAN_POINT('Ctrl Pts',(58.5762489646464,-64.8887211766839,-10.));
#39301=CARTESIAN_POINT('Ctrl Pts',(58.6769607093948,-64.9246350255102,-10.));
#39302=CARTESIAN_POINT('Ctrl Pts',(64.2628730310814,-59.999902186829,-7.57968167058906));
#39303=CARTESIAN_POINT('Ctrl Pts',(64.2624542707466,-60.4879393559667,-7.60701019445077));
#39304=CARTESIAN_POINT('Ctrl Pts',(64.1786779858871,-60.9761189685309,-7.63433871831249));
#39305=CARTESIAN_POINT('Ctrl Pts',(64.0144041626786,-61.4355115568657,-7.6616672421742));
#39306=CARTESIAN_POINT('Ctrl Pts',(63.7801392459165,-62.0906345969544,-7.70063945480464));
#39307=CARTESIAN_POINT('Ctrl Pts',(63.3821699194345,-62.6872146939206,-7.73961166743506));
#39308=CARTESIAN_POINT('Ctrl Pts',(62.8672751264245,-63.1551325221511,-7.77858388006549));
#39309=CARTESIAN_POINT('Ctrl Pts',(62.3523803334146,-63.6230503503815,-7.81755609269592));
#39310=CARTESIAN_POINT('Ctrl Pts',(61.7205600738767,-63.9623059098762,-7.85652830532635));
#39311=CARTESIAN_POINT('Ctrl Pts',(61.0460813901126,-64.1330191040233,-7.89550051795678));
#39312=CARTESIAN_POINT('Ctrl Pts',(60.3716027063484,-64.3037322981704,-7.93447273058721));
#39313=CARTESIAN_POINT('Ctrl Pts',(59.654465598358,-64.3059031269698,-7.97344494321764));
#39314=CARTESIAN_POINT('Ctrl Pts',(58.9789655312245,-64.1392775723992,-8.01241715584807));
#39315=CARTESIAN_POINT('Ctrl Pts',(58.3034654640909,-63.9726520178286,-8.0513893684785));
#39316=CARTESIAN_POINT('Ctrl Pts',(57.6696024378142,-63.637230079888,-8.09036158110893));
#39317=CARTESIAN_POINT('Ctrl Pts',(57.1518835570005,-63.1724382162409,-8.12933379373936));
#39318=CARTESIAN_POINT('Ctrl Pts',(56.6341646761868,-62.7076463525939,-8.16830600636979));
#39319=CARTESIAN_POINT('Ctrl Pts',(56.2325899408361,-62.1134845632405,-8.20727821900022));
#39320=CARTESIAN_POINT('Ctrl Pts',(55.9943622305744,-61.4597935272245,-8.24625043163065));
#39321=CARTESIAN_POINT('Ctrl Pts',(55.7561345203128,-60.8061024912086,-8.28522264426108));
#39322=CARTESIAN_POINT('Ctrl Pts',(55.6812538351402,-60.0928822085302,-8.32419485689151));
#39323=CARTESIAN_POINT('Ctrl Pts',(55.7785219894409,-59.4039676536234,-8.36316706952194));
#39324=CARTESIAN_POINT('Ctrl Pts',(55.8757901437417,-58.7150530987165,-8.40213928215237));
#39325=CARTESIAN_POINT('Ctrl Pts',(56.1452071375158,-58.0504442715813,-8.4411114947828));
#39326=CARTESIAN_POINT('Ctrl Pts',(56.5551044905297,-57.4882623288071,-8.48008370741323));
#39327=CARTESIAN_POINT('Ctrl Pts',(56.9650018435436,-56.9260803860329,-8.51905592004366));
#39328=CARTESIAN_POINT('Ctrl Pts',(57.5153795557971,-56.4663253276198,-8.55802813267409));
#39329=CARTESIAN_POINT('Ctrl Pts',(58.1415437805544,-56.1630387578257,-8.59700034530452));
#39330=CARTESIAN_POINT('Ctrl Pts',(58.7677080053116,-55.8597521880315,-8.63597255793495));
#39331=CARTESIAN_POINT('Ctrl Pts',(59.4696587425724,-55.7129341068562,-8.67494477056538));
#39332=CARTESIAN_POINT('Ctrl Pts',(60.1648855564949,-55.7398422498282,-8.71391698319581));
#39333=CARTESIAN_POINT('Ctrl Pts',(60.8601123704174,-55.7667503928002,-8.75288919582624));
#39334=CARTESIAN_POINT('Ctrl Pts',(61.5486152610015,-55.9673847599195,-8.79186140845667));
#39335=CARTESIAN_POINT('Ctrl Pts',(62.1494645520024,-56.3181617324103,-8.8308336210871));
#39336=CARTESIAN_POINT('Ctrl Pts',(62.7503138430034,-56.668938704901,-8.86980583371753));
#39337=CARTESIAN_POINT('Ctrl Pts',(63.2635095344213,-57.1698582827631,-8.90877804634796));
#39338=CARTESIAN_POINT('Ctrl Pts',(63.6287282560618,-57.7620404787157,-8.94775025897839));
#39339=CARTESIAN_POINT('Ctrl Pts',(63.9939469777023,-58.3542226746683,-8.98672247160882));
#39340=CARTESIAN_POINT('Ctrl Pts',(64.2111887295655,-59.0376674887114,-9.02569468423925));
#39341=CARTESIAN_POINT('Ctrl Pts',(64.2549180718975,-59.7320390461549,-9.06466689686968));
#39342=CARTESIAN_POINT('Ctrl Pts',(64.2605339208635,-59.8212122553767,-9.0696718214428));
#39343=CARTESIAN_POINT('Ctrl Pts',(64.2632881266013,-59.9105656732725,-9.07467674601593));
#39344=CARTESIAN_POINT('Ctrl Pts',(64.2632129993401,-59.9999237120662,-9.07968167058906));
#39345=CARTESIAN_POINT('Ctrl Pts',(61.322884965569,-64.9244061944433,-10.));
#39346=CARTESIAN_POINT('Ctrl Pts',(62.1267766598728,-64.7084499564018,-9.96102778736957));
#39347=CARTESIAN_POINT('Ctrl Pts',(63.6260271020141,-63.8754856296126,-9.88308336210871));
#39348=CARTESIAN_POINT('Ctrl Pts',(65.0229772435633,-61.7140881496855,-9.76616672421742));
#39349=CARTESIAN_POINT('Ctrl Pts',(65.2388166219534,-59.1499371274841,-9.64925008632613));
#39350=CARTESIAN_POINT('Ctrl Pts',(64.2231822374133,-56.7854927040709,-9.53233344843484));
#39351=CARTESIAN_POINT('Ctrl Pts',(62.2146698199313,-55.1767965300925,-9.41541681054356));
#39352=CARTESIAN_POINT('Ctrl Pts',(59.6855379300098,-54.7019554558395,-9.29850017265226));
#39353=CARTESIAN_POINT('Ctrl Pts',(57.2303209690299,-55.4726378662523,-9.18158353476098));
#39354=CARTESIAN_POINT('Ctrl Pts',(55.4262302424911,-57.3076473811431,-9.06466689686968));
#39355=CARTESIAN_POINT('Ctrl Pts',(54.6973796557714,-59.775601760132,-8.9477502589784));
#39356=CARTESIAN_POINT('Ctrl Pts',(55.2151175549311,-62.2963084797734,-8.8308336210871));
#39357=CARTESIAN_POINT('Ctrl Pts',(56.8577277980376,-64.2771790632985,-8.71391698319582));
#39358=CARTESIAN_POINT('Ctrl Pts',(59.2390517062358,-65.2525319290857,-8.59700034530453));
#39359=CARTESIAN_POINT('Ctrl Pts',(61.7992659861865,-64.9930728587382,-8.48008370741324));
#39360=CARTESIAN_POINT('Ctrl Pts',(63.9364928774652,-63.5597974904555,-8.36316706952195));
#39361=CARTESIAN_POINT('Ctrl Pts',(65.1482937026264,-61.2896533828664,-8.24625043163066));
#39362=CARTESIAN_POINT('Ctrl Pts',(65.1497880187566,-58.7163255770949,-8.12933379373937));
#39363=CARTESIAN_POINT('Ctrl Pts',(63.9406234799139,-56.4447764036095,-8.01241715584808));
#39364=CARTESIAN_POINT('Ctrl Pts',(61.8050635175092,-55.0090188089158,-7.89550051795678));
#39365=CARTESIAN_POINT('Ctrl Pts',(59.2451498180026,-54.7465902155457,-7.7785838800655));
#39366=CARTESIAN_POINT('Ctrl Pts',(56.8627001404056,-55.7191702005741,-7.66166724217421));
#39367=CARTESIAN_POINT('Ctrl Pts',(55.217779590162,-57.6981472392852,-7.54475060428292));
#39368=CARTESIAN_POINT('Ctrl Pts',(54.6971392178688,-60.21821824206,-7.42783396639163));
#39369=CARTESIAN_POINT('Ctrl Pts',(55.4230712207726,-62.6870881580822,-7.31091732850034));
#39370=CARTESIAN_POINT('Ctrl Pts',(57.2251428783372,-64.5240383042407,-7.19400069060906));
#39371=CARTESIAN_POINT('Ctrl Pts',(59.6792195378112,-65.2979014573777,-7.07708405271776));
#39372=CARTESIAN_POINT('Ctrl Pts',(62.2094281655486,-64.8252835759928,-6.96016741482648));
#39373=CARTESIAN_POINT('Ctrl Pts',(64.2186727163164,-63.2204586132884,-6.84325077693518));
#39374=CARTESIAN_POINT('Ctrl Pts',(65.2395163218884,-60.8538584389166,-6.7263341390439));
#39375=CARTESIAN_POINT('Ctrl Pts',(65.0214094514788,-58.2965905321897,-6.6094175011526));
#39376=CARTESIAN_POINT('Ctrl Pts',(63.1773262290866,-55.3916806820179,-6.45352865063089));
#39377=CARTESIAN_POINT('Ctrl Pts',(58.6661395049216,-54.1559238915272,-6.25866758747873));
#39378=CARTESIAN_POINT('Ctrl Pts',(54.3971988313774,-57.8690311013926,-6.02483431169616));
#39379=CARTESIAN_POINT('Ctrl Pts',(54.9957837258839,-62.5079530267534,-5.82997324854401));
#39380=CARTESIAN_POINT('Ctrl Pts',(57.6170694121072,-64.7368553395382,-5.67408439802229));
#39381=CARTESIAN_POINT('Ctrl Pts',(60.1194267752203,-65.3072914717773,-5.557167760131));
#39382=CARTESIAN_POINT('Ctrl Pts',(62.6046736799591,-64.6243084010734,-5.44025112223971));
#39383=CARTESIAN_POINT('Ctrl Pts',(64.4724887605417,-62.8568826882213,-5.32333448434842));
#39384=CARTESIAN_POINT('Ctrl Pts',(65.2912291347546,-60.4165983684538,-5.20641784645713));
#39385=CARTESIAN_POINT('Ctrl Pts',(64.8649669487591,-57.8789504458245,-5.08950120856584));
#39386=CARTESIAN_POINT('Ctrl Pts',(63.2955109178121,-55.8396721751708,-4.97258457067455));
#39387=CARTESIAN_POINT('Ctrl Pts',(60.9510823423798,-54.7785639854422,-4.85566793278326));
#39388=CARTESIAN_POINT('Ctrl Pts',(58.3831733906512,-54.9449006048999,-4.73875129489197));
#39389=CARTESIAN_POINT('Ctrl Pts',(56.1953121953125,-56.2996615164319,-4.62183465700068));
#39390=CARTESIAN_POINT('Ctrl Pts',(54.9019142627768,-58.5243188117934,-4.50491801910939));
#39391=CARTESIAN_POINT('Ctrl Pts',(54.8070090534039,-61.0958980757912,-4.3880013812181));
#39392=CARTESIAN_POINT('Ctrl Pts',(55.932923519751,-63.4098412167327,-4.27108474332681));
#39393=CARTESIAN_POINT('Ctrl Pts',(58.0149603071344,-64.9221696503736,-4.15416810543553));
#39394=CARTESIAN_POINT('Ctrl Pts',(60.5636590522025,-65.2773499477182,-4.03725146754423));
#39395=CARTESIAN_POINT('Ctrl Pts',(62.9798472271926,-64.3918839378294,-3.92033482965295));
#39396=CARTESIAN_POINT('Ctrl Pts',(64.6955066967082,-62.4739345776163,-3.80341819176165));
#39397=CARTESIAN_POINT('Ctrl Pts',(65.3073040903922,-59.9743905230445,-3.68650155387037));
#39398=CARTESIAN_POINT('Ctrl Pts',(64.6714138259177,-57.4808672112921,-3.56958491597907));
#39399=CARTESIAN_POINT('Ctrl Pts',(62.9373243124707,-55.5795635648098,-3.45266827808779));
#39400=CARTESIAN_POINT('Ctrl Pts',(60.5127057471208,-54.7174568009332,-3.3357516401965));
#39401=CARTESIAN_POINT('Ctrl Pts',(57.9675484622588,-55.0972147578633,-3.21883500230521));
#39402=CARTESIAN_POINT('Ctrl Pts',(55.9002136741803,-56.629568839814,-3.10191836441392));
#39403=CARTESIAN_POINT('Ctrl Pts',(54.7966592387799,-58.9542608884761,-2.98500172652263));
#39404=CARTESIAN_POINT('Ctrl Pts',(54.9164249969225,-61.5248185706029,-2.86808508863134));
#39405=CARTESIAN_POINT('Ctrl Pts',(56.2311219369973,-63.7368377969517,-2.75116845074005));
#39406=CARTESIAN_POINT('Ctrl Pts',(58.4321698206392,-65.0704408031689,-2.63425181284876));
#39407=CARTESIAN_POINT('Ctrl Pts',(60.1446943002093,-65.1644693350243,-2.5563073875879));
#39408=CARTESIAN_POINT('Ctrl Pts',(60.9621351249183,-65.0074042178956,-2.51733517495747));
#39409=CARTESIAN_POINT('Ctrl Pts',(61.2505876634042,-64.655281295538,-10.1608882750142));
#39410=CARTESIAN_POINT('Ctrl Pts',(62.0105456807492,-64.4511273334331,-10.1219160623837));
#39411=CARTESIAN_POINT('Ctrl Pts',(63.4278602289486,-63.6636855389833,-10.0439716371229));
#39412=CARTESIAN_POINT('Ctrl Pts',(64.7484653147133,-61.6204111088842,-9.9270549992316));
#39413=CARTESIAN_POINT('Ctrl Pts',(64.9525088036914,-59.1963941165292,-9.81013836134031));
#39414=CARTESIAN_POINT('Ctrl Pts',(63.9923800964395,-56.9611695099411,-9.69322172344902));
#39415=CARTESIAN_POINT('Ctrl Pts',(62.093635370728,-55.4403905747315,-9.57630508555773));
#39416=CARTESIAN_POINT('Ctrl Pts',(59.702723671692,-54.9915001534219,-9.45938844766644));
#39417=CARTESIAN_POINT('Ctrl Pts',(57.3816873591647,-55.7200638153805,-9.34247180977515));
#39418=CARTESIAN_POINT('Ctrl Pts',(55.6761924257478,-57.4547877870635,-9.22555517188386));
#39419=CARTESIAN_POINT('Ctrl Pts',(54.9871744264961,-59.7878654019264,-9.10863853399257));
#39420=CARTESIAN_POINT('Ctrl Pts',(55.4766173080904,-62.1708123766754,-8.99172189610128));
#39421=CARTESIAN_POINT('Ctrl Pts',(57.0294568665373,-64.0434259288984,-8.87480525820999));
#39422=CARTESIAN_POINT('Ctrl Pts',(59.2806384731565,-64.9654745522983,-8.7578886203187));
#39423=CARTESIAN_POINT('Ctrl Pts',(61.7009338711017,-64.7201952415646,-8.64097198242741));
#39424=CARTESIAN_POINT('Ctrl Pts',(63.7213586651647,-63.3652501477072,-8.52405534453613));
#39425=CARTESIAN_POINT('Ctrl Pts',(64.8669330740459,-61.2191722278638,-8.40713870664483));
#39426=CARTESIAN_POINT('Ctrl Pts',(64.8683457239484,-58.7864799745289,-8.29022206875354));
#39427=CARTESIAN_POINT('Ctrl Pts',(63.7252635250725,-56.6390737773809,-8.17330543086226));
#39428=CARTESIAN_POINT('Ctrl Pts',(61.7064145601557,-55.281782113861,-8.05638879297096));
#39429=CARTESIAN_POINT('Ctrl Pts',(59.2864033155609,-55.0336955682165,-7.93947215507968));
#39430=CARTESIAN_POINT('Ctrl Pts',(57.0341574642351,-55.9531228522261,-7.82255551718839));
#39431=CARTESIAN_POINT('Ctrl Pts',(55.4791338597982,-57.823946344205,-7.7056388792971));
#39432=CARTESIAN_POINT('Ctrl Pts',(54.9869471288226,-60.2062923448016,-7.58872224140581));
#39433=CARTESIAN_POINT('Ctrl Pts',(55.6732060484796,-62.5402354614648,-7.47180560351452));
#39434=CARTESIAN_POINT('Ctrl Pts',(57.3767922575429,-64.2767940065127,-7.35488896562323));
#39435=CARTESIAN_POINT('Ctrl Pts',(59.6967505874543,-65.0083645796653,-7.23797232773194));
#39436=CARTESIAN_POINT('Ctrl Pts',(62.0886801792508,-64.5615758509794,-7.12105568984065));
#39437=CARTESIAN_POINT('Ctrl Pts',(63.9881170262568,-63.044456560552,-7.00413905194936));
#39438=CARTESIAN_POINT('Ctrl Pts',(64.9531702641583,-60.8071940174658,-6.88722241405807));
#39439=CARTESIAN_POINT('Ctrl Pts',(64.7469832044083,-58.3896839697977,-6.77030577616678));
#39440=CARTESIAN_POINT('Ctrl Pts',(63.0036814145795,-55.6435310415546,-6.61441692564505));
#39441=CARTESIAN_POINT('Ctrl Pts',(58.7390366333706,-54.4753098905259,-6.41955586249292));
#39442=CARTESIAN_POINT('Ctrl Pts',(54.7033988560207,-57.9854911915564,-6.18572258671033));
#39443=CARTESIAN_POINT('Ctrl Pts',(55.2692703445124,-62.3708902869766,-5.99086152355819));
#39444=CARTESIAN_POINT('Ctrl Pts',(57.7472995207219,-64.4779803271924,-5.83497267303646));
#39445=CARTESIAN_POINT('Ctrl Pts',(60.112899954008,-65.0172414181455,-5.71805603514517));
#39446=CARTESIAN_POINT('Ctrl Pts',(62.4623250366666,-64.3715842183384,-5.60113939725388));
#39447=CARTESIAN_POINT('Ctrl Pts',(64.2280617092367,-62.7007505101895,-5.4842227593626));
#39448=CARTESIAN_POINT('Ctrl Pts',(65.0020569077392,-60.3938307515336,-5.3673061214713));
#39449=CARTESIAN_POINT('Ctrl Pts',(64.5990904782641,-57.994868431527,-5.25038948358002));
#39450=CARTESIAN_POINT('Ctrl Pts',(63.1154071636583,-56.0670392446326,-5.13347284568872));
#39451=CARTESIAN_POINT('Ctrl Pts',(60.8991045141632,-55.0639219319788,-5.01655620779744));
#39452=CARTESIAN_POINT('Ctrl Pts',(58.471534967785,-55.2211680491245,-4.89963956990615));
#39453=CARTESIAN_POINT('Ctrl Pts',(56.4032430971049,-56.5018895985567,-4.78272293201486));
#39454=CARTESIAN_POINT('Ctrl Pts',(55.1805309638501,-58.6049666168101,-4.66580629412357));
#39455=CARTESIAN_POINT('Ctrl Pts',(55.0908124417384,-61.0360058883453,-4.54888965623228));
#39456=CARTESIAN_POINT('Ctrl Pts',(56.1551942877113,-63.2234891701099,-4.43197301834099));
#39457=CARTESIAN_POINT('Ctrl Pts',(58.1234451854266,-64.6531669813724,-4.3150563804497));
#39458=CARTESIAN_POINT('Ctrl Pts',(60.532854386736,-64.9889362354679,-4.19813974255841));
#39459=CARTESIAN_POINT('Ctrl Pts',(62.8169948847769,-64.1518620399393,-4.08122310466712));
#39460=CARTESIAN_POINT('Ctrl Pts',(64.4388914389159,-62.338730988227,-3.96430646677583));
#39461=CARTESIAN_POINT('Ctrl Pts',(65.0172533471374,-59.9757901126853,-3.84738982888454));
#39462=CARTESIAN_POINT('Ctrl Pts',(64.4161152733605,-57.6185409389093,-3.73047319099325));
#39463=CARTESIAN_POINT('Ctrl Pts',(62.7767959000222,-55.8211458920516,-3.61355655310196));
#39464=CARTESIAN_POINT('Ctrl Pts',(60.4846857428982,-55.0061543308031,-3.49663991521067));
#39465=CARTESIAN_POINT('Ctrl Pts',(58.0786244566074,-55.3651580449409,-3.37972327731938));
#39466=CARTESIAN_POINT('Ctrl Pts',(56.1242720757222,-56.8137670780251,-3.26280663942809));
#39467=CARTESIAN_POINT('Ctrl Pts',(55.0810282573051,-59.0114118263877,-3.1458900015368));
#39468=CARTESIAN_POINT('Ctrl Pts',(55.1942486683988,-61.4414853467666,-3.02897336364552));
#39469=CARTESIAN_POINT('Ctrl Pts',(56.4370957920453,-63.532614982135,-2.91205672575423));
#39470=CARTESIAN_POINT('Ctrl Pts',(58.5178536821771,-64.7933349319883,-2.79514008786294));
#39471=CARTESIAN_POINT('Ctrl Pts',(60.1367865774548,-64.8822246880949,-2.71719566260207));
#39472=CARTESIAN_POINT('Ctrl Pts',(60.9095532484437,-64.7337433741902,-2.67822344997165));
#39473=CARTESIAN_POINT('Ctrl Pts',(61.1782903612393,-64.3861563966327,-10.3217765500284));
#39474=CARTESIAN_POINT('Ctrl Pts',(61.8943147016256,-64.1938047104644,-10.2828043373979));
#39475=CARTESIAN_POINT('Ctrl Pts',(63.229693355883,-63.451885448354,-10.2048599121371));
#39476=CARTESIAN_POINT('Ctrl Pts',(64.4739533858633,-61.526734068083,-10.0879432742458));
#39477=CARTESIAN_POINT('Ctrl Pts',(64.6662009854295,-59.2428511055743,-9.97102663635449));
#39478=CARTESIAN_POINT('Ctrl Pts',(63.7615779554656,-57.1368463158114,-9.8541099984632));
#39479=CARTESIAN_POINT('Ctrl Pts',(61.9726009215247,-55.7039846193705,-9.73719336057191));
#39480=CARTESIAN_POINT('Ctrl Pts',(59.7199094133741,-55.2810448510043,-9.62027672268062));
#39481=CARTESIAN_POINT('Ctrl Pts',(57.5330537492994,-55.9674897645086,-9.50336008478933));
#39482=CARTESIAN_POINT('Ctrl Pts',(55.9261546090045,-57.6019281929839,-9.38644344689803));
#39483=CARTESIAN_POINT('Ctrl Pts',(55.2769691972207,-59.8001290437208,-9.26952680900675));
#39484=CARTESIAN_POINT('Ctrl Pts',(55.7381170612497,-62.0453162735774,-9.15261017111546));
#39485=CARTESIAN_POINT('Ctrl Pts',(57.201185935037,-63.8096727944984,-9.03569353322417));
#39486=CARTESIAN_POINT('Ctrl Pts',(59.3222252400773,-64.678417175511,-8.91877689533288));
#39487=CARTESIAN_POINT('Ctrl Pts',(61.6026017560169,-64.4473176243909,-8.80186025744159));
#39488=CARTESIAN_POINT('Ctrl Pts',(63.5062244528641,-63.1707028049589,-8.68494361955031));
#39489=CARTESIAN_POINT('Ctrl Pts',(64.5855724454654,-61.148691072861,-8.56802698165901));
#39490=CARTESIAN_POINT('Ctrl Pts',(64.5869034291403,-58.856634371963,-8.45111034376772));
#39491=CARTESIAN_POINT('Ctrl Pts',(63.5099035702312,-56.8333711511524,-8.33419370587643));
#39492=CARTESIAN_POINT('Ctrl Pts',(61.6077656028021,-55.5545454188062,-8.21727706798514));
#39493=CARTESIAN_POINT('Ctrl Pts',(59.3276568131192,-55.3208009208871,-8.10036043009385));
#39494=CARTESIAN_POINT('Ctrl Pts',(57.2056147880647,-56.1870755038781,-7.98344379220256));
#39495=CARTESIAN_POINT('Ctrl Pts',(55.7404881294344,-57.9497454491247,-7.86652715431127));
#39496=CARTESIAN_POINT('Ctrl Pts',(55.2767550397765,-60.1943664475432,-7.74961051641999));
#39497=CARTESIAN_POINT('Ctrl Pts',(55.9233408761866,-62.3933827648474,-7.63269387852869));
#39498=CARTESIAN_POINT('Ctrl Pts',(57.5284416367487,-64.0295497087847,-7.51577724063741));
#39499=CARTESIAN_POINT('Ctrl Pts',(59.7142816370973,-64.7188277019528,-7.39886060274611));
#39500=CARTESIAN_POINT('Ctrl Pts',(61.9679321929529,-64.297868125966,-7.28194396485483));
#39501=CARTESIAN_POINT('Ctrl Pts',(63.7575613361973,-62.8684545078156,-7.16502732696354));
#39502=CARTESIAN_POINT('Ctrl Pts',(64.666824206428,-60.7605295960148,-7.04811068907225));
#39503=CARTESIAN_POINT('Ctrl Pts',(64.4725569573379,-58.4827774074056,-6.93119405118095));
#39504=CARTESIAN_POINT('Ctrl Pts',(62.8300366000722,-55.8953814010913,-6.77530520065924));
#39505=CARTESIAN_POINT('Ctrl Pts',(58.8119337618197,-54.7946958895247,-6.58044413750709));
#39506=CARTESIAN_POINT('Ctrl Pts',(55.009598880664,-58.1019512817202,-6.34661086172451));
#39507=CARTESIAN_POINT('Ctrl Pts',(55.542756963141,-62.2338275471998,-6.15174979857236));
#39508=CARTESIAN_POINT('Ctrl Pts',(57.8775296293365,-64.2191053148466,-5.99586094805064));
#39509=CARTESIAN_POINT('Ctrl Pts',(60.1063731327958,-64.7271913645137,-5.87894431015935));
#39510=CARTESIAN_POINT('Ctrl Pts',(62.319976393374,-64.1188600356034,-5.76202767226806));
#39511=CARTESIAN_POINT('Ctrl Pts',(63.9836346579317,-62.5446183321576,-5.64511103437678));
#39512=CARTESIAN_POINT('Ctrl Pts',(64.7128846807238,-60.3710631346135,-5.52819439648548));
#39513=CARTESIAN_POINT('Ctrl Pts',(64.3332140077691,-58.1107864172294,-5.4112777585942));
#39514=CARTESIAN_POINT('Ctrl Pts',(62.9353034095045,-56.2944063140944,-5.2943611207029));
#39515=CARTESIAN_POINT('Ctrl Pts',(60.8471266859465,-55.3492798785154,-5.17744448281161));
#39516=CARTESIAN_POINT('Ctrl Pts',(58.5598965449188,-55.4974354933491,-5.06052784492033));
#39517=CARTESIAN_POINT('Ctrl Pts',(56.6111739988973,-56.7041176806815,-4.94361120702903));
#39518=CARTESIAN_POINT('Ctrl Pts',(55.4591476649235,-58.6856144218269,-4.82669456913774));
#39519=CARTESIAN_POINT('Ctrl Pts',(55.374615830073,-60.9761137008993,-4.70977793124646));
#39520=CARTESIAN_POINT('Ctrl Pts',(56.3774650556715,-63.0371371234872,-4.59286129335517));
#39521=CARTESIAN_POINT('Ctrl Pts',(58.2319300637188,-64.3841643123711,-4.47594465546388));
#39522=CARTESIAN_POINT('Ctrl Pts',(60.5020497212695,-64.7005225232177,-4.35902801757259));
#39523=CARTESIAN_POINT('Ctrl Pts',(62.6541425423612,-63.9118401420491,-4.2421113796813));
#39524=CARTESIAN_POINT('Ctrl Pts',(64.1822761811237,-62.2035273988379,-4.12519474179001));
#39525=CARTESIAN_POINT('Ctrl Pts',(64.7272026038827,-59.977189702326,-4.00827810389872));
#39526=CARTESIAN_POINT('Ctrl Pts',(64.1608167208033,-57.7562146665265,-3.89136146600743));
#39527=CARTESIAN_POINT('Ctrl Pts',(62.6162674875737,-56.0627282192935,-3.77444482811614));
#39528=CARTESIAN_POINT('Ctrl Pts',(60.4566657386756,-55.294851860673,-3.65752819022485));
#39529=CARTESIAN_POINT('Ctrl Pts',(58.1897004509561,-55.6331013320185,-3.54061155233356));
#39530=CARTESIAN_POINT('Ctrl Pts',(56.348330477264,-56.9979653162363,-3.42369491444227));
#39531=CARTESIAN_POINT('Ctrl Pts',(55.3653972758303,-59.0685627642994,-3.30677827655098));
#39532=CARTESIAN_POINT('Ctrl Pts',(55.4720723398751,-61.3581521229303,-3.18986163865969));
#39533=CARTESIAN_POINT('Ctrl Pts',(56.6430696470934,-63.3283921673183,-3.0729450007684));
#39534=CARTESIAN_POINT('Ctrl Pts',(58.603537543715,-64.5162290608077,-2.95602836287711));
#39535=CARTESIAN_POINT('Ctrl Pts',(60.1288788547004,-64.5999800411654,-2.87808393761625));
#39536=CARTESIAN_POINT('Ctrl Pts',(60.8569713719691,-64.4600825304849,-2.83911172498582));
#39537=CARTESIAN_POINT('Ctrl Pts',(61.1059930590745,-64.1170314977274,-10.4826648250425));
#39538=CARTESIAN_POINT('Ctrl Pts',(61.778083722502,-63.9364820874957,-10.4436926124121));
#39539=CARTESIAN_POINT('Ctrl Pts',(63.0315264828174,-63.2400853577248,-10.3657481871512));
#39540=CARTESIAN_POINT('Ctrl Pts',(64.1994414570133,-61.4330570272817,-10.2488315492599));
#39541=CARTESIAN_POINT('Ctrl Pts',(64.3798931671675,-59.2893080946195,-10.1319149113687));
#39542=CARTESIAN_POINT('Ctrl Pts',(63.5307758144917,-57.3125231216816,-10.0149982734774));
#39543=CARTESIAN_POINT('Ctrl Pts',(61.8515664723214,-55.9675786640095,-9.89808163558608));
#39544=CARTESIAN_POINT('Ctrl Pts',(59.7370951550563,-55.5705895485867,-9.78116499769479));
#39545=CARTESIAN_POINT('Ctrl Pts',(57.6844201394341,-56.2149157136367,-9.6642483598035));
#39546=CARTESIAN_POINT('Ctrl Pts',(56.1761167922612,-57.7490685989043,-9.54733172191221));
#39547=CARTESIAN_POINT('Ctrl Pts',(55.5667639679454,-59.8123926855153,-9.43041508402093));
#39548=CARTESIAN_POINT('Ctrl Pts',(55.9996168144089,-61.9198201704793,-9.31349844612963));
#39549=CARTESIAN_POINT('Ctrl Pts',(57.3729150035368,-63.5759196600984,-9.19658180823834));
#39550=CARTESIAN_POINT('Ctrl Pts',(59.3638120069981,-64.3913597987237,-9.07966517034706));
#39551=CARTESIAN_POINT('Ctrl Pts',(61.5042696409321,-64.1744400072173,-8.96274853245577));
#39552=CARTESIAN_POINT('Ctrl Pts',(63.2910902405636,-62.9761554622106,-8.84583189456448));
#39553=CARTESIAN_POINT('Ctrl Pts',(64.3042118168849,-61.0782099178583,-8.72891525667318));
#39554=CARTESIAN_POINT('Ctrl Pts',(64.3054611343321,-58.926788769397,-8.6119986187819));
#39555=CARTESIAN_POINT('Ctrl Pts',(63.2945436153898,-57.0276685249239,-8.49508198089061));
#39556=CARTESIAN_POINT('Ctrl Pts',(61.5091166454485,-55.8273087237513,-8.37816534299932));
#39557=CARTESIAN_POINT('Ctrl Pts',(59.3689103106776,-55.6079062735578,-8.26124870510803));
#39558=CARTESIAN_POINT('Ctrl Pts',(57.3770721118943,-56.42102815553,-8.14433206721674));
#39559=CARTESIAN_POINT('Ctrl Pts',(56.0018423990706,-58.0755445540445,-8.02741542932545));
#39560=CARTESIAN_POINT('Ctrl Pts',(55.5665629507304,-60.1824405502847,-7.91049879143416));
#39561=CARTESIAN_POINT('Ctrl Pts',(56.1734757038936,-62.2465300682299,-7.79358215354287));
#39562=CARTESIAN_POINT('Ctrl Pts',(57.6800910159544,-63.7823054110567,-7.67666551565158));
#39563=CARTESIAN_POINT('Ctrl Pts',(59.7318126867404,-64.4292908242403,-7.55974887776029));
#39564=CARTESIAN_POINT('Ctrl Pts',(61.847184206655,-64.0341604009526,-7.442832239869));
#39565=CARTESIAN_POINT('Ctrl Pts',(63.5270056461378,-62.6924524550791,-7.32591560197771));
#39566=CARTESIAN_POINT('Ctrl Pts',(64.3804781486979,-60.713865174564,-7.20899896408643));
#39567=CARTESIAN_POINT('Ctrl Pts',(64.1981307102675,-58.5758708450136,-7.09208232619513));
#39568=CARTESIAN_POINT('Ctrl Pts',(62.656391785565,-56.147231760628,-6.93619347567341));
#39569=CARTESIAN_POINT('Ctrl Pts',(58.8848308902688,-55.1140818885234,-6.74133241252126));
#39570=CARTESIAN_POINT('Ctrl Pts',(55.3157989053073,-58.218411371884,-6.50749913673868));
#39571=CARTESIAN_POINT('Ctrl Pts',(55.8162435817696,-62.096764807423,-6.31263807358654));
#39572=CARTESIAN_POINT('Ctrl Pts',(58.0077597379512,-63.9602303025007,-6.15674922306482));
#39573=CARTESIAN_POINT('Ctrl Pts',(60.0998463115835,-64.4371413108819,-6.03983258517352));
#39574=CARTESIAN_POINT('Ctrl Pts',(62.1776277500815,-63.8661358528684,-5.92291594728224));
#39575=CARTESIAN_POINT('Ctrl Pts',(63.7392076066267,-62.3884861541258,-5.80599930939095));
#39576=CARTESIAN_POINT('Ctrl Pts',(64.4237124537083,-60.3482955176934,-5.68908267149966));
#39577=CARTESIAN_POINT('Ctrl Pts',(64.067337537274,-58.2267044029319,-5.57216603360837));
#39578=CARTESIAN_POINT('Ctrl Pts',(62.7551996553507,-56.5217733835562,-5.45524939571708));
#39579=CARTESIAN_POINT('Ctrl Pts',(60.7951488577299,-55.634637825052,-5.33833275782579));
#39580=CARTESIAN_POINT('Ctrl Pts',(58.6482581220525,-55.7737029375737,-5.2214161199345));
#39581=CARTESIAN_POINT('Ctrl Pts',(56.8191049006898,-56.9063457628063,-5.10449948204321));
#39582=CARTESIAN_POINT('Ctrl Pts',(55.7377643659967,-58.7662622268436,-4.98758284415192));
#39583=CARTESIAN_POINT('Ctrl Pts',(55.6584192184076,-60.9162215134532,-4.87066620626063));
#39584=CARTESIAN_POINT('Ctrl Pts',(56.5997358236318,-62.8507850768644,-4.75374956836934));
#39585=CARTESIAN_POINT('Ctrl Pts',(58.340414942011,-64.1151616433698,-4.63683293047805));
#39586=CARTESIAN_POINT('Ctrl Pts',(60.471245055803,-64.4121088109674,-4.51991629258676));
#39587=CARTESIAN_POINT('Ctrl Pts',(62.4912901999455,-63.671818244159,-4.40299965469547));
#39588=CARTESIAN_POINT('Ctrl Pts',(63.9256609233314,-62.0683238094486,-4.28608301680419));
#39589=CARTESIAN_POINT('Ctrl Pts',(64.4371518606279,-59.9785892919668,-4.1691663789129));
#39590=CARTESIAN_POINT('Ctrl Pts',(63.9055181682461,-57.8938883941436,-4.0522497410216));
#39591=CARTESIAN_POINT('Ctrl Pts',(62.4557390751251,-56.3043105465354,-3.93533310313032));
#39592=CARTESIAN_POINT('Ctrl Pts',(60.428645734453,-55.5835493905429,-3.81841646523903));
#39593=CARTESIAN_POINT('Ctrl Pts',(58.3007764453048,-55.9010446190962,-3.70149982734774));
#39594=CARTESIAN_POINT('Ctrl Pts',(56.5723888788058,-57.1821635544474,-3.58458318945645));
#39595=CARTESIAN_POINT('Ctrl Pts',(55.6497662943555,-59.125713702211,-3.46766655156516));
#39596=CARTESIAN_POINT('Ctrl Pts',(55.7498960113514,-61.274818899094,-3.35074991367387));
#39597=CARTESIAN_POINT('Ctrl Pts',(56.8490435021415,-63.1241693525015,-3.23383327578258));
#39598=CARTESIAN_POINT('Ctrl Pts',(58.689221405253,-64.2391231896272,-3.11691663789129));
#39599=CARTESIAN_POINT('Ctrl Pts',(60.1209711319459,-64.3177353942359,-3.03897221263043));
#39600=CARTESIAN_POINT('Ctrl Pts',(60.8043894954946,-64.1864216867795,-3.));
#39601=CARTESIAN_POINT('Ctrl Pts',(64.2626697207193,-59.9999992453659,-8.67031832941094));
#39602=CARTESIAN_POINT('Ctrl Pts',(64.262671834753,-59.6527912162173,-8.65087842586792));
#39603=CARTESIAN_POINT('Ctrl Pts',(64.2207061795405,-59.3055836956379,-8.63143852232491));
#39604=CARTESIAN_POINT('Ctrl Pts',(64.1367666616005,-58.9688389200618,-8.6119986187819));
#39605=CARTESIAN_POINT('Ctrl Pts',(63.968488628018,-58.293748687906,-8.57302640615147));
#39606=CARTESIAN_POINT('Ctrl Pts',(63.6315161217039,-57.660708606415,-8.53405419352104));
#39607=CARTESIAN_POINT('Ctrl Pts',(63.16545870689,-57.1441285988073,-8.49508198089061));
#39608=CARTESIAN_POINT('Ctrl Pts',(62.6994012920761,-56.6275485911997,-8.45610976826018));
#39609=CARTESIAN_POINT('Ctrl Pts',(62.1042589687623,-56.2274286574755,-8.41713755562975));
#39610=CARTESIAN_POINT('Ctrl Pts',(61.4499867513102,-55.9908016155812,-8.37816534299932));
#39611=CARTESIAN_POINT('Ctrl Pts',(60.7957145338582,-55.7541745736868,-8.33919313036889));
#39612=CARTESIAN_POINT('Ctrl Pts',(60.0823124222679,-55.6810404236223,-8.30022091773846));
#39613=CARTESIAN_POINT('Ctrl Pts',(59.3936383333422,-55.7799936622521,-8.26124870510803));
#39614=CARTESIAN_POINT('Ctrl Pts',(58.7049642444165,-55.8789469008819,-8.2222764924776));
#39615=CARTESIAN_POINT('Ctrl Pts',(58.0410181781554,-56.149987528206,-8.18330427984717));
#39616=CARTESIAN_POINT('Ctrl Pts',(57.4798401928875,-56.5612605749537,-8.14433206721674));
#39617=CARTESIAN_POINT('Ctrl Pts',(56.9186622076197,-56.9725336217015,-8.10535985458631));
#39618=CARTESIAN_POINT('Ctrl Pts',(56.4602523033451,-57.524039087873,-8.06638764195588));
#39619=CARTESIAN_POINT('Ctrl Pts',(56.1585007764845,-58.1509411536655,-8.02741542932545));
#39620=CARTESIAN_POINT('Ctrl Pts',(55.8567492496238,-58.7778432194579,-7.98844321669502));
#39621=CARTESIAN_POINT('Ctrl Pts',(55.7116561001771,-59.4801418848713,-7.94947100406459));
#39622=CARTESIAN_POINT('Ctrl Pts',(55.740261650981,-60.1753061372356,-7.91049879143416));
#39623=CARTESIAN_POINT('Ctrl Pts',(55.7688672017848,-60.8704703895998,-7.87152657880373));
#39624=CARTESIAN_POINT('Ctrl Pts',(55.9711714528392,-61.5585002289149,-7.8325543661733));
#39625=CARTESIAN_POINT('Ctrl Pts',(56.3234261303765,-62.1584777057102,-7.79358215354287));
#39626=CARTESIAN_POINT('Ctrl Pts',(56.6756808079139,-62.7584551825055,-7.75460994091244));
#39627=CARTESIAN_POINT('Ctrl Pts',(57.1778859119341,-63.2703802967811,-7.71563772828201));
#39628=CARTESIAN_POINT('Ctrl Pts',(57.7709420757419,-63.6341737561162,-7.67666551565158));
#39629=CARTESIAN_POINT('Ctrl Pts',(58.3639982395497,-63.9979672154512,-7.63769330302115));
#39630=CARTESIAN_POINT('Ctrl Pts',(59.0479054631451,-64.2136290198458,-7.59872109039072));
#39631=CARTESIAN_POINT('Ctrl Pts',(59.7424209949285,-64.2556048514951,-7.55974887776029));
#39632=CARTESIAN_POINT('Ctrl Pts',(60.4369365267119,-64.2975806831444,-7.52077666512986));
#39633=CARTESIAN_POINT('Ctrl Pts',(61.1420603666835,-64.1658705420485,-7.48180445249943));
#39634=CARTESIAN_POINT('Ctrl Pts',(61.774592526583,-63.8763974805216,-7.442832239869));
#39635=CARTESIAN_POINT('Ctrl Pts',(62.4071246864826,-63.5869244189948,-7.40386002723857));
#39636=CARTESIAN_POINT('Ctrl Pts',(62.9670651663102,-63.139688437037,-7.36488781460814));
#39637=CARTESIAN_POINT('Ctrl Pts',(63.3892808233173,-62.5863058993055,-7.32591560197771));
#39638=CARTESIAN_POINT('Ctrl Pts',(63.8114964803245,-62.0329233615741,-7.28694338934728));
#39639=CARTESIAN_POINT('Ctrl Pts',(64.0959873145112,-61.373394268069,-7.24797117671685));
#39640=CARTESIAN_POINT('Ctrl Pts',(64.2078414918661,-60.6872973330581,-7.20899896408642));
#39641=CARTESIAN_POINT('Ctrl Pts',(64.2448472649471,-60.4603094092367,-7.1961054191946));
#39642=CARTESIAN_POINT('Ctrl Pts',(64.2629571388165,-60.2304135094119,-7.18321187430277));
#39643=CARTESIAN_POINT('Ctrl Pts',(64.2625444778277,-60.0004819773136,-7.17031832941094));
#39644=CARTESIAN_POINT('Ctrl Pts',(61.322884965569,-64.9244061944433,-10.));
#39645=CARTESIAN_POINT('Ctrl Pts',(61.4613623246005,-64.8748976721282,-10.));
#39646=CARTESIAN_POINT('Ctrl Pts',(61.5973330124332,-64.8193822244967,-10.));
#39647=CARTESIAN_POINT('Ctrl Pts',(61.7304725875119,-64.7581350229247,-10.));
#39648=CARTESIAN_POINT('Ctrl Pts',(61.8646633567708,-64.6964042483669,-10.));
#39649=CARTESIAN_POINT('Ctrl Pts',(61.9959787853947,-64.6288503940197,-10.));
#39650=CARTESIAN_POINT('Ctrl Pts',(62.124061050615,-64.5557090887474,-10.));
#39651=CARTESIAN_POINT('Ctrl Pts',(62.2511463812403,-64.4831370824129,-10.));
#39652=CARTESIAN_POINT('Ctrl Pts',(62.3750492404002,-64.4050637267884,-10.));
#39653=CARTESIAN_POINT('Ctrl Pts',(62.4953860081466,-64.3216816235178,-10.));
#39654=CARTESIAN_POINT('Ctrl Pts',(62.6141471290516,-64.2393912958542,-10.));
#39655=CARTESIAN_POINT('Ctrl Pts',(62.7294354075239,-64.1519298171547,-10.));
#39656=CARTESIAN_POINT('Ctrl Pts',(62.8408411996036,-64.0594534298754,-10.));
#39657=CARTESIAN_POINT('Ctrl Pts',(62.8725488799996,-64.0331333285837,-10.));
#39658=CARTESIAN_POINT('Ctrl Pts',(62.9039417776373,-64.0064068380026,-10.));
#39659=CARTESIAN_POINT('Ctrl Pts',(62.9350097493468,-63.9792772123792,-10.));
#39660=CARTESIAN_POINT('Ctrl Pts',(62.9507442400537,-63.9655373118076,-10.));
#39661=CARTESIAN_POINT('Ctrl Pts',(62.9663953835516,-63.9516940067249,-10.));
#39662=CARTESIAN_POINT('Ctrl Pts',(62.9819618294733,-63.9377477067006,-10.));
#39663=CARTESIAN_POINT('Ctrl Pts',(62.9973179297238,-63.9239898597024,-10.));
#39664=CARTESIAN_POINT('Ctrl Pts',(63.0125855686787,-63.910137153214,-10.));
#39665=CARTESIAN_POINT('Ctrl Pts',(63.0277587514538,-63.8961948001996,-10.));
#39666=CARTESIAN_POINT('Ctrl Pts',(63.1388322518447,-63.7941314443465,-10.));
#39667=CARTESIAN_POINT('Ctrl Pts',(63.2449332640284,-63.6871911500671,-10.));
#39668=CARTESIAN_POINT('Ctrl Pts',(63.3456717247427,-63.5756161384795,-10.));
#39669=CARTESIAN_POINT('Ctrl Pts',(63.4421342550849,-63.4687770239606,-10.));
#39670=CARTESIAN_POINT('Ctrl Pts',(63.5336799426146,-63.357687351767,-10.));
#39671=CARTESIAN_POINT('Ctrl Pts',(63.6201050981688,-63.2427298910755,-10.));
#39672=CARTESIAN_POINT('Ctrl Pts',(63.7063798474185,-63.1279724916591,-10.));
#39673=CARTESIAN_POINT('Ctrl Pts',(63.7875521734868,-63.0093599943829,-10.));
#39674=CARTESIAN_POINT('Ctrl Pts',(63.8633716796039,-62.8872534540177,-10.));
#39675=CARTESIAN_POINT('Ctrl Pts',(63.9290488265557,-62.7814810795189,-10.));
#39676=CARTESIAN_POINT('Ctrl Pts',(63.9907088369082,-62.673086342403,-10.));
#39677=CARTESIAN_POINT('Ctrl Pts',(64.0481572499681,-62.5622984835444,-10.));
#39678=CARTESIAN_POINT('Ctrl Pts',(64.0632545281217,-62.5331837520463,-10.));
#39679=CARTESIAN_POINT('Ctrl Pts',(64.0780607782463,-62.503903736544,-10.));
#39680=CARTESIAN_POINT('Ctrl Pts',(64.0925721116377,-62.4744625907651,-10.));
#39681=CARTESIAN_POINT('Ctrl Pts',(64.1048378651431,-62.449577362971,-10.));
#39682=CARTESIAN_POINT('Ctrl Pts',(64.1168955806734,-62.4245711361352,-10.));
#39683=CARTESIAN_POINT('Ctrl Pts',(64.1287279154018,-62.3994786971242,-10.));
#39684=CARTESIAN_POINT('Ctrl Pts',(64.1887507438292,-62.2721902797369,-10.));
#39685=CARTESIAN_POINT('Ctrl Pts',(64.2430415183514,-62.1425620239058,-10.));
#39686=CARTESIAN_POINT('Ctrl Pts',(64.2914122654767,-62.0109529642666,-10.));
#39687=CARTESIAN_POINT('Ctrl Pts',(64.3393952507057,-61.8803989426737,-10.));
#39688=CARTESIAN_POINT('Ctrl Pts',(64.3815529444373,-61.7478950157847,-10.));
#39689=CARTESIAN_POINT('Ctrl Pts',(64.4176522968207,-61.6137795372952,-10.));
#39690=CARTESIAN_POINT('Ctrl Pts',(64.4263872805874,-61.5813275277682,-10.));
#39691=CARTESIAN_POINT('Ctrl Pts',(64.434767312545,-61.5487811344807,-10.));
#39692=CARTESIAN_POINT('Ctrl Pts',(64.4427886296526,-61.5161451164515,-10.));
#39693=CARTESIAN_POINT('Ctrl Pts',(64.4762031655552,-61.3801927059519,-10.));
#39694=CARTESIAN_POINT('Ctrl Pts',(64.5033968610052,-61.2426844061195,-10.));
#39695=CARTESIAN_POINT('Ctrl Pts',(64.5243233415044,-61.1040536373285,-10.));
#39696=CARTESIAN_POINT('Ctrl Pts',(64.5357567077351,-61.0283115004466,-10.));
#39697=CARTESIAN_POINT('Ctrl Pts',(64.5453183642338,-60.9522344126642,-10.));
#39698=CARTESIAN_POINT('Ctrl Pts',(64.5529943411578,-60.8758947124787,-10.));
#39699=CARTESIAN_POINT('Ctrl Pts',(64.5578649511831,-60.8274551571315,-10.));
#39700=CARTESIAN_POINT('Ctrl Pts',(64.5619762515211,-60.7789098960979,-10.));
#39701=CARTESIAN_POINT('Ctrl Pts',(64.5653237401983,-60.7302777963119,-10.));
#39702=CARTESIAN_POINT('Ctrl Pts',(64.5666136683959,-60.7115378025806,-10.));
#39703=CARTESIAN_POINT('Ctrl Pts',(64.5677903120768,-60.6927823909094,-10.));
#39704=CARTESIAN_POINT('Ctrl Pts',(64.5688529252364,-60.674020922828,-10.));
#39705=CARTESIAN_POINT('Ctrl Pts',(64.5766121022954,-60.5370251107424,-10.));
#39706=CARTESIAN_POINT('Ctrl Pts',(64.5782806847897,-60.4000015709537,-10.));
#39707=CARTESIAN_POINT('Ctrl Pts',(64.5738795675567,-60.2633559862213,-10.));
#39708=CARTESIAN_POINT('Ctrl Pts',(64.5694908670336,-60.1270959146419,-10.));
#39709=CARTESIAN_POINT('Ctrl Pts',(64.5590665340938,-59.9912108741169,-10.));
#39710=CARTESIAN_POINT('Ctrl Pts',(64.5425762288987,-59.8561105901884,-10.));
#39711=CARTESIAN_POINT('Ctrl Pts',(64.5263562657352,-59.7232251400541,-10.));
#39712=CARTESIAN_POINT('Ctrl Pts',(64.5042673687703,-59.591098245371,-10.));
#39713=CARTESIAN_POINT('Ctrl Pts',(64.4762339973929,-59.4601379044057,-10.));
#39714=CARTESIAN_POINT('Ctrl Pts',(64.4633631459476,-59.4000105985925,-10.));
#39715=CARTESIAN_POINT('Ctrl Pts',(64.4492385854436,-59.3401295138928,-10.));
#39716=CARTESIAN_POINT('Ctrl Pts',(64.4338498151205,-59.2805360376953,-10.));
#39717=CARTESIAN_POINT('Ctrl Pts',(64.4113888497131,-59.1935552731982,-10.));
#39718=CARTESIAN_POINT('Ctrl Pts',(64.386234919835,-59.1071868765827,-10.));
#39719=CARTESIAN_POINT('Ctrl Pts',(64.3584258428979,-59.0215528078984,-10.));
#39720=CARTESIAN_POINT('Ctrl Pts',(64.3510564791945,-58.99885990806,-10.));
#39721=CARTESIAN_POINT('Ctrl Pts',(64.3435006224636,-58.9762186151633,-10.));
#39722=CARTESIAN_POINT('Ctrl Pts',(64.3357588976533,-58.9536312872786,-10.));
#39723=CARTESIAN_POINT('Ctrl Pts',(64.3287506921548,-58.9331840821199,-10.));
#39724=CARTESIAN_POINT('Ctrl Pts',(64.3215927201184,-58.912788626874,-10.));
#39725=CARTESIAN_POINT('Ctrl Pts',(64.3142878414638,-58.89245214144,-10.));
#39726=CARTESIAN_POINT('Ctrl Pts',(64.2688704537925,-58.7660119791177,-10.));
#39727=CARTESIAN_POINT('Ctrl Pts',(64.2177539118103,-58.6417791973703,-10.));
#39728=CARTESIAN_POINT('Ctrl Pts',(64.1611296886114,-58.5201308918513,-10.));
#39729=CARTESIAN_POINT('Ctrl Pts',(64.1136394178399,-58.4181054574767,-10.));
#39730=CARTESIAN_POINT('Ctrl Pts',(64.0622740603448,-58.3178981596683,-10.));
#39731=CARTESIAN_POINT('Ctrl Pts',(64.0071247424474,-58.2197495594681,-10.));
#39732=CARTESIAN_POINT('Ctrl Pts',(63.9749821324795,-58.1625457300211,-10.));
#39733=CARTESIAN_POINT('Ctrl Pts',(63.9415537977568,-58.1060415534713,-10.));
#39734=CARTESIAN_POINT('Ctrl Pts',(63.9068550908843,-58.0502878625428,-10.));
#39735=CARTESIAN_POINT('Ctrl Pts',(63.894935289402,-58.031135191228,-10.));
#39736=CARTESIAN_POINT('Ctrl Pts',(63.8828641530877,-58.0120689321377,-10.));
#39737=CARTESIAN_POINT('Ctrl Pts',(63.8706469244938,-57.9930984434797,-10.));
#39738=CARTESIAN_POINT('Ctrl Pts',(63.7998198660847,-57.8831206446772,-10.));
#39739=CARTESIAN_POINT('Ctrl Pts',(63.7241685364943,-57.776484465394,-10.));
#39740=CARTESIAN_POINT('Ctrl Pts',(63.6438531316869,-57.6735585118278,-10.));
#39741=CARTESIAN_POINT('Ctrl Pts',(63.5707659340086,-57.5798956643011,-10.));
#39742=CARTESIAN_POINT('Ctrl Pts',(63.4938156874143,-57.4893053118143,-10.));
#39743=CARTESIAN_POINT('Ctrl Pts',(63.4130998443829,-57.4020947050989,-10.));
#39744=CARTESIAN_POINT('Ctrl Pts',(63.3520427052235,-57.3361246309421,-10.));
#39745=CARTESIAN_POINT('Ctrl Pts',(63.2888302587009,-57.2720891084511,-10.));
#39746=CARTESIAN_POINT('Ctrl Pts',(63.2235668665311,-57.2100812780842,-10.));
#39747=CARTESIAN_POINT('Origin',(60.,-60.,-6.));
#39748=CARTESIAN_POINT('Origin',(60.,-60.,-2.));
#39749=CARTESIAN_POINT('Origin',(-60.,-60.,-2.));
#39750=CARTESIAN_POINT('Origin',(-60.,60.,-2.));
#39751=CARTESIAN_POINT('Origin',(60.,60.,-2.));
#39752=CARTESIAN_POINT('Origin',(46.,46.,-9.));
#39753=CARTESIAN_POINT('Ctrl Pts',(47.303382040875,49.1291532909119,-9.));
#39754=CARTESIAN_POINT('Ctrl Pts',(47.2095003437181,49.1799520323928,-9.));
#39755=CARTESIAN_POINT('Ctrl Pts',(47.1132613420209,49.2258395436386,-9.));
#39756=CARTESIAN_POINT('Ctrl Pts',(47.0150562309281,49.2669287082647,-9.));
#39757=CARTESIAN_POINT('Ctrl Pts',(46.9145918383911,49.3089631596092,-9.));
#39758=CARTESIAN_POINT('Ctrl Pts',(46.812069257442,49.3459762081224,-9.));
#39759=CARTESIAN_POINT('Ctrl Pts',(46.707872720993,49.3780464210823,-9.));
#39760=CARTESIAN_POINT('Ctrl Pts',(46.6771621977228,49.3874986836522,-9.));
#39761=CARTESIAN_POINT('Ctrl Pts',(46.6463060667852,49.3965212754824,-9.));
#39762=CARTESIAN_POINT('Ctrl Pts',(46.6153137287552,49.4051154780772,-9.));
#39763=CARTESIAN_POINT('Ctrl Pts',(46.5945556568678,49.4108717096692,-9.));
#39764=CARTESIAN_POINT('Ctrl Pts',(46.5737364779143,49.4164357562519,-9.));
#39765=CARTESIAN_POINT('Ctrl Pts',(46.5528589766229,49.4218079179609,-9.));
#39766=CARTESIAN_POINT('Ctrl Pts',(46.5322666250878,49.4271067054389,-9.));
#39767=CARTESIAN_POINT('Ctrl Pts',(46.5116250548014,49.4322168424348,-9.));
#39768=CARTESIAN_POINT('Ctrl Pts',(46.4909426777974,49.4371377247396,-9.));
#39769=CARTESIAN_POINT('Ctrl Pts',(46.381602528281,49.4631526265499,-9.));
#39770=CARTESIAN_POINT('Ctrl Pts',(46.271075774618,49.4838943672931,-9.));
#39771=CARTESIAN_POINT('Ctrl Pts',(46.159777013667,49.4994555398657,-9.));
#39772=CARTESIAN_POINT('Ctrl Pts',(46.0642245606241,49.5128151514089,-9.));
#39773=CARTESIAN_POINT('Ctrl Pts',(45.9681022304316,49.5223556770029,-9.));
#39774=CARTESIAN_POINT('Ctrl Pts',(45.8716585758946,49.5281082647279,-9.));
#39775=CARTESIAN_POINT('Ctrl Pts',(45.8389977514598,49.5300563893468,-9.));
#39776=CARTESIAN_POINT('Ctrl Pts',(45.8062999961371,49.5315698759885,-9.));
#39777=CARTESIAN_POINT('Ctrl Pts',(45.7735747590549,49.5326492595276,-9.));
#39778=CARTESIAN_POINT('Ctrl Pts',(45.7546015622976,49.5332750565604,-9.));
#39779=CARTESIAN_POINT('Ctrl Pts',(45.7356170483531,49.5337549639071,-9.));
#39780=CARTESIAN_POINT('Ctrl Pts',(45.7166296773268,49.534088921975,-9.));
#39781=CARTESIAN_POINT('Ctrl Pts',(45.6016680354385,49.536110916898,-9.));
#39782=CARTESIAN_POINT('Ctrl Pts',(45.4868632273739,49.5327830594677,-9.));
#39783=CARTESIAN_POINT('Ctrl Pts',(45.3726342188022,49.5242075664881,-9.));
#39784=CARTESIAN_POINT('Ctrl Pts',(45.2568059442603,49.5155120121138,-9.));
#39785=CARTESIAN_POINT('Ctrl Pts',(45.1415688620258,49.5014210476731,-9.));
#39786=CARTESIAN_POINT('Ctrl Pts',(45.0273402886265,49.4819915828865,-9.));
#39787=CARTESIAN_POINT('Ctrl Pts',(44.9134534204498,49.4626202397186,-9.));
#39788=CARTESIAN_POINT('Ctrl Pts',(44.8005681218786,49.4379423495987,-9.));
#39789=CARTESIAN_POINT('Ctrl Pts',(44.6890920364815,49.4079635851062,-9.));
#39790=CARTESIAN_POINT('Ctrl Pts',(44.6225621987322,49.3900720137391,-9.));
#39791=CARTESIAN_POINT('Ctrl Pts',(44.5565342440641,49.3702914035182,-9.));
#39792=CARTESIAN_POINT('Ctrl Pts',(44.4910958743778,49.348614160014,-9.));
#39793=CARTESIAN_POINT('Ctrl Pts',(44.4459975185961,49.3336747896629,-9.));
#39794=CARTESIAN_POINT('Ctrl Pts',(44.4011792119794,49.3178344584821,-9.));
#39795=CARTESIAN_POINT('Ctrl Pts',(44.3566702061303,49.3010888272762,-9.));
#39796=CARTESIAN_POINT('Ctrl Pts',(44.3429049139472,49.295909908944,-9.));
#39797=CARTESIAN_POINT('Ctrl Pts',(44.329171756633,49.2906453099285,-9.));
#39798=CARTESIAN_POINT('Ctrl Pts',(44.3154794690321,49.2852981639857,-9.));
#39799=CARTESIAN_POINT('Ctrl Pts',(44.2045205723958,49.2419662218545,-9.));
#39800=CARTESIAN_POINT('Ctrl Pts',(44.0960946986793,49.1931609847136,-9.));
#39801=CARTESIAN_POINT('Ctrl Pts',(43.9906292093804,49.1389421571216,-9.));
#39802=CARTESIAN_POINT('Ctrl Pts',(43.9680094585534,49.1273135535052,-9.));
#39803=CARTESIAN_POINT('Ctrl Pts',(43.9455258739352,49.1154357360948,-9.));
#39804=CARTESIAN_POINT('Ctrl Pts',(43.9231826707197,49.103308981174,-9.));
#39805=CARTESIAN_POINT('Ctrl Pts',(43.8230330597324,49.0489528632912,-9.));
#39806=CARTESIAN_POINT('Ctrl Pts',(43.7257027174543,48.9895994060328,-9.));
#39807=CARTESIAN_POINT('Ctrl Pts',(43.6313319971842,48.925638065059,-9.));
#39808=CARTESIAN_POINT('Ctrl Pts',(43.5349249824448,48.8602965913012,-9.));
#39809=CARTESIAN_POINT('Ctrl Pts',(43.4416061360124,48.7901458503572,-9.));
#39810=CARTESIAN_POINT('Ctrl Pts',(43.3515448917371,48.7155502884153,-9.));
#39811=CARTESIAN_POINT('Ctrl Pts',(43.3010473619187,48.673724399335,-9.));
#39812=CARTESIAN_POINT('Ctrl Pts',(43.2515743796257,48.6305002430066,-9.));
#39813=CARTESIAN_POINT('Ctrl Pts',(43.2031594672964,48.5859360444519,-9.));
#39814=CARTESIAN_POINT('Ctrl Pts',(43.1829715430466,48.5673537808187,-9.));
#39815=CARTESIAN_POINT('Ctrl Pts',(43.1629676207064,48.5485384762816,-9.));
#39816=CARTESIAN_POINT('Ctrl Pts',(43.1431502891677,48.529494156865,-9.));
#39817=CARTESIAN_POINT('Ctrl Pts',(43.1324187548122,48.5191812261005,-9.));
#39818=CARTESIAN_POINT('Ctrl Pts',(43.121743487207,48.5088025745941,-9.));
#39819=CARTESIAN_POINT('Ctrl Pts',(43.1111312671148,48.4983653312045,-9.));
#39820=CARTESIAN_POINT('Ctrl Pts',(43.0256520113981,48.4142954769306,-9.));
#39821=CARTESIAN_POINT('Ctrl Pts',(42.9441414511906,48.3263133292321,-9.));
#39822=CARTESIAN_POINT('Ctrl Pts',(42.8667459989365,48.2348514385974,-9.));
#39823=CARTESIAN_POINT('Ctrl Pts',(42.787931061766,48.1417120750572,-9.));
#39824=CARTESIAN_POINT('Ctrl Pts',(42.7133829724,48.044963650616,-9.));
#39825=CARTESIAN_POINT('Ctrl Pts',(42.6432802370783,47.9450129154862,-9.));
#39826=CARTESIAN_POINT('Ctrl Pts',(42.5726093244938,47.8442520873573,-9.));
#39827=CARTESIAN_POINT('Ctrl Pts',(42.5064555090162,47.7402361868037,-9.));
#39828=CARTESIAN_POINT('Ctrl Pts',(42.4450347854646,47.6333403909136,-9.));
#39829=CARTESIAN_POINT('Ctrl Pts',(42.4087714981893,47.5702282565925,-9.));
#39830=CARTESIAN_POINT('Ctrl Pts',(42.3741587493154,47.5061115052744,-9.));
#39831=CARTESIAN_POINT('Ctrl Pts',(42.3412476747171,47.4410620511533,-9.));
#39832=CARTESIAN_POINT('Ctrl Pts',(42.3239077246593,47.4067892630564,-9.));
#39833=CARTESIAN_POINT('Ctrl Pts',(42.3070402397616,47.3722575030078,-9.));
#39834=CARTESIAN_POINT('Ctrl Pts',(42.2906533294539,47.3374769421819,-9.));
#39835=CARTESIAN_POINT('Ctrl Pts',(42.2831049729279,47.3214558577702,-9.));
#39836=CARTESIAN_POINT('Ctrl Pts',(42.2756578447827,47.3053803342217,-9.));
#39837=CARTESIAN_POINT('Ctrl Pts',(42.2683151293564,47.2892565389712,-9.));
#39838=CARTESIAN_POINT('Ctrl Pts',(42.2158991652036,47.1741568483538,-9.));
#39839=CARTESIAN_POINT('Ctrl Pts',(42.168965298218,47.0569640824966,-9.));
#39840=CARTESIAN_POINT('Ctrl Pts',(42.1276944818575,46.9381059675892,-9.));
#39841=CARTESIAN_POINT('Ctrl Pts',(42.0863438342069,46.8190179421183,-9.));
#39842=CARTESIAN_POINT('Ctrl Pts',(42.0506775878683,46.6982573766557,-8.99999999999999));
#39843=CARTESIAN_POINT('Ctrl Pts',(42.0209156826669,46.5762184848755,-8.99999999999999));
#39844=CARTESIAN_POINT('Ctrl Pts',(41.9916665549266,46.4562822405122,-8.99999999999999));
#39845=CARTESIAN_POINT('Ctrl Pts',(41.9681196436424,46.3351105546335,-8.99999999999999));
#39846=CARTESIAN_POINT('Ctrl Pts',(41.9505275256033,46.2130543478546,-8.99999999999999));
#39847=CARTESIAN_POINT('Ctrl Pts',(41.9396355979066,46.1374848583697,-8.99999999999999));
#39848=CARTESIAN_POINT('Ctrl Pts',(41.9310272093262,46.0615758916198,-8.99999999999999));
#39849=CARTESIAN_POINT('Ctrl Pts',(41.9247720476892,45.9854081088662,-8.99999999999999));
#39850=CARTESIAN_POINT('Ctrl Pts',(41.9193705997876,45.9196358180438,-8.99999999999999));
#39851=CARTESIAN_POINT('Ctrl Pts',(41.915724009091,45.853670483811,-9.));
#39852=CARTESIAN_POINT('Ctrl Pts',(41.913803751014,45.7875629828621,-9.));
#39853=CARTESIAN_POINT('Ctrl Pts',(42.5743852316216,43.7746037524369,-9.));
#39854=CARTESIAN_POINT('Ctrl Pts',(42.6510842818103,43.6758334867864,-9.));
#39855=CARTESIAN_POINT('Ctrl Pts',(42.7325420871954,43.5810568881625,-9.));
#39856=CARTESIAN_POINT('Ctrl Pts',(42.8183507984011,43.4904132403405,-9.));
#39857=CARTESIAN_POINT('Ctrl Pts',(42.905364412483,43.3984967987608,-9.));
#39858=CARTESIAN_POINT('Ctrl Pts',(42.9968527722929,43.3108297865861,-9.));
#39859=CARTESIAN_POINT('Ctrl Pts',(43.0924206985133,43.227601359625,-9.));
#39860=CARTESIAN_POINT('Ctrl Pts',(43.132839147332,43.1924016430629,-9.));
#39861=CARTESIAN_POINT('Ctrl Pts',(43.173987598655,43.1579964196685,-9.));
#39862=CARTESIAN_POINT('Ctrl Pts',(43.2158372090038,43.1244025849901,-9.));
#39863=CARTESIAN_POINT('Ctrl Pts',(43.2398459933853,43.105130072615,-9.));
#39864=CARTESIAN_POINT('Ctrl Pts',(43.2640899712917,43.0861213997981,-9.00000000000001));
#39865=CARTESIAN_POINT('Ctrl Pts',(43.2885383440716,43.0673990171184,-9.00000000000001));
#39866=CARTESIAN_POINT('Ctrl Pts',(43.3879649260166,42.9912588775487,-9.00000000000001));
#39867=CARTESIAN_POINT('Ctrl Pts',(43.4908351416811,42.9197950946123,-9.));
#39868=CARTESIAN_POINT('Ctrl Pts',(43.5967555748348,42.8531796409371,-9.));
#39869=CARTESIAN_POINT('Ctrl Pts',(43.6847791881397,42.7978198509528,-9.));
#39870=CARTESIAN_POINT('Ctrl Pts',(43.7749100890708,42.7458091399839,-9.));
#39871=CARTESIAN_POINT('Ctrl Pts',(43.8669310813763,42.6972722115845,-9.));
#39872=CARTESIAN_POINT('Ctrl Pts',(43.9071902655099,42.6760373054098,-9.));
#39873=CARTESIAN_POINT('Ctrl Pts',(43.947811291,42.6554676190036,-9.));
#39874=CARTESIAN_POINT('Ctrl Pts',(43.9887761666103,42.6355751083769,-9.));
#39875=CARTESIAN_POINT('Ctrl Pts',(44.0111456695219,42.6247124957666,-9.));
#39876=CARTESIAN_POINT('Ctrl Pts',(44.0336177053014,42.6140518249009,-9.00000000000001));
#39877=CARTESIAN_POINT('Ctrl Pts',(44.0561893468518,42.6035951629003,-9.00000000000001));
#39878=CARTESIAN_POINT('Ctrl Pts',(44.0723891995466,42.5960903306215,-9.00000000000001));
#39879=CARTESIAN_POINT('Ctrl Pts',(44.0886318158707,42.588694547595,-9.));
#39880=CARTESIAN_POINT('Ctrl Pts',(44.1049153261628,42.5814085416912,-9.));
#39881=CARTESIAN_POINT('Ctrl Pts',(44.2166366261869,42.5314191943725,-9.));
#39882=CARTESIAN_POINT('Ctrl Pts',(44.3302925187242,42.4865883391233,-9.));
#39883=CARTESIAN_POINT('Ctrl Pts',(44.4455161968859,42.4470741286609,-9.));
#39884=CARTESIAN_POINT('Ctrl Pts',(44.5598765647727,42.4078559773457,-9.));
#39885=CARTESIAN_POINT('Ctrl Pts',(44.6757821335432,42.373874917401,-9.));
#39886=CARTESIAN_POINT('Ctrl Pts',(44.792883255394,42.3453358774941,-9.));
#39887=CARTESIAN_POINT('Ctrl Pts',(44.9068402971432,42.3175630900882,-9.));
#39888=CARTESIAN_POINT('Ctrl Pts',(45.0219302512138,42.2949440193141,-9.));
#39889=CARTESIAN_POINT('Ctrl Pts',(45.1378283160657,42.2777163964233,-9.));
#39890=CARTESIAN_POINT('Ctrl Pts',(45.2059618398419,42.2675887152119,-9.));
#39891=CARTESIAN_POINT('Ctrl Pts',(45.2743745433235,42.2593252243489,-9.00000000000001));
#39892=CARTESIAN_POINT('Ctrl Pts',(45.3429985825323,42.2529824582519,-9.00000000000001));
#39893=CARTESIAN_POINT('Ctrl Pts',(45.3908522461537,42.2485594514057,-9.00000000000001));
#39894=CARTESIAN_POINT('Ctrl Pts',(45.4388086450026,42.2450705638683,-9.00000000000001));
#39895=CARTESIAN_POINT('Ctrl Pts',(45.4868441510479,42.2425367943612,-9.00000000000001));
#39896=CARTESIAN_POINT('Ctrl Pts',(45.5023223922575,42.2417203504673,-9.00000000000001));
#39897=CARTESIAN_POINT('Ctrl Pts',(45.5178054105008,42.2410033048907,-9.00000000000001));
#39898=CARTESIAN_POINT('Ctrl Pts',(45.5332839477313,42.2403864886124,-9.00000000000001));
#39899=CARTESIAN_POINT('Ctrl Pts',(45.6490313924479,42.2357739785926,-9.00000000000001));
#39900=CARTESIAN_POINT('Ctrl Pts',(45.764669155912,42.2367543881879,-9.));
#39901=CARTESIAN_POINT('Ctrl Pts',(45.8798835216575,42.2435111643161,-9.));
#39902=CARTESIAN_POINT('Ctrl Pts',(45.9071533193596,42.24511040862,-9.));
#39903=CARTESIAN_POINT('Ctrl Pts',(45.9343993777372,42.2470334785817,-9.00000000000001));
#39904=CARTESIAN_POINT('Ctrl Pts',(45.9616174822091,42.2492832354607,-9.00000000000001));
#39905=CARTESIAN_POINT('Ctrl Pts',(46.0782918804937,42.2589271484086,-9.00000000000001));
#39906=CARTESIAN_POINT('Ctrl Pts',(46.1944539855328,42.2745701138262,-9.00000000000001));
#39907=CARTESIAN_POINT('Ctrl Pts',(46.3097410037823,42.2959688621477,-9.00000000000001));
#39908=CARTESIAN_POINT('Ctrl Pts',(46.4259783104462,42.3175439961796,-9.00000000000001));
#39909=CARTESIAN_POINT('Ctrl Pts',(46.5413268637747,42.34497071593,-9.));
#39910=CARTESIAN_POINT('Ctrl Pts',(46.6553901598249,42.3780460483423,-9.));
#39911=CARTESIAN_POINT('Ctrl Pts',(46.7119947706127,42.394459885069,-9.));
#39912=CARTESIAN_POINT('Ctrl Pts',(46.7682824036172,42.41226547109,-9.));
#39913=CARTESIAN_POINT('Ctrl Pts',(46.8242014173664,42.4314415738847,-9.));
#39914=CARTESIAN_POINT('Ctrl Pts',(46.8468220071947,42.4391987699927,-9.));
#39915=CARTESIAN_POINT('Ctrl Pts',(46.8693822489463,42.4471802617996,-9.00000000000001));
#39916=CARTESIAN_POINT('Ctrl Pts',(46.8918786073677,42.4553847402839,-9.00000000000001));
#39917=CARTESIAN_POINT('Ctrl Pts',(46.9070987891954,42.4609355788682,-9.00000000000001));
#39918=CARTESIAN_POINT('Ctrl Pts',(46.9222893594991,42.4665884167866,-9.00000000000001));
#39919=CARTESIAN_POINT('Ctrl Pts',(46.9374364480238,42.4723378131064,-9.00000000000001));
#39920=CARTESIAN_POINT('Ctrl Pts',(47.0458970233733,42.5135063077472,-9.00000000000001));
#39921=CARTESIAN_POINT('Ctrl Pts',(47.1523003889298,42.559683022919,-9.));
#39922=CARTESIAN_POINT('Ctrl Pts',(47.2563046800238,42.6106192638709,-9.));
#39923=CARTESIAN_POINT('Ctrl Pts',(47.360207427149,42.661505773528,-9.));
#39924=CARTESIAN_POINT('Ctrl Pts',(47.4617165213352,42.7171431270938,-9.00000000000001));
#39925=CARTESIAN_POINT('Ctrl Pts',(47.5604619593116,42.7773262218468,-9.00000000000001));
#39926=CARTESIAN_POINT('Ctrl Pts',(47.6578154101236,42.8366609321364,-9.00000000000001));
#39927=CARTESIAN_POINT('Ctrl Pts',(47.7524831733156,42.9004147535575,-9.00000000000001));
#39928=CARTESIAN_POINT('Ctrl Pts',(47.8440725207098,42.9684235448621,-9.00000000000001));
#39929=CARTESIAN_POINT('Ctrl Pts',(47.8943346524018,43.0057452085929,-9.00000000000001));
#39930=CARTESIAN_POINT('Ctrl Pts',(47.9436689753247,43.0443487994871,-9.));
#39931=CARTESIAN_POINT('Ctrl Pts',(47.992004612389,43.0842104204041,-9.));
#39932=CARTESIAN_POINT('Ctrl Pts',(48.0190276146188,43.1064958548445,-9.));
#39933=CARTESIAN_POINT('Ctrl Pts',(48.0457383875639,43.1291745351713,-9.));
#39934=CARTESIAN_POINT('Ctrl Pts',(48.0721238936586,43.1522425378067,-9.));
#39935=CARTESIAN_POINT('Ctrl Pts',(48.0885406740473,43.166595202937,-9.));
#39936=CARTESIAN_POINT('Ctrl Pts',(48.1048350306298,43.1811018865408,-9.));
#39937=CARTESIAN_POINT('Ctrl Pts',(48.1209818661767,43.195741480298,-9.));
#39938=CARTESIAN_POINT('Ctrl Pts',(48.203597770096,43.2706455237401,-9.));
#39939=CARTESIAN_POINT('Ctrl Pts',(48.2824577883745,43.3491133390206,-9.00000000000001));
#39940=CARTESIAN_POINT('Ctrl Pts',(48.3572276601944,43.4309575696696,-9.00000000000001));
#39941=CARTESIAN_POINT('Ctrl Pts',(48.4308859028047,43.5115849942012,-9.00000000000001));
#39942=CARTESIAN_POINT('Ctrl Pts',(48.5005752103064,43.595489772052,-9.));
#39943=CARTESIAN_POINT('Ctrl Pts',(48.5659337048761,43.6825193013962,-9.));
#39944=CARTESIAN_POINT('Ctrl Pts',(48.6294063439469,43.767037678708,-9.));
#39945=CARTESIAN_POINT('Ctrl Pts',(48.6887947814722,43.8545036158363,-9.));
#39946=CARTESIAN_POINT('Ctrl Pts',(48.7437218093839,43.9447943433075,-9.));
#39947=CARTESIAN_POINT('Ctrl Pts',(48.7713759357979,43.9902530416283,-9.));
#39948=CARTESIAN_POINT('Ctrl Pts',(48.7978984149478,44.0364279976715,-9.));
#39949=CARTESIAN_POINT('Ctrl Pts',(48.8232361680781,44.0833046267998,-9.));
#39950=CARTESIAN_POINT('Ctrl Pts',(48.8494363766439,44.1317768592706,-9.));
#39951=CARTESIAN_POINT('Ctrl Pts',(48.8743697772796,44.1809994232774,-9.));
#39952=CARTESIAN_POINT('Ctrl Pts',(48.8980277622168,44.2309202005125,-9.));
#39953=CARTESIAN_POINT('Origin',(46.,46.,2.76038497140452));
#39954=CARTESIAN_POINT('Ctrl Pts',(41.9098427756084,46.0018622022123,-0.364615028595478));
#39955=CARTESIAN_POINT('Ctrl Pts',(41.9091327304014,46.1207445798862,-0.370425837919348));
#39956=CARTESIAN_POINT('Ctrl Pts',(41.9672599456507,47.5746593135514,-0.441524166511648));
#39957=CARTESIAN_POINT('Ctrl Pts',(43.7008748484235,50.2221781462026,-0.57791001437238));
#39958=CARTESIAN_POINT('Ctrl Pts',(48.2448533065531,50.250832896341,-0.773772572177673));
#39959=CARTESIAN_POINT('Ctrl Pts',(50.7830589135395,46.4820553202928,-0.969635129982967));
#39960=CARTESIAN_POINT('Ctrl Pts',(49.0478253450961,42.2823235547161,-1.16549768778826));
#39961=CARTESIAN_POINT('Ctrl Pts',(44.589457028671,41.4043184071032,-1.36136024559355));
#39962=CARTESIAN_POINT('Ctrl Pts',(42.1450237582726,43.8716100607599,-1.51106602586263));
#39963=CARTESIAN_POINT('Ctrl Pts',(41.9140059020135,45.6034148009506,-1.59548428686327));
#39964=CARTESIAN_POINT('Ctrl Pts',(41.9171329418229,45.9966889238588,-1.61461502859548));
#39965=CARTESIAN_POINT('Ctrl Pts',(41.9194198683446,45.9961669413359,-0.260384971404518));
#39966=CARTESIAN_POINT('Ctrl Pts',(41.9254629731548,46.896854157291,-0.304165019473208));
#39967=CARTESIAN_POINT('Ctrl Pts',(42.657307638586,49.1524155369128,-0.413232586810329));
#39968=CARTESIAN_POINT('Ctrl Pts',(46.3558078761971,50.7932688919524,-0.58758767341588));
#39969=CARTESIAN_POINT('Ctrl Pts',(50.1895250164382,48.3572314578353,-0.783450231221173));
#39970=CARTESIAN_POINT('Ctrl Pts',(50.281582214734,43.813490556254,-0.979312789026467));
#39971=CARTESIAN_POINT('Ctrl Pts',(46.5474666641534,41.224098161527,-1.17517534683176));
#39972=CARTESIAN_POINT('Ctrl Pts',(42.7307414732583,42.7400789827082,-1.35219940762444));
#39973=CARTESIAN_POINT('Ctrl Pts',(41.9246669057656,45.0485594281921,-1.4639359491487));
#39974=CARTESIAN_POINT('Ctrl Pts',(41.9169756956685,46.0033346419049,-1.51038497140452));
#39975=CARTESIAN_POINT('Ctrl Pts',(48.5732344270147,48.2065515280923,5.55111512312578E-16));
#39976=CARTESIAN_POINT('Ctrl Pts',(49.2973603516437,47.3620909591791,-0.0652875192684306));
#39977=CARTESIAN_POINT('Ctrl Pts',(49.8377925944869,44.9184923727932,-0.195862557805293));
#39978=CARTESIAN_POINT('Ctrl Pts',(47.2195282996038,42.1996736729428,-0.391725115610586));
#39979=CARTESIAN_POINT('Ctrl Pts',(43.5104542156236,42.8839736999474,-0.58758767341588));
#39980=CARTESIAN_POINT('Ctrl Pts',(42.0262713464695,46.3485997621082,-0.783450231221173));
#39981=CARTESIAN_POINT('Ctrl Pts',(44.0921763812591,49.5035809965949,-0.979312789026468));
#39982=CARTESIAN_POINT('Ctrl Pts',(47.8627886158846,49.5273588275085,-1.17517534683176));
#39983=CARTESIAN_POINT('Ctrl Pts',(49.9690021914738,46.4000115108843,-1.37103790463705));
#39984=CARTESIAN_POINT('Ctrl Pts',(48.5290981550892,42.9150566143449,-1.56690046244235));
#39985=CARTESIAN_POINT('Ctrl Pts',(44.8295255723225,42.1864842889787,-1.76276302024764));
#39986=CARTESIAN_POINT('Ctrl Pts',(42.175734997888,44.8650909885955,-1.95862557805293));
#39987=CARTESIAN_POINT('Ctrl Pts',(42.9387745105419,48.5577202457448,-2.15448813585823));
#39988=CARTESIAN_POINT('Ctrl Pts',(46.4369034383315,49.9651124328758,-2.35035069366352));
#39989=CARTESIAN_POINT('Ctrl Pts',(49.5446749708226,47.8298347952992,-2.54621325146882));
#39990=CARTESIAN_POINT('Ctrl Pts',(49.4854159118642,44.0596670739996,-2.74207580927411));
#39991=CARTESIAN_POINT('Ctrl Pts',(46.3120712712219,42.0231137852872,-2.9379383670794));
#39992=CARTESIAN_POINT('Ctrl Pts',(42.8599030363351,43.5397550088008,-3.1338009248847));
#39993=CARTESIAN_POINT('Ctrl Pts',(42.2132908762849,47.2545310563557,-3.32966348268999));
#39994=CARTESIAN_POINT('Ctrl Pts',(44.9499580211573,49.8484315832432,-3.52552604049528));
#39995=CARTESIAN_POINT('Ctrl Pts',(48.6247973634805,49.0039062645874,-3.72138859830058));
#39996=CARTESIAN_POINT('Ctrl Pts',(49.9544810003903,45.4755059401351,-3.91725115610587));
#39997=CARTESIAN_POINT('Ctrl Pts',(47.7509876224225,42.415720949153,-4.11311371391117));
#39998=CARTESIAN_POINT('Ctrl Pts',(43.9830540035483,42.5583517256725,-4.30897627171646));
#39999=CARTESIAN_POINT('Ctrl Pts',(42.01718422667,45.7759631591032,-4.50483882952175));
#40000=CARTESIAN_POINT('Ctrl Pts',(43.6098074945965,49.193742909423,-4.70070138732704));
#40001=CARTESIAN_POINT('Ctrl Pts',(47.3379760358727,49.7580359388642,-4.89656394513234));
#40002=CARTESIAN_POINT('Ctrl Pts',(49.8707143391289,46.9646680784839,-5.09242650293763));
#40003=CARTESIAN_POINT('Ctrl Pts',(48.945117923424,43.3094063135909,-5.28828906074292));
#40004=CARTESIAN_POINT('Ctrl Pts',(45.3881716774698,42.0580867456233,-5.48415161854822));
#40005=CARTESIAN_POINT('Ctrl Pts',(42.3778705394672,44.3287153991906,-5.68001417635351));
#40006=CARTESIAN_POINT('Ctrl Pts',(42.6038031037161,48.0925726868875,-5.87587673415881));
#40007=CARTESIAN_POINT('Ctrl Pts',(45.864107183199,49.9867966215158,-6.07173929196409));
#40008=CARTESIAN_POINT('Ctrl Pts',(49.2458264323451,48.3189707046506,-6.26760184976939));
#40009=CARTESIAN_POINT('Ctrl Pts',(49.7275240173135,44.5792336070115,-6.46346440757468));
#40010=CARTESIAN_POINT('Ctrl Pts',(46.8788225841872,42.1088964537141,-6.65932696537998));
#40011=CARTESIAN_POINT('Ctrl Pts',(43.2449255924472,43.1151116077546,-6.85518952318527));
#40012=CARTESIAN_POINT('Ctrl Pts',(42.0725845216841,46.6988625619225,-7.05105208099057));
#40013=CARTESIAN_POINT('Ctrl Pts',(44.4092330005664,49.6582092212329,-7.24691463879585));
#40014=CARTESIAN_POINT('Ctrl Pts',(48.1671818964547,49.3490810528002,-7.44277719660116));
#40015=CARTESIAN_POINT('Ctrl Pts',(49.9888141460323,46.0476882843631,-7.63863975440645));
#40016=CARTESIAN_POINT('Ctrl Pts',(48.2466406173425,42.703665807707,-7.83450231221174));
#40017=CARTESIAN_POINT('Ctrl Pts',(44.4970847166944,42.304836504839,-8.03036487001704));
#40018=CARTESIAN_POINT('Ctrl Pts',(42.090520508291,45.2074018487415,-8.22622742782232));
#40019=CARTESIAN_POINT('Ctrl Pts',(43.1765285507875,48.8183115043247,-8.42208998562762));
#40020=CARTESIAN_POINT('Ctrl Pts',(46.7860126959185,49.9107832013404,-8.61795254343292));
#40021=CARTESIAN_POINT('Ctrl Pts',(49.691563339236,47.5099066949763,-8.81381510123821));
#40022=CARTESIAN_POINT('Ctrl Pts',(49.3022537239607,43.7583823233551,-9.0096776590435));
#40023=CARTESIAN_POINT('Ctrl Pts',(45.955486114933,42.0129799022276,-9.20554021684879));
#40024=CARTESIAN_POINT('Ctrl Pts',(43.7634250628647,43.2205019121706,-9.33611525538566));
#40025=CARTESIAN_POINT('Ctrl Pts',(43.1574106092752,44.1533569326372,-9.40140277465409));
#40026=CARTESIAN_POINT('Ctrl Pts',(48.7491609934165,48.3574087643591,0.133800924884696));
#40027=CARTESIAN_POINT('Ctrl Pts',(49.5227938678302,47.4552142218945,0.0685134056162651));
#40028=CARTESIAN_POINT('Ctrl Pts',(50.1001743140156,44.8445519958907,-0.0620616329205973));
#40029=CARTESIAN_POINT('Ctrl Pts',(47.3029048564098,41.9398534424552,-0.257924190725891));
#40030=CARTESIAN_POINT('Ctrl Pts',(43.3402492637749,42.6709376073043,-0.453786748531184));
#40031=CARTESIAN_POINT('Ctrl Pts',(41.7545959676198,46.3724327866287,-0.649649306336477));
#40032=CARTESIAN_POINT('Ctrl Pts',(43.9617425369805,49.7431133797975,-0.845511864141772));
#40033=CARTESIAN_POINT('Ctrl Pts',(47.9901435127741,49.7685168504526,-1.04137442194706));
#40034=CARTESIAN_POINT('Ctrl Pts',(50.2403544321623,46.4273594473539,-1.23723697975236));
#40035=CARTESIAN_POINT('Ctrl Pts',(48.7020072184249,42.7041455944686,-1.43309953755765));
#40036=CARTESIAN_POINT('Ctrl Pts',(44.7495027244386,41.9257623283536,-1.62896209536294));
#40037=CARTESIAN_POINT('Ctrl Pts',(41.9142781310867,44.7874996726008,-1.82482465316824));
#40038=CARTESIAN_POINT('Ctrl Pts',(42.7294850327982,48.7325861405604,-2.02068721097353));
#40039=CARTESIAN_POINT('Ctrl Pts',(46.4667735974386,50.2361987390397,-2.21654976877882));
#40040=CARTESIAN_POINT('Ctrl Pts',(49.7870168616665,47.9549367095438,-2.41241232658412));
#40041=CARTESIAN_POINT('Ctrl Pts',(49.7237063868474,43.9270106375071,-2.60827488438941));
#40042=CARTESIAN_POINT('Ctrl Pts',(46.3334069204898,41.7512225306933,-2.80413744219471));
#40043=CARTESIAN_POINT('Ctrl Pts',(42.6452212836014,43.3715532898804,-3.));
#40044=CARTESIAN_POINT('Ctrl Pts',(41.954401625036,47.3403006772158,-3.19586255780529));
#40045=CARTESIAN_POINT('Ctrl Pts',(44.8781688837292,50.1115406678118,-3.39172511561059));
#40046=CARTESIAN_POINT('Ctrl Pts',(48.8042491782122,49.2092769488025,-3.58758767341588));
#40047=CARTESIAN_POINT('Ctrl Pts',(50.2248404581203,45.4396473964744,-3.78345023122117));
#40048=CARTESIAN_POINT('Ctrl Pts',(47.8706989231075,42.1706714115666,-3.97931278902647));
#40049=CARTESIAN_POINT('Ctrl Pts',(43.8451596943284,42.3230535510061,-4.17517534683176));
#40050=CARTESIAN_POINT('Ctrl Pts',(41.7448875807613,45.7606462366524,-4.37103790463706));
#40051=CARTESIAN_POINT('Ctrl Pts',(43.44639511518,49.4120923214029,-4.56690046244234));
#40052=CARTESIAN_POINT('Ctrl Pts',(47.4294506125564,50.0149648654316,-4.76276302024764));
#40053=CARTESIAN_POINT('Ctrl Pts',(50.1353468483384,47.0306203838718,-4.95862557805293));
#40054=CARTESIAN_POINT('Ctrl Pts',(49.1464693737532,43.1254561441609,-5.15448813585823));
#40055=CARTESIAN_POINT('Ctrl Pts',(45.3463422759663,41.7885865179659,-5.35035069366352));
#40056=CARTESIAN_POINT('Ctrl Pts',(42.1302332498505,44.2144532246239,-5.54621325146881));
#40057=CARTESIAN_POINT('Ctrl Pts',(42.371612343125,48.2356374321302,-5.74207580927411));
#40058=CARTESIAN_POINT('Ctrl Pts',(45.8548164802582,50.2593654295507,-5.9379383670794));
#40059=CARTESIAN_POINT('Ctrl Pts',(49.4677366840439,48.477513800986,-6.1338009248847));
#40060=CARTESIAN_POINT('Ctrl Pts',(49.9823669086808,44.482098829646,-6.32966348268999));
#40061=CARTESIAN_POINT('Ctrl Pts',(46.9389058156602,41.8428699777639,-6.52552604049529));
#40062=CARTESIAN_POINT('Ctrl Pts',(43.0565670132156,42.9178779224082,-6.72138859830057));
#40063=CARTESIAN_POINT('Ctrl Pts',(41.8040754761498,46.7466423093156,-6.91725115610587));
#40064=CARTESIAN_POINT('Ctrl Pts',(44.3004756432042,49.9083132073737,-7.11311371391116));
#40065=CARTESIAN_POINT('Ctrl Pts',(48.3153475147166,49.5780506033531,-7.30897627171646));
#40066=CARTESIAN_POINT('Ctrl Pts',(50.2615208879286,46.0509486309672,-7.50483882952175));
#40067=CARTESIAN_POINT('Ctrl Pts',(48.4002386594014,42.4783024478534,-7.70070138732704));
#40068=CARTESIAN_POINT('Ctrl Pts',(44.394333594368,42.0522060335642,-7.89656394513234));
#40069=CARTESIAN_POINT('Ctrl Pts',(41.8232377080245,45.1532135984121,-8.09242650293763));
#40070=CARTESIAN_POINT('Ctrl Pts',(42.9834938112478,49.0109934694039,-8.28828906074292));
#40071=CARTESIAN_POINT('Ctrl Pts',(46.8397507126687,50.1781551334624,-8.48415161854822));
#40072=CARTESIAN_POINT('Ctrl Pts',(49.9439476755051,47.613135805253,-8.68001417635351));
#40073=CARTESIAN_POINT('Ctrl Pts',(49.5280217896079,43.6051276890717,-8.8758767341588));
#40074=CARTESIAN_POINT('Ctrl Pts',(45.9524427952592,41.7403958155962,-9.0717392919641));
#40075=CARTESIAN_POINT('Ctrl Pts',(43.6105151899593,43.0304735378497,-9.20231433050096));
#40076=CARTESIAN_POINT('Ctrl Pts',(42.963068816724,44.0271058725704,-9.26760184976939));
#40077=CARTESIAN_POINT('Ctrl Pts',(48.9250875598184,48.5082660006259,0.267601849769392));
#40078=CARTESIAN_POINT('Ctrl Pts',(49.7482273840168,47.54833748461,0.202314330500961));
#40079=CARTESIAN_POINT('Ctrl Pts',(50.3625560335442,44.7706116189882,0.0717392919640985));
#40080=CARTESIAN_POINT('Ctrl Pts',(47.3862814132159,41.6800332119675,-0.124123265841195));
#40081=CARTESIAN_POINT('Ctrl Pts',(43.1700443119262,42.4579015146611,-0.319985823646489));
#40082=CARTESIAN_POINT('Ctrl Pts',(41.4829205887701,46.3962658111493,-0.515848381451782));
#40083=CARTESIAN_POINT('Ctrl Pts',(43.831308692702,49.982645763,-0.711710939257075));
#40084=CARTESIAN_POINT('Ctrl Pts',(48.1174984096636,50.0096748733969,-0.90757349706237));
#40085=CARTESIAN_POINT('Ctrl Pts',(50.5117066728509,46.4547073838233,-1.10343605486766));
#40086=CARTESIAN_POINT('Ctrl Pts',(48.8749162817605,42.4932345745924,-1.29929861267296));
#40087=CARTESIAN_POINT('Ctrl Pts',(44.6694798765548,41.6650403677284,-1.49516117047825));
#40088=CARTESIAN_POINT('Ctrl Pts',(41.6528212642855,44.7099083566062,-1.69102372828354));
#40089=CARTESIAN_POINT('Ctrl Pts',(42.5201955550544,48.9074520353761,-1.88688628608884));
#40090=CARTESIAN_POINT('Ctrl Pts',(46.4966437565457,50.5072850452035,-2.08274884389413));
#40091=CARTESIAN_POINT('Ctrl Pts',(50.0293587525104,48.0800386237884,-2.27861140169942));
#40092=CARTESIAN_POINT('Ctrl Pts',(49.9619968618307,43.7943542010146,-2.47447395950472));
#40093=CARTESIAN_POINT('Ctrl Pts',(46.3547425697576,41.4793312760994,-2.67033651731001));
#40094=CARTESIAN_POINT('Ctrl Pts',(42.4305395308676,43.20335157096,-2.86619907511531));
#40095=CARTESIAN_POINT('Ctrl Pts',(41.6955123737871,47.4260702980758,-3.0620616329206));
#40096=CARTESIAN_POINT('Ctrl Pts',(44.8063797463012,50.3746497523805,-3.25792419072589));
#40097=CARTESIAN_POINT('Ctrl Pts',(48.9837009929438,49.4146476330176,-3.45378674853119));
#40098=CARTESIAN_POINT('Ctrl Pts',(50.4951999158503,45.4037888528138,-3.64964930633648));
#40099=CARTESIAN_POINT('Ctrl Pts',(47.9904102237924,41.9256218739801,-3.84551186414177));
#40100=CARTESIAN_POINT('Ctrl Pts',(43.7072653851086,42.0877553763397,-4.04137442194707));
#40101=CARTESIAN_POINT('Ctrl Pts',(41.4725909348526,45.7453293142015,-4.23723697975236));
#40102=CARTESIAN_POINT('Ctrl Pts',(43.2829827357634,49.6304417333827,-4.43309953755765));
#40103=CARTESIAN_POINT('Ctrl Pts',(47.5209251892401,50.271893791999,-4.62896209536295));
#40104=CARTESIAN_POINT('Ctrl Pts',(50.399979357548,47.0965726892597,-4.82482465316823));
#40105=CARTESIAN_POINT('Ctrl Pts',(49.3478208240825,42.9415059747309,-5.02068721097354));
#40106=CARTESIAN_POINT('Ctrl Pts',(45.3045128744628,41.5190862903084,-5.21654976877882));
#40107=CARTESIAN_POINT('Ctrl Pts',(41.8825959602337,44.1001910500571,-5.41241232658413));
#40108=CARTESIAN_POINT('Ctrl Pts',(42.1394215825338,48.3787021773728,-5.60827488438941));
#40109=CARTESIAN_POINT('Ctrl Pts',(45.8455257773174,50.5319342375856,-5.80413744219471));
#40110=CARTESIAN_POINT('Ctrl Pts',(49.6896469357427,48.6360568973213,-5.99999999999999));
#40111=CARTESIAN_POINT('Ctrl Pts',(50.2372098000482,44.3849640522804,-6.1958625578053));
#40112=CARTESIAN_POINT('Ctrl Pts',(46.9989890471331,41.5768435018138,-6.39172511561059));
#40113=CARTESIAN_POINT('Ctrl Pts',(42.8682084339841,42.7206442370619,-6.58758767341588));
#40114=CARTESIAN_POINT('Ctrl Pts',(41.5355664306156,46.7944220567085,-6.78345023122118));
#40115=CARTESIAN_POINT('Ctrl Pts',(44.191718285842,50.1584171935145,-6.97931278902647));
#40116=CARTESIAN_POINT('Ctrl Pts',(48.4635131329785,49.8070201539059,-7.17517534683176));
#40117=CARTESIAN_POINT('Ctrl Pts',(50.5342276298249,46.0542089775713,-7.37103790463706));
#40118=CARTESIAN_POINT('Ctrl Pts',(48.5538367014603,42.2529390879997,-7.56690046244235));
#40119=CARTESIAN_POINT('Ctrl Pts',(44.2915824720416,41.7995755622895,-7.76276302024764));
#40120=CARTESIAN_POINT('Ctrl Pts',(41.5559549077579,45.0990253480827,-7.95862557805293));
#40121=CARTESIAN_POINT('Ctrl Pts',(42.790459071708,49.2036754344831,-8.15448813585823));
#40122=CARTESIAN_POINT('Ctrl Pts',(46.8934887294189,50.4455270655844,-8.35035069366353));
#40123=CARTESIAN_POINT('Ctrl Pts',(50.1963320117741,47.7163649155299,-8.54621325146881));
#40124=CARTESIAN_POINT('Ctrl Pts',(49.7537898552552,43.4518730547882,-8.74207580927411));
#40125=CARTESIAN_POINT('Ctrl Pts',(45.9493994755854,41.4678117289649,-8.93793836707941));
#40126=CARTESIAN_POINT('Ctrl Pts',(43.4576053170538,42.8404451635287,-9.06851340561627));
#40127=CARTESIAN_POINT('Ctrl Pts',(42.7687270241728,43.9008548125037,-9.1338009248847));
#40128=CARTESIAN_POINT('Ctrl Pts',(49.1010141262202,48.6591232368927,0.401402774654088));
#40129=CARTESIAN_POINT('Ctrl Pts',(49.9736609002034,47.6414607473255,0.336115255385657));
#40130=CARTESIAN_POINT('Ctrl Pts',(50.6249377530729,44.6966712420858,0.205540216848794));
#40131=CARTESIAN_POINT('Ctrl Pts',(47.4696579700219,41.4202129814799,0.0096776590435005));
#40132=CARTESIAN_POINT('Ctrl Pts',(42.9998393600774,42.2448654220179,-0.186184898761793));
#40133=CARTESIAN_POINT('Ctrl Pts',(41.2112452099204,46.4200988356699,-0.382047456567087));
#40134=CARTESIAN_POINT('Ctrl Pts',(43.7008748484235,50.2221781462026,-0.57791001437238));
#40135=CARTESIAN_POINT('Ctrl Pts',(48.2448533065531,50.250832896341,-0.773772572177673));
#40136=CARTESIAN_POINT('Ctrl Pts',(50.7830589135395,46.4820553202928,-0.969635129982967));
#40137=CARTESIAN_POINT('Ctrl Pts',(49.0478253450961,42.2823235547161,-1.16549768778826));
#40138=CARTESIAN_POINT('Ctrl Pts',(44.589457028671,41.4043184071032,-1.36136024559355));
#40139=CARTESIAN_POINT('Ctrl Pts',(41.3913643974842,44.6323170406115,-1.55722280339885));
#40140=CARTESIAN_POINT('Ctrl Pts',(42.3109060773107,49.0823179301917,-1.75308536120414));
#40141=CARTESIAN_POINT('Ctrl Pts',(46.5265139156528,50.7783713513675,-1.94894791900943));
#40142=CARTESIAN_POINT('Ctrl Pts',(50.2717006433544,48.205140538033,-2.14481047681473));
#40143=CARTESIAN_POINT('Ctrl Pts',(50.2002873368139,43.661697764522,-2.34067303462002));
#40144=CARTESIAN_POINT('Ctrl Pts',(46.3760782190255,41.2074400215055,-2.53653559242531));
#40145=CARTESIAN_POINT('Ctrl Pts',(42.2158577781337,43.0351498520396,-2.73239815023061));
#40146=CARTESIAN_POINT('Ctrl Pts',(41.4366231225383,47.5118399189359,-2.9282607080359));
#40147=CARTESIAN_POINT('Ctrl Pts',(44.7345906088731,50.6377588369492,-3.1241232658412));
#40148=CARTESIAN_POINT('Ctrl Pts',(49.1631528076755,49.6200183172327,-3.31998582364649));
#40149=CARTESIAN_POINT('Ctrl Pts',(50.7655593735804,45.3679303091532,-3.51584838145178));
#40150=CARTESIAN_POINT('Ctrl Pts',(48.1101215244772,41.6805723363936,-3.71171093925708));
#40151=CARTESIAN_POINT('Ctrl Pts',(43.5693710758889,41.8524572016734,-3.90757349706237));
#40152=CARTESIAN_POINT('Ctrl Pts',(41.2002942889438,45.7300123917506,-4.10343605486766));
#40153=CARTESIAN_POINT('Ctrl Pts',(43.1195703563469,49.8487911453627,-4.29929861267296));
#40154=CARTESIAN_POINT('Ctrl Pts',(47.6123997659237,50.5288227185664,-4.49516117047825));
#40155=CARTESIAN_POINT('Ctrl Pts',(50.6646118667576,47.1625249946476,-4.69102372828354));
#40156=CARTESIAN_POINT('Ctrl Pts',(49.5491722744117,42.7575558053009,-4.88688628608884));
#40157=CARTESIAN_POINT('Ctrl Pts',(45.2626834729594,41.249586062651,-5.08274884389413));
#40158=CARTESIAN_POINT('Ctrl Pts',(41.6349586706169,43.9859288754904,-5.27861140169943));
#40159=CARTESIAN_POINT('Ctrl Pts',(41.9072308219428,48.5217669226154,-5.47447395950471));
#40160=CARTESIAN_POINT('Ctrl Pts',(45.8362350743765,50.8045030456205,-5.67033651731001));
#40161=CARTESIAN_POINT('Ctrl Pts',(49.9115571874415,48.7945999936567,-5.86619907511531));
#40162=CARTESIAN_POINT('Ctrl Pts',(50.4920526914155,44.2878292749147,-6.0620616329206));
#40163=CARTESIAN_POINT('Ctrl Pts',(47.059072278606,41.3108170258638,-6.2579241907259));
#40164=CARTESIAN_POINT('Ctrl Pts',(42.6798498547524,42.5234105517155,-6.45378674853118));
#40165=CARTESIAN_POINT('Ctrl Pts',(41.2670573850813,46.8422018041016,-6.64964930633648));
#40166=CARTESIAN_POINT('Ctrl Pts',(44.0829609284797,50.4085211796553,-6.84551186414177));
#40167=CARTESIAN_POINT('Ctrl Pts',(48.6116787512404,50.0359897044587,-7.04137442194707));
#40168=CARTESIAN_POINT('Ctrl Pts',(50.8069343717212,46.0574693241754,-7.23723697975236));
#40169=CARTESIAN_POINT('Ctrl Pts',(48.7074347435192,42.027575728146,-7.43309953755765));
#40170=CARTESIAN_POINT('Ctrl Pts',(44.1888313497151,41.5469450910147,-7.62896209536295));
#40171=CARTESIAN_POINT('Ctrl Pts',(41.2886721074914,45.0448370977533,-7.82482465316824));
#40172=CARTESIAN_POINT('Ctrl Pts',(42.5974243321682,49.3963573995622,-8.02068721097353));
#40173=CARTESIAN_POINT('Ctrl Pts',(46.9472267461691,50.7128989977065,-8.21654976877883));
#40174=CARTESIAN_POINT('Ctrl Pts',(50.4487163480431,47.8195940258066,-8.41241232658412));
#40175=CARTESIAN_POINT('Ctrl Pts',(49.9795579209025,43.2986184205048,-8.6082748843894));
#40176=CARTESIAN_POINT('Ctrl Pts',(45.9463561559116,41.1952276423334,-8.80413744219472));
#40177=CARTESIAN_POINT('Ctrl Pts',(43.3046954441484,42.6504167892078,-8.93471248073157));
#40178=CARTESIAN_POINT('Ctrl Pts',(42.5743852316216,43.7746037524369,-9.));
#40179=CARTESIAN_POINT('Ctrl Pts',(48.5732344270147,48.2065515280923,5.55111512312578E-16));
#40180=CARTESIAN_POINT('Ctrl Pts',(48.6498724529377,48.1336147846407,5.78603323158961E-16));
#40181=CARTESIAN_POINT('Ctrl Pts',(48.7225777107301,48.0570419129107,6.40347147519076E-16));
#40182=CARTESIAN_POINT('Ctrl Pts',(48.7913526914527,47.9772484866014,6.6266436782314E-16));
#40183=CARTESIAN_POINT('Ctrl Pts',(48.8618448358061,47.895462789728,6.85538801210275E-16));
#40184=CARTESIAN_POINT('Ctrl Pts',(48.928208390305,47.8102933006344,-6.7353910572983E-17));
#40185=CARTESIAN_POINT('Ctrl Pts',(48.9904198866102,47.7221391971955,2.77555756156289E-17));
#40186=CARTESIAN_POINT('Ctrl Pts',(49.0539468746188,47.6321210332761,1.24876197163927E-16));
#40187=CARTESIAN_POINT('Ctrl Pts',(49.1131448017078,47.5389901598639,1.68613647211554E-16));
#40188=CARTESIAN_POINT('Ctrl Pts',(49.1679552588207,47.4431291844734,5.55111512312578E-17));
#40189=CARTESIAN_POINT('Ctrl Pts',(49.2206161206072,47.3510277527091,-5.3155610957163E-17));
#40190=CARTESIAN_POINT('Ctrl Pts',(49.2692269857254,47.256405341668,1.53540688649506E-16));
#40191=CARTESIAN_POINT('Ctrl Pts',(49.3137022105639,47.1595731524251,1.66533453693773E-16));
#40192=CARTESIAN_POINT('Ctrl Pts',(49.3201152987639,47.1456104715737,1.68406940528153E-16));
#40193=CARTESIAN_POINT('Ctrl Pts',(49.326442337575,47.1316018071751,9.73571062393719E-16));
#40194=CARTESIAN_POINT('Ctrl Pts',(49.3326830075834,47.117548056573,9.85322934354826E-16));
#40195=CARTESIAN_POINT('Ctrl Pts',(49.3392332224637,47.1027972227374,9.97657713551053E-16));
#40196=CARTESIAN_POINT('Ctrl Pts',(49.3456847257789,47.088004706165,9.48337458744454E-16));
#40197=CARTESIAN_POINT('Ctrl Pts',(49.3520361876581,47.0731747255739,9.43689570931383E-16));
#40198=CARTESIAN_POINT('Ctrl Pts',(49.3968937084238,46.9684372375794,9.10863628170813E-16));
#40199=CARTESIAN_POINT('Ctrl Pts',(49.4367850985609,46.861787055252,3.49398990348419E-16));
#40200=CARTESIAN_POINT('Ctrl Pts',(49.4716812246059,46.7536536486796,4.44089209850063E-16));
#40201=CARTESIAN_POINT('Ctrl Pts',(49.5070988999261,46.6439041056987,5.40194647054708E-16));
#40202=CARTESIAN_POINT('Ctrl Pts',(49.5373713257785,46.5326259596867,6.64417056314631E-16));
#40203=CARTESIAN_POINT('Ctrl Pts',(49.5624283638924,46.4202317504508,6.93889390390723E-16));
#40204=CARTESIAN_POINT('Ctrl Pts',(49.5887049858113,46.3023670559666,7.2479621090423E-16));
#40205=CARTESIAN_POINT('Ctrl Pts',(49.6092470262998,46.1832742500753,7.37675641547393E-16));
#40206=CARTESIAN_POINT('Ctrl Pts',(49.6239198903984,46.0634004456029,8.88178419700125E-16));
#40207=CARTESIAN_POINT('Ctrl Pts',(49.6349245384724,45.9734950922486,1.00105550331467E-15));
#40208=CARTESIAN_POINT('Ctrl Pts',(49.642626697916,45.8831497171793,8.62982642107592E-16));
#40209=CARTESIAN_POINT('Ctrl Pts',(49.6469468769482,45.792547505348,8.88178419700125E-16));
#40210=CARTESIAN_POINT('Ctrl Pts',(49.647900301194,45.7725524206909,8.93738898807436E-16));
#40211=CARTESIAN_POINT('Ctrl Pts',(49.6486889090152,45.7525424656911,6.35931628352248E-16));
#40212=CARTESIAN_POINT('Ctrl Pts',(49.6493112460234,45.7325433534409,6.38378239159465E-16));
#40213=CARTESIAN_POINT('Ctrl Pts',(49.6529992119657,45.6140287160447,6.5287684234946E-16));
#40214=CARTESIAN_POINT('Ctrl Pts',(49.6508619840611,45.4957189678778,7.3986846148943E-16));
#40215=CARTESIAN_POINT('Ctrl Pts',(49.6428335563179,45.3780417000535,6.38378239159465E-16));
#40216=CARTESIAN_POINT('Ctrl Pts',(49.6348310508051,45.2607443892198,5.37215709001142E-16));
#40217=CARTESIAN_POINT('Ctrl Pts',(49.6209756516749,45.1440745969525,1.03714765940918E-15));
#40218=CARTESIAN_POINT('Ctrl Pts',(49.6011537548333,45.0284382457395,1.19348975147204E-15));
#40219=CARTESIAN_POINT('Ctrl Pts',(49.5986006508385,45.0135440288755,1.21362695746072E-15));
#40220=CARTESIAN_POINT('Ctrl Pts',(49.5959484928759,44.9986669435562,6.39393560469819E-16));
#40221=CARTESIAN_POINT('Ctrl Pts',(49.5931969753943,44.9838078477401,6.38378239159465E-16));
#40222=CARTESIAN_POINT('Ctrl Pts',(49.5723040282194,44.8709790883241,6.02913079779512E-16));
#40223=CARTESIAN_POINT('Ctrl Pts',(49.5456866559789,44.7591873160563,3.64931038818624E-16));
#40224=CARTESIAN_POINT('Ctrl Pts',(49.5136431171323,44.6486943685595,2.77555756156289E-16));
#40225=CARTESIAN_POINT('Ctrl Pts',(49.4934334709872,44.5790072038202,2.22448748379061E-16));
#40226=CARTESIAN_POINT('Ctrl Pts',(49.4710643432933,44.5098366898445,2.79582804221843E-16));
#40227=CARTESIAN_POINT('Ctrl Pts',(49.4466001824985,44.4412500442809,2.22044604925031E-16));
#40228=CARTESIAN_POINT('Ctrl Pts',(49.437958075777,44.4170214138529,2.0171890223469E-16));
#40229=CARTESIAN_POINT('Ctrl Pts',(49.4290544610887,44.3928656610227,1.16258512332692E-15));
#40230=CARTESIAN_POINT('Ctrl Pts',(49.4198919565046,44.3687858124111,1.16573417585641E-15));
#40231=CARTESIAN_POINT('Ctrl Pts',(49.4140177808709,44.3533479745711,1.1677530657209E-15));
#40232=CARTESIAN_POINT('Ctrl Pts',(49.4080385614616,44.3379450507796,4.6560458043002E-16));
#40233=CARTESIAN_POINT('Ctrl Pts',(49.4019587711633,44.3225866875802,4.71844785465692E-16));
#40234=CARTESIAN_POINT('Ctrl Pts',(49.3590836254494,44.2142783368314,5.15851188164403E-16));
#40235=CARTESIAN_POINT('Ctrl Pts',(49.3111615328034,44.1080549532259,2.48937019875304E-16));
#40236=CARTESIAN_POINT('Ctrl Pts',(49.2585466556507,44.0041726189596,3.33066907387547E-16));
#40237=CARTESIAN_POINT('Ctrl Pts',(49.2040876136808,43.8966491824735,4.20145568840418E-16));
#40238=CARTESIAN_POINT('Ctrl Pts',(49.1446009389686,43.7916331003358,8.50083000759442E-16));
#40239=CARTESIAN_POINT('Ctrl Pts',(49.0804234387592,43.6894117471813,8.32667268468867E-16));
#40240=CARTESIAN_POINT('Ctrl Pts',(49.0155503679019,43.5860824952676,8.1506278042816E-16));
#40241=CARTESIAN_POINT('Ctrl Pts',(48.9458838603176,43.4856081197834,5.53746625258472E-16));
#40242=CARTESIAN_POINT('Ctrl Pts',(48.871719760908,43.3882998852588,6.10622663543836E-16));
#40243=CARTESIAN_POINT('Ctrl Pts',(48.8190210220156,43.3191556323909,6.51037035385447E-16));
#40244=CARTESIAN_POINT('Ctrl Pts',(48.764050303434,43.251610267159,-1.27380500588882E-16));
#40245=CARTESIAN_POINT('Ctrl Pts',(48.7068997131453,43.1857830872598,-1.11022302462516E-16));
#40246=CARTESIAN_POINT('Ctrl Pts',(48.6896338669553,43.1658959442308,-1.060803039395E-16));
#40247=CARTESIAN_POINT('Ctrl Pts',(48.6721689865425,43.1461656757307,8.76550187881266E-16));
#40248=CARTESIAN_POINT('Ctrl Pts',(48.6545074240829,43.1265957195894,8.88178419700125E-16));
#40249=CARTESIAN_POINT('Ctrl Pts',(48.6371228895828,43.1073327252489,8.99624258520571E-16));
#40250=CARTESIAN_POINT('Ctrl Pts',(48.6195440978478,43.0882212546125,1.08275417850399E-15));
#40251=CARTESIAN_POINT('Ctrl Pts',(48.6017950003255,43.0692874663464,1.0547118733939E-15));
#40252=CARTESIAN_POINT('Ctrl Pts',(48.5161349724081,42.977909928451,9.19375153564364E-16));
#40253=CARTESIAN_POINT('Ctrl Pts',(48.4264330472783,42.8905783040618,1.12985113368144E-15));
#40254=CARTESIAN_POINT('Ctrl Pts',(48.3330185610229,42.8076088281368,8.88178419700125E-16));
#40255=CARTESIAN_POINT('Ctrl Pts',(48.2522205241438,42.7358451109195,6.79145734945449E-16));
#40256=CARTESIAN_POINT('Ctrl Pts',(48.1686440240513,42.6673447664859,6.67861884923022E-16));
#40257=CARTESIAN_POINT('Ctrl Pts',(48.0824754659943,42.6023283204542,7.7715611723761E-16));
#40258=CARTESIAN_POINT('Ctrl Pts',(48.0430744722317,42.5725992331592,8.27131438431595E-16));
#40259=CARTESIAN_POINT('Ctrl Pts',(48.003131210002,42.5435988074275,1.18894675673887E-15));
#40260=CARTESIAN_POINT('Ctrl Pts',(47.9626620077452,42.5153495000384,1.16573417585641E-15));
#40261=CARTESIAN_POINT('Ctrl Pts',(47.9441427039662,42.5024222003658,1.15511175651322E-15));
#40262=CARTESIAN_POINT('Ctrl Pts',(47.9255113044799,42.4896509007091,3.58310774532543E-16));
#40263=CARTESIAN_POINT('Ctrl Pts',(47.9067756067456,42.4770420458757,3.33066907387547E-16));
#40264=CARTESIAN_POINT('Ctrl Pts',(47.8018201929055,42.4064085634267,1.9165341103939E-16));
#40265=CARTESIAN_POINT('Ctrl Pts',(47.6937577709793,42.3409782246222,1.69127847991709E-16));
#40266=CARTESIAN_POINT('Ctrl Pts',(47.5828994070635,42.2810832344563,1.11022302462516E-16));
#40267=CARTESIAN_POINT('Ctrl Pts',(47.4730677670903,42.2217429667153,5.34549062680856E-17));
#40268=CARTESIAN_POINT('Ctrl Pts',(47.3604911538792,42.1678352915987,7.49804862520293E-17));
#40269=CARTESIAN_POINT('Ctrl Pts',(47.2454366428579,42.1197191971386,1.66533453693773E-16));
#40270=CARTESIAN_POINT('Ctrl Pts',(47.1845208924579,42.0942440725709,2.69415779354553E-16));
#40271=CARTESIAN_POINT('Ctrl Pts',(47.1229099962542,42.0703931037216,1.36788762772911E-16));
#40272=CARTESIAN_POINT('Ctrl Pts',(47.0606640384105,42.0481501283249,1.66533453693773E-16));
#40273=CARTESIAN_POINT('Ctrl Pts',(42.612019924001,45.9972524552388,-2.01601780324957));
#40274=CARTESIAN_POINT('Ctrl Pts',(42.6094250933538,45.6709119514131,-1.99688706151736));
#40275=CARTESIAN_POINT('Ctrl Pts',(42.6528677689476,45.3452478112547,-1.97775631978515));
#40276=CARTESIAN_POINT('Ctrl Pts',(42.7452066790694,45.0340947481843,-1.95862557805294));
#40277=CARTESIAN_POINT('Ctrl Pts',(43.0603318560328,43.9722220887233,-1.8933380587845));
#40278=CARTESIAN_POINT('Ctrl Pts',(43.9449287141776,43.079353188851,-1.82805053951607));
#40279=CARTESIAN_POINT('Ctrl Pts',(45.0038225737112,42.7543474598092,-1.76276302024764));
#40280=CARTESIAN_POINT('Ctrl Pts',(46.0627164332447,42.4293417307674,-1.69747550097921));
#40281=CARTESIAN_POINT('Ctrl Pts',(47.295907294167,42.6721991725562,-1.63218798171078));
#40282=CARTESIAN_POINT('Ctrl Pts',(48.1524867306922,43.3744537095404,-1.56690046244235));
#40283=CARTESIAN_POINT('Ctrl Pts',(49.0090661672174,44.0767082465247,-1.50161294317392));
#40284=CARTESIAN_POINT('Ctrl Pts',(49.4890341793456,45.2383598787045,-1.43632542390549));
#40285=CARTESIAN_POINT('Ctrl Pts',(49.3779825894782,46.3404102475651,-1.37103790463705));
#40286=CARTESIAN_POINT('Ctrl Pts',(49.2669309996107,47.4424606164257,-1.30575038536862));
#40287=CARTESIAN_POINT('Ctrl Pts',(48.5648598077476,48.4849097219671,-1.24046286610019));
#40288=CARTESIAN_POINT('Ctrl Pts',(47.5853888393785,49.0021713029189,-1.17517534683176));
#40289=CARTESIAN_POINT('Ctrl Pts',(46.6059178710094,49.5194328838706,-1.10988782756333));
#40290=CARTESIAN_POINT('Ctrl Pts',(45.3490471261342,49.5115069402328,-1.0446003082949));
#40291=CARTESIAN_POINT('Ctrl Pts',(44.3762942478984,48.981713762666,-0.979312789026468));
#40292=CARTESIAN_POINT('Ctrl Pts',(43.4035413696625,48.4519205850993,-0.914025269758036));
#40293=CARTESIAN_POINT('Ctrl Pts',(42.714906358066,47.4002601736038,-0.848737750489605));
#40294=CARTESIAN_POINT('Ctrl Pts',(42.6179526637934,46.2969922908292,-0.783450231221173));
#40295=CARTESIAN_POINT('Ctrl Pts',(42.6093234581355,46.198797729728,-0.777639421897304));
#40296=CARTESIAN_POINT('Ctrl Pts',(42.60538131527,46.1001943548762,-0.771828612573434));
#40297=CARTESIAN_POINT('Ctrl Pts',(42.6059705137377,46.0015452631454,-0.766017803249565));
#40298=CARTESIAN_POINT('Ctrl Pts',(44.942095577027,42.0543614925016,0.));
#40299=CARTESIAN_POINT('Ctrl Pts',(43.6472519732775,42.4015349025496,-0.0652875192684312));
#40300=CARTESIAN_POINT('Ctrl Pts',(41.4469681313217,44.4642342884812,-0.195862557805293));
#40301=CARTESIAN_POINT('Ctrl Pts',(42.2010812738077,48.9500090171859,-0.391725115610587));
#40302=CARTESIAN_POINT('Ctrl Pts',(46.3558078761971,50.7932688919524,-0.58758767341588));
#40303=CARTESIAN_POINT('Ctrl Pts',(50.1895250164382,48.3572314578353,-0.783450231221173));
#40304=CARTESIAN_POINT('Ctrl Pts',(50.281582214734,43.813490556254,-0.979312789026467));
#40305=CARTESIAN_POINT('Ctrl Pts',(46.5474666641534,41.224098161527,-1.17517534683176));
#40306=CARTESIAN_POINT('Ctrl Pts',(42.3245742788969,42.9014062059293,-1.37103790463705));
#40307=CARTESIAN_POINT('Ctrl Pts',(41.3853558532093,47.3473770059323,-1.56690046244235));
#40308=CARTESIAN_POINT('Ctrl Pts',(44.5692318828111,50.5894261400569,-1.76276302024764));
#40309=CARTESIAN_POINT('Ctrl Pts',(49.0314017551548,49.7310441604199,-1.95862557805294));
#40310=CARTESIAN_POINT('Ctrl Pts',(50.7851513154972,45.5390953919881,-2.15448813585823));
#40311=CARTESIAN_POINT('Ctrl Pts',(48.2635416323089,41.7589579733313,-2.35035069366352));
#40312=CARTESIAN_POINT('Ctrl Pts',(43.7195493508676,41.7680235772757,-2.54621325146881));
#40313=CARTESIAN_POINT('Ctrl Pts',(41.2130497701183,45.558200280547,-2.74207580927411));
#40314=CARTESIAN_POINT('Ctrl Pts',(42.9835077018007,49.7431068173874,-2.9379383670794));
#40315=CARTESIAN_POINT('Ctrl Pts',(47.4490851541316,50.5836916797423,-3.1338009248847));
#40316=CARTESIAN_POINT('Ctrl Pts',(50.619960918391,47.3289236340817,-3.32966348268999));
#40317=CARTESIAN_POINT('Ctrl Pts',(49.6630787639445,42.8868134693702,-3.52552604049528));
#40318=CARTESIAN_POINT('Ctrl Pts',(45.4333763810852,41.2262159220479,-3.72138859830058));
#40319=CARTESIAN_POINT('Ctrl Pts',(41.7099304228444,43.8308112789577,-3.91725115610586));
#40320=CARTESIAN_POINT('Ctrl Pts',(41.8194970071128,48.3734934933536,-4.11311371391117));
#40321=CARTESIAN_POINT('Ctrl Pts',(45.664182571157,50.7955503680233,-4.30897627171645));
#40322=CARTESIAN_POINT('Ctrl Pts',(49.8089081243513,48.9329670248342,-4.50483882952175));
#40323=CARTESIAN_POINT('Ctrl Pts',(50.5505204413009,44.4498902060922,-4.70070138732704));
#40324=CARTESIAN_POINT('Ctrl Pts',(47.226417382704,41.351776998474,-4.89656394513234));
#40325=CARTESIAN_POINT('Ctrl Pts',(42.8065574559861,42.4066726567364,-5.09242650293762));
#40326=CARTESIAN_POINT('Ctrl Pts',(41.2399158926326,46.6720683948219,-5.28828906074293));
#40327=CARTESIAN_POINT('Ctrl Pts',(43.926226788663,50.3369968125737,-5.48415161854822));
#40328=CARTESIAN_POINT('Ctrl Pts',(48.4653744868355,50.126985023971,-5.68001417635351));
#40329=CARTESIAN_POINT('Ctrl Pts',(50.8018046472976,46.229670491242,-5.87587673415881));
#40330=CARTESIAN_POINT('Ctrl Pts',(48.8480067336088,42.1271542042059,-6.07173929196409));
#40331=CARTESIAN_POINT('Ctrl Pts',(44.3496239015183,41.4848769748296,-6.26760184976939));
#40332=CARTESIAN_POINT('Ctrl Pts',(41.3257891865932,44.8766889552318,-6.46346440757468));
#40333=CARTESIAN_POINT('Ctrl Pts',(42.4781816117647,49.2721361120468,-6.65932696537998));
#40334=CARTESIAN_POINT('Ctrl Pts',(46.7771853228611,50.7440554992066,-6.85518952318527));
#40335=CARTESIAN_POINT('Ctrl Pts',(50.3818002707934,47.9773428079219,-7.05105208099057));
#40336=CARTESIAN_POINT('Ctrl Pts',(50.0714520002853,43.4439513347231,-7.24691463879585));
#40337=CARTESIAN_POINT('Ctrl Pts',(46.1234029772789,41.1942889357184,-7.44277719660116));
#40338=CARTESIAN_POINT('Ctrl Pts',(42.0651280613364,43.2383496733801,-7.63863975440644));
#40339=CARTESIAN_POINT('Ctrl Pts',(41.5224490242513,47.7498293223045,-7.83450231221174));
#40340=CARTESIAN_POINT('Ctrl Pts',(44.9804150360981,50.6979233958617,-8.03036487001703));
#40341=CARTESIAN_POINT('Ctrl Pts',(49.3490853663058,49.448562791698,-8.22622742782233));
#40342=CARTESIAN_POINT('Ctrl Pts',(50.7259992165293,45.1181263046889,-8.42208998562762));
#40343=CARTESIAN_POINT('Ctrl Pts',(47.8793454040792,41.5754411676036,-8.61795254343291));
#40344=CARTESIAN_POINT('Ctrl Pts',(43.3557537989775,41.986275053806,-8.81381510123821));
#40345=CARTESIAN_POINT('Ctrl Pts',(41.190215141007,45.9824985745015,-9.0096776590435));
#40346=CARTESIAN_POINT('Ctrl Pts',(43.3312719327635,49.99581856708,-9.2055402168488));
#40347=CARTESIAN_POINT('Ctrl Pts',(46.3331931919405,50.2864153592086,-9.33611525538566));
#40348=CARTESIAN_POINT('Ctrl Pts',(47.5707104172798,49.7709539622022,-9.40140277465409));
#40349=CARTESIAN_POINT('Ctrl Pts',(45.0021125537771,42.2782052438144,0.133800924884696));
#40350=CARTESIAN_POINT('Ctrl Pts',(43.780727947621,42.6056828306607,0.0685134056162645));
#40351=CARTESIAN_POINT('Ctrl Pts',(41.7052704900895,44.5513612661175,-0.0620616329205976));
#40352=CARTESIAN_POINT('Ctrl Pts',(42.4166013263891,48.7826492644973,-0.257924190725891));
#40353=CARTESIAN_POINT('Ctrl Pts',(46.3356222029269,50.5213374193184,-0.453786748531185));
#40354=CARTESIAN_POINT('Ctrl Pts',(49.9518451088349,48.2235011297195,-0.649649306336477));
#40355=CARTESIAN_POINT('Ctrl Pts',(50.0386797231148,43.9375354922609,-0.845511864141771));
#40356=CARTESIAN_POINT('Ctrl Pts',(46.5164078148468,41.4950443674184,-1.04137442194706));
#40357=CARTESIAN_POINT('Ctrl Pts',(42.5330883329644,43.0771954621779,-1.23723697975236));
#40358=CARTESIAN_POINT('Ctrl Pts',(41.6471535964207,47.2709376861956,-1.43309953755765));
#40359=CARTESIAN_POINT('Ctrl Pts',(44.6504021425806,50.3290590634453,-1.62896209536294));
#40360=CARTESIAN_POINT('Ctrl Pts',(48.8594244340393,49.5193747640485,-1.82482465316824));
#40361=CARTESIAN_POINT('Ctrl Pts',(50.5136803687734,45.5652434073875,-2.02068721097353));
#40362=CARTESIAN_POINT('Ctrl Pts',(48.1351265103291,41.9995605411846,-2.21654976877883));
#40363=CARTESIAN_POINT('Ctrl Pts',(43.8489237542792,42.0081118357741,-2.41241232658412));
#40364=CARTESIAN_POINT('Ctrl Pts',(41.484622772756,45.5832644384377,-2.60827488438941));
#40365=CARTESIAN_POINT('Ctrl Pts',(43.1546391804072,49.5307530830105,-2.80413744219471));
#40366=CARTESIAN_POINT('Ctrl Pts',(47.3668757332087,50.3236499302245,-3.));
#40367=CARTESIAN_POINT('Ctrl Pts',(50.3578615443795,47.2535312100429,-3.19586255780529));
#40368=CARTESIAN_POINT('Ctrl Pts',(49.4552651767856,43.0634305999634,-3.39172511561059));
#40369=CARTESIAN_POINT('Ctrl Pts',(45.4655220417176,41.4970419832635,-3.58758767341588));
#40370=CARTESIAN_POINT('Ctrl Pts',(41.9533144190514,43.953873576657,-3.78345023122117));
#40371=CARTESIAN_POINT('Ctrl Pts',(42.0566650777619,48.2388405883145,-3.97931278902647));
#40372=CARTESIAN_POINT('Ctrl Pts',(45.6832341474444,50.5234894628117,-4.17517534683176));
#40373=CARTESIAN_POINT('Ctrl Pts',(49.5928213537715,48.7665740975379,-4.37103790463706));
#40374=CARTESIAN_POINT('Ctrl Pts',(50.292360560696,44.5378309514381,-4.56690046244235));
#40375=CARTESIAN_POINT('Ctrl Pts',(47.1568403377979,41.615479735464,-4.76276302024764));
#40376=CARTESIAN_POINT('Ctrl Pts',(42.9877276664084,42.6105291100537,-4.95862557805293));
#40377=CARTESIAN_POINT('Ctrl Pts',(41.5099647278547,46.6339406468415,-5.15448813585822));
#40378=CARTESIAN_POINT('Ctrl Pts',(44.0438759788044,50.0909505429741,-5.35035069366352));
#40379=CARTESIAN_POINT('Ctrl Pts',(48.3255089942224,49.8928531318523,-5.54621325146881));
#40380=CARTESIAN_POINT('Ctrl Pts',(50.529388924651,46.2166408373019,-5.74207580927411));
#40381=CARTESIAN_POINT('Ctrl Pts',(48.6864337689787,42.3468682833185,-5.9379383670794));
#40382=CARTESIAN_POINT('Ctrl Pts',(44.4432529494554,41.7410286911291,-6.13380092488469));
#40383=CARTESIAN_POINT('Ctrl Pts',(41.5909662627271,44.940416576927,-6.32966348268999));
#40384=CARTESIAN_POINT('Ctrl Pts',(42.6779812228965,49.0865014623609,-6.52552604049528));
#40385=CARTESIAN_POINT('Ctrl Pts',(46.7330940869803,50.4749159981194,-6.72138859830058));
#40386=CARTESIAN_POINT('Ctrl Pts',(50.1332122138151,47.8651643022338,-6.91725115610587));
#40387=CARTESIAN_POINT('Ctrl Pts',(49.8404706046755,43.5889609499442,-7.11311371391116));
#40388=CARTESIAN_POINT('Ctrl Pts',(46.1164020862178,41.4669262770029,-7.30897627171645));
#40389=CARTESIAN_POINT('Ctrl Pts',(42.2883610042459,43.3950234709796,-7.50483882952175));
#40390=CARTESIAN_POINT('Ctrl Pts',(41.7764692050663,47.6505580994295,-7.70070138732704));
#40391=CARTESIAN_POINT('Ctrl Pts',(45.03825807536,50.4314010587771,-7.89656394513233));
#40392=CARTESIAN_POINT('Ctrl Pts',(49.1590852356714,49.2529191131237,-8.09242650293763));
#40393=CARTESIAN_POINT('Ctrl Pts',(50.4578840834986,45.1681567156775,-8.28828906074292));
#40394=CARTESIAN_POINT('Ctrl Pts',(47.7727264818281,41.8264550009959,-8.48415161854822));
#40395=CARTESIAN_POINT('Ctrl Pts',(43.5057670320466,42.213981481292,-8.6800141763535));
#40396=CARTESIAN_POINT('Ctrl Pts',(41.4630835965936,45.9834914644304,-8.8758767341588));
#40397=CARTESIAN_POINT('Ctrl Pts',(43.4826740697482,49.7691280033295,-9.0717392919641));
#40398=CARTESIAN_POINT('Ctrl Pts',(46.3142904937197,50.0432386738974,-9.20231433050096));
#40399=CARTESIAN_POINT('Ctrl Pts',(47.4816009584782,49.5570204051054,-9.26760184976939));
#40400=CARTESIAN_POINT('Ctrl Pts',(45.0621295305271,42.5020489951272,0.267601849769391));
#40401=CARTESIAN_POINT('Ctrl Pts',(43.9142039219644,42.8098307587719,0.20231433050096));
#40402=CARTESIAN_POINT('Ctrl Pts',(41.9635728488572,44.6384882437539,0.0717392919640979));
#40403=CARTESIAN_POINT('Ctrl Pts',(42.6321213789705,48.6152895118088,-0.124123265841195));
#40404=CARTESIAN_POINT('Ctrl Pts',(46.3154365296567,50.2494059466843,-0.319985823646489));
#40405=CARTESIAN_POINT('Ctrl Pts',(49.7141652012317,48.0897708016036,-0.515848381451782));
#40406=CARTESIAN_POINT('Ctrl Pts',(49.7957772314955,44.0615804282678,-0.711710939257076));
#40407=CARTESIAN_POINT('Ctrl Pts',(46.4853489655401,41.7659905733098,-0.90757349706237));
#40408=CARTESIAN_POINT('Ctrl Pts',(42.7416023870319,43.2529847184266,-1.10343605486766));
#40409=CARTESIAN_POINT('Ctrl Pts',(41.9089513396321,47.1944983664588,-1.29929861267296));
#40410=CARTESIAN_POINT('Ctrl Pts',(44.7315724023501,50.0686919868338,-1.49516117047825));
#40411=CARTESIAN_POINT('Ctrl Pts',(48.6874471129237,49.307705367677,-1.69102372828354));
#40412=CARTESIAN_POINT('Ctrl Pts',(50.2422094220497,45.591391422787,-1.88688628608883));
#40413=CARTESIAN_POINT('Ctrl Pts',(48.0067113883493,42.2401631090378,-2.08274884389413));
#40414=CARTESIAN_POINT('Ctrl Pts',(43.9782981576908,42.2482000942726,-2.27861140169942));
#40415=CARTESIAN_POINT('Ctrl Pts',(41.7561957753938,45.6083285963283,-2.47447395950472));
#40416=CARTESIAN_POINT('Ctrl Pts',(43.3257706590138,49.3183993486336,-2.67033651731001));
#40417=CARTESIAN_POINT('Ctrl Pts',(47.2846663122857,50.0636081807067,-2.86619907511531));
#40418=CARTESIAN_POINT('Ctrl Pts',(50.095762170368,47.1781387860041,-3.0620616329206));
#40419=CARTESIAN_POINT('Ctrl Pts',(49.2474515896267,43.2400477305567,-3.25792419072589));
#40420=CARTESIAN_POINT('Ctrl Pts',(45.4976677023501,41.7678680444789,-3.45378674853118));
#40421=CARTESIAN_POINT('Ctrl Pts',(42.1966984152584,44.0769358743563,-3.64964930633648));
#40422=CARTESIAN_POINT('Ctrl Pts',(42.2938331484111,48.1041876832753,-3.84551186414177));
#40423=CARTESIAN_POINT('Ctrl Pts',(45.702285723732,50.2514285576001,-4.04137442194706));
#40424=CARTESIAN_POINT('Ctrl Pts',(49.3767345831917,48.6001811702416,-4.23723697975236));
#40425=CARTESIAN_POINT('Ctrl Pts',(50.034200680091,44.6257716967841,-4.43309953755765));
#40426=CARTESIAN_POINT('Ctrl Pts',(47.0872632928917,41.8791824724537,-4.62896209536295));
#40427=CARTESIAN_POINT('Ctrl Pts',(43.1688978768307,42.8143855633711,-4.82482465316823));
#40428=CARTESIAN_POINT('Ctrl Pts',(41.7800135630769,46.595812898861,-5.02068721097354));
#40429=CARTESIAN_POINT('Ctrl Pts',(44.1615251689457,49.8449042733747,-5.21654976877882));
#40430=CARTESIAN_POINT('Ctrl Pts',(48.1856435016095,49.6587212397334,-5.41241232658412));
#40431=CARTESIAN_POINT('Ctrl Pts',(50.2569732020045,46.2036111833619,-5.60827488438941));
#40432=CARTESIAN_POINT('Ctrl Pts',(48.5248608043486,42.5665823624312,-5.80413744219471));
#40433=CARTESIAN_POINT('Ctrl Pts',(44.5368819973926,41.9971804074285,-6.));
#40434=CARTESIAN_POINT('Ctrl Pts',(41.8561433388609,45.0041441986222,-6.19586255780529));
#40435=CARTESIAN_POINT('Ctrl Pts',(42.8777808340284,48.900866812675,-6.39172511561059));
#40436=CARTESIAN_POINT('Ctrl Pts',(46.6890028510995,50.2057764970322,-6.58758767341588));
#40437=CARTESIAN_POINT('Ctrl Pts',(49.8846241568369,47.7529857965456,-6.78345023122117));
#40438=CARTESIAN_POINT('Ctrl Pts',(49.6094892090656,43.7339705651652,-6.97931278902646));
#40439=CARTESIAN_POINT('Ctrl Pts',(46.1094011951568,41.7395636182874,-7.17517534683176));
#40440=CARTESIAN_POINT('Ctrl Pts',(42.5115939471553,43.5516972685792,-7.37103790463705));
#40441=CARTESIAN_POINT('Ctrl Pts',(42.0304893858815,47.5512868765546,-7.56690046244235));
#40442=CARTESIAN_POINT('Ctrl Pts',(45.0961011146216,50.1648787216924,-7.76276302024763));
#40443=CARTESIAN_POINT('Ctrl Pts',(48.9690851050371,49.0572754345494,-7.95862557805294));
#40444=CARTESIAN_POINT('Ctrl Pts',(50.1897689504678,45.218187126666,-8.15448813585822));
#40445=CARTESIAN_POINT('Ctrl Pts',(47.6661075595772,42.0774688343883,-8.35035069366352));
#40446=CARTESIAN_POINT('Ctrl Pts',(43.6557802651156,42.441687908778,-8.54621325146882));
#40447=CARTESIAN_POINT('Ctrl Pts',(41.7359520521803,45.9844843543592,-8.74207580927411));
#40448=CARTESIAN_POINT('Ctrl Pts',(43.6340762067327,49.542437439579,-8.9379383670794));
#40449=CARTESIAN_POINT('Ctrl Pts',(46.2953877954988,49.8000619885861,-9.06851340561627));
#40450=CARTESIAN_POINT('Ctrl Pts',(47.3924914996766,49.3430868480086,-9.1338009248847));
#40451=CARTESIAN_POINT('Ctrl Pts',(45.1221465072772,42.72589274644,0.401402774654087));
#40452=CARTESIAN_POINT('Ctrl Pts',(44.0476798963078,43.0139786868831,0.336115255385656));
#40453=CARTESIAN_POINT('Ctrl Pts',(42.221875207625,44.7256152213902,0.205540216848794));
#40454=CARTESIAN_POINT('Ctrl Pts',(42.8476414315519,48.4479297591202,0.00967765904350007));
#40455=CARTESIAN_POINT('Ctrl Pts',(46.2952508563866,49.9774744740503,-0.186184898761793));
#40456=CARTESIAN_POINT('Ctrl Pts',(49.4764852936283,47.9560404734877,-0.382047456567087));
#40457=CARTESIAN_POINT('Ctrl Pts',(49.5528747398763,44.1856253642746,-0.57791001437238));
#40458=CARTESIAN_POINT('Ctrl Pts',(46.4542901162335,42.0369367792011,-0.773772572177674));
#40459=CARTESIAN_POINT('Ctrl Pts',(42.9501164410994,43.4287739746753,-0.969635129982967));
#40460=CARTESIAN_POINT('Ctrl Pts',(42.1707490828436,47.118059046722,-1.16549768778826));
#40461=CARTESIAN_POINT('Ctrl Pts',(44.8127426621197,49.8083249102222,-1.36136024559355));
#40462=CARTESIAN_POINT('Ctrl Pts',(48.5154697918081,49.0960359713057,-1.55722280339885));
#40463=CARTESIAN_POINT('Ctrl Pts',(49.970738475326,45.6175394381864,-1.75308536120414));
#40464=CARTESIAN_POINT('Ctrl Pts',(47.8782962663694,42.4807656768911,-1.94894791900943));
#40465=CARTESIAN_POINT('Ctrl Pts',(44.1076725611025,42.4882883527711,-2.14481047681473));
#40466=CARTESIAN_POINT('Ctrl Pts',(42.0277687780314,45.6333927542189,-2.34067303462002));
#40467=CARTESIAN_POINT('Ctrl Pts',(43.4969021376203,49.1060456142567,-2.53653559242531));
#40468=CARTESIAN_POINT('Ctrl Pts',(47.2024568913628,49.8035664311889,-2.73239815023061));
#40469=CARTESIAN_POINT('Ctrl Pts',(49.8336627963565,47.1027463619653,-2.9282607080359));
#40470=CARTESIAN_POINT('Ctrl Pts',(49.0396380024677,43.4166648611499,-3.12412326584119));
#40471=CARTESIAN_POINT('Ctrl Pts',(45.5298133629825,42.0386941056945,-3.31998582364649));
#40472=CARTESIAN_POINT('Ctrl Pts',(42.4400824114655,44.1999981720555,-3.51584838145178));
#40473=CARTESIAN_POINT('Ctrl Pts',(42.5310012190602,47.9695347782363,-3.71171093925708));
#40474=CARTESIAN_POINT('Ctrl Pts',(45.7213373000194,49.9793676523885,-3.90757349706237));
#40475=CARTESIAN_POINT('Ctrl Pts',(49.1606478126119,48.4337882429453,-4.10343605486766));
#40476=CARTESIAN_POINT('Ctrl Pts',(49.776040799486,44.7137124421301,-4.29929861267295));
#40477=CARTESIAN_POINT('Ctrl Pts',(47.0176862479855,42.1428852094436,-4.49516117047825));
#40478=CARTESIAN_POINT('Ctrl Pts',(43.3500680872531,43.0182420166884,-4.69102372828354));
#40479=CARTESIAN_POINT('Ctrl Pts',(42.0500623982989,46.5576851508807,-4.88688628608884));
#40480=CARTESIAN_POINT('Ctrl Pts',(44.279174359087,49.5988580037752,-5.08274884389412));
#40481=CARTESIAN_POINT('Ctrl Pts',(48.0457780089964,49.4245893476147,-5.27861140169943));
#40482=CARTESIAN_POINT('Ctrl Pts',(49.9845574793579,46.1905815294217,-5.47447395950471));
#40483=CARTESIAN_POINT('Ctrl Pts',(48.3632878397186,42.7862964415439,-5.67033651731002));
#40484=CARTESIAN_POINT('Ctrl Pts',(44.6305110453297,42.2533321237279,-5.8661990751153));
#40485=CARTESIAN_POINT('Ctrl Pts',(42.1213204149949,45.0678718203174,-6.06206163292059));
#40486=CARTESIAN_POINT('Ctrl Pts',(43.0775804451602,48.7152321629891,-6.25792419072589));
#40487=CARTESIAN_POINT('Ctrl Pts',(46.6449116152187,49.936636995945,-6.45378674853118));
#40488=CARTESIAN_POINT('Ctrl Pts',(49.6360360998585,47.6408072908576,-6.64964930633648));
#40489=CARTESIAN_POINT('Ctrl Pts',(49.3785078134558,43.8789801803862,-6.84551186414177));
#40490=CARTESIAN_POINT('Ctrl Pts',(46.1024003040958,42.012200959572,-7.04137442194707));
#40491=CARTESIAN_POINT('Ctrl Pts',(42.7348268900648,43.7083710661787,-7.23723697975235));
#40492=CARTESIAN_POINT('Ctrl Pts',(42.2845095666966,47.4520156536797,-7.43309953755766));
#40493=CARTESIAN_POINT('Ctrl Pts',(45.1539441538833,49.8983563846077,-7.62896209536294));
#40494=CARTESIAN_POINT('Ctrl Pts',(48.7790849744028,48.8616317559751,-7.82482465316824));
#40495=CARTESIAN_POINT('Ctrl Pts',(49.921653817437,45.2682175376546,-8.02068721097353));
#40496=CARTESIAN_POINT('Ctrl Pts',(47.5594886373262,42.3284826677807,-8.21654976877883));
#40497=CARTESIAN_POINT('Ctrl Pts',(43.8057934981846,42.6693943362641,-8.41241232658412));
#40498=CARTESIAN_POINT('Ctrl Pts',(42.008820507767,45.985477244288,-8.60827488438941));
#40499=CARTESIAN_POINT('Ctrl Pts',(43.7854783437173,49.3157468758285,-8.80413744219471));
#40500=CARTESIAN_POINT('Ctrl Pts',(46.276485097278,49.5568853032748,-8.93471248073157));
#40501=CARTESIAN_POINT('Ctrl Pts',(47.303382040875,49.1291532909119,-9.));
#40502=CARTESIAN_POINT('Ctrl Pts',(42.6118894404877,46.0027670997301,-1.10898219675043));
#40503=CARTESIAN_POINT('Ctrl Pts',(42.6093009894316,46.3240935072758,-1.12782069376304));
#40504=CARTESIAN_POINT('Ctrl Pts',(42.6514001366817,46.6447561369006,-1.14665919077565));
#40505=CARTESIAN_POINT('Ctrl Pts',(42.7409759057656,46.9515558452975,-1.16549768778826));
#40506=CARTESIAN_POINT('Ctrl Pts',(43.0514136092689,48.0148143345554,-1.23078520705669));
#40507=CARTESIAN_POINT('Ctrl Pts',(43.9320781356943,48.9115696223888,-1.29607272632512));
#40508=CARTESIAN_POINT('Ctrl Pts',(44.9895315871884,49.2412324431528,-1.36136024559355));
#40509=CARTESIAN_POINT('Ctrl Pts',(46.0469850386825,49.5708952639167,-1.42664776486199));
#40510=CARTESIAN_POINT('Ctrl Pts',(47.2812274152453,49.3334656176112,-1.49193528413042));
#40511=CARTESIAN_POINT('Ctrl Pts',(48.140893384113,48.6350013722719,-1.55722280339885));
#40512=CARTESIAN_POINT('Ctrl Pts',(49.0005593529807,47.9365371269326,-1.62251032266728));
#40513=CARTESIAN_POINT('Ctrl Pts',(49.4856489141533,46.7770382825595,-1.68779784193571));
#40514=CARTESIAN_POINT('Ctrl Pts',(49.3794533265802,45.6744932334904,-1.75308536120414));
#40515=CARTESIAN_POINT('Ctrl Pts',(49.2732577390071,44.5719481844213,-1.81837288047257));
#40516=CARTESIAN_POINT('Ctrl Pts',(48.5757770026882,43.5263569306562,-1.883660399741));
#40517=CARTESIAN_POINT('Ctrl Pts',(47.5985993503177,43.004815083087,-1.94894791900943));
#40518=CARTESIAN_POINT('Ctrl Pts',(46.6214216979471,42.4832732355177,-2.01423543827787));
#40519=CARTESIAN_POINT('Ctrl Pts',(45.3645471295248,42.4857807941444,-2.0795229575463));
#40520=CARTESIAN_POINT('Ctrl Pts',(44.3894592148018,43.0112186403657,-2.14481047681473));
#40521=CARTESIAN_POINT('Ctrl Pts',(43.4143713000788,43.536656486587,-2.21009799608316));
#40522=CARTESIAN_POINT('Ctrl Pts',(42.7210700390551,44.585024620403,-2.27538551535159));
#40523=CARTESIAN_POINT('Ctrl Pts',(42.6192749684748,45.6879841639839,-2.34067303462002));
#40524=CARTESIAN_POINT('Ctrl Pts',(42.6097592015399,45.7910884292043,-2.34677608866349));
#40525=CARTESIAN_POINT('Ctrl Pts',(42.6054122782067,45.8946697383908,-2.35287914270696));
#40526=CARTESIAN_POINT('Ctrl Pts',(42.6060554931448,45.9983056788579,-2.35898219675043));
#40527=CARTESIAN_POINT('Ctrl Pts',(44.942095577027,42.0543614925016,0.));
#40528=CARTESIAN_POINT('Ctrl Pts',(44.8266307302754,42.0960014427504,4.42886871984448E-17));
#40529=CARTESIAN_POINT('Ctrl Pts',(44.7135214812892,42.1431495451391,-5.03172530635855E-16));
#40530=CARTESIAN_POINT('Ctrl Pts',(44.6029924719227,42.1954516455847,-3.95516952522712E-16));
#40531=CARTESIAN_POINT('Ctrl Pts',(44.4901067525159,42.2488689363858,-2.85565931943401E-16));
#40532=CARTESIAN_POINT('Ctrl Pts',(44.3799118551348,42.3076629065189,1.44264892563786E-16));
#40533=CARTESIAN_POINT('Ctrl Pts',(44.2726743864217,42.3715030161957,1.66533453693773E-16));
#40534=CARTESIAN_POINT('Ctrl Pts',(44.1607060042205,42.4381595112235,1.89784419924096E-16));
#40535=CARTESIAN_POINT('Ctrl Pts',(44.0519608304487,42.5103177258471,-2.8701074745102E-17));
#40536=CARTESIAN_POINT('Ctrl Pts',(43.946783909642,42.5876437180967,6.93889390390723E-17));
#40537=CARTESIAN_POINT('Ctrl Pts',(43.8547541039362,42.655303961315,1.55217701100225E-16));
#40538=CARTESIAN_POINT('Ctrl Pts',(43.765456599975,42.726921786639,-2.27548279265547E-16));
#40539=CARTESIAN_POINT('Ctrl Pts',(43.6791551681974,42.8022928629544,-2.4980018054066E-16));
#40540=CARTESIAN_POINT('Ctrl Pts',(43.6621958485022,42.8171042299581,-2.54172959760878E-16));
#40541=CARTESIAN_POINT('Ctrl Pts',(43.6453523327829,42.8320605803158,-3.03677325780712E-16));
#40542=CARTESIAN_POINT('Ctrl Pts',(43.6286267795443,42.8471604216388,-2.91433543964104E-16));
#40543=CARTESIAN_POINT('Ctrl Pts',(43.6160043212654,42.858555985923,-2.82193393701082E-16));
#40544=CARTESIAN_POINT('Ctrl Pts',(43.6034490907185,42.8700333172051,-2.10429711059181E-16));
#40545=CARTESIAN_POINT('Ctrl Pts',(43.5909724483507,42.8815818989063,-2.08166817117217E-16));
#40546=CARTESIAN_POINT('Ctrl Pts',(43.5004972697294,42.9653271856134,-1.9175729542341E-16));
#40547=CARTESIAN_POINT('Ctrl Pts',(43.4140102484227,43.05294274113,-3.77380346460283E-16));
#40548=CARTESIAN_POINT('Ctrl Pts',(43.3317690097074,43.1441141207288,-2.77555756156289E-16));
#40549=CARTESIAN_POINT('Ctrl Pts',(43.2498535715234,43.2349243228407,-1.78126623229546E-16));
#40550=CARTESIAN_POINT('Ctrl Pts',(43.1721498672441,43.3292629650551,-1.87918282286947E-16));
#40551=CARTESIAN_POINT('Ctrl Pts',(43.0989549512928,43.4268482158262,-2.91433543964104E-16));
#40552=CARTESIAN_POINT('Ctrl Pts',(43.0268392362533,43.5229946495667,-3.93422555308908E-16));
#40553=CARTESIAN_POINT('Ctrl Pts',(42.9590999801082,43.6222933564817,2.20767809209777E-16));
#40554=CARTESIAN_POINT('Ctrl Pts',(42.8960686068535,43.7244922554337,3.05311331771918E-16));
#40555=CARTESIAN_POINT('Ctrl Pts',(42.8445094854135,43.8080900761696,3.74467206404779E-16));
#40556=CARTESIAN_POINT('Ctrl Pts',(42.7961012115271,43.8936289130541,-5.33629442249871E-16));
#40557=CARTESIAN_POINT('Ctrl Pts',(42.7510518070775,43.980974939088,-4.9960036108132E-16));
#40558=CARTESIAN_POINT('Ctrl Pts',(42.74041777222,44.0015932068954,-4.91567703608139E-16));
#40559=CARTESIAN_POINT('Ctrl Pts',(42.7299710086774,44.0223121796291,-4.88458287812069E-16));
#40560=CARTESIAN_POINT('Ctrl Pts',(42.7197144645543,44.0431301039729,-4.9960036108132E-16));
#40561=CARTESIAN_POINT('Ctrl Pts',(42.7124726338891,44.0578290007056,-5.07467436668099E-16));
#40562=CARTESIAN_POINT('Ctrl Pts',(42.7053263583429,44.0725758823316,1.51950655804844E-16));
#40563=CARTESIAN_POINT('Ctrl Pts',(42.6982817518653,44.0873590202079,1.38777878078145E-16));
#40564=CARTESIAN_POINT('Ctrl Pts',(42.6476425106855,44.1936256919781,4.40870716540678E-17));
#40565=CARTESIAN_POINT('Ctrl Pts',(42.6021758605503,44.3019194279858,-6.69941841300824E-16));
#40566=CARTESIAN_POINT('Ctrl Pts',(42.5621529437021,44.41198419035,-6.38378239159465E-16));
#40567=CARTESIAN_POINT('Ctrl Pts',(42.5229361716051,44.5198320195807,-6.07450393584487E-16));
#40568=CARTESIAN_POINT('Ctrl Pts',(42.4889458186532,44.6293808836332,-3.54776608850978E-16));
#40569=CARTESIAN_POINT('Ctrl Pts',(42.4604858664397,44.7404006911176,-2.22044604925031E-16));
#40570=CARTESIAN_POINT('Ctrl Pts',(42.4550252974187,44.7617018977013,-1.96577511259863E-16));
#40571=CARTESIAN_POINT('Ctrl Pts',(42.4497684749154,44.7830572714539,-1.49720226808031E-16));
#40572=CARTESIAN_POINT('Ctrl Pts',(42.4447177681396,44.8044652044406,-1.66533453693773E-16));
#40573=CARTESIAN_POINT('Ctrl Pts',(42.4175098232356,44.9197888387505,-2.84861175164851E-16));
#40574=CARTESIAN_POINT('Ctrl Pts',(42.3962790783293,45.0366384306533,-9.22849484574937E-16));
#40575=CARTESIAN_POINT('Ctrl Pts',(42.3809409474924,45.1545774247301,-1.0547118733939E-15));
#40576=CARTESIAN_POINT('Ctrl Pts',(42.3724305620896,45.2200160563527,-1.1278759219288E-15));
#40577=CARTESIAN_POINT('Ctrl Pts',(42.3657352040573,45.2857899368098,1.34755129582655E-16));
#40578=CARTESIAN_POINT('Ctrl Pts',(42.3608470177873,45.3518224752913,1.66533453693773E-16));
#40579=CARTESIAN_POINT('Ctrl Pts',(42.3589207553668,45.3778435780852,1.79056174420974E-16));
#40580=CARTESIAN_POINT('Ctrl Pts',(42.3572751729226,45.4039048254304,-5.56858868693118E-16));
#40581=CARTESIAN_POINT('Ctrl Pts',(42.3559099796205,45.4300014357341,-5.55111512312578E-16));
#40582=CARTESIAN_POINT('Ctrl Pts',(42.3550355815509,45.4467161571147,-5.53992341097868E-16));
#40583=CARTESIAN_POINT('Ctrl Pts',(42.3542762567425,45.4634458531474,-4.42970038635353E-16));
#40584=CARTESIAN_POINT('Ctrl Pts',(42.3536323516061,45.4801738313914,-4.44089209850063E-16));
#40585=CARTESIAN_POINT('Ctrl Pts',(42.3490550645524,45.5990869350797,-4.52044990325077E-16));
#40586=CARTESIAN_POINT('Ctrl Pts',(42.3502944925708,45.7181022972958,-2.70567314906092E-16));
#40587=CARTESIAN_POINT('Ctrl Pts',(42.3571975065646,45.8367846513465,-3.88578058618805E-16));
#40588=CARTESIAN_POINT('Ctrl Pts',(42.3639586270055,45.9530274534999,-5.04163055589147E-16));
#40589=CARTESIAN_POINT('Ctrl Pts',(42.3761534299899,46.0689517074927,-3.47685979037171E-16));
#40590=CARTESIAN_POINT('Ctrl Pts',(42.3936903792512,46.1841385916871,-2.77555756156289E-16));
#40591=CARTESIAN_POINT('Ctrl Pts',(42.4110240724559,46.2979904414069,-2.0823835381404E-16));
#40592=CARTESIAN_POINT('Ctrl Pts',(42.4335771976944,46.4111227280688,-2.32655623883673E-16));
#40593=CARTESIAN_POINT('Ctrl Pts',(42.4613062683471,46.5231086200947,-5.55111512312578E-17));
#40594=CARTESIAN_POINT('Ctrl Pts',(42.4793959719044,46.5961652188794,6.00531616599059E-17));
#40595=CARTESIAN_POINT('Ctrl Pts',(42.4996894082884,46.6687334385816,-3.21939151686953E-16));
#40596=CARTESIAN_POINT('Ctrl Pts',(42.5221838062526,46.7406870735208,-2.77555756156289E-16));
#40597=CARTESIAN_POINT('Ctrl Pts',(42.5314101376854,46.7701996697149,-2.59351405102697E-16));
#40598=CARTESIAN_POINT('Ctrl Pts',(42.5410068236004,46.7996087909298,-9.55235496976607E-16));
#40599=CARTESIAN_POINT('Ctrl Pts',(42.5509740049686,46.8289053625447,-9.99200722162641E-16));
#40600=CARTESIAN_POINT('Ctrl Pts',(42.5570607607216,46.8467961853593,-1.02604939456517E-15));
#40601=CARTESIAN_POINT('Ctrl Pts',(42.5632829918888,46.8646370330611,-8.8363779498305E-16));
#40602=CARTESIAN_POINT('Ctrl Pts',(42.5696388615209,46.8824218237155,-8.32667268468867E-16));
#40603=CARTESIAN_POINT('Ctrl Pts',(42.6078192628296,46.9892569987086,-5.2648176280675E-16));
#40604=CARTESIAN_POINT('Ctrl Pts',(42.6508353549956,47.0941210422799,-1.56418195276785E-15));
#40605=CARTESIAN_POINT('Ctrl Pts',(42.6986278307943,47.1966030771671,-1.38777878078145E-15));
#40606=CARTESIAN_POINT('Ctrl Pts',(42.737019496892,47.2789268320815,-1.24607422239025E-15));
#40607=CARTESIAN_POINT('Ctrl Pts',(42.7784942288083,47.3597131960483,-4.31564916260592E-16));
#40608=CARTESIAN_POINT('Ctrl Pts',(42.8230399677098,47.4387323947075,-2.22044604925031E-16));
#40609=CARTESIAN_POINT('Ctrl Pts',(42.845116479876,47.4778936779992,-1.18208013225659E-16));
#40610=CARTESIAN_POINT('Ctrl Pts',(42.8679475116497,47.5166206644653,-1.64609701332461E-15));
#40611=CARTESIAN_POINT('Ctrl Pts',(42.8915329771438,47.5548836868594,-1.88737914186277E-15));
#40612=CARTESIAN_POINT('Ctrl Pts',(42.9049283273751,47.5766151462621,-2.02441517437781E-15));
#40613=CARTESIAN_POINT('Ctrl Pts',(42.9185688329768,47.598199463855,-2.01487937691598E-16));
#40614=CARTESIAN_POINT('Ctrl Pts',(42.9324408350102,47.6196104178753,-2.77555756156289E-16));
#40615=CARTESIAN_POINT('Ctrl Pts',(42.990991151139,47.7099808001382,-5.9861934940153E-16));
#40616=CARTESIAN_POINT('Ctrl Pts',(43.053708488674,47.7973421754918,-3.6468209649014E-17));
#40617=CARTESIAN_POINT('Ctrl Pts',(43.1205609304308,47.8813134312875,-1.11022302462516E-16));
#40618=CARTESIAN_POINT('Ctrl Pts',(43.1787978512499,47.9544630013906,-1.75968334137956E-16));
#40619=CARTESIAN_POINT('Ctrl Pts',(43.2401733961615,48.0250397128339,-9.64438377216789E-17));
#40620=CARTESIAN_POINT('Ctrl Pts',(43.3046859799344,48.0927658552249,5.55111512312578E-16));
#40621=CARTESIAN_POINT('Ctrl Pts',(43.342705354392,48.1326790848235,9.39711714460504E-16));
#40622=CARTESIAN_POINT('Ctrl Pts',(43.3818146654666,48.1716017370957,-1.4559310714997E-16));
#40623=CARTESIAN_POINT('Ctrl Pts',(43.4219648396841,48.2095124983745,-1.11022302462516E-16));
#40624=CARTESIAN_POINT('Origin',(46.,46.,-5.));
#40625=CARTESIAN_POINT('Origin',(-46.,46.,-9.));
#40626=CARTESIAN_POINT('Ctrl Pts',(-44.696617959125,49.1291532909119,-9.));
#40627=CARTESIAN_POINT('Ctrl Pts',(-44.7904996223388,49.1799520140265,-9.));
#40628=CARTESIAN_POINT('Ctrl Pts',(-44.8867385915556,49.2258395047784,-9.));
#40629=CARTESIAN_POINT('Ctrl Pts',(-44.9849436714741,49.2669286477321,-9.));
#40630=CARTESIAN_POINT('Ctrl Pts',(-45.0854080385689,49.3089630796041,-9.));
#40631=CARTESIAN_POINT('Ctrl Pts',(-45.1879305957063,49.3459761067654,-9.));
#40632=CARTESIAN_POINT('Ctrl Pts',(-45.2921271097238,49.3780462975193,-9.));
#40633=CARTESIAN_POINT('Ctrl Pts',(-45.3228377156123,49.3874985810078,-9.));
#40634=CARTESIAN_POINT('Ctrl Pts',(-45.3536939301342,49.3965211911857,-8.99999999999999));
#40635=CARTESIAN_POINT('Ctrl Pts',(-45.3846863526263,49.4051154095944,-8.99999999999999));
#40636=CARTESIAN_POINT('Ctrl Pts',(-45.4054444996056,49.4108716569141,-8.99999999999999));
#40637=CARTESIAN_POINT('Ctrl Pts',(-45.4262637541538,49.4164357177448,-9.));
#40638=CARTESIAN_POINT('Ctrl Pts',(-45.4471413315095,49.4218078922329,-9.));
#40639=CARTESIAN_POINT('Ctrl Pts',(-45.4677336090854,49.4271066539791,-9.));
#40640=CARTESIAN_POINT('Ctrl Pts',(-45.4883751049533,49.4322167664951,-9.));
#40641=CARTESIAN_POINT('Ctrl Pts',(-45.5090574073606,49.4371376256381,-9.));
#40642=CARTESIAN_POINT('Ctrl Pts',(-45.6183975459561,49.4631524962317,-9.));
#40643=CARTESIAN_POINT('Ctrl Pts',(-45.7289242899367,49.4838942050191,-9.));
#40644=CARTESIAN_POINT('Ctrl Pts',(-45.8402230421101,49.4994553459788,-9.));
#40645=CARTESIAN_POINT('Ctrl Pts',(-45.9357755114348,49.5128149337116,-9.));
#40646=CARTESIAN_POINT('Ctrl Pts',(-46.0318978588596,49.5223554338441,-9.));
#40647=CARTESIAN_POINT('Ctrl Pts',(-46.1283415311861,49.528107995161,-9.));
#40648=CARTESIAN_POINT('Ctrl Pts',(-46.1610023378608,49.530056109418,-9.));
#40649=CARTESIAN_POINT('Ctrl Pts',(-46.1937000754335,49.5315695862222,-9.));
#40650=CARTESIAN_POINT('Ctrl Pts',(-46.2264252947816,49.532648960474,-9.));
#40651=CARTESIAN_POINT('Ctrl Pts',(-46.2453984913202,49.5332747524542,-9.));
#40652=CARTESIAN_POINT('Ctrl Pts',(-46.2643830050267,49.5337546547774,-9.));
#40653=CARTESIAN_POINT('Ctrl Pts',(-46.2833703759129,49.5340886078599,-9.));
#40654=CARTESIAN_POINT('Ctrl Pts',(-46.3983320105817,49.5361105724853,-9.));
#40655=CARTESIAN_POINT('Ctrl Pts',(-46.5131368120173,49.5327826867357,-9.));
#40656=CARTESIAN_POINT('Ctrl Pts',(-46.6273658142106,49.5242071685151,-9.));
#40657=CARTESIAN_POINT('Ctrl Pts',(-46.743194097363,49.5155115874144,-9.));
#40658=CARTESIAN_POINT('Ctrl Pts',(-46.8584311883117,49.5014205980068,-9.));
#40659=CARTESIAN_POINT('Ctrl Pts',(-46.9726597700209,49.4819911111919,-9.));
#40660=CARTESIAN_POINT('Ctrl Pts',(-47.0865466693785,49.4626197421671,-9.));
#40661=CARTESIAN_POINT('Ctrl Pts',(-47.1994319983269,49.4379418269772,-9.));
#40662=CARTESIAN_POINT('Ctrl Pts',(-47.3109081125593,49.4079630393852,-9.));
#40663=CARTESIAN_POINT('Ctrl Pts',(-47.377437977202,49.3900714516277,-9.));
#40664=CARTESIAN_POINT('Ctrl Pts',(-47.4434659580683,49.3702908251682,-9.));
#40665=CARTESIAN_POINT('Ctrl Pts',(-47.5089043530615,49.3486135658251,-9.));
#40666=CARTESIAN_POINT('Ctrl Pts',(-47.5540027434167,49.3336741788828,-9.));
#40667=CARTESIAN_POINT('Ctrl Pts',(-47.5988210839709,49.3178338306162,-9.));
#40668=CARTESIAN_POINT('Ctrl Pts',(-47.6433301230227,49.3010881819055,-9.));
#40669=CARTESIAN_POINT('Ctrl Pts',(-47.6570954003034,49.2959092676296,-9.));
#40670=CARTESIAN_POINT('Ctrl Pts',(-47.6708285427968,49.2906446729309,-9.));
#40671=CARTESIAN_POINT('Ctrl Pts',(-47.6845208156298,49.2852975315791,-9.));
#40672=CARTESIAN_POINT('Ctrl Pts',(-47.7954797276198,49.24196557392,-9.));
#40673=CARTESIAN_POINT('Ctrl Pts',(-47.9039056143507,49.1931603257822,-9.));
#40674=CARTESIAN_POINT('Ctrl Pts',(-48.0093711136693,49.1389414929264,-9.));
#40675=CARTESIAN_POINT('Ctrl Pts',(-48.0319908991973,49.1273128714464,-9.));
#40676=CARTESIAN_POINT('Ctrl Pts',(-48.0544745179869,49.1154350357187,-9.));
#40677=CARTESIAN_POINT('Ctrl Pts',(-48.0768177548194,49.1033082620402,-9.));
#40678=CARTESIAN_POINT('Ctrl Pts',(-48.1769673925503,49.0489521273469,-9.));
#40679=CARTESIAN_POINT('Ctrl Pts',(-48.2742977574197,48.9895986568041,-9.));
#40680=CARTESIAN_POINT('Ctrl Pts',(-48.3686684964881,48.9256373054214,-9.));
#40681=CARTESIAN_POINT('Ctrl Pts',(-48.4650755230169,48.8602958260555,-9.));
#40682=CARTESIAN_POINT('Ctrl Pts',(-48.5583943777551,48.7901450832442,-9.));
#40683=CARTESIAN_POINT('Ctrl Pts',(-48.6484556272283,48.7155495224137,-9.));
#40684=CARTESIAN_POINT('Ctrl Pts',(-48.6989531510327,48.6737236413519,-9.));
#40685=CARTESIAN_POINT('Ctrl Pts',(-48.7484261266963,48.6304994944732,-9.));
#40686=CARTESIAN_POINT('Ctrl Pts',(-48.7968410318596,48.585935306637,-9.));
#40687=CARTESIAN_POINT('Ctrl Pts',(-48.8170290143165,48.5673529911454,-9.));
#40688=CARTESIAN_POINT('Ctrl Pts',(-48.8370329936549,48.5485376335577,-9.));
#40689=CARTESIAN_POINT('Ctrl Pts',(-48.8568503809651,48.5294932599232,-9.));
#40690=CARTESIAN_POINT('Ctrl Pts',(-48.8675819585321,48.5191802872961,-9.));
#40691=CARTESIAN_POINT('Ctrl Pts',(-48.878257268696,48.5088015935768,-9.));
#40692=CARTESIAN_POINT('Ctrl Pts',(-48.8888695308225,48.4983643075092,-9.));
#40693=CARTESIAN_POINT('Ctrl Pts',(-48.9743487820228,48.4142944469096,-9.));
#40694=CARTESIAN_POINT('Ctrl Pts',(-49.0558593342174,48.3263122954055,-9.));
#40695=CARTESIAN_POINT('Ctrl Pts',(-49.1332547753371,48.2348504026783,-9.));
#40696=CARTESIAN_POINT('Ctrl Pts',(-49.2120696940868,48.1417110453766,-9.));
#40697=CARTESIAN_POINT('Ctrl Pts',(-49.2866177625613,48.0449626295991,-9.00000000000001));
#40698=CARTESIAN_POINT('Ctrl Pts',(-49.3567204749084,47.9450119046275,-9.00000000000001));
#40699=CARTESIAN_POINT('Ctrl Pts',(-49.4273913584228,47.8442510951645,-9.00000000000001));
#40700=CARTESIAN_POINT('Ctrl Pts',(-49.4935451434678,47.7402352153407,-9.));
#40701=CARTESIAN_POINT('Ctrl Pts',(-49.5549658356322,47.6333394412306,-9.));
#40702=CARTESIAN_POINT('Ctrl Pts',(-49.5912290899789,47.5702273448256,-9.));
#40703=CARTESIAN_POINT('Ctrl Pts',(-49.6258418069011,47.506110632588,-9.));
#40704=CARTESIAN_POINT('Ctrl Pts',(-49.6587528506667,47.4410612184224,-9.));
#40705=CARTESIAN_POINT('Ctrl Pts',(-49.6760927446588,47.4067885300837,-9.));
#40706=CARTESIAN_POINT('Ctrl Pts',(-49.6929601759713,47.3722568712257,-9.));
#40707=CARTESIAN_POINT('Ctrl Pts',(-49.7093470352523,47.3374764129113,-9.));
#40708=CARTESIAN_POINT('Ctrl Pts',(-49.7168953641755,47.3214553844182,-9.));
#40709=CARTESIAN_POINT('Ctrl Pts',(-49.7243424653822,47.3053799171024,-9.));
#40710=CARTESIAN_POINT('Ctrl Pts',(-49.7316851545068,47.2892561784676,-9.));
#40711=CARTESIAN_POINT('Ctrl Pts',(-49.7841011013623,47.1741565176969,-9.));
#40712=CARTESIAN_POINT('Ctrl Pts',(-49.8310349508625,47.0569637809862,-9.));
#40713=CARTESIAN_POINT('Ctrl Pts',(-49.8723057500299,46.938105693547,-9.));
#40714=CARTESIAN_POINT('Ctrl Pts',(-49.9136563789374,46.8190176999652,-9.));
#40715=CARTESIAN_POINT('Ctrl Pts',(-49.9493226072422,46.6982571648312,-9.));
#40716=CARTESIAN_POINT('Ctrl Pts',(-49.9790844956097,46.5762183008083,-9.));
#40717=CARTESIAN_POINT('Ctrl Pts',(-50.0083336073707,46.4562820814085,-9.));
#40718=CARTESIAN_POINT('Ctrl Pts',(-50.0318805036137,46.335110417964,-9.));
#40719=CARTESIAN_POINT('Ctrl Pts',(-50.049472608,46.2130542301493,-9.));
#40720=CARTESIAN_POINT('Ctrl Pts',(-50.060364521469,46.1374847924716,-9.));
#40721=CARTESIAN_POINT('Ctrl Pts',(-50.0689728987746,46.0615758765585,-9.));
#40722=CARTESIAN_POINT('Ctrl Pts',(-50.0752280523108,45.9854081433151,-9.));
#40723=CARTESIAN_POINT('Ctrl Pts',(-50.0806294959961,45.9196358614081,-9.));
#40724=CARTESIAN_POINT('Ctrl Pts',(-50.0842760830383,45.8536705349028,-9.));
#40725=CARTESIAN_POINT('Ctrl Pts',(-50.0861963379778,45.7875630405759,-9.));
#40726=CARTESIAN_POINT('Ctrl Pts',(-49.4256147683784,43.7746037524369,-9.));
#40727=CARTESIAN_POINT('Ctrl Pts',(-49.3489156851343,43.6758334442189,-9.));
#40728=CARTESIAN_POINT('Ctrl Pts',(-49.2674578564169,43.5810567995784,-9.));
#40729=CARTESIAN_POINT('Ctrl Pts',(-49.181649129582,43.490413103789,-9.));
#40730=CARTESIAN_POINT('Ctrl Pts',(-49.0946355246868,43.3984966400144,-9.));
#40731=CARTESIAN_POINT('Ctrl Pts',(-49.0031471845609,43.3108296011929,-9.00000000000001));
#40732=CARTESIAN_POINT('Ctrl Pts',(-48.9075792861019,43.2276011445689,-9.));
#40733=CARTESIAN_POINT('Ctrl Pts',(-48.8671606571012,43.1924012483188,-9.));
#40734=CARTESIAN_POINT('Ctrl Pts',(-48.8260120201089,43.157995852241,-9.));
#40735=CARTESIAN_POINT('Ctrl Pts',(-48.7841622188313,43.124401852238,-9.));
#40736=CARTESIAN_POINT('Ctrl Pts',(-48.7601537028534,43.1051295483988,-9.));
#40737=CARTESIAN_POINT('Ctrl Pts',(-48.7359099990676,43.0861210782675,-9.));
#40738=CARTESIAN_POINT('Ctrl Pts',(-48.711461905359,43.0673988919303,-9.));
#40739=CARTESIAN_POINT('Ctrl Pts',(-48.6120353794127,42.9912587246101,-9.));
#40740=CARTESIAN_POINT('Ctrl Pts',(-48.5091652266986,42.9197949105889,-9.));
#40741=CARTESIAN_POINT('Ctrl Pts',(-48.403244860894,42.8531794238142,-9.));
#40742=CARTESIAN_POINT('Ctrl Pts',(-48.3152213037729,42.7978196064578,-9.));
#40743=CARTESIAN_POINT('Ctrl Pts',(-48.2250904620759,42.7458088667081,-9.));
#40744=CARTESIAN_POINT('Ctrl Pts',(-48.1330695305898,42.6972719088762,-9.));
#40745=CARTESIAN_POINT('Ctrl Pts',(-48.0928103730647,42.6760369898247,-9.));
#40746=CARTESIAN_POINT('Ctrl Pts',(-48.0521893744864,42.655467290417,-9.));
#40747=CARTESIAN_POINT('Ctrl Pts',(-48.0112245259672,42.6355747667283,-9.));
#40748=CARTESIAN_POINT('Ctrl Pts',(-47.988854995164,42.6247121262574,-9.));
#40749=CARTESIAN_POINT('Ctrl Pts',(-47.9663829311551,42.6140514282838,-9.));
#40750=CARTESIAN_POINT('Ctrl Pts',(-47.943811261034,42.6035947399501,-9.));
#40751=CARTESIAN_POINT('Ctrl Pts',(-47.9276114508231,42.5960899179529,-9.));
#40752=CARTESIAN_POINT('Ctrl Pts',(-47.9113688772611,42.5886941448197,-9.));
#40753=CARTESIAN_POINT('Ctrl Pts',(-47.8950854098512,42.5814081483561,-9.));
#40754=CARTESIAN_POINT('Ctrl Pts',(-47.783364187915,42.5314187691019,-9.));
#40755=CARTESIAN_POINT('Ctrl Pts',(-47.6697083738472,42.4865878815946,-9.));
#40756=CARTESIAN_POINT('Ctrl Pts',(-47.5544847720591,42.4470736397854,-9.));
#40757=CARTESIAN_POINT('Ctrl Pts',(-47.4401244943331,42.4078554622826,-9.));
#40758=CARTESIAN_POINT('Ctrl Pts',(-47.3242190140508,42.373874375732,-9.));
#40759=CARTESIAN_POINT('Ctrl Pts',(-47.2071179764348,42.3453353099349,-9.));
#40760=CARTESIAN_POINT('Ctrl Pts',(-47.0931610163015,42.3175624972469,-9.));
#40761=CARTESIAN_POINT('Ctrl Pts',(-46.9780711398153,42.2949434018992,-9.));
#40762=CARTESIAN_POINT('Ctrl Pts',(-46.8621731460597,42.2777157561986,-9.));
#40763=CARTESIAN_POINT('Ctrl Pts',(-46.7940396442691,42.2675880586332,-9.));
#40764=CARTESIAN_POINT('Ctrl Pts',(-46.7256269603666,42.2593245531098,-9.));
#40765=CARTESIAN_POINT('Ctrl Pts',(-46.6570029378699,42.252981774315,-9.));
#40766=CARTESIAN_POINT('Ctrl Pts',(-46.6091492630523,42.2485587565022,-9.));
#40767=CARTESIAN_POINT('Ctrl Pts',(-46.5611928515148,42.2450698598449,-9.));
#40768=CARTESIAN_POINT('Ctrl Pts',(-46.5131573311611,42.2425360831896,-9.));
#40769=CARTESIAN_POINT('Ctrl Pts',(-46.4976790891648,42.2417196371941,-9.));
#40770=CARTESIAN_POINT('Ctrl Pts',(-46.48219606998,42.2410025896726,-9.));
#40771=CARTESIAN_POINT('Ctrl Pts',(-46.4667175316418,42.2403857716101,-9.));
#40772=CARTESIAN_POINT('Ctrl Pts',(-46.3509701417906,42.2357732507639,-9.));
#40773=CARTESIAN_POINT('Ctrl Pts',(-46.2353324238638,42.2367536523897,-9.));
#40774=CARTESIAN_POINT('Ctrl Pts',(-46.1201180919468,42.243510424435,-9.));
#40775=CARTESIAN_POINT('Ctrl Pts',(-46.0928482837347,42.2451096688584,-9.));
#40776=CARTESIAN_POINT('Ctrl Pts',(-46.0656022142227,42.2470327395972,-9.));
#40777=CARTESIAN_POINT('Ctrl Pts',(-46.0383840979687,42.2492824979304,-9.));
#40778=CARTESIAN_POINT('Ctrl Pts',(-45.9217097098913,42.2589264120937,-9.));
#40779=CARTESIAN_POINT('Ctrl Pts',(-45.8055476026248,42.2745693849197,-9.));
#40780=CARTESIAN_POINT('Ctrl Pts',(-45.6902605716738,42.2959681457642,-9.));
#40781=CARTESIAN_POINT('Ctrl Pts',(-45.5740232449465,42.3175432937693,-9.));
#40782=CARTESIAN_POINT('Ctrl Pts',(-45.4586746610144,42.344970033424,-9.));
#40783=CARTESIAN_POINT('Ctrl Pts',(-45.3446113258486,42.3780453905501,-9.));
#40784=CARTESIAN_POINT('Ctrl Pts',(-45.2880066971767,42.3944592390983,-9.));
#40785=CARTESIAN_POINT('Ctrl Pts',(-45.2317190441744,42.4122648380503,-9.));
#40786=CARTESIAN_POINT('Ctrl Pts',(-45.1758000085569,42.4314409547508,-9.));
#40787=CARTESIAN_POINT('Ctrl Pts',(-45.1531794291222,42.4391981498863,-9.));
#40788=CARTESIAN_POINT('Ctrl Pts',(-45.1306191973553,42.4471796404986,-9.));
#40789=CARTESIAN_POINT('Ctrl Pts',(-45.108122848517,42.4553841175605,-9.));
#40790=CARTESIAN_POINT('Ctrl Pts',(-45.0929026543741,42.4609349620386,-9.));
#40791=CARTESIAN_POINT('Ctrl Pts',(-45.077712071619,42.4665878060077,-9.));
#40792=CARTESIAN_POINT('Ctrl Pts',(-45.0625649705552,42.4723372085153,-9.));
#40793=CARTESIAN_POINT('Ctrl Pts',(-44.9541043446988,42.5135057325545,-9.));
#40794=CARTESIAN_POINT('Ctrl Pts',(-44.8477009223801,42.5596824806258,-9.));
#40795=CARTESIAN_POINT('Ctrl Pts',(-44.7436965702623,42.6106187568676,-9.));
#40796=CARTESIAN_POINT('Ctrl Pts',(-44.63979376496,42.6615053004152,-9.));
#40797=CARTESIAN_POINT('Ctrl Pts',(-44.5382846082116,42.7171426900045,-9.));
#40798=CARTESIAN_POINT('Ctrl Pts',(-44.4395391052149,42.7773258218427,-9.));
#40799=CARTESIAN_POINT('Ctrl Pts',(-44.3421856021374,42.8366605614795,-9.));
#40800=CARTESIAN_POINT('Ctrl Pts',(-44.2475177836353,42.9004144122074,-9.));
#40801=CARTESIAN_POINT('Ctrl Pts',(-44.1559283796025,42.9684232317984,-9.));
#40802=CARTESIAN_POINT('Ctrl Pts',(-44.1056662078478,43.0057449177206,-9.));
#40803=CARTESIAN_POINT('Ctrl Pts',(-44.0563318447938,43.0443485309563,-9.));
#40804=CARTESIAN_POINT('Ctrl Pts',(-44.007996167856,43.0842101741848,-9.));
#40805=CARTESIAN_POINT('Ctrl Pts',(-43.9809731477155,43.1064956174855,-9.));
#40806=CARTESIAN_POINT('Ctrl Pts',(-43.9542623568393,43.1291743065356,-9.));
#40807=CARTESIAN_POINT('Ctrl Pts',(-43.9278768328444,43.1522423177272,-9.));
#40808=CARTESIAN_POINT('Ctrl Pts',(-43.9114600205802,43.1665950063119,-9.));
#40809=CARTESIAN_POINT('Ctrl Pts',(-43.8951656324309,43.1811017137048,-9.));
#40810=CARTESIAN_POINT('Ctrl Pts',(-43.8790187657196,43.195741331518,-9.));
#40811=CARTESIAN_POINT('Ctrl Pts',(-43.7964028050777,43.2706454049021,-9.));
#40812=CARTESIAN_POINT('Ctrl Pts',(-43.7175427311938,43.3491132482605,-9.));
#40813=CARTESIAN_POINT('Ctrl Pts',(-43.642772806583,43.4309575041822,-9.));
#40814=CARTESIAN_POINT('Ctrl Pts',(-43.5691145212186,43.5115849434834,-9.));
#40815=CARTESIAN_POINT('Ctrl Pts',(-43.4994251726958,43.5954897325599,-9.));
#40816=CARTESIAN_POINT('Ctrl Pts',(-43.4340666403476,43.6825192687086,-9.));
#40817=CARTESIAN_POINT('Ctrl Pts',(-43.3705939763842,43.7670376369213,-9.));
#40818=CARTESIAN_POINT('Ctrl Pts',(-43.3112055155065,43.854503559686,-9.));
#40819=CARTESIAN_POINT('Ctrl Pts',(-43.2562784669833,43.9447942667368,-9.));
#40820=CARTESIAN_POINT('Ctrl Pts',(-43.2286242788146,43.9902530392324,-9.));
#40821=CARTESIAN_POINT('Ctrl Pts',(-43.2021017428087,44.036428070575,-9.));
#40822=CARTESIAN_POINT('Ctrl Pts',(-43.176763938175,44.0833047759387,-9.));
#40823=CARTESIAN_POINT('Ctrl Pts',(-43.1505637145409,44.1317770165891,-9.00000000000001));
#40824=CARTESIAN_POINT('Ctrl Pts',(-43.1256303008689,44.1809995875891,-9.));
#40825=CARTESIAN_POINT('Ctrl Pts',(-43.1019723047815,44.2309203707047,-9.));
#40826=CARTESIAN_POINT('Origin',(-46.,46.,2.76038497140452));
#40827=CARTESIAN_POINT('Ctrl Pts',(-50.0901569545599,46.0018621213198,-0.364615028595479));
#40828=CARTESIAN_POINT('Ctrl Pts',(-50.0908670066917,46.1207444808691,-0.370425837919348));
#40829=CARTESIAN_POINT('Ctrl Pts',(-50.0327398704972,47.5746590118461,-0.441524166511649));
#40830=CARTESIAN_POINT('Ctrl Pts',(-48.2991248954935,50.2221780497669,-0.577910014372381));
#40831=CARTESIAN_POINT('Ctrl Pts',(-43.7551468972239,50.2508324710758,-0.773772572177673));
#40832=CARTESIAN_POINT('Ctrl Pts',(-41.216941413185,46.4820553508686,-0.969635129982968));
#40833=CARTESIAN_POINT('Ctrl Pts',(-42.9521748839983,42.2823237877054,-1.16549768778826));
#40834=CARTESIAN_POINT('Ctrl Pts',(-47.4105428653624,41.4043187587238,-1.36136024559355));
#40835=CARTESIAN_POINT('Ctrl Pts',(-49.8549759634627,43.8716102112686,-1.51106602586263));
#40836=CARTESIAN_POINT('Ctrl Pts',(-50.0859938031716,45.6034148261523,-1.59548428686327));
#40837=CARTESIAN_POINT('Ctrl Pts',(-50.0828667635534,45.9966889209644,-1.61461502859548));
#40838=CARTESIAN_POINT('Ctrl Pts',(-50.0805800719598,45.9961676961768,-0.260384971404518));
#40839=CARTESIAN_POINT('Ctrl Pts',(-50.074537021219,46.8968546972385,-0.304165019473208));
#40840=CARTESIAN_POINT('Ctrl Pts',(-49.3426925538961,49.1524151445276,-0.413232586810328));
#40841=CARTESIAN_POINT('Ctrl Pts',(-45.6441921094362,50.7932694144525,-0.587587673415879));
#40842=CARTESIAN_POINT('Ctrl Pts',(-41.8104748163565,48.3572313450219,-0.783450231221174));
#40843=CARTESIAN_POINT('Ctrl Pts',(-41.7184176569125,43.8134905867626,-0.979312789026467));
#40844=CARTESIAN_POINT('Ctrl Pts',(-45.4525333012251,41.2240979371497,-1.17517534683176));
#40845=CARTESIAN_POINT('Ctrl Pts',(-49.2692586484769,42.740078891428,-1.35219940762444));
#40846=CARTESIAN_POINT('Ctrl Pts',(-50.0753332382032,45.0485594015793,-1.4639359491487));
#40847=CARTESIAN_POINT('Ctrl Pts',(-50.0830244466748,46.0033346430494,-1.51038497140452));
#40848=CARTESIAN_POINT('Ctrl Pts',(-43.4267655729853,48.2065515280923,0.));
#40849=CARTESIAN_POINT('Ctrl Pts',(-42.7026396483563,47.3620909591791,-0.0652875192684312));
#40850=CARTESIAN_POINT('Ctrl Pts',(-42.1622053861818,44.918494548316,-0.195862557805293));
#40851=CARTESIAN_POINT('Ctrl Pts',(-44.780472506665,42.1996731612585,-0.391725115610587));
#40852=CARTESIAN_POINT('Ctrl Pts',(-48.4895452540558,42.8839744308764,-0.58758767341588));
#40853=CARTESIAN_POINT('Ctrl Pts',(-49.9737285271075,46.3485994374708,-0.783450231221174));
#40854=CARTESIAN_POINT('Ctrl Pts',(-47.9078234062422,49.5035809165722,-0.979312789026467));
#40855=CARTESIAN_POINT('Ctrl Pts',(-44.1372115532105,49.5273584746216,-1.17517534683176));
#40856=CARTESIAN_POINT('Ctrl Pts',(-42.0309980796435,46.4000115362563,-1.37103790463705));
#40857=CARTESIAN_POINT('Ctrl Pts',(-43.4709020350142,42.9150568076804,-1.56690046244235));
#40858=CARTESIAN_POINT('Ctrl Pts',(-47.170474339746,42.186484580755,-1.76276302024764));
#40859=CARTESIAN_POINT('Ctrl Pts',(-49.8242647271257,44.8650910620353,-1.95862557805294));
#40860=CARTESIAN_POINT('Ctrl Pts',(-49.0612252674608,48.5577200654077,-2.15448813585823));
#40861=CARTESIAN_POINT('Ctrl Pts',(-45.5630965935586,49.9651121437844,-2.35035069366352));
#40862=CARTESIAN_POINT('Ctrl Pts',(-42.4553252853163,47.8298346642785,-2.54621325146881));
#40863=CARTESIAN_POINT('Ctrl Pts',(-42.5145843401837,44.0596672136162,-2.74207580927411));
#40864=CARTESIAN_POINT('Ctrl Pts',(-45.6879287513146,42.0231140731554,-2.9379383670794));
#40865=CARTESIAN_POINT('Ctrl Pts',(-49.1400967366528,43.5397551864917,-3.1338009248847));
#40866=CARTESIAN_POINT('Ctrl Pts',(-49.7867088499387,47.2545309657486,-3.32966348268999));
#40867=CARTESIAN_POINT('Ctrl Pts',(-47.0500419029285,49.848431304961,-3.52552604049528));
#40868=CARTESIAN_POINT('Ctrl Pts',(-43.3752028262867,49.0039060474354,-3.72138859830057));
#40869=CARTESIAN_POINT('Ctrl Pts',(-42.0455192855114,45.4755059780424,-3.91725115610587));
#40870=CARTESIAN_POINT('Ctrl Pts',(-44.2490125041704,42.4157212082961,-4.11311371391116));
#40871=CARTESIAN_POINT('Ctrl Pts',(-48.0169458506302,42.5583519744937,-4.30897627171646));
#40872=CARTESIAN_POINT('Ctrl Pts',(-49.9828154853804,45.7759631753024,-4.50483882952175));
#40873=CARTESIAN_POINT('Ctrl Pts',(-48.3901923325963,49.1937426785204,-4.70070138732704));
#40874=CARTESIAN_POINT('Ctrl Pts',(-44.662024060862,49.7580356671663,-4.89656394513234));
#40875=CARTESIAN_POINT('Ctrl Pts',(-42.1292859407132,46.9646680087392,-5.09242650293763));
#40876=CARTESIAN_POINT('Ctrl Pts',(-43.0548822895087,43.3094065081176,-5.28828906074292));
#40877=CARTESIAN_POINT('Ctrl Pts',(-46.6118282782839,42.0580870306127,-5.48415161854822));
#40878=CARTESIAN_POINT('Ctrl Pts',(-49.6221291986836,44.3287155200276,-5.68001417635351));
#40879=CARTESIAN_POINT('Ctrl Pts',(-49.3961966506987,48.0925725355867,-5.87587673415881));
#40880=CARTESIAN_POINT('Ctrl Pts',(-46.1358928070669,49.9867963332999,-6.0717392919641));
#40881=CARTESIAN_POINT('Ctrl Pts',(-42.7541738021461,48.3189705369532,-6.2676018497694));
#40882=CARTESIAN_POINT('Ctrl Pts',(-42.2724762525193,44.5792337098036,-6.46346440757469));
#40883=CARTESIAN_POINT('Ctrl Pts',(-45.1211774786945,42.1088967349022,-6.65932696537998));
#40884=CARTESIAN_POINT('Ctrl Pts',(-48.7550742096251,43.1151118165565,-6.85518952318527));
#40885=CARTESIAN_POINT('Ctrl Pts',(-49.9274151919628,46.6988625110037,-7.05105208099057));
#40886=CARTESIAN_POINT('Ctrl Pts',(-47.5907668890102,49.658208957394,-7.24691463879586));
#40887=CARTESIAN_POINT('Ctrl Pts',(-43.8328182515428,49.3490808096796,-7.44277719660115));
#40888=CARTESIAN_POINT('Ctrl Pts',(-42.0111861586986,46.0476882822715,-7.63863975440645));
#40889=CARTESIAN_POINT('Ctrl Pts',(-43.7533595145448,42.7036660446114,-7.83450231221174));
#40890=CARTESIAN_POINT('Ctrl Pts',(-47.5029152312013,42.3048367721094,-8.03036487001704));
#40891=CARTESIAN_POINT('Ctrl Pts',(-49.9094791054614,45.2074019114722,-8.22622742782233));
#40892=CARTESIAN_POINT('Ctrl Pts',(-48.8234714323549,48.8183112778844,-8.42208998562762));
#40893=CARTESIAN_POINT('Ctrl Pts',(-45.2139870282641,49.9107829885096,-8.61795254343291));
#40894=CARTESIAN_POINT('Ctrl Pts',(-42.3084375115684,47.5099063922733,-8.81381510123821));
#40895=CARTESIAN_POINT('Ctrl Pts',(-42.6977455577746,43.7583829526296,-9.00967765904351));
#40896=CARTESIAN_POINT('Ctrl Pts',(-46.0445165417033,42.0129785782631,-9.20554021684879));
#40897=CARTESIAN_POINT('Ctrl Pts',(-48.2365749371353,43.2205019121706,-9.33611525538566));
#40898=CARTESIAN_POINT('Ctrl Pts',(-48.8425893907247,44.1533569326372,-9.40140277465409));
#40899=CARTESIAN_POINT('Ctrl Pts',(-43.2508390065835,48.3574087643591,0.133800924884696));
#40900=CARTESIAN_POINT('Ctrl Pts',(-42.4772061321698,47.4552142218946,0.0685134056162645));
#40901=CARTESIAN_POINT('Ctrl Pts',(-41.8998235285957,44.8445543201494,-0.0620616329205977));
#40902=CARTESIAN_POINT('Ctrl Pts',(-44.6970960049819,41.9398528957881,-0.257924190725891));
#40903=CARTESIAN_POINT('Ctrl Pts',(-48.6597501696476,42.6709383882054,-0.453786748531184));
#40904=CARTESIAN_POINT('Ctrl Pts',(-50.245403897314,46.3724324397966,-0.649649306336479));
#40905=CARTESIAN_POINT('Ctrl Pts',(-48.0382572359926,49.7431132943038,-0.845511864141771));
#40906=CARTESIAN_POINT('Ctrl Pts',(-44.0098566678816,49.7685164734396,-1.04137442194707));
#40907=CARTESIAN_POINT('Ctrl Pts',(-41.7596458574907,46.4273594744604,-1.23723697975236));
#40908=CARTESIAN_POINT('Ctrl Pts',(-43.2979929846756,42.7041458010221,-1.43309953755765));
#40909=CARTESIAN_POINT('Ctrl Pts',(-47.2504971816181,41.9257626400779,-1.62896209536295));
#40910=CARTESIAN_POINT('Ctrl Pts',(-50.0857215751267,44.7874997510615,-1.82482465316824));
#40911=CARTESIAN_POINT('Ctrl Pts',(-49.2705147300271,48.732585947894,-2.02068721097353));
#40912=CARTESIAN_POINT('Ctrl Pts',(-45.5332264366317,50.2361984301837,-2.21654976877883));
#40913=CARTESIAN_POINT('Ctrl Pts',(-42.2129834119841,47.9549365695654,-2.41241232658412));
#40914=CARTESIAN_POINT('Ctrl Pts',(-42.2762938824324,43.927010786669,-2.60827488438942));
#40915=CARTESIAN_POINT('Ctrl Pts',(-45.6665931035876,41.7512228382424,-2.80413744219471));
#40916=CARTESIAN_POINT('Ctrl Pts',(-49.3547784738662,43.3715534797197,-3.));
#40917=CARTESIAN_POINT('Ctrl Pts',(-50.0455980824701,47.3403005804141,-3.1958625578053));
#40918=CARTESIAN_POINT('Ctrl Pts',(-47.1218310351665,50.111540370504,-3.39172511561058));
#40919=CARTESIAN_POINT('Ctrl Pts',(-43.195751024529,49.2092767168044,-3.58758767341588));
#40920=CARTESIAN_POINT('Ctrl Pts',(-41.7751598473278,45.4396474369734,-3.78345023122118));
#40921=CARTESIAN_POINT('Ctrl Pts',(-44.1293012121405,42.1706716884267,-3.97931278902647));
#40922=CARTESIAN_POINT('Ctrl Pts',(-48.1548401498805,42.3230538168387,-4.17517534683176));
#40923=CARTESIAN_POINT('Ctrl Pts',(-50.2551121116026,45.7606462539591,-4.37103790463705));
#40924=CARTESIAN_POINT('Ctrl Pts',(-48.5536047001984,49.4120920747139,-4.56690046244235));
#40925=CARTESIAN_POINT('Ctrl Pts',(-44.5705494907919,50.0149645751583,-4.76276302024764));
#40926=CARTESIAN_POINT('Ctrl Pts',(-41.8646534506358,47.0306203093587,-4.95862557805294));
#40927=CARTESIAN_POINT('Ctrl Pts',(-42.8535308537372,43.125456351987,-5.15448813585823));
#40928=CARTESIAN_POINT('Ctrl Pts',(-46.6536576767624,41.7885868224394,-5.35035069366352));
#40929=CARTESIAN_POINT('Ctrl Pts',(-49.8697664703983,44.2144533537222,-5.54621325146882));
#40930=CARTESIAN_POINT('Ctrl Pts',(-49.6283873944997,48.2356372704853,-5.74207580927411));
#40931=CARTESIAN_POINT('Ctrl Pts',(-46.1451835093422,50.2593651216301,-5.9379383670794));
#40932=CARTESIAN_POINT('Ctrl Pts',(-42.532263566479,48.4775136218234,-6.1338009248847));
#40933=CARTESIAN_POINT('Ctrl Pts',(-42.0176333795999,44.4820989394656,-6.32966348268999));
#40934=CARTESIAN_POINT('Ctrl Pts',(-45.0610942515207,41.8428702781764,-6.52552604049528));
#40935=CARTESIAN_POINT('Ctrl Pts',(-48.9434327753248,42.9178781454855,-6.72138859830058));
#40936=CARTESIAN_POINT('Ctrl Pts',(-50.1959242179196,46.7466422549156,-6.91725115610587));
#40937=CARTESIAN_POINT('Ctrl Pts',(-47.6995242388231,49.9083129254967,-7.11311371391117));
#40938=CARTESIAN_POINT('Ctrl Pts',(-43.6846526433991,49.5780503436108,-7.30897627171646));
#40939=CARTESIAN_POINT('Ctrl Pts',(-41.7384794376362,46.0509486287325,-7.50483882952175));
#40940=CARTESIAN_POINT('Ctrl Pts',(-43.5997614815028,42.4783027009544,-7.70070138732705));
#40941=CARTESIAN_POINT('Ctrl Pts',(-47.6056663499655,42.0522063191074,-7.89656394513234));
#40942=CARTESIAN_POINT('Ctrl Pts',(-50.176761879321,45.1532136654315,-8.09242650293763));
#40943=CARTESIAN_POINT('Ctrl Pts',(-49.0165061707422,49.0109932274824,-8.28828906074293));
#40944=CARTESIAN_POINT('Ctrl Pts',(-45.1602489926568,50.1781549060808,-8.48415161854822));
#40945=CARTESIAN_POINT('Ctrl Pts',(-42.056053233467,47.6131354818549,-8.68001417635352));
#40946=CARTESIAN_POINT('Ctrl Pts',(-42.4719774430211,43.6051283613683,-8.8758767341588));
#40947=CARTESIAN_POINT('Ctrl Pts',(-46.0475600430057,41.7403944011151,-9.0717392919641));
#40948=CARTESIAN_POINT('Ctrl Pts',(-48.3894848100407,43.0304735378497,-9.20231433050096));
#40949=CARTESIAN_POINT('Ctrl Pts',(-49.036931183276,44.0271058725704,-9.2676018497694));
#40950=CARTESIAN_POINT('Ctrl Pts',(-43.0749124401816,48.5082660006259,0.267601849769391));
#40951=CARTESIAN_POINT('Ctrl Pts',(-42.2517726159832,47.54833748461,0.20231433050096));
#40952=CARTESIAN_POINT('Ctrl Pts',(-41.6374416710097,44.7706140919828,0.0717392919640979));
#40953=CARTESIAN_POINT('Ctrl Pts',(-44.6137195032988,41.6800326303177,-0.124123265841196));
#40954=CARTESIAN_POINT('Ctrl Pts',(-48.8299550852394,42.4579023455342,-0.319985823646489));
#40955=CARTESIAN_POINT('Ctrl Pts',(-50.5170792675203,46.3962654421224,-0.515848381451782));
#40956=CARTESIAN_POINT('Ctrl Pts',(-48.1686910657431,49.9826456720353,-0.711710939257076));
#40957=CARTESIAN_POINT('Ctrl Pts',(-43.8825017825528,50.0096744722577,-0.907573497062369));
#40958=CARTESIAN_POINT('Ctrl Pts',(-41.4882936353378,46.4547074126645,-1.10343605486766));
#40959=CARTESIAN_POINT('Ctrl Pts',(-43.1250839343369,42.4932347943637,-1.29929861267296));
#40960=CARTESIAN_POINT('Ctrl Pts',(-47.3305200234903,41.6650406994009,-1.49516117047825));
#40961=CARTESIAN_POINT('Ctrl Pts',(-50.3471784231277,44.7099084400878,-1.69102372828354));
#40962=CARTESIAN_POINT('Ctrl Pts',(-49.4798041925933,48.9074518303804,-1.88688628608884));
#40963=CARTESIAN_POINT('Ctrl Pts',(-45.5033562797049,50.507284716583,-2.08274884389413));
#40964=CARTESIAN_POINT('Ctrl Pts',(-41.9706415386519,48.0800384748524,-2.27861140169942));
#40965=CARTESIAN_POINT('Ctrl Pts',(-42.0380034246811,43.7943543597217,-2.47447395950472));
#40966=CARTESIAN_POINT('Ctrl Pts',(-45.6452574558605,41.4793316033294,-2.67033651731001));
#40967=CARTESIAN_POINT('Ctrl Pts',(-49.5694602110796,43.2033517729476,-2.8661990751153));
#40968=CARTESIAN_POINT('Ctrl Pts',(-50.3044873150015,47.4260701950796,-3.0620616329206));
#40969=CARTESIAN_POINT('Ctrl Pts',(-47.1936201674044,50.3746494360471,-3.25792419072589));
#40970=CARTESIAN_POINT('Ctrl Pts',(-43.0162992227714,49.4146473861733,-3.45378674853119));
#40971=CARTESIAN_POINT('Ctrl Pts',(-41.5048004091442,45.4037888959043,-3.64964930633648));
#40972=CARTESIAN_POINT('Ctrl Pts',(-44.0095899201106,41.9256221685573,-3.84551186414177));
#40973=CARTESIAN_POINT('Ctrl Pts',(-48.2927344491307,42.0877556591837,-4.04137442194706));
#40974=CARTESIAN_POINT('Ctrl Pts',(-50.5274087378249,45.7453293326157,-4.23723697975236));
#40975=CARTESIAN_POINT('Ctrl Pts',(-48.7170170678005,49.6304414709075,-4.43309953755765));
#40976=CARTESIAN_POINT('Ctrl Pts',(-44.4790749207218,50.2718934831503,-4.62896209536295));
#40977=CARTESIAN_POINT('Ctrl Pts',(-41.6000209605584,47.0965726099784,-4.82482465316824));
#40978=CARTESIAN_POINT('Ctrl Pts',(-42.6521794179657,42.9415061958563,-5.02068721097354));
#40979=CARTESIAN_POINT('Ctrl Pts',(-46.6954870752408,41.5190866142661,-5.21654976877883));
#40980=CARTESIAN_POINT('Ctrl Pts',(-50.117403742113,44.1001911874169,-5.41241232658411));
#40981=CARTESIAN_POINT('Ctrl Pts',(-49.8605781383007,48.3787020053837,-5.60827488438942));
#40982=CARTESIAN_POINT('Ctrl Pts',(-46.1544742116175,50.5319339099603,-5.8041374421947));
#40983=CARTESIAN_POINT('Ctrl Pts',(-42.3103533308119,48.6360567066936,-6.00000000000001));
#40984=CARTESIAN_POINT('Ctrl Pts',(-41.7627905066804,44.3849641691278,-6.19586255780529));
#40985=CARTESIAN_POINT('Ctrl Pts',(-45.0010110243469,41.5768438214505,-6.39172511561059));
#40986=CARTESIAN_POINT('Ctrl Pts',(-49.1317913410244,42.7206444744145,-6.58758767341588));
#40987=CARTESIAN_POINT('Ctrl Pts',(-50.4644332438766,46.7944219988274,-6.78345023122118));
#40988=CARTESIAN_POINT('Ctrl Pts',(-47.8082815886359,50.1584168935994,-6.97931278902647));
#40989=CARTESIAN_POINT('Ctrl Pts',(-43.5364870352555,49.807019877542,-7.17517534683176));
#40990=CARTESIAN_POINT('Ctrl Pts',(-41.4657727165736,46.0542089751936,-7.37103790463705));
#40991=CARTESIAN_POINT('Ctrl Pts',(-43.4461634484607,42.2529393572974,-7.56690046244235));
#40992=CARTESIAN_POINT('Ctrl Pts',(-47.7084174687297,41.7995758661054,-7.76276302024764));
#40993=CARTESIAN_POINT('Ctrl Pts',(-50.4440446531807,45.0990254193909,-7.95862557805294));
#40994=CARTESIAN_POINT('Ctrl Pts',(-49.2095409091294,49.2036751770803,-8.15448813585823));
#40995=CARTESIAN_POINT('Ctrl Pts',(-45.1065109570496,50.4455268236521,-8.35035069366353));
#40996=CARTESIAN_POINT('Ctrl Pts',(-41.8036689553657,47.7163645714366,-8.54621325146882));
#40997=CARTESIAN_POINT('Ctrl Pts',(-42.2462093282676,43.451873770107,-8.74207580927411));
#40998=CARTESIAN_POINT('Ctrl Pts',(-46.0506035443081,41.4678102239671,-8.93793836707941));
#40999=CARTESIAN_POINT('Ctrl Pts',(-48.5423946829461,42.8404451635287,-9.06851340561627));
#41000=CARTESIAN_POINT('Ctrl Pts',(-49.2312729758272,43.9008548125037,-9.1338009248847));
#41001=CARTESIAN_POINT('Ctrl Pts',(-42.8989858737798,48.6591232368927,0.401402774654087));
#41002=CARTESIAN_POINT('Ctrl Pts',(-42.0263390997967,47.6414607473255,0.336115255385656));
#41003=CARTESIAN_POINT('Ctrl Pts',(-41.3750598134236,44.6966738638162,0.205540216848794));
#41004=CARTESIAN_POINT('Ctrl Pts',(-44.5303430016157,41.4202123648473,0.00967765904350021));
#41005=CARTESIAN_POINT('Ctrl Pts',(-49.0001600008312,42.2448663028631,-0.186184898761794));
#41006=CARTESIAN_POINT('Ctrl Pts',(-50.7887546377267,46.4200984444482,-0.382047456567086));
#41007=CARTESIAN_POINT('Ctrl Pts',(-48.2991248954935,50.2221780497669,-0.577910014372381));
#41008=CARTESIAN_POINT('Ctrl Pts',(-43.7551468972239,50.2508324710758,-0.773772572177673));
#41009=CARTESIAN_POINT('Ctrl Pts',(-41.216941413185,46.4820553508686,-0.969635129982968));
#41010=CARTESIAN_POINT('Ctrl Pts',(-42.9521748839983,42.2823237877054,-1.16549768778826));
#41011=CARTESIAN_POINT('Ctrl Pts',(-47.4105428653624,41.4043187587238,-1.36136024559355));
#41012=CARTESIAN_POINT('Ctrl Pts',(-50.6086352711288,44.632317129114,-1.55722280339885));
#41013=CARTESIAN_POINT('Ctrl Pts',(-49.6890936551595,49.0823177128668,-1.75308536120414));
#41014=CARTESIAN_POINT('Ctrl Pts',(-45.4734861227781,50.7783710029823,-1.94894791900944));
#41015=CARTESIAN_POINT('Ctrl Pts',(-41.7282996653196,48.2051403801394,-2.14481047681473));
#41016=CARTESIAN_POINT('Ctrl Pts',(-41.7997129669298,43.6616979327745,-2.34067303462002));
#41017=CARTESIAN_POINT('Ctrl Pts',(-45.6239218081334,41.2074403684165,-2.53653559242531));
#41018=CARTESIAN_POINT('Ctrl Pts',(-49.784141948293,43.0351500661756,-2.73239815023061));
#41019=CARTESIAN_POINT('Ctrl Pts',(-50.5633765475329,47.511839809745,-2.9282607080359));
#41020=CARTESIAN_POINT('Ctrl Pts',(-47.2654092996424,50.6377585015902,-3.1241232658412));
#41021=CARTESIAN_POINT('Ctrl Pts',(-42.8368474210137,49.6200180555421,-3.31998582364649));
#41022=CARTESIAN_POINT('Ctrl Pts',(-41.2344409709606,45.3679303548353,-3.51584838145178));
#41023=CARTESIAN_POINT('Ctrl Pts',(-43.8898786280806,41.6805726486878,-3.71171093925708));
#41024=CARTESIAN_POINT('Ctrl Pts',(-48.430628748381,41.8524575015287,-3.90757349706237));
#41025=CARTESIAN_POINT('Ctrl Pts',(-50.7997053640471,45.7300124112724,-4.10343605486767));
#41026=CARTESIAN_POINT('Ctrl Pts',(-48.8804294354025,49.848790867101,-4.29929861267296));
#41027=CARTESIAN_POINT('Ctrl Pts',(-44.3876003506517,50.5288223911423,-4.49516117047825));
#41028=CARTESIAN_POINT('Ctrl Pts',(-41.3353884704811,47.1625249105979,-4.69102372828355));
#41029=CARTESIAN_POINT('Ctrl Pts',(-42.4508279821942,42.7575560397258,-4.88688628608884));
#41030=CARTESIAN_POINT('Ctrl Pts',(-46.7373164737192,41.2495864060927,-5.08274884389414));
#41031=CARTESIAN_POINT('Ctrl Pts',(-50.3650410138277,43.9859290211115,-5.27861140169942));
#41032=CARTESIAN_POINT('Ctrl Pts',(-50.0927688821017,48.5217667402822,-5.47447395950472));
#41033=CARTESIAN_POINT('Ctrl Pts',(-46.1637649138928,50.8045026982905,-5.67033651731001));
#41034=CARTESIAN_POINT('Ctrl Pts',(-42.0884430951448,48.7945997915639,-5.86619907511531));
#41035=CARTESIAN_POINT('Ctrl Pts',(-41.507947633761,44.2878293987898,-6.0620616329206));
#41036=CARTESIAN_POINT('Ctrl Pts',(-44.940927797173,41.3108173647246,-6.25792419072589));
#41037=CARTESIAN_POINT('Ctrl Pts',(-49.3201499067242,42.5234108033435,-6.45378674853119));
#41038=CARTESIAN_POINT('Ctrl Pts',(-50.7329422698335,46.8422017427392,-6.64964930633648));
#41039=CARTESIAN_POINT('Ctrl Pts',(-47.9170389384488,50.4085208617021,-6.84551186414178));
#41040=CARTESIAN_POINT('Ctrl Pts',(-43.3883214271118,50.0359894114731,-7.04137442194707));
#41041=CARTESIAN_POINT('Ctrl Pts',(-41.1930659955112,46.0574693216547,-7.23723697975236));
#41042=CARTESIAN_POINT('Ctrl Pts',(-43.2925654154187,42.0275760136403,-7.43309953755766));
#41043=CARTESIAN_POINT('Ctrl Pts',(-47.8111685874939,41.5469454131034,-7.62896209536294));
#41044=CARTESIAN_POINT('Ctrl Pts',(-50.7113274270403,45.0448371733502,-7.82482465316825));
#41045=CARTESIAN_POINT('Ctrl Pts',(-49.4025756475167,49.3963571266783,-8.02068721097353));
#41046=CARTESIAN_POINT('Ctrl Pts',(-45.0527729214423,50.7128987412233,-8.21654976877883));
#41047=CARTESIAN_POINT('Ctrl Pts',(-41.5512846772643,47.8195936610183,-8.41241232658412));
#41048=CARTESIAN_POINT('Ctrl Pts',(-42.0204412135141,43.2986191788456,-8.60827488438942));
#41049=CARTESIAN_POINT('Ctrl Pts',(-46.0536470456105,41.195226046819,-8.80413744219471));
#41050=CARTESIAN_POINT('Ctrl Pts',(-48.6953045558515,42.6504167892078,-8.93471248073157));
#41051=CARTESIAN_POINT('Ctrl Pts',(-49.4256147683784,43.7746037524369,-9.));
#41052=CARTESIAN_POINT('Ctrl Pts',(-43.4267655729853,48.2065515280923,0.));
#41053=CARTESIAN_POINT('Ctrl Pts',(-43.350127485791,48.1336147263286,-7.04754888835137E-18));
#41054=CARTESIAN_POINT('Ctrl Pts',(-43.2774221639843,48.0570418002056,-2.0037929668525E-16));
#41055=CARTESIAN_POINT('Ctrl Pts',(-43.2086471182341,47.9772483225893,-1.80411241501588E-16));
#41056=CARTESIAN_POINT('Ctrl Pts',(-43.1381549137597,47.8954625807044,-1.59944628740986E-16));
#41057=CARTESIAN_POINT('Ctrl Pts',(-43.0717912973076,47.8102930504676,-2.80029045420587E-16));
#41058=CARTESIAN_POINT('Ctrl Pts',(-43.0095797390392,47.722138908728,-3.05311331771918E-16));
#41059=CARTESIAN_POINT('Ctrl Pts',(-42.9460526993407,47.632120722112,-3.31128219395583E-16));
#41060=CARTESIAN_POINT('Ctrl Pts',(-42.8868547189701,47.5389898301017,-7.05663083191702E-16));
#41061=CARTESIAN_POINT('Ctrl Pts',(-42.8320442088995,47.443128838907,-7.21644966006352E-16));
#41062=CARTESIAN_POINT('Ctrl Pts',(-42.7793833374229,47.3510274639989,-7.37000048011074E-16));
#41063=CARTESIAN_POINT('Ctrl Pts',(-42.7307724565797,47.256405116335,-2.18211742452875E-16));
#41064=CARTESIAN_POINT('Ctrl Pts',(-42.6862972115001,47.1595729951209,-1.2490009027033E-16));
#41065=CARTESIAN_POINT('Ctrl Pts',(-42.6798840800015,47.1456102361632,-1.11444967207507E-16));
#41066=CARTESIAN_POINT('Ctrl Pts',(-42.6735569988815,47.1316014931762,-5.23608940400973E-16));
#41067=CARTESIAN_POINT('Ctrl Pts',(-42.6673162875643,47.1175476635147,-5.27355936696949E-16));
#41068=CARTESIAN_POINT('Ctrl Pts',(-42.6607661644965,47.102797051096,-5.31288707438301E-16));
#41069=CARTESIAN_POINT('Ctrl Pts',(-42.6543147503395,47.0880047578612,7.95783905053014E-17));
#41070=CARTESIAN_POINT('Ctrl Pts',(-42.6479633745278,47.0731750014718,6.93889390390723E-17));
#41071=CARTESIAN_POINT('Ctrl Pts',(-42.6031057839847,46.9684375147142,-2.57566442362801E-18));
#41072=CARTESIAN_POINT('Ctrl Pts',(-42.5632143269563,46.8617873344586,-4.68138119745799E-16));
#41073=CARTESIAN_POINT('Ctrl Pts',(-42.5283181388421,46.7536539294655,-3.60822483003176E-16));
#41074=CARTESIAN_POINT('Ctrl Pts',(-42.4929004096067,46.643904416229,-2.51902959975767E-16));
#41075=CARTESIAN_POINT('Ctrl Pts',(-42.4626279321656,46.5326263002381,-1.62036195599726E-16));
#41076=CARTESIAN_POINT('Ctrl Pts',(-42.4375708467752,46.4202321196064,-2.08166817117217E-16));
#41077=CARTESIAN_POINT('Ctrl Pts',(-42.4112941893324,46.302367518157,-2.56542696448442E-16));
#41078=CARTESIAN_POINT('Ctrl Pts',(-42.3907521119287,46.183274805057,1.09214840709062E-16));
#41079=CARTESIAN_POINT('Ctrl Pts',(-42.3760792116234,46.0634010904814,1.38777878078145E-16));
#41080=CARTESIAN_POINT('Ctrl Pts',(-42.3650745363945,45.9734958045497,1.60950156104956E-16));
#41081=CARTESIAN_POINT('Ctrl Pts',(-42.3573723501925,45.8831504952769,2.7624515033776E-16));
#41082=CARTESIAN_POINT('Ctrl Pts',(-42.3530521456739,45.7925483464972,4.16333634234434E-16));
#41083=CARTESIAN_POINT('Ctrl Pts',(-42.3520987176639,45.7725533147698,4.47249829025506E-16));
#41084=CARTESIAN_POINT('Ctrl Pts',(-42.3513101054994,45.7525434126973,-6.43493868513383E-16));
#41085=CARTESIAN_POINT('Ctrl Pts',(-42.3506877635742,45.7325443531856,-6.38378239159465E-16));
#41086=CARTESIAN_POINT('Ctrl Pts',(-42.3469997598448,45.6140297503959,-6.08062974556997E-16));
#41087=CARTESIAN_POINT('Ctrl Pts',(-42.3491369571258,45.495720031201,-1.89016809378538E-16));
#41088=CARTESIAN_POINT('Ctrl Pts',(-42.3571653633738,45.3780427848328,-1.94289029309402E-16));
#41089=CARTESIAN_POINT('Ctrl Pts',(-42.365167844959,45.2607455320572,-1.99544224625444E-16));
#41090=CARTESIAN_POINT('Ctrl Pts',(-42.3790232255707,45.1440757899907,5.28835535732368E-17));
#41091=CARTESIAN_POINT('Ctrl Pts',(-42.3988451111656,45.0284394788713,5.55111512312578E-17));
#41092=CARTESIAN_POINT('Ctrl Pts',(-42.4013982106115,45.0135452852572,5.58495911890846E-17));
#41093=CARTESIAN_POINT('Ctrl Pts',(-42.4040503639055,44.9986682229785,-4.58137967173707E-16));
#41094=CARTESIAN_POINT('Ctrl Pts',(-42.4068018766013,44.9838091499857,-4.71844785465692E-16));
#41095=CARTESIAN_POINT('Ctrl Pts',(-42.4276948097905,44.8709804431543,-6.0624956633226E-16));
#41096=CARTESIAN_POINT('Ctrl Pts',(-42.4543121735532,44.7591887131703,-8.63511011112326E-16));
#41097=CARTESIAN_POINT('Ctrl Pts',(-42.4863557082657,44.6486957988342,-9.71445146547012E-16));
#41098=CARTESIAN_POINT('Ctrl Pts',(-42.5065653594726,44.5790086285643,-1.03951851142446E-15));
#41099=CARTESIAN_POINT('Ctrl Pts',(-42.528934495595,44.509838105819,-9.38420932093488E-16));
#41100=CARTESIAN_POINT('Ctrl Pts',(-42.5533986678225,44.441251448601,-9.99200722162641E-16));
#41101=CARTESIAN_POINT('Ctrl Pts',(-42.5620407794544,44.4170228116121,-1.02067153776408E-15));
#41102=CARTESIAN_POINT('Ctrl Pts',(-42.5709443994809,44.3928670518755,-3.880055035361E-16));
#41103=CARTESIAN_POINT('Ctrl Pts',(-42.5801069098143,44.3687871960285,-3.88578058618805E-16));
#41104=CARTESIAN_POINT('Ctrl Pts',(-42.5859810783122,44.3533493819905,-3.88945128876595E-16));
#41105=CARTESIAN_POINT('Ctrl Pts',(-42.5919602903931,44.3379464816701,-9.54382670255255E-18));
#41106=CARTESIAN_POINT('Ctrl Pts',(-42.5980400731475,44.3225881416726,0.));
#41107=CARTESIAN_POINT('Ctrl Pts',(-42.6409152181459,44.2142798219628,6.73038774974722E-17));
#41108=CARTESIAN_POINT('Ctrl Pts',(-42.6888373119785,44.1080564604858,-3.4716028785113E-16));
#41109=CARTESIAN_POINT('Ctrl Pts',(-42.741452191163,44.0041741405836,-3.88578058618805E-16));
#41110=CARTESIAN_POINT('Ctrl Pts',(-42.7959112494356,43.8966506909297,-4.31447543956746E-16));
#41111=CARTESIAN_POINT('Ctrl Pts',(-42.8553979439767,43.791634588613,-3.1798967153709E-16));
#41112=CARTESIAN_POINT('Ctrl Pts',(-42.9195754661052,43.6894132096538,-5.55111512312578E-16));
#41113=CARTESIAN_POINT('Ctrl Pts',(-42.9844485692458,43.5860839155262,-7.94803372069007E-16));
#41114=CARTESIAN_POINT('Ctrl Pts',(-43.0541151127463,43.4856094929693,-7.88000339611239E-16));
#41115=CARTESIAN_POINT('Ctrl Pts',(-43.1282792501117,43.3883012080013,-7.21644966006352E-16));
#41116=CARTESIAN_POINT('Ctrl Pts',(-43.1809780311253,43.3191568994108,-6.74494855091483E-16));
#41117=CARTESIAN_POINT('Ctrl Pts',(-43.2359487941652,43.2516114776716,-8.53408132386238E-17));
#41118=CARTESIAN_POINT('Ctrl Pts',(-43.2930994306075,43.1857842411025,-5.55111512312578E-17));
#41119=CARTESIAN_POINT('Ctrl Pts',(-43.3103646730886,43.1658977923772,-4.64995919600553E-17));
#41120=CARTESIAN_POINT('Ctrl Pts',(-43.327828935708,43.1461682069428,-1.02592134112036E-16));
#41121=CARTESIAN_POINT('Ctrl Pts',(-43.345489866523,43.1265989222763,-1.11022302462516E-16));
#41122=CARTESIAN_POINT('Ctrl Pts',(-43.3628751859287,43.1073350302407,-1.19320912029112E-16));
#41123=CARTESIAN_POINT('Ctrl Pts',(-43.3804547805861,43.0882226751835,2.41217254613375E-16));
#41124=CARTESIAN_POINT('Ctrl Pts',(-43.3982046967558,43.0692880183209,2.22044604925031E-16));
#41125=CARTESIAN_POINT('Ctrl Pts',(-43.4838647831345,42.9779104407086,1.295184874654E-16));
#41126=CARTESIAN_POINT('Ctrl Pts',(-43.5735667660932,42.8905787756105,1.54127168466576E-16));
#41127=CARTESIAN_POINT('Ctrl Pts',(-43.6669813080034,42.8076092595666,-1.11022302462516E-16));
#41128=CARTESIAN_POINT('Ctrl Pts',(-43.7477793817384,42.7358455176695,-3.40360969278814E-16));
#41129=CARTESIAN_POINT('Ctrl Pts',(-43.8313559162862,42.6673451480848,-3.95274884398571E-16));
#41130=CARTESIAN_POINT('Ctrl Pts',(-43.9175245054789,42.602328677346,-1.66533453693773E-16));
#41131=CARTESIAN_POINT('Ctrl Pts',(-43.9569254786932,42.5725996049999,-6.19404103510884E-17));
#41132=CARTESIAN_POINT('Ctrl Pts',(-43.9968687187229,42.5435991930232,-9.45628619310071E-17));
#41133=CARTESIAN_POINT('Ctrl Pts',(-44.0373378970811,42.5153498982221,-5.55111512312578E-17));
#41134=CARTESIAN_POINT('Ctrl Pts',(-44.0558572039848,42.5024225944947,-3.76404989249141E-17));
#41135=CARTESIAN_POINT('Ctrl Pts',(-44.074488606412,42.4896512907743,7.87308458251505E-18));
#41136=CARTESIAN_POINT('Ctrl Pts',(-44.0932243068781,42.4770424318878,0.));
#41137=CARTESIAN_POINT('Ctrl Pts',(-44.1981797728502,42.4064089019487,-4.41042096338891E-17));
#41138=CARTESIAN_POINT('Ctrl Pts',(-44.3062422429739,42.3409785193577,4.59490679880944E-16));
#41139=CARTESIAN_POINT('Ctrl Pts',(-44.4171006494925,42.2810834907564,4.44089209850063E-16));
#41140=CARTESIAN_POINT('Ctrl Pts',(-44.5269323221333,42.2217431900906,4.28830383138215E-16));
#41141=CARTESIAN_POINT('Ctrl Pts',(-44.6395089620466,42.1678354863558,-2.86547826934204E-16));
#41142=CARTESIAN_POINT('Ctrl Pts',(-44.7545634922447,42.1197193691043,-2.22044604925031E-16));
#41143=CARTESIAN_POINT('Ctrl Pts',(-44.815479257569,42.0942442304743,-1.87893293127013E-16));
#41144=CARTESIAN_POINT('Ctrl Pts',(-44.8770901666956,42.0703932494507,-2.5515543336404E-16));
#41145=CARTESIAN_POINT('Ctrl Pts',(-44.9393361356002,42.0481502636203,-2.77555756156289E-16));
#41146=CARTESIAN_POINT('Ctrl Pts',(-49.387979831519,45.997252452837,-2.01601780324957));
#41147=CARTESIAN_POINT('Ctrl Pts',(-49.3905746620075,45.6709119723256,-1.99688706151736));
#41148=CARTESIAN_POINT('Ctrl Pts',(-49.347131989526,45.3452478557311,-1.97775631978515));
#41149=CARTESIAN_POINT('Ctrl Pts',(-49.2547930859516,45.0340948157173,-1.95862557805294));
#41150=CARTESIAN_POINT('Ctrl Pts',(-48.9396679313325,43.9722222349419,-1.8933380587845));
#41151=CARTESIAN_POINT('Ctrl Pts',(-48.0550711355392,43.0793534078484,-1.82805053951607));
#41152=CARTESIAN_POINT('Ctrl Pts',(-46.9961773535207,42.7543476987893,-1.76276302024764));
#41153=CARTESIAN_POINT('Ctrl Pts',(-45.9372835715021,42.4293419897301,-1.69747550097921));
#41154=CARTESIAN_POINT('Ctrl Pts',(-44.7040928032581,42.6721993987052,-1.63218798171078));
#41155=CARTESIAN_POINT('Ctrl Pts',(-43.8475134265744,43.3744538912888,-1.56690046244235));
#41156=CARTESIAN_POINT('Ctrl Pts',(-42.9909340498907,44.0767083838724,-1.50161294317392));
#41157=CARTESIAN_POINT('Ctrl Pts',(-42.5109660647671,45.2383599600643,-1.43632542390549));
#41158=CARTESIAN_POINT('Ctrl Pts',(-42.6220176511331,46.3404102378879,-1.37103790463705));
#41159=CARTESIAN_POINT('Ctrl Pts',(-42.7330692374992,47.4424605157114,-1.30575038536862));
#41160=CARTESIAN_POINT('Ctrl Pts',(-43.4351403953548,48.4849094951665,-1.24046286610019));
#41161=CARTESIAN_POINT('Ctrl Pts',(-44.4146112831213,49.0021710585525,-1.17517534683176));
#41162=CARTESIAN_POINT('Ctrl Pts',(-45.3940821708877,49.5194326219384,-1.10988782756333));
#41163=CARTESIAN_POINT('Ctrl Pts',(-46.6509527885649,49.5115067692553,-1.0446003082949));
#41164=CARTESIAN_POINT('Ctrl Pts',(-47.6237056175478,48.9817135963969,-0.979312789026467));
#41165=CARTESIAN_POINT('Ctrl Pts',(-48.5964584465306,48.4519204235384,-0.914025269758036));
#41166=CARTESIAN_POINT('Ctrl Pts',(-49.2850934868191,47.4002599305046,-0.848737750489605));
#41167=CARTESIAN_POINT('Ctrl Pts',(-49.3820471281213,46.2969921828887,-0.783450231221174));
#41168=CARTESIAN_POINT('Ctrl Pts',(-49.3906763290647,46.198797633817,-0.777639421897305));
#41169=CARTESIAN_POINT('Ctrl Pts',(-49.3946184665688,46.1001942727114,-0.771828612573436));
#41170=CARTESIAN_POINT('Ctrl Pts',(-49.3940292623548,46.0015451960205,-0.766017803249567));
#41171=CARTESIAN_POINT('Ctrl Pts',(-47.0579044229729,42.0543614925016,5.55111512312578E-16));
#41172=CARTESIAN_POINT('Ctrl Pts',(-48.3527480267224,42.4015349025495,-0.0652875192684306));
#41173=CARTESIAN_POINT('Ctrl Pts',(-50.5530316149402,44.4642359903368,-0.195862557805293));
#41174=CARTESIAN_POINT('Ctrl Pts',(-49.7989189441901,48.9500085119455,-0.391725115610587));
#41175=CARTESIAN_POINT('Ctrl Pts',(-45.6441921094362,50.7932694144525,-0.587587673415879));
#41176=CARTESIAN_POINT('Ctrl Pts',(-41.8104748163565,48.3572313450219,-0.783450231221174));
#41177=CARTESIAN_POINT('Ctrl Pts',(-41.7184176569125,43.8134905867626,-0.979312789026467));
#41178=CARTESIAN_POINT('Ctrl Pts',(-45.4525333012251,41.2240979371497,-1.17517534683176));
#41179=CARTESIAN_POINT('Ctrl Pts',(-49.6754258594775,42.9014061288129,-1.37103790463705));
#41180=CARTESIAN_POINT('Ctrl Pts',(-50.6146443015424,47.3473770364547,-1.56690046244235));
#41181=CARTESIAN_POINT('Ctrl Pts',(-47.4307681707597,50.5894263088653,-1.76276302024764));
#41182=CARTESIAN_POINT('Ctrl Pts',(-42.968598137007,49.7310442859955,-1.95862557805294));
#41183=CARTESIAN_POINT('Ctrl Pts',(-41.2148485187469,45.539095378305,-2.15448813585823));
#41184=CARTESIAN_POINT('Ctrl Pts',(-43.7364582880855,41.758957824139,-2.35035069366352));
#41185=CARTESIAN_POINT('Ctrl Pts',(-48.2804507290339,41.7680234302945,-2.54621325146882));
#41186=CARTESIAN_POINT('Ctrl Pts',(-50.7869503966815,45.5582002648003,-2.74207580927411));
#41187=CARTESIAN_POINT('Ctrl Pts',(-49.0164924035275,49.7431069481348,-2.9379383670794));
#41188=CARTESIAN_POINT('Ctrl Pts',(-44.5509147952652,50.5836918395513,-3.13380092488469));
#41189=CARTESIAN_POINT('Ctrl Pts',(-41.380038920474,47.3289236804855,-3.32966348268999));
#41190=CARTESIAN_POINT('Ctrl Pts',(-42.3369211082577,42.8868133607463,-3.52552604049528));
#41191=CARTESIAN_POINT('Ctrl Pts',(-46.5666236386886,41.2262157555308,-3.72138859830058));
#41192=CARTESIAN_POINT('Ctrl Pts',(-50.2900697268067,43.8308112032815,-3.91725115610587));
#41193=CARTESIAN_POINT('Ctrl Pts',(-50.1805031387222,48.3734935761537,-4.11311371391116));
#41194=CARTESIAN_POINT('Ctrl Pts',(-46.3358174405565,50.7955505353102,-4.30897627171646));
#41195=CARTESIAN_POINT('Ctrl Pts',(-42.1910917427793,48.9329671271487,-4.50483882952175));
#41196=CARTESIAN_POINT('Ctrl Pts',(-41.4494793999576,44.4498901520179,-4.70070138732704));
#41197=CARTESIAN_POINT('Ctrl Pts',(-44.7735825745146,41.351776836325,-4.89656394513234));
#41198=CARTESIAN_POINT('Ctrl Pts',(-49.1934426554123,42.406672531387,-5.09242650293763));
#41199=CARTESIAN_POINT('Ctrl Pts',(-50.7600842734221,46.6720684182653,-5.28828906074293));
#41200=CARTESIAN_POINT('Ctrl Pts',(-48.0737732836718,50.3369969638681,-5.48415161854822));
#41201=CARTESIAN_POINT('Ctrl Pts',(-43.5346254271756,50.1269851679324,-5.68001417635351));
#41202=CARTESIAN_POINT('Ctrl Pts',(-41.19819518517,46.2296704992633,-5.87587673415881));
#41203=CARTESIAN_POINT('Ctrl Pts',(-43.1519931670912,42.1271540690863,-6.07173929196409));
#41204=CARTESIAN_POINT('Ctrl Pts',(-47.650376155957,41.4848768173615,-6.2676018497694));
#41205=CARTESIAN_POINT('Ctrl Pts',(-50.6742109766474,44.8766889159707,-6.46346440757468));
#41206=CARTESIAN_POINT('Ctrl Pts',(-49.5218185107369,49.2721362263424,-6.65932696537998));
#41207=CARTESIAN_POINT('Ctrl Pts',(-45.2228146507001,50.7440556643996,-6.85518952318527));
#41208=CARTESIAN_POINT('Ctrl Pts',(-41.6181995750799,47.9773428774946,-7.05105208099057));
#41209=CARTESIAN_POINT('Ctrl Pts',(-41.9285478600743,43.4439512443748,-7.24691463879586));
#41210=CARTESIAN_POINT('Ctrl Pts',(-45.8765970139655,41.1942887704259,-7.44277719660115));
#41211=CARTESIAN_POINT('Ctrl Pts',(-49.934872084144,43.2383495723774,-7.63863975440645));
#41212=CARTESIAN_POINT('Ctrl Pts',(-50.4775511169527,47.7498293925976,-7.83450231221174));
#41213=CARTESIAN_POINT('Ctrl Pts',(-47.0195850264259,50.6979235414129,-8.03036487001704));
#41214=CARTESIAN_POINT('Ctrl Pts',(-42.6509144693004,49.448562948282,-8.22622742782232));
#41215=CARTESIAN_POINT('Ctrl Pts',(-41.274000700432,45.1181262021708,-8.42208998562762));
#41216=CARTESIAN_POINT('Ctrl Pts',(-44.1206543946181,41.5754411548869,-8.61795254343291));
#41217=CARTESIAN_POINT('Ctrl Pts',(-48.6442465086048,41.9862746311881,-8.81381510123821));
#41218=CARTESIAN_POINT('Ctrl Pts',(-50.8097847232332,45.9824991077558,-9.0096776590435));
#41219=CARTESIAN_POINT('Ctrl Pts',(-48.6687289051654,49.9958170642257,-9.2055402168488));
#41220=CARTESIAN_POINT('Ctrl Pts',(-45.6668068080595,50.2864153592086,-9.33611525538566));
#41221=CARTESIAN_POINT('Ctrl Pts',(-44.4292895827202,49.7709539622022,-9.40140277465409));
#41222=CARTESIAN_POINT('Ctrl Pts',(-46.9978874462229,42.2782052438144,0.133800924884696));
#41223=CARTESIAN_POINT('Ctrl Pts',(-48.219272052379,42.6056828306607,0.0685134056162651));
#41224=CARTESIAN_POINT('Ctrl Pts',(-50.2947292705676,44.5513628714236,-0.062061632920597));
#41225=CARTESIAN_POINT('Ctrl Pts',(-49.5833988792412,48.7826487879202,-0.257924190725891));
#41226=CARTESIAN_POINT('Ctrl Pts',(-45.6643777835214,50.521337912176,-0.453786748531184));
#41227=CARTESIAN_POINT('Ctrl Pts',(-42.0481547334457,48.2235010233062,-0.649649306336478));
#41228=CARTESIAN_POINT('Ctrl Pts',(-41.9613201558135,43.9375355210387,-0.845511864141771));
#41229=CARTESIAN_POINT('Ctrl Pts',(-45.4835921524958,41.4950441557703,-1.04137442194707));
#41230=CARTESIAN_POINT('Ctrl Pts',(-49.4669117975598,43.0771953894366,-1.23723697975236));
#41231=CARTESIAN_POINT('Ctrl Pts',(-50.3528465495515,47.2709377149863,-1.43309953755765));
#41232=CARTESIAN_POINT('Ctrl Pts',(-47.349597907951,50.3290592226769,-1.62896209536294));
#41233=CARTESIAN_POINT('Ctrl Pts',(-43.1405754642404,49.5193748824999,-1.82482465316824));
#41234=CARTESIAN_POINT('Ctrl Pts',(-41.4863194748743,45.5652433944807,-2.02068721097353));
#41235=CARTESIAN_POINT('Ctrl Pts',(-43.8648734145815,41.9995604004562,-2.21654976877883));
#41236=CARTESIAN_POINT('Ctrl Pts',(-48.1510763210893,42.0081116971315,-2.41241232658412));
#41237=CARTESIAN_POINT('Ctrl Pts',(-50.5153773845809,45.5832644235843,-2.60827488438941));
#41238=CARTESIAN_POINT('Ctrl Pts',(-48.8453609189455,49.5307532063404,-2.80413744219471));
#41239=CARTESIAN_POINT('Ctrl Pts',(-44.6331242190589,50.3236500809672,-3.));
#41240=CARTESIAN_POINT('Ctrl Pts',(-41.642138303627,47.2535312538142,-3.19586255780529));
#41241=CARTESIAN_POINT('Ctrl Pts',(-42.5447347026668,43.063430497502,-3.39172511561059));
#41242=CARTESIAN_POINT('Ctrl Pts',(-46.5344779769343,41.4970418261931,-3.58758767341588));
#41243=CARTESIAN_POINT('Ctrl Pts',(-50.0466857221096,43.9538735052741,-3.78345023122118));
#41244=CARTESIAN_POINT('Ctrl Pts',(-49.9433350597996,48.2388406664172,-3.97931278902647));
#41245=CARTESIAN_POINT('Ctrl Pts',(-46.3167658636045,50.523489620608,-4.17517534683176));
#41246=CARTESIAN_POINT('Ctrl Pts',(-42.407178520897,48.7665741940479,-4.37103790463706));
#41247=CARTESIAN_POINT('Ctrl Pts',(-41.7076392895683,44.5378309004316,-4.56690046244235));
#41248=CARTESIAN_POINT('Ctrl Pts',(-44.8431596218478,41.6154795825139,-4.76276302024764));
#41249=CARTESIAN_POINT('Ctrl Pts',(-49.0122724386701,42.6105289918156,-4.95862557805293));
#41250=CARTESIAN_POINT('Ctrl Pts',(-50.4900354287793,46.6339406689548,-5.15448813585823));
#41251=CARTESIAN_POINT('Ctrl Pts',(-47.9561240894267,50.0909506856854,-5.35035069366352));
#41252=CARTESIAN_POINT('Ctrl Pts',(-43.6744909246669,49.8928532676464,-5.54621325146882));
#41253=CARTESIAN_POINT('Ctrl Pts',(-41.470610917321,46.2166408448682,-5.74207580927411));
#41254=CARTESIAN_POINT('Ctrl Pts',(-43.3135661373547,42.3468681558645,-5.9379383670794));
#41255=CARTESIAN_POINT('Ctrl Pts',(-47.5567471047592,41.7410285425945,-6.13380092488469));
#41256=CARTESIAN_POINT('Ctrl Pts',(-50.4090338912526,44.9404165398932,-6.32966348268999));
#41257=CARTESIAN_POINT('Ctrl Pts',(-49.3220188926554,49.0865015701723,-6.52552604049528));
#41258=CARTESIAN_POINT('Ctrl Pts',(-45.2669058880808,50.4749161539406,-6.72138859830057));
#41259=CARTESIAN_POINT('Ctrl Pts',(-41.8667876408021,47.8651643678596,-6.91725115610587));
#41260=CARTESIAN_POINT('Ctrl Pts',(-42.1595292636062,43.5889608647215,-7.11311371391116));
#41261=CARTESIAN_POINT('Ctrl Pts',(-45.8835979055232,41.4669261210878,-7.30897627171646));
#41262=CARTESIAN_POINT('Ctrl Pts',(-49.7116391329811,43.395023375707,-7.50483882952176));
#41263=CARTESIAN_POINT('Ctrl Pts',(-50.2235309281268,47.6505581657348,-7.70070138732704));
#41264=CARTESIAN_POINT('Ctrl Pts',(-46.961741983617,50.4314011960709,-7.89656394513235));
#41265=CARTESIAN_POINT('Ctrl Pts',(-42.8409146092611,49.2529192608244,-8.09242650293762));
#41266=CARTESIAN_POINT('Ctrl Pts',(-41.5421158381738,45.1681566189754,-8.28828906074293));
#41267=CARTESIAN_POINT('Ctrl Pts',(-44.2272733282894,41.8264549890007,-8.48415161854821));
#41268=CARTESIAN_POINT('Ctrl Pts',(-48.4942332580861,42.2139810826501,-8.68001417635352));
#41269=CARTESIAN_POINT('Ctrl Pts',(-50.5369162753484,45.9834919674321,-8.8758767341588));
#41270=CARTESIAN_POINT('Ctrl Pts',(-48.5173267206434,49.769126585735,-9.0717392919641));
#41271=CARTESIAN_POINT('Ctrl Pts',(-45.6857095062803,50.0432386738974,-9.20231433050096));
#41272=CARTESIAN_POINT('Ctrl Pts',(-44.5183990415218,49.5570204051054,-9.26760184976939));
#41273=CARTESIAN_POINT('Ctrl Pts',(-46.9378704694728,42.5020489951272,0.267601849769392));
#41274=CARTESIAN_POINT('Ctrl Pts',(-48.0857960780355,42.8098307587719,0.202314330500961));
#41275=CARTESIAN_POINT('Ctrl Pts',(-50.0364269261949,44.6384897525104,0.0717392919640985));
#41276=CARTESIAN_POINT('Ctrl Pts',(-49.3678788142924,48.6152890638949,-0.124123265841195));
#41277=CARTESIAN_POINT('Ctrl Pts',(-45.6845634576067,50.2494064098995,-0.319985823646489));
#41278=CARTESIAN_POINT('Ctrl Pts',(-42.2858346505349,48.0897707015904,-0.515848381451782));
#41279=CARTESIAN_POINT('Ctrl Pts',(-42.2042226547145,44.0615804553148,-0.711710939257076));
#41280=CARTESIAN_POINT('Ctrl Pts',(-45.5146510037666,41.765990374391,-0.907573497062369));
#41281=CARTESIAN_POINT('Ctrl Pts',(-49.2583977356421,43.2529846500602,-1.10343605486766));
#41282=CARTESIAN_POINT('Ctrl Pts',(-50.0910487975607,47.194498393518,-1.29929861267296));
#41283=CARTESIAN_POINT('Ctrl Pts',(-47.2684276451423,50.0686921364886,-1.49516117047825));
#41284=CARTESIAN_POINT('Ctrl Pts',(-43.3125527914738,49.3077054790043,-1.69102372828354));
#41285=CARTESIAN_POINT('Ctrl Pts',(-41.7577904310017,45.5913914106565,-1.88688628608883));
#41286=CARTESIAN_POINT('Ctrl Pts',(-43.9932885410775,42.2401629767734,-2.08274884389413));
#41287=CARTESIAN_POINT('Ctrl Pts',(-48.0217019131448,42.2481999639685,-2.27861140169942));
#41288=CARTESIAN_POINT('Ctrl Pts',(-50.2438043724803,45.6083285823682,-2.47447395950472));
#41289=CARTESIAN_POINT('Ctrl Pts',(-48.6742294343635,49.318399464546,-2.67033651731001));
#41290=CARTESIAN_POINT('Ctrl Pts',(-44.7153336428526,50.0636083223831,-2.8661990751153));
#41291=CARTESIAN_POINT('Ctrl Pts',(-41.9042376867801,47.1781388271428,-3.0620616329206));
#41292=CARTESIAN_POINT('Ctrl Pts',(-42.7525482970759,43.2400476342577,-3.25792419072589));
#41293=CARTESIAN_POINT('Ctrl Pts',(-46.5023323151801,41.7678678968555,-3.45378674853118));
#41294=CARTESIAN_POINT('Ctrl Pts',(-49.8033017174126,44.0769358072666,-3.64964930633648));
#41295=CARTESIAN_POINT('Ctrl Pts',(-49.706166980877,48.1041877566808,-3.84551186414177));
#41296=CARTESIAN_POINT('Ctrl Pts',(-46.2977142866525,50.2514287059059,-4.04137442194707));
#41297=CARTESIAN_POINT('Ctrl Pts',(-42.6232652990147,48.6001812609472,-4.23723697975236));
#41298=CARTESIAN_POINT('Ctrl Pts',(-41.965799179179,44.6257716488452,-4.43309953755766));
#41299=CARTESIAN_POINT('Ctrl Pts',(-44.912736669181,41.8791823287028,-4.62896209536295));
#41300=CARTESIAN_POINT('Ctrl Pts',(-48.8311022219279,42.8143854522443,-4.82482465316824));
#41301=CARTESIAN_POINT('Ctrl Pts',(-50.2199865841366,46.5958129196444,-5.02068721097354));
#41302=CARTESIAN_POINT('Ctrl Pts',(-47.8384748951817,49.8449044075027,-5.21654976877883));
#41303=CARTESIAN_POINT('Ctrl Pts',(-43.8143564221583,49.6587213673604,-5.41241232658412));
#41304=CARTESIAN_POINT('Ctrl Pts',(-41.743026649472,46.2036111904731,-5.60827488438941));
#41305=CARTESIAN_POINT('Ctrl Pts',(-43.4751391076183,42.5665822426429,-5.80413744219471));
#41306=CARTESIAN_POINT('Ctrl Pts',(-47.4631180535614,41.9971802678274,-6.));
#41307=CARTESIAN_POINT('Ctrl Pts',(-50.1438568058577,45.0041441638159,-6.1958625578053));
#41308=CARTESIAN_POINT('Ctrl Pts',(-49.1222192745738,48.9008669140022,-6.39172511561059));
#41309=CARTESIAN_POINT('Ctrl Pts',(-45.3109971254615,50.2057766434817,-6.58758767341588));
#41310=CARTESIAN_POINT('Ctrl Pts',(-42.1153757065243,47.7529858582244,-6.78345023122117));
#41311=CARTESIAN_POINT('Ctrl Pts',(-42.3905106671381,43.7339704850681,-6.97931278902647));
#41312=CARTESIAN_POINT('Ctrl Pts',(-45.890598797081,41.7395634717496,-7.17517534683176));
#41313=CARTESIAN_POINT('Ctrl Pts',(-49.4884061818182,43.5516971790367,-7.37103790463706));
#41314=CARTESIAN_POINT('Ctrl Pts',(-49.9695107393009,47.551286938872,-7.56690046244235));
#41315=CARTESIAN_POINT('Ctrl Pts',(-46.9038989408082,50.1648788507288,-7.76276302024764));
#41316=CARTESIAN_POINT('Ctrl Pts',(-43.0309147492218,49.0572755733668,-7.95862557805294));
#41317=CARTESIAN_POINT('Ctrl Pts',(-41.8102309759155,45.21818703578,-8.15448813585822));
#41318=CARTESIAN_POINT('Ctrl Pts',(-44.3338922619607,42.0774688231145,-8.35035069366353));
#41319=CARTESIAN_POINT('Ctrl Pts',(-48.3442200075673,42.4416875341121,-8.54621325146881));
#41320=CARTESIAN_POINT('Ctrl Pts',(-50.2640478274637,45.9844848271084,-8.74207580927412));
#41321=CARTESIAN_POINT('Ctrl Pts',(-48.3659245361215,49.5424361072444,-8.9379383670794));
#41322=CARTESIAN_POINT('Ctrl Pts',(-45.7046122045012,49.8000619885861,-9.06851340561627));
#41323=CARTESIAN_POINT('Ctrl Pts',(-44.6075085003234,49.3430868480087,-9.1338009248847));
#41324=CARTESIAN_POINT('Ctrl Pts',(-46.8778534927228,42.72589274644,0.401402774654088));
#41325=CARTESIAN_POINT('Ctrl Pts',(-47.9523201036921,43.0139786868831,0.336115255385657));
#41326=CARTESIAN_POINT('Ctrl Pts',(-49.7781245818222,44.7256166335971,0.205540216848794));
#41327=CARTESIAN_POINT('Ctrl Pts',(-49.1523587493435,48.4479293398696,0.00967765904350058));
#41328=CARTESIAN_POINT('Ctrl Pts',(-45.7047491316919,49.9774749076231,-0.186184898761793));
#41329=CARTESIAN_POINT('Ctrl Pts',(-42.5235145676241,47.9560403798747,-0.382047456567086));
#41330=CARTESIAN_POINT('Ctrl Pts',(-42.4471251536154,44.1856253895909,-0.57791001437238));
#41331=CARTESIAN_POINT('Ctrl Pts',(-45.5457098550374,42.0369365930118,-0.773772572177673));
#41332=CARTESIAN_POINT('Ctrl Pts',(-49.0498836737243,43.4287739106838,-0.969635129982967));
#41333=CARTESIAN_POINT('Ctrl Pts',(-49.82925104557,47.1180590720496,-1.16549768778826));
#41334=CARTESIAN_POINT('Ctrl Pts',(-47.1872573823336,49.8083250503002,-1.36136024559355));
#41335=CARTESIAN_POINT('Ctrl Pts',(-43.4845301187073,49.0960360755087,-1.55722280339885));
#41336=CARTESIAN_POINT('Ctrl Pts',(-42.0292613871291,45.6175394268322,-1.75308536120414));
#41337=CARTESIAN_POINT('Ctrl Pts',(-44.1217036675735,42.4807655530906,-1.94894791900944));
#41338=CARTESIAN_POINT('Ctrl Pts',(-47.8923275052001,42.4882882308056,-2.14481047681473));
#41339=CARTESIAN_POINT('Ctrl Pts',(-49.9722313603797,45.6333927411522,-2.34067303462002));
#41340=CARTESIAN_POINT('Ctrl Pts',(-48.5030979497815,49.1060457227516,-2.53653559242532));
#41341=CARTESIAN_POINT('Ctrl Pts',(-44.7975430666463,49.8035665637991,-2.73239815023061));
#41342=CARTESIAN_POINT('Ctrl Pts',(-42.1663370699331,47.1027464004715,-2.9282607080359));
#41343=CARTESIAN_POINT('Ctrl Pts',(-42.960361891485,43.4166647710134,-3.1241232658412));
#41344=CARTESIAN_POINT('Ctrl Pts',(-46.4701866534259,42.0386939675179,-3.31998582364649));
#41345=CARTESIAN_POINT('Ctrl Pts',(-49.5599177127155,44.1999981092592,-3.51584838145178));
#41346=CARTESIAN_POINT('Ctrl Pts',(-49.4689989019545,47.9695348469442,-3.71171093925708));
#41347=CARTESIAN_POINT('Ctrl Pts',(-46.2786627097004,49.9793677912038,-3.90757349706237));
#41348=CARTESIAN_POINT('Ctrl Pts',(-42.8393520771325,48.4337883278464,-4.10343605486766));
#41349=CARTESIAN_POINT('Ctrl Pts',(-42.2239590687897,44.7137123972589,-4.29929861267296));
#41350=CARTESIAN_POINT('Ctrl Pts',(-44.9823137165143,42.1428850748917,-4.49516117047826));
#41351=CARTESIAN_POINT('Ctrl Pts',(-48.6499320051857,43.018241912673,-4.69102372828354));
#41352=CARTESIAN_POINT('Ctrl Pts',(-49.9499377394939,46.557685170334,-4.88688628608884));
#41353=CARTESIAN_POINT('Ctrl Pts',(-47.7208257009366,49.59885812932,-5.08274884389413));
#41354=CARTESIAN_POINT('Ctrl Pts',(-43.9542219196496,49.4245894670743,-5.27861140169942));
#41355=CARTESIAN_POINT('Ctrl Pts',(-42.015442381623,46.1905815360779,-5.47447395950472));
#41356=CARTESIAN_POINT('Ctrl Pts',(-43.6367120778818,42.7862963294211,-5.67033651731001));
#41357=CARTESIAN_POINT('Ctrl Pts',(-47.3694890023636,42.2533319930603,-5.86619907511531));
#41358=CARTESIAN_POINT('Ctrl Pts',(-49.8786797204628,45.0678717877384,-6.06206163292059));
#41359=CARTESIAN_POINT('Ctrl Pts',(-48.9224196564922,48.7152322578321,-6.2579241907259));
#41360=CARTESIAN_POINT('Ctrl Pts',(-45.3550883628422,49.9366371330228,-6.45378674853118));
#41361=CARTESIAN_POINT('Ctrl Pts',(-42.3639637722466,47.6408073485894,-6.64964930633649));
#41362=CARTESIAN_POINT('Ctrl Pts',(-42.6214920706699,43.8789801054148,-6.84551186414177));
#41363=CARTESIAN_POINT('Ctrl Pts',(-45.8975996886388,42.0122008224115,-7.04137442194707));
#41364=CARTESIAN_POINT('Ctrl Pts',(-49.2651732306554,43.7083709823662,-7.23723697975236));
#41365=CARTESIAN_POINT('Ctrl Pts',(-49.715490550475,47.4520157120093,-7.43309953755766));
#41366=CARTESIAN_POINT('Ctrl Pts',(-46.8460558979993,49.8983565053867,-7.62896209536295));
#41367=CARTESIAN_POINT('Ctrl Pts',(-43.2209148891825,48.8616318859092,-7.82482465316825));
#41368=CARTESIAN_POINT('Ctrl Pts',(-42.0783461136572,45.2682174525847,-8.02068721097353));
#41369=CARTESIAN_POINT('Ctrl Pts',(-44.440511195632,42.3284826572283,-8.21654976877883));
#41370=CARTESIAN_POINT('Ctrl Pts',(-48.1942067570486,42.6693939855741,-8.41241232658413));
#41371=CARTESIAN_POINT('Ctrl Pts',(-49.9911793795789,45.9854776867847,-8.60827488438941));
#41372=CARTESIAN_POINT('Ctrl Pts',(-48.2145223515996,49.3157456287537,-8.8041374421947));
#41373=CARTESIAN_POINT('Ctrl Pts',(-45.723514902722,49.5568853032748,-8.93471248073157));
#41374=CARTESIAN_POINT('Ctrl Pts',(-44.696617959125,49.1291532909119,-9.));
#41375=CARTESIAN_POINT('Ctrl Pts',(-49.3881106776293,46.0027671006797,-1.10898219675043));
#41376=CARTESIAN_POINT('Ctrl Pts',(-49.3906991281383,46.3240935175671,-1.12782069376304));
#41377=CARTESIAN_POINT('Ctrl Pts',(-49.3485999788577,46.6447561566529,-1.14665919077565));
#41378=CARTESIAN_POINT('Ctrl Pts',(-49.2590242063896,46.9515558748637,-1.16549768778826));
#41379=CARTESIAN_POINT('Ctrl Pts',(-48.9485864911578,48.0148143981331,-1.23078520705669));
#41380=CARTESIAN_POINT('Ctrl Pts',(-48.0679219367457,48.9115697242166,-1.29607272632512));
#41381=CARTESIAN_POINT('Ctrl Pts',(-47.0104684489353,49.2412325581265,-1.36136024559355));
#41382=CARTESIAN_POINT('Ctrl Pts',(-45.9530149611248,49.5708953920363,-1.42664776486198));
#41383=CARTESIAN_POINT('Ctrl Pts',(-44.7187725399161,49.3334657337725,-1.49193528413041));
#41384=CARTESIAN_POINT('Ctrl Pts',(-43.8591065407153,48.6350014631945,-1.55722280339884));
#41385=CARTESIAN_POINT('Ctrl Pts',(-42.9994405415145,47.9365371926165,-1.62251032266727));
#41386=CARTESIAN_POINT('Ctrl Pts',(-42.5143509643218,46.7770383097244,-1.6877978419357));
#41387=CARTESIAN_POINT('Ctrl Pts',(-42.6205465557995,45.6744932226547,-1.75308536120414));
#41388=CARTESIAN_POINT('Ctrl Pts',(-42.7267421472772,44.571948135585,-1.81837288047257));
#41389=CARTESIAN_POINT('Ctrl Pts',(-43.4242229074254,43.5263568443378,-1.883660399741));
#41390=CARTESIAN_POINT('Ctrl Pts',(-44.4014005937706,43.0048149783333,-1.94894791900943));
#41391=CARTESIAN_POINT('Ctrl Pts',(-45.3785782801157,42.4832731123289,-2.01423543827786));
#41392=CARTESIAN_POINT('Ctrl Pts',(-46.6354528926579,42.4857806715673,-2.07952295754629));
#41393=CARTESIAN_POINT('Ctrl Pts',(-47.610540841459,43.0112185362442,-2.14481047681472));
#41394=CARTESIAN_POINT('Ctrl Pts',(-48.58562879026,43.5366564009211,-2.21009799608315));
#41395=CARTESIAN_POINT('Ctrl Pts',(-49.2789300753199,44.5850245710367,-2.27538551535158));
#41396=CARTESIAN_POINT('Ctrl Pts',(-49.3807251494168,45.6879841530277,-2.34067303462002));
#41397=CARTESIAN_POINT('Ctrl Pts',(-49.3902409166803,45.7910884218386,-2.34677608866349));
#41398=CARTESIAN_POINT('Ctrl Pts',(-49.394587840163,45.8946697346342,-2.35287914270696));
#41399=CARTESIAN_POINT('Ctrl Pts',(-49.3939446252011,45.9983056787136,-2.35898219675043));
#41400=CARTESIAN_POINT('Ctrl Pts',(-47.0579044229729,42.0543614925016,5.55111512312578E-16));
#41401=CARTESIAN_POINT('Ctrl Pts',(-47.1733692374414,42.0960014311082,5.66013339959512E-16));
#41402=CARTESIAN_POINT('Ctrl Pts',(-47.2864784544055,42.1431495258543,1.12270800514822E-15));
#41403=CARTESIAN_POINT('Ctrl Pts',(-47.3970074324165,42.1954516216316,9.71445146547012E-16));
#41404=CARTESIAN_POINT('Ctrl Pts',(-47.5098931343429,42.2488689145469,8.16957026998136E-16));
#41405=CARTESIAN_POINT('Ctrl Pts',(-47.620088014245,42.3076628912825,-2.48568638880629E-16));
#41406=CARTESIAN_POINT('Ctrl Pts',(-47.7273254658327,42.3715030108371,-1.94289029309402E-16));
#41407=CARTESIAN_POINT('Ctrl Pts',(-47.8392938527237,42.4381595296151,-1.37614796242688E-16));
#41408=CARTESIAN_POINT('Ctrl Pts',(-47.9480390302718,42.5103177737784,2.81552683011295E-16));
#41409=CARTESIAN_POINT('Ctrl Pts',(-48.0532159541544,42.5876437997826,2.08166817117217E-16));
#41410=CARTESIAN_POINT('Ctrl Pts',(-48.1452457625517,42.6553040725363,1.43954184459898E-16));
#41411=CARTESIAN_POINT('Ctrl Pts',(-48.234543268668,42.7269219306243,3.57553482541936E-16));
#41412=CARTESIAN_POINT('Ctrl Pts',(-48.3208447022047,42.8022930418766,2.91433543964104E-16));
#41413=CARTESIAN_POINT('Ctrl Pts',(-48.3378037817389,42.8171042057001,2.78440326456705E-16));
#41414=CARTESIAN_POINT('Ctrl Pts',(-48.3546470605663,42.8320603488493,-9.65298675504177E-17));
#41415=CARTESIAN_POINT('Ctrl Pts',(-48.3713723802753,42.8471599789909,-1.11022302462516E-16));
#41416=CARTESIAN_POINT('Ctrl Pts',(-48.3839949979561,42.8585556869185,-1.21959759464334E-16));
#41417=CARTESIAN_POINT('Ctrl Pts',(-48.3965503865158,42.8700331641752,6.34306447284316E-16));
#41418=CARTESIAN_POINT('Ctrl Pts',(-48.4090271849394,42.8815818936618,6.24500451351651E-16));
#41419=CARTESIAN_POINT('Ctrl Pts',(-48.4995023665661,42.9653272073537,5.53392525029661E-16));
#41420=CARTESIAN_POINT('Ctrl Pts',(-48.5859893911482,43.0529427915412,6.24851978512991E-16));
#41421=CARTESIAN_POINT('Ctrl Pts',(-48.6682306336821,43.1441142001542,5.55111512312578E-16));
#41422=CARTESIAN_POINT('Ctrl Pts',(-48.7501460833931,43.2349244397276,4.85647318000291E-16));
#41423=CARTESIAN_POINT('Ctrl Pts',(-48.8278497989444,43.3292631204114,2.29444790427909E-16));
#41424=CARTESIAN_POINT('Ctrl Pts',(-48.9010447261095,43.4268484092624,1.80411241501588E-16));
#41425=CARTESIAN_POINT('Ctrl Pts',(-48.9731604547005,43.5229948838586,1.32100651640001E-16));
#41426=CARTESIAN_POINT('Ctrl Pts',(-49.0408997240368,43.6222936314722,4.78619745031733E-16));
#41427=CARTESIAN_POINT('Ctrl Pts',(-49.1039311102743,43.7244925695876,5.55111512312578E-16));
#41428=CARTESIAN_POINT('Ctrl Pts',(-49.155490252746,43.8080904392409,6.17681132982036E-16));
#41429=CARTESIAN_POINT('Ctrl Pts',(-49.2038985462528,43.8936293247998,4.03026082704482E-17));
#41430=CARTESIAN_POINT('Ctrl Pts',(-49.2489479688624,43.9809753984075,-2.77555756156289E-17));
#41431=CARTESIAN_POINT('Ctrl Pts',(-49.2595819350771,44.0015935360423,-4.38207854709016E-17));
#41432=CARTESIAN_POINT('Ctrl Pts',(-49.270028632464,44.0223123771606,-2.25961482045739E-16));
#41433=CARTESIAN_POINT('Ctrl Pts',(-49.2802851129785,44.0431301684709,-2.4980018054066E-16));
#41434=CARTESIAN_POINT('Ctrl Pts',(-49.2875269453717,44.0578290659389,-2.66632061489241E-16));
#41435=CARTESIAN_POINT('Ctrl Pts',(-49.2946732228582,44.0725759485657,7.95634595235508E-16));
#41436=CARTESIAN_POINT('Ctrl Pts',(-49.301717831292,44.0873590873138,7.7715611723761E-16));
#41437=CARTESIAN_POINT('Ctrl Pts',(-49.3523570973335,44.1936257880164,6.44325943328169E-16));
#41438=CARTESIAN_POINT('Ctrl Pts',(-49.397823772424,44.3019195500152,4.63255393197704E-18));
#41439=CARTESIAN_POINT('Ctrl Pts',(-49.4378467145292,44.4119843341003,1.38777878078145E-16));
#41440=CARTESIAN_POINT('Ctrl Pts',(-49.4770635111394,44.5198321839678,2.70221235726126E-16));
#41441=CARTESIAN_POINT('Ctrl Pts',(-49.5110538889566,44.6293810645388,7.52076617720226E-16));
#41442=CARTESIAN_POINT('Ctrl Pts',(-49.5395138665875,44.7404008831522,8.04911692853238E-16));
#41443=CARTESIAN_POINT('Ctrl Pts',(-49.5449744944973,44.7617023025674,8.15049180999944E-16));
#41444=CARTESIAN_POINT('Ctrl Pts',(-49.5502313718793,44.7830578900246,-4.5156980917228E-16));
#41445=CARTESIAN_POINT('Ctrl Pts',(-49.5552821294542,44.804466037532,-4.71844785465692E-16));
#41446=CARTESIAN_POINT('Ctrl Pts',(-49.5824900757527,44.9197896734607,-6.10151655747883E-16));
#41447=CARTESIAN_POINT('Ctrl Pts',(-49.6037208233721,45.0366392601437,7.24995094299097E-16));
#41448=CARTESIAN_POINT('Ctrl Pts',(-49.6190589580299,45.1545782432542,8.04911692853238E-16));
#41449=CARTESIAN_POINT('Ctrl Pts',(-49.6275693456393,45.2200168694572,8.4925354049578E-16));
#41450=CARTESIAN_POINT('Ctrl Pts',(-49.6342647061823,45.285790742732,9.91139680797571E-17));
#41451=CARTESIAN_POINT('Ctrl Pts',(-49.6391528952321,45.3518232724505,5.55111512312578E-17));
#41452=CARTESIAN_POINT('Ctrl Pts',(-49.6410791584549,45.3778443678321,3.83288160858751E-17));
#41453=CARTESIAN_POINT('Ctrl Pts',(-49.6427247418287,45.4039056075073,7.48033515296283E-16));
#41454=CARTESIAN_POINT('Ctrl Pts',(-49.6440899361851,45.4300022098967,7.7715611723761E-16));
#41455=CARTESIAN_POINT('Ctrl Pts',(-49.6449643353021,45.4467169333192,7.95808975932785E-16));
#41456=CARTESIAN_POINT('Ctrl Pts',(-49.6457236611113,45.4634466313103,-2.3566119177251E-16));
#41457=CARTESIAN_POINT('Ctrl Pts',(-49.6463675672004,45.4801746114213,-2.22044604925031E-16));
#41458=CARTESIAN_POINT('Ctrl Pts',(-49.650944859773,45.5990876958098,-1.25249275773564E-16));
#41459=CARTESIAN_POINT('Ctrl Pts',(-49.6497054380441,45.7181030341178,-2.85690848750654E-16));
#41460=CARTESIAN_POINT('Ctrl Pts',(-49.642802430889,45.8367853608077,-2.22044604925031E-16));
#41461=CARTESIAN_POINT('Ctrl Pts',(-49.6360413171965,45.9530281353007,-1.59706629468275E-16));
#41462=CARTESIAN_POINT('Ctrl Pts',(-49.6238465215681,46.0689523583233,3.31802632205194E-16));
#41463=CARTESIAN_POINT('Ctrl Pts',(-49.6063095800648,46.1841392093055,1.11022302462516E-16));
#41464=CARTESIAN_POINT('Ctrl Pts',(-49.5889758936611,46.297991031893,-1.07199158740278E-16));
#41465=CARTESIAN_POINT('Ctrl Pts',(-49.5664227750947,46.4111232891586,5.10322680618708E-17));
#41466=CARTESIAN_POINT('Ctrl Pts',(-49.5386937107918,46.5231091504923,-5.55111512312578E-17));
#41467=CARTESIAN_POINT('Ctrl Pts',(-49.5206040122694,46.5961657256503,-1.25017223037783E-16));
#41468=CARTESIAN_POINT('Ctrl Pts',(-49.5003105810002,46.6687339212223,-6.47114358888512E-16));
#41469=CARTESIAN_POINT('Ctrl Pts',(-49.477816188174,46.7406875318196,-7.21644966006352E-16));
#41470=CARTESIAN_POINT('Ctrl Pts',(-49.4685898886408,46.7702000227321,-7.52214437739744E-16));
#41471=CARTESIAN_POINT('Ctrl Pts',(-49.458993237021,46.799609039298,3.77824931536309E-18));
#41472=CARTESIAN_POINT('Ctrl Pts',(-49.4490260923412,46.8289055070053,0.));
#41473=CARTESIAN_POINT('Ctrl Pts',(-49.4429393126163,46.8467964026811,-2.30731789967445E-18));
#41474=CARTESIAN_POINT('Ctrl Pts',(-49.4367170562216,46.8646373229998,2.9761811420164E-16));
#41475=CARTESIAN_POINT('Ctrl Pts',(-49.4303611602144,46.8824221857011,3.33066907387547E-16));
#41476=CARTESIAN_POINT('Ctrl Pts',(-49.392180766493,46.9892573289204,5.46010743984259E-16));
#41477=CARTESIAN_POINT('Ctrl Pts',(-49.3491646814368,47.0941213407157,-6.96374359617231E-16));
#41478=CARTESIAN_POINT('Ctrl Pts',(-49.3013722120853,47.1966033447963,-6.66133814775094E-16));
#41479=CARTESIAN_POINT('Ctrl Pts',(-49.2629805514864,47.278927074278,-6.41841604105534E-16));
#41480=CARTESIAN_POINT('Ctrl Pts',(-49.2215058246924,47.3597134134632,1.18644211359586E-16));
#41481=CARTESIAN_POINT('Ctrl Pts',(-49.1769600904346,47.4387325885125,2.77555756156289E-16));
#41482=CARTESIAN_POINT('Ctrl Pts',(-49.1548835763497,47.4778938675894,3.56311062706237E-16));
#41483=CARTESIAN_POINT('Ctrl Pts',(-49.1320525422512,47.5166208499627,-1.58005809035499E-16));
#41484=CARTESIAN_POINT('Ctrl Pts',(-49.1084670740132,47.5548838684341,-1.66533453693773E-16));
#41485=CARTESIAN_POINT('Ctrl Pts',(-49.0950717251622,47.5766153208413,-1.71376723029023E-16));
#41486=CARTESIAN_POINT('Ctrl Pts',(-49.0814312209137,47.5981996315565,7.12245490477885E-18));
#41487=CARTESIAN_POINT('Ctrl Pts',(-49.0675592202023,47.6196105788371,0.));
#41488=CARTESIAN_POINT('Ctrl Pts',(-49.0090089012406,47.709980945637,-3.0062138485895E-17));
#41489=CARTESIAN_POINT('Ctrl Pts',(-48.9462915591126,47.7973423071076,5.3888875104828E-16));
#41490=CARTESIAN_POINT('Ctrl Pts',(-48.8794391108352,47.8813135513516,3.88578058618805E-16));
#41491=CARTESIAN_POINT('Ctrl Pts',(-48.8212022036609,47.954463087118,2.57638503406439E-16));
#41492=CARTESIAN_POINT('Ctrl Pts',(-48.7598266730131,48.0250397676994,8.03315147564942E-16));
#41493=CARTESIAN_POINT('Ctrl Pts',(-48.6953141039964,48.0927658834935,9.99200722162641E-16));
#41494=CARTESIAN_POINT('Ctrl Pts',(-48.6572947310406,48.1326791049708,1.06036603675156E-15));
#41495=CARTESIAN_POINT('Ctrl Pts',(-48.6181854212265,48.1716017502292,2.12735497367301E-16));
#41496=CARTESIAN_POINT('Ctrl Pts',(-48.5780352480409,48.2095125055216,2.77555756156289E-16));
#41497=CARTESIAN_POINT('Origin',(-46.,46.,-5.));
#41498=CARTESIAN_POINT('Origin',(46.,-46.,-9.));
#41499=CARTESIAN_POINT('Ctrl Pts',(47.3033820408749,-42.8708467090881,-9.));
#41500=CARTESIAN_POINT('Ctrl Pts',(47.2095002176375,-42.8200478993858,-9.));
#41501=CARTESIAN_POINT('Ctrl Pts',(47.1132610952936,-42.7741603120111,-9.));
#41502=CARTESIAN_POINT('Ctrl Pts',(47.0150558684064,-42.7330710668746,-9.));
#41503=CARTESIAN_POINT('Ctrl Pts',(46.9145913812888,-42.6910365431579,-9.));
#41504=CARTESIAN_POINT('Ctrl Pts',(46.8120687118127,-42.6540234152959,-9.));
#41505=CARTESIAN_POINT('Ctrl Pts',(46.7078720919618,-42.6219531198193,-9.));
#41506=CARTESIAN_POINT('Ctrl Pts',(46.6771618756247,-42.6125009349644,-9.));
#41507=CARTESIAN_POINT('Ctrl Pts',(46.6463060552087,-42.6034784112983,-9.));
#41508=CARTESIAN_POINT('Ctrl Pts',(46.6153140309619,-42.594884267454,-9.));
#41509=CARTESIAN_POINT('Ctrl Pts',(46.5945562374165,-42.5891280941173,-9.));
#41510=CARTESIAN_POINT('Ctrl Pts',(46.5737373386698,-42.5835641003044,-9.));
#41511=CARTESIAN_POINT('Ctrl Pts',(46.5528601193257,-42.5781919859202,-9.));
#41512=CARTESIAN_POINT('Ctrl Pts',(46.5322674936134,-42.5728931030098,-9.));
#41513=CARTESIAN_POINT('Ctrl Pts',(46.511625647447,-42.5677828752221,-9.));
#41514=CARTESIAN_POINT('Ctrl Pts',(46.4909429939031,-42.562861907011,-9.));
#41515=CARTESIAN_POINT('Ctrl Pts',(46.3816028037924,-42.5368468892283,-9.));
#41516=CARTESIAN_POINT('Ctrl Pts',(46.2710760141354,-42.5161050297694,-9.));
#41517=CARTESIAN_POINT('Ctrl Pts',(46.1597772205501,-42.5005437397571,-9.));
#41518=CARTESIAN_POINT('Ctrl Pts',(46.064224827999,-42.4871840397643,-9.));
#41519=CARTESIAN_POINT('Ctrl Pts',(45.9681025618294,-42.477643419586,-9.));
#41520=CARTESIAN_POINT('Ctrl Pts',(45.871658973384,-42.471890733761,-9.));
#41521=CARTESIAN_POINT('Ctrl Pts',(45.8389980828378,-42.469942570642,-9.));
#41522=CARTESIAN_POINT('Ctrl Pts',(45.8063002614413,-42.4684290474514,-9.));
#41523=CARTESIAN_POINT('Ctrl Pts',(45.7735749583434,-42.4673496294112,-9.));
#41524=CARTESIAN_POINT('Ctrl Pts',(45.7546017607775,-42.4667238136114,-9.));
#41525=CARTESIAN_POINT('Ctrl Pts',(45.7356172459526,-42.4662438876058,-9.));
#41526=CARTESIAN_POINT('Ctrl Pts',(45.7166298744102,-42.46590991102,-9.));
#41527=CARTESIAN_POINT('Ctrl Pts',(45.6016682057186,-42.4638878035618,-9.));
#41528=CARTESIAN_POINT('Ctrl Pts',(45.4868633730437,-42.4672155558052,-9.));
#41529=CARTESIAN_POINT('Ctrl Pts',(45.3726343407908,-42.4757909550345,-9.));
#41530=CARTESIAN_POINT('Ctrl Pts',(45.2568060982418,-42.4844864101417,-9.));
#41531=CARTESIAN_POINT('Ctrl Pts',(45.1415690483829,-42.4985772818533,-9.));
#41532=CARTESIAN_POINT('Ctrl Pts',(45.027340505856,-42.5180066648298,-9.));
#41533=CARTESIAN_POINT('Ctrl Pts',(44.9134537535134,-42.5373779119652,-9.));
#41534=CARTESIAN_POINT('Ctrl Pts',(44.8005685677885,-42.5620557089792,-9.));
#41535=CARTESIAN_POINT('Ctrl Pts',(44.6890925895062,-42.59203438769,-9.));
#41536=CARTESIAN_POINT('Ctrl Pts',(44.6225628516896,-42.609925898179,-9.));
#41537=CARTESIAN_POINT('Ctrl Pts',(44.5565349943705,-42.6297064480852,-9.));
#41538=CARTESIAN_POINT('Ctrl Pts',(44.4910967187206,-42.6513836327597,-9.));
#41539=CARTESIAN_POINT('Ctrl Pts',(44.4459984914548,-42.6663229414629,-9.));
#41540=CARTESIAN_POINT('Ctrl Pts',(44.4011803109893,-42.6821632091557,-9.));
#41541=CARTESIAN_POINT('Ctrl Pts',(44.3566714285601,-42.6989087753146,-9.));
#41542=CARTESIAN_POINT('Ctrl Pts',(44.3429060791653,-42.7040877094151,-9.));
#41543=CARTESIAN_POINT('Ctrl Pts',(44.3291728649523,-42.7093523251889,-9.));
#41544=CARTESIAN_POINT('Ctrl Pts',(44.3154805206596,-42.7146994889312,-9.));
#41545=CARTESIAN_POINT('Ctrl Pts',(44.2045216811668,-42.7580313735766,-9.));
#41546=CARTESIAN_POINT('Ctrl Pts',(44.0960958559045,-42.8068365700647,-9.));
#41547=CARTESIAN_POINT('Ctrl Pts',(43.9906304039359,-42.8610553783041,-9.));
#41548=CARTESIAN_POINT('Ctrl Pts',(43.9680107837524,-42.8726839147232,-9.));
#41549=CARTESIAN_POINT('Ctrl Pts',(43.9455273277897,-42.884561663214,-9.));
#41550=CARTESIAN_POINT('Ctrl Pts',(43.9231842511489,-42.8966883475411,-9.));
#41551=CARTESIAN_POINT('Ctrl Pts',(43.8230347394897,-42.9510444030179,-9.));
#41552=CARTESIAN_POINT('Ctrl Pts',(43.7257044811106,-43.0103978109749,-9.));
#41553=CARTESIAN_POINT('Ctrl Pts',(43.6313338306458,-43.0743591133346,-9.));
#41554=CARTESIAN_POINT('Ctrl Pts',(43.5349268596731,-43.1397005663137,-9.));
#41555=CARTESIAN_POINT('Ctrl Pts',(43.4416080440628,-43.2098513003804,-9.));
#41556=CARTESIAN_POINT('Ctrl Pts',(43.3515468190621,-43.2844468665137,-9.));
#41557=CARTESIAN_POINT('Ctrl Pts',(43.3010492668727,-43.3262727854248,-9.));
#41558=CARTESIAN_POINT('Ctrl Pts',(43.2515762599215,-43.3694969769026,-9.));
#41559=CARTESIAN_POINT('Ctrl Pts',(43.2031613209412,-43.4140612153216,-9.));
#41560=CARTESIAN_POINT('Ctrl Pts',(43.1829736128673,-43.432643286366,-9.));
#41561=CARTESIAN_POINT('Ctrl Pts',(43.1629699022135,-43.451458393887,-9.));
#41562=CARTESIAN_POINT('Ctrl Pts',(43.1431527778045,-43.4705025119526,-9.));
#41563=CARTESIAN_POINT('Ctrl Pts',(43.132421404081,-43.480815287105,-9.));
#41564=CARTESIAN_POINT('Ctrl Pts',(43.121746294682,-43.4911937816965,-9.));
#41565=CARTESIAN_POINT('Ctrl Pts',(43.1111342308463,-43.5016308664422,-9.));
#41566=CARTESIAN_POINT('Ctrl Pts',(43.0256549583025,-43.5857006972837,-9.));
#41567=CARTESIAN_POINT('Ctrl Pts',(42.9441443682772,-43.673682830914,-9.));
#41568=CARTESIAN_POINT('Ctrl Pts',(42.866748874609,-43.7651447138442,-9.));
#41569=CARTESIAN_POINT('Ctrl Pts',(42.7879338689578,-43.858284100627,-9.));
#41570=CARTESIAN_POINT('Ctrl Pts',(42.7133857019319,-43.9550325573196,-9.));
#41571=CARTESIAN_POINT('Ctrl Pts',(42.6432828812115,-44.0549833302515,-9.));
#41572=CARTESIAN_POINT('Ctrl Pts',(42.5726118605758,-44.1557442277995,-9.));
#41573=CARTESIAN_POINT('Ctrl Pts',(42.5064579319861,-44.2597602054382,-9.));
#41574=CARTESIAN_POINT('Ctrl Pts',(42.4450370917787,-44.3666560823119,-9.));
#41575=CARTESIAN_POINT('Ctrl Pts',(42.4087736821331,-44.4297683575496,-9.));
#41576=CARTESIAN_POINT('Ctrl Pts',(42.3741608145198,-44.4938852541093,-9.));
#41577=CARTESIAN_POINT('Ctrl Pts',(42.3412496253407,-44.558934856722,-9.));
#41578=CARTESIAN_POINT('Ctrl Pts',(42.3239094669499,-44.5932080155078,-9.));
#41579=CARTESIAN_POINT('Ctrl Pts',(42.3070417829367,-44.6277401515673,-9.));
#41580=CARTESIAN_POINT('Ctrl Pts',(42.2906546830202,-44.6625210933121,-9.));
#41581=CARTESIAN_POINT('Ctrl Pts',(42.2831062240436,-44.6785423852592,-9.));
#41582=CARTESIAN_POINT('Ctrl Pts',(42.2756589959128,-44.6946181175088,-9.));
#41583=CARTESIAN_POINT('Ctrl Pts',(42.2683161828643,-44.7107421228823,-9.));
#41584=CARTESIAN_POINT('Ctrl Pts',(42.2159001543897,-44.8258419244431,-9.));
#41585=CARTESIAN_POINT('Ctrl Pts',(42.168966222388,-44.943034798637,-9.));
#41586=CARTESIAN_POINT('Ctrl Pts',(42.1276953421017,-45.0618930156386,-9.));
#41587=CARTESIAN_POINT('Ctrl Pts',(42.0863446247567,-45.1809811596584,-9.));
#41588=CARTESIAN_POINT('Ctrl Pts',(42.0506783113667,-45.3017418378647,-9.));
#41589=CARTESIAN_POINT('Ctrl Pts',(42.0209163435797,-45.4237808328287,-9.));
#41590=CARTESIAN_POINT('Ctrl Pts',(41.9916671564445,-45.5437171699371,-9.));
#41591=CARTESIAN_POINT('Ctrl Pts',(41.9681201892527,-45.664888939155,-9.));
#41592=CARTESIAN_POINT('Ctrl Pts',(41.9505280204683,-45.7869452163697,-9.));
#41593=CARTESIAN_POINT('Ctrl Pts',(41.9396360398584,-45.8625148985972,-9.));
#41594=CARTESIAN_POINT('Ctrl Pts',(41.9310276093539,-45.9384240544824,-9.));
#41595=CARTESIAN_POINT('Ctrl Pts',(41.9247724176044,-46.0145920214405,-9.));
#41596=CARTESIAN_POINT('Ctrl Pts',(41.919370954043,-46.0803643453827,-9.));
#41597=CARTESIAN_POINT('Ctrl Pts',(41.9157243497761,-46.1463297083195,-9.));
#41598=CARTESIAN_POINT('Ctrl Pts',(41.9138040800513,-46.2124372338607,-9.));
#41599=CARTESIAN_POINT('Ctrl Pts',(42.5743852316216,-48.2253962475631,-9.));
#41600=CARTESIAN_POINT('Ctrl Pts',(42.6510842550578,-48.3241664787627,-9.));
#41601=CARTESIAN_POINT('Ctrl Pts',(42.7325420415582,-48.4189430401456,-9.00000000000001));
#41602=CARTESIAN_POINT('Ctrl Pts',(42.8183507401128,-48.5095866491488,-9.));
#41603=CARTESIAN_POINT('Ctrl Pts',(42.9053643616367,-48.6015030727773,-9.));
#41604=CARTESIAN_POINT('Ctrl Pts',(42.9968527373842,-48.689170063398,-9.));
#41605=CARTESIAN_POINT('Ctrl Pts',(43.0924206860801,-48.7723984663639,-9.));
#41606=CARTESIAN_POINT('Ctrl Pts',(43.13283898909,-48.8075980375173,-9.));
#41607=CARTESIAN_POINT('Ctrl Pts',(43.173987290164,-48.8420031211714,-9.));
#41608=CARTESIAN_POINT('Ctrl Pts',(43.2158367460076,-48.8755968220645,-9.));
#41609=CARTESIAN_POINT('Ctrl Pts',(43.2398457476193,-48.8948695032171,-9.));
#41610=CARTESIAN_POINT('Ctrl Pts',(43.2640899473829,-48.9138783400765,-9.));
#41611=CARTESIAN_POINT('Ctrl Pts',(43.2885385460266,-48.9326008816648,-9.));
#41612=CARTESIAN_POINT('Ctrl Pts',(43.3879651732933,-49.0087409987781,-9.));
#41613=CARTESIAN_POINT('Ctrl Pts',(43.4908354399055,-49.0802047565596,-9.));
#41614=CARTESIAN_POINT('Ctrl Pts',(43.5967559275673,-49.1468201834493,-9.));
#41615=CARTESIAN_POINT('Ctrl Pts',(43.6847795863373,-49.202179951279,-9.));
#41616=CARTESIAN_POINT('Ctrl Pts',(43.7749105352022,-49.2541906389536,-9.00000000000001));
#41617=CARTESIAN_POINT('Ctrl Pts',(43.8669315767247,-49.3027275435314,-9.00000000000001));
#41618=CARTESIAN_POINT('Ctrl Pts',(43.9071907823908,-49.3239624392841,-9.00000000000001));
#41619=CARTESIAN_POINT('Ctrl Pts',(43.9478118296589,-49.3445321151676,-9.));
#41620=CARTESIAN_POINT('Ctrl Pts',(43.9887767271923,-49.3644246152224,-9.));
#41621=CARTESIAN_POINT('Ctrl Pts',(44.011146208365,-49.37528720569,-9.));
#41622=CARTESIAN_POINT('Ctrl Pts',(44.0336182221398,-49.3859478550071,-9.));
#41623=CARTESIAN_POINT('Ctrl Pts',(44.0561898414164,-49.396404496071,-9.));
#41624=CARTESIAN_POINT('Ctrl Pts',(44.0723897277928,-49.4039093363325,-9.));
#41625=CARTESIAN_POINT('Ctrl Pts',(44.0886323780177,-49.411305127036,-9.00000000000001));
#41626=CARTESIAN_POINT('Ctrl Pts',(44.1049159223051,-49.4185911402604,-9.00000000000001));
#41627=CARTESIAN_POINT('Ctrl Pts',(44.2166372855396,-49.468580461725,-9.00000000000001));
#41628=CARTESIAN_POINT('Ctrl Pts',(44.3302932415966,-49.5134112908577,-9.));
#41629=CARTESIAN_POINT('Ctrl Pts',(44.4455169815829,-49.5529254759394,-9.));
#41630=CARTESIAN_POINT('Ctrl Pts',(44.5598774224311,-49.5921436060422,-9.));
#41631=CARTESIAN_POINT('Ctrl Pts',(44.67578306281,-49.6261246444362,-9.));
#41632=CARTESIAN_POINT('Ctrl Pts',(44.7928842528278,-49.6546636633717,-9.));
#41633=CARTESIAN_POINT('Ctrl Pts',(44.9068413606339,-49.682436430301,-9.));
#41634=CARTESIAN_POINT('Ctrl Pts',(45.0219313774996,-49.7050554811712,-9.));
#41635=CARTESIAN_POINT('Ctrl Pts',(45.1378294998974,-49.7222830855843,-9.));
#41636=CARTESIAN_POINT('Ctrl Pts',(45.2059630414309,-49.732410753544,-9.));
#41637=CARTESIAN_POINT('Ctrl Pts',(45.2743757607225,-49.7406742325277,-9.));
#41638=CARTESIAN_POINT('Ctrl Pts',(45.3429998134215,-49.7470169883357,-9.));
#41639=CARTESIAN_POINT('Ctrl Pts',(45.3908534678175,-49.7514399862849,-9.));
#41640=CARTESIAN_POINT('Ctrl Pts',(45.4388098562325,-49.7549288664261,-9.));
#41641=CARTESIAN_POINT('Ctrl Pts',(45.4868453505332,-49.7574626301393,-9.));
#41642=CARTESIAN_POINT('Ctrl Pts',(45.5023235914912,-49.7582790723526,-9.));
#41643=CARTESIAN_POINT('Ctrl Pts',(45.5178066093579,-49.7589961163705,-9.00000000000001));
#41644=CARTESIAN_POINT('Ctrl Pts',(45.5332851460771,-49.7596129312151,-9.00000000000001));
#41645=CARTESIAN_POINT('Ctrl Pts',(45.6490326352122,-49.764225432436,-9.00000000000001));
#41646=CARTESIAN_POINT('Ctrl Pts',(45.764670435547,-49.7632450163518,-9.));
#41647=CARTESIAN_POINT('Ctrl Pts',(45.8798848286888,-49.7564882368775,-9.));
#41648=CARTESIAN_POINT('Ctrl Pts',(45.9071546175464,-49.7548889926807,-9.));
#41649=CARTESIAN_POINT('Ctrl Pts',(45.9344006665752,-49.752965923366,-9.00000000000001));
#41650=CARTESIAN_POINT('Ctrl Pts',(45.9616187611747,-49.7507161676903,-9.00000000000001));
#41651=CARTESIAN_POINT('Ctrl Pts',(46.0782931677331,-49.7410722557185,-9.00000000000001));
#41652=CARTESIAN_POINT('Ctrl Pts',(46.1944552709857,-49.725429296288,-9.));
#41653=CARTESIAN_POINT('Ctrl Pts',(46.3097422789741,-49.7040305580922,-9.));
#41654=CARTESIAN_POINT('Ctrl Pts',(46.4259795694295,-49.6824554353576,-9.));
#41655=CARTESIAN_POINT('Ctrl Pts',(46.5413280980213,-49.6550287317031,-9.));
#41656=CARTESIAN_POINT('Ctrl Pts',(46.6553913624472,-49.6219534192776,-9.));
#41657=CARTESIAN_POINT('Ctrl Pts',(46.7119959587765,-49.6055395921112,-9.));
#41658=CARTESIAN_POINT('Ctrl Pts',(46.7682835756122,-49.5877340165484,-9.));
#41659=CARTESIAN_POINT('Ctrl Pts',(46.8242025716789,-49.5685579250005,-9.));
#41660=CARTESIAN_POINT('Ctrl Pts',(46.8468231694633,-49.5608007282607,-9.));
#41661=CARTESIAN_POINT('Ctrl Pts',(46.8693834188428,-49.5528192356515,-9.));
#41662=CARTESIAN_POINT('Ctrl Pts',(46.8918797845697,-49.5446147561897,-9.));
#41663=CARTESIAN_POINT('Ctrl Pts',(46.907099956639,-49.5390639223056,-9.));
#41664=CARTESIAN_POINT('Ctrl Pts',(46.9222905170742,-49.5334110892113,-9.));
#41665=CARTESIAN_POINT('Ctrl Pts',(46.9374375956582,-49.5276616978241,-9.));
#41666=CARTESIAN_POINT('Ctrl Pts',(47.0458981301604,-49.4864932269893,-9.));
#41667=CARTESIAN_POINT('Ctrl Pts',(47.1523014498086,-49.4403165384569,-9.));
#41668=CARTESIAN_POINT('Ctrl Pts',(47.2563056915469,-49.3893803260793,-9.));
#41669=CARTESIAN_POINT('Ctrl Pts',(47.3602083916416,-49.3384938438533,-9.));
#41670=CARTESIAN_POINT('Ctrl Pts',(47.4617174352489,-49.2828565194432,-9.));
#41671=CARTESIAN_POINT('Ctrl Pts',(47.5604628206564,-49.222673454704,-9.));
#41672=CARTESIAN_POINT('Ctrl Pts',(47.6578162292091,-49.1633387681732,-9.));
#41673=CARTESIAN_POINT('Ctrl Pts',(47.7524839476778,-49.0995849704782,-9.));
#41674=CARTESIAN_POINT('Ctrl Pts',(47.8440732492731,-49.0315762020744,-9.));
#41675=CARTESIAN_POINT('Ctrl Pts',(47.8943353485933,-48.9942545562859,-9.));
#41676=CARTESIAN_POINT('Ctrl Pts',(47.9436696390876,-48.9556509834542,-9.));
#41677=CARTESIAN_POINT('Ctrl Pts',(47.9920052439302,-48.9157893805739,-9.));
#41678=CARTESIAN_POINT('Ctrl Pts',(48.0190282317517,-48.8935039532438,-9.));
#41679=CARTESIAN_POINT('Ctrl Pts',(48.0457389902699,-48.8708252799141,-9.));
#41680=CARTESIAN_POINT('Ctrl Pts',(48.072124481961,-48.8477572841386,-9.));
#41681=CARTESIAN_POINT('Ctrl Pts',(48.0885412369069,-48.8334046376852,-9.));
#41682=CARTESIAN_POINT('Ctrl Pts',(48.1048355682913,-48.8188979730226,-9.));
#41683=CARTESIAN_POINT('Ctrl Pts',(48.1209823789593,-48.8042583984171,-9.));
#41684=CARTESIAN_POINT('Ctrl Pts',(48.2035982369658,-48.7293543791815,-9.));
#41685=CARTESIAN_POINT('Ctrl Pts',(48.2824582102327,-48.6508865866008,-9.));
#41686=CARTESIAN_POINT('Ctrl Pts',(48.3572280393153,-48.5690423763841,-9.));
#41687=CARTESIAN_POINT('Ctrl Pts',(48.4308862472868,-48.4884149638116,-9.));
#41688=CARTESIAN_POINT('Ctrl Pts',(48.5005755215514,-48.4045101950566,-9.));
#41689=CARTESIAN_POINT('Ctrl Pts',(48.565933985507,-48.3174806712345,-9.));
#41690=CARTESIAN_POINT('Ctrl Pts',(48.6294066043965,-48.23296228657,-9.));
#41691=CARTESIAN_POINT('Ctrl Pts',(48.6887950229853,-48.1454963378325,-9.));
#41692=CARTESIAN_POINT('Ctrl Pts',(48.7437220341769,-48.0552055938548,-9.));
#41693=CARTESIAN_POINT('Ctrl Pts',(48.771376110491,-48.0097469557412,-9.));
#41694=CARTESIAN_POINT('Ctrl Pts',(48.7978985435134,-47.9635720608222,-9.));
#41695=CARTESIAN_POINT('Ctrl Pts',(48.8232362548565,-47.9166954935817,-9.));
#41696=CARTESIAN_POINT('Ctrl Pts',(48.8494364512248,-47.8682232677308,-9.));
#41697=CARTESIAN_POINT('Ctrl Pts',(48.8743698413062,-47.8190007093841,-9.));
#41698=CARTESIAN_POINT('Ctrl Pts',(48.8980278172144,-47.7690799369094,-9.));
#41699=CARTESIAN_POINT('Origin',(46.,-46.,2.76038497140452));
#41700=CARTESIAN_POINT('Ctrl Pts',(41.9098425569998,-45.9981377324218,-0.364615028595479));
#41701=CARTESIAN_POINT('Ctrl Pts',(41.9091325173901,-45.879255340082,-0.370425837919348));
#41702=CARTESIAN_POINT('Ctrl Pts',(41.9672597965486,-44.4253404423929,-0.441524166511649));
#41703=CARTESIAN_POINT('Ctrl Pts',(43.700874641208,-41.7778217753375,-0.577910014372381));
#41704=CARTESIAN_POINT('Ctrl Pts',(48.2448534714975,-41.7491667594488,-0.773772572177674));
#41705=CARTESIAN_POINT('Ctrl Pts',(50.7830591782025,-45.5179447043461,-0.969635129982967));
#41706=CARTESIAN_POINT('Ctrl Pts',(49.0478255306161,-49.7176766340539,-1.16549768778826));
#41707=CARTESIAN_POINT('Ctrl Pts',(44.5894569428605,-50.5956818776348,-1.36136024559355));
#41708=CARTESIAN_POINT('Ctrl Pts',(42.1450235329037,-48.1283900611451,-1.51106602586263));
#41709=CARTESIAN_POINT('Ctrl Pts',(41.9140056632401,-46.3965852194679,-1.59548428686327));
#41710=CARTESIAN_POINT('Ctrl Pts',(41.9171327032046,-46.0033110738038,-1.61461502859548));
#41711=CARTESIAN_POINT('Ctrl Pts',(41.9194196464784,-46.0038358614086,-0.260384971404518));
#41712=CARTESIAN_POINT('Ctrl Pts',(41.9254629522515,-45.1031478464201,-0.304165019473208));
#41713=CARTESIAN_POINT('Ctrl Pts',(42.6573083539943,-42.8475830013967,-0.413232586810328));
#41714=CARTESIAN_POINT('Ctrl Pts',(46.3558078226787,-41.2067330502749,-0.58758767341588));
#41715=CARTESIAN_POINT('Ctrl Pts',(50.1895243958238,-43.6427681215851,-0.783450231221173));
#41716=CARTESIAN_POINT('Ctrl Pts',(50.2815817385072,-48.1865095580738,-0.979312789026466));
#41717=CARTESIAN_POINT('Ctrl Pts',(46.547466535547,-50.7759010051096,-1.17517534683176));
#41718=CARTESIAN_POINT('Ctrl Pts',(42.7307419251195,-49.2599206787868,-1.35219940762444));
#41719=CARTESIAN_POINT('Ctrl Pts',(41.9246674400896,-46.9514404731118,-1.4639359491487));
#41720=CARTESIAN_POINT('Ctrl Pts',(41.9169762239431,-45.9966653623493,-1.51038497140452));
#41721=CARTESIAN_POINT('Ctrl Pts',(48.5732344270147,-43.7934484719077,0.));
#41722=CARTESIAN_POINT('Ctrl Pts',(49.2973603516436,-44.6379090408209,-0.0652875192684312));
#41723=CARTESIAN_POINT('Ctrl Pts',(49.8377909604978,-47.0815093877498,-0.195862557805293));
#41724=CARTESIAN_POINT('Ctrl Pts',(47.2195289512052,-49.8003259140453,-0.391725115610587));
#41725=CARTESIAN_POINT('Ctrl Pts',(43.5104537866883,-49.1160268913033,-0.58758767341588));
#41726=CARTESIAN_POINT('Ctrl Pts',(42.0262712437735,-45.6513999754492,-0.783450231221174));
#41727=CARTESIAN_POINT('Ctrl Pts',(44.0921762093107,-42.4964189382987,-0.979312789026468));
#41728=CARTESIAN_POINT('Ctrl Pts',(47.8627887527562,-42.4726408868645,-1.17517534683176));
#41729=CARTESIAN_POINT('Ctrl Pts',(49.9690024110922,-45.5999885095611,-1.37103790463705));
#41730=CARTESIAN_POINT('Ctrl Pts',(48.5290983090345,-49.0849435422972,-1.56690046244235));
#41731=CARTESIAN_POINT('Ctrl Pts',(44.8295255011166,-49.8135159472981,-1.76276302024764));
#41732=CARTESIAN_POINT('Ctrl Pts',(42.1757347751709,-47.1349090709021,-1.95862557805294));
#41733=CARTESIAN_POINT('Ctrl Pts',(42.9387743307483,-43.4422796081895,-2.15448813585823));
#41734=CARTESIAN_POINT('Ctrl Pts',(46.436903464158,-42.034887332994,-2.35035069366352));
#41735=CARTESIAN_POINT('Ctrl Pts',(49.5446751782708,-44.1701650985836,-2.54621325146882));
#41736=CARTESIAN_POINT('Ctrl Pts',(49.485416115998,-47.9403330390778,-2.74207580927411));
#41737=CARTESIAN_POINT('Ctrl Pts',(46.3120712894746,-49.9768864478569,-2.9379383670794));
#41738=CARTESIAN_POINT('Ctrl Pts',(42.8599028524774,-48.4602451351121,-3.13380092488469));
#41739=CARTESIAN_POINT('Ctrl Pts',(42.2132906545528,-44.7454688702612,-3.32966348268999));
#41740=CARTESIAN_POINT('Ctrl Pts',(44.9499579596742,-42.1515681913754,-3.52552604049528));
#41741=CARTESIAN_POINT('Ctrl Pts',(48.6247975171733,-42.9960935595406,-3.72138859830058));
#41742=CARTESIAN_POINT('Ctrl Pts',(49.9544812319427,-46.524494090566,-3.91725115610587));
#41743=CARTESIAN_POINT('Ctrl Pts',(47.7509877249507,-49.5842792607275,-4.11311371391117));
#41744=CARTESIAN_POINT('Ctrl Pts',(43.983053885447,-49.4416484758484,-4.30897627171645));
#41745=CARTESIAN_POINT('Ctrl Pts',(42.017183993459,-46.2240368540166,-4.50483882952175));
#41746=CARTESIAN_POINT('Ctrl Pts',(43.6098073546396,-42.8062569035684,-4.70070138732704));
#41747=CARTESIAN_POINT('Ctrl Pts',(47.3379761142184,-42.241963841087,-4.89656394513234));
#41748=CARTESIAN_POINT('Ctrl Pts',(49.8707145657737,-45.0353318650296,-5.09242650293763));
#41749=CARTESIAN_POINT('Ctrl Pts',(48.9451180958786,-48.6905938439567,-5.28828906074293));
#41750=CARTESIAN_POINT('Ctrl Pts',(45.3881716416347,-49.9419134851903,-5.48415161854822));
#41751=CARTESIAN_POINT('Ctrl Pts',(42.3778703273949,-47.6712846986755,-5.68001417635351));
#41752=CARTESIAN_POINT('Ctrl Pts',(42.6038029048162,-43.9074271905735,-5.8758767341588));
#41753=CARTESIAN_POINT('Ctrl Pts',(45.864107175315,-42.0132031450575,-6.0717392919641));
#41754=CARTESIAN_POINT('Ctrl Pts',(49.2458266222607,-43.6810291595308,-6.26760184976939));
#41755=CARTESIAN_POINT('Ctrl Pts',(49.7275242358509,-47.4207664762398,-6.46346440757469));
#41756=CARTESIAN_POINT('Ctrl Pts',(46.878822635117,-49.8911037740211,-6.65932696537998));
#41757=CARTESIAN_POINT('Ctrl Pts',(43.244925432142,-48.8848885613543,-6.85518952318528));
#41758=CARTESIAN_POINT('Ctrl Pts',(42.0725842897717,-45.3011373968387,-7.05105208099057));
#41759=CARTESIAN_POINT('Ctrl Pts',(44.4092329111238,-42.3417905650828,-7.24691463879586));
#41760=CARTESIAN_POINT('Ctrl Pts',(48.1671820163374,-42.6509187502963,-7.44277719660115));
#41761=CARTESIAN_POINT('Ctrl Pts',(49.9888143927997,-45.9523117139429,-7.63863975440644));
#41762=CARTESIAN_POINT('Ctrl Pts',(48.2466407242209,-49.2963343841598,-7.83450231221174));
#41763=CARTESIAN_POINT('Ctrl Pts',(44.4970846743848,-49.6951637116331,-8.03036487001703));
#41764=CARTESIAN_POINT('Ctrl Pts',(42.0905201956602,-46.7925982020384,-8.22622742782233));
#41765=CARTESIAN_POINT('Ctrl Pts',(43.1765285368071,-43.1816883123461,-8.42208998562762));
#41766=CARTESIAN_POINT('Ctrl Pts',(46.7860124730819,-42.08921662613,-8.61795254343292));
#41767=CARTESIAN_POINT('Ctrl Pts',(49.6915640274424,-44.4900930602074,-8.81381510123821));
#41768=CARTESIAN_POINT('Ctrl Pts',(49.302253143976,-48.24161818535,-9.0096776590435));
#41769=CARTESIAN_POINT('Ctrl Pts',(45.9554882647734,-49.987019026503,-9.2055402168488));
#41770=CARTESIAN_POINT('Ctrl Pts',(43.7634250628647,-48.7794980878294,-9.33611525538566));
#41771=CARTESIAN_POINT('Ctrl Pts',(43.1574106092752,-47.8466430673628,-9.40140277465409));
#41772=CARTESIAN_POINT('Ctrl Pts',(48.7491609934165,-43.6425912356409,0.133800924884696));
#41773=CARTESIAN_POINT('Ctrl Pts',(49.5227938678302,-44.5447857781054,0.0685134056162645));
#41774=CARTESIAN_POINT('Ctrl Pts',(50.1001725683141,-47.1554498850168,-0.0620616329205977));
#41775=CARTESIAN_POINT('Ctrl Pts',(47.3029055525598,-50.0601461162962,-0.257924190725891));
#41776=CARTESIAN_POINT('Ctrl Pts',(43.3402488055142,-49.3290630243691,-0.453786748531185));
#41777=CARTESIAN_POINT('Ctrl Pts',(41.7545958579027,-45.627566932986,-0.649649306336477));
#41778=CARTESIAN_POINT('Ctrl Pts',(43.9617423532765,-42.256886550645,-0.845511864141773));
#41779=CARTESIAN_POINT('Ctrl Pts',(47.9901436590033,-42.2314828443926,-1.04137442194706));
#41780=CARTESIAN_POINT('Ctrl Pts',(50.2403546667957,-45.5726405744894,-1.23723697975236));
#41781=CARTESIAN_POINT('Ctrl Pts',(48.702007382895,-49.2958545728828,-1.43309953755765));
#41782=CARTESIAN_POINT('Ctrl Pts',(44.7495026483646,-50.0742379240769,-1.62896209536295));
#41783=CARTESIAN_POINT('Ctrl Pts',(41.9142778931429,-47.2125003909646,-1.82482465316824));
#41784=CARTESIAN_POINT('Ctrl Pts',(42.7294848407124,-43.2674137033876,-2.02068721097353));
#41785=CARTESIAN_POINT('Ctrl Pts',(46.4667736250309,-41.7638010108231,-2.21654976877883));
#41786=CARTESIAN_POINT('Ctrl Pts',(49.7870170832974,-44.045063177084,-2.41241232658412));
#41787=CARTESIAN_POINT('Ctrl Pts',(49.7237066049375,-48.0729894833012,-2.60827488438941));
#41788=CARTESIAN_POINT('Ctrl Pts',(46.3334069399903,-50.2487777183904,-2.80413744219471));
#41789=CARTESIAN_POINT('Ctrl Pts',(42.6452210871736,-48.6284468638715,-3.));
#41790=CARTESIAN_POINT('Ctrl Pts',(41.9544013881446,-44.659699244384,-3.19586255780529));
#41791=CARTESIAN_POINT('Ctrl Pts',(44.8781688180426,-41.8884590913979,-3.39172511561059));
#41792=CARTESIAN_POINT('Ctrl Pts',(48.8042493424128,-42.7907228633015,-3.58758767341588));
#41793=CARTESIAN_POINT('Ctrl Pts',(50.2248407055034,-46.5603526363256,-3.78345023122117));
#41794=CARTESIAN_POINT('Ctrl Pts',(47.8706990326452,-49.8293288126631,-3.97931278902647));
#41795=CARTESIAN_POINT('Ctrl Pts',(43.8451595681529,-49.6769466642923,-4.17517534683176));
#41796=CARTESIAN_POINT('Ctrl Pts',(41.7448873316061,-46.2393537773645,-4.37103790463705));
#41797=CARTESIAN_POINT('Ctrl Pts',(43.4463949656544,-42.5879074788031,-4.56690046244235));
#41798=CARTESIAN_POINT('Ctrl Pts',(47.4294506962584,-41.9850348994753,-4.76276302024764));
#41799=CARTESIAN_POINT('Ctrl Pts',(50.1353470904784,-44.9693795557798,-4.95862557805293));
#41800=CARTESIAN_POINT('Ctrl Pts',(49.1464695579982,-48.8745440241578,-5.15448813585823));
#41801=CARTESIAN_POINT('Ctrl Pts',(45.3463422376812,-50.211413728628,-5.35035069366352));
#41802=CARTESIAN_POINT('Ctrl Pts',(42.1302330232793,-47.7855468799332,-5.54621325146881));
#41803=CARTESIAN_POINT('Ctrl Pts',(42.3716121306267,-43.7643624369532,-5.74207580927411));
#41804=CARTESIAN_POINT('Ctrl Pts',(45.8548164718352,-41.7406343210637,-5.9379383670794));
#41805=CARTESIAN_POINT('Ctrl Pts',(49.4677368869436,-43.5224860539098,-6.1338009248847));
#41806=CARTESIAN_POINT('Ctrl Pts',(49.9823671421591,-47.5179012592972,-6.32966348268999));
#41807=CARTESIAN_POINT('Ctrl Pts',(46.9389058700719,-50.157130265541,-6.52552604049529));
#41808=CARTESIAN_POINT('Ctrl Pts',(43.0565668419507,-49.0821222582622,-6.72138859830057));
#41809=CARTESIAN_POINT('Ctrl Pts',(41.8040752283821,-45.2533576466263,-6.91725115610587));
#41810=CARTESIAN_POINT('Ctrl Pts',(44.3004755476465,-42.0916865643329,-7.11311371391116));
#41811=CARTESIAN_POINT('Ctrl Pts',(48.3153476427955,-42.4219491862816,-7.30897627171646));
#41812=CARTESIAN_POINT('Ctrl Pts',(50.2615211515669,-45.949051367223,-7.50483882952175));
#41813=CARTESIAN_POINT('Ctrl Pts',(48.4002387735869,-49.5216977571311,-7.70070138732704));
#41814=CARTESIAN_POINT('Ctrl Pts',(44.3943335491657,-49.9477941977075,-7.89656394513234));
#41815=CARTESIAN_POINT('Ctrl Pts',(41.8232373740198,-46.8467864558395,-8.09242650293763));
#41816=CARTESIAN_POINT('Ctrl Pts',(42.9834937963114,-42.989006334733,-8.28828906074292));
#41817=CARTESIAN_POINT('Ctrl Pts',(46.8397504745972,-41.8218446822126,-8.48415161854822));
#41818=CARTESIAN_POINT('Ctrl Pts',(49.9439484107626,-44.386863933193,-8.68001417635351));
#41819=CARTESIAN_POINT('Ctrl Pts',(49.5280211699711,-48.3948728544126,-8.8758767341588));
#41820=CARTESIAN_POINT('Ctrl Pts',(45.9524450920796,-50.2596030398939,-9.07173929196411));
#41821=CARTESIAN_POINT('Ctrl Pts',(43.6105151899593,-48.9695264621503,-9.20231433050096));
#41822=CARTESIAN_POINT('Ctrl Pts',(42.963068816724,-47.9728941274296,-9.2676018497694));
#41823=CARTESIAN_POINT('Ctrl Pts',(48.9250875598184,-43.4917339993741,0.267601849769391));
#41824=CARTESIAN_POINT('Ctrl Pts',(49.7482273840168,-44.45166251539,0.20231433050096));
#41825=CARTESIAN_POINT('Ctrl Pts',(50.3625541761304,-47.2293903822839,0.071739291964098));
#41826=CARTESIAN_POINT('Ctrl Pts',(47.3862821539145,-50.3199663185471,-0.124123265841196));
#41827=CARTESIAN_POINT('Ctrl Pts',(43.17004382434,-49.5420991574348,-0.319985823646489));
#41828=CARTESIAN_POINT('Ctrl Pts',(41.482920472032,-45.6037338905227,-0.515848381451783));
#41829=CARTESIAN_POINT('Ctrl Pts',(43.8313084972421,-42.0173541629913,-0.711710939257076));
#41830=CARTESIAN_POINT('Ctrl Pts',(48.1174985652505,-41.9903248019207,-0.907573497062369));
#41831=CARTESIAN_POINT('Ctrl Pts',(50.511706922499,-45.5452926394177,-1.10343605486766));
#41832=CARTESIAN_POINT('Ctrl Pts',(48.8749164567556,-49.5067656034683,-1.29929861267296));
#41833=CARTESIAN_POINT('Ctrl Pts',(44.6694797956125,-50.3349599008559,-1.49516117047825));
#41834=CARTESIAN_POINT('Ctrl Pts',(41.652821011115,-47.290091711027,-1.69102372828354));
#41835=CARTESIAN_POINT('Ctrl Pts',(42.5201953506765,-43.0925477985858,-1.88688628608884));
#41836=CARTESIAN_POINT('Ctrl Pts',(46.4966437859037,-41.4927146886523,-2.08274884389413));
#41837=CARTESIAN_POINT('Ctrl Pts',(50.0293589883241,-43.9199612555844,-2.27861140169942));
#41838=CARTESIAN_POINT('Ctrl Pts',(49.961997093877,-48.2056459275246,-2.47447395950472));
#41839=CARTESIAN_POINT('Ctrl Pts',(46.354742590506,-50.5206689889239,-2.67033651731001));
#41840=CARTESIAN_POINT('Ctrl Pts',(42.4305393218699,-48.7966485926308,-2.8661990751153));
#41841=CARTESIAN_POINT('Ctrl Pts',(41.6955121217363,-44.5739296185069,-3.0620616329206));
#41842=CARTESIAN_POINT('Ctrl Pts',(44.8063796764111,-41.6253499914204,-3.25792419072589));
#41843=CARTESIAN_POINT('Ctrl Pts',(48.983701167652,-42.5853521670624,-3.45378674853119));
#41844=CARTESIAN_POINT('Ctrl Pts',(50.4952001790642,-46.5962111820853,-3.64964930633648));
#41845=CARTESIAN_POINT('Ctrl Pts',(47.9904103403397,-50.0743783645986,-3.84551186414178));
#41846=CARTESIAN_POINT('Ctrl Pts',(43.7072652508588,-49.9122448527363,-4.04137442194706));
#41847=CARTESIAN_POINT('Ctrl Pts',(41.4725906697532,-46.2546707007123,-4.23723697975236));
#41848=CARTESIAN_POINT('Ctrl Pts',(43.2829825766694,-42.3695580540379,-4.43309953755765));
#41849=CARTESIAN_POINT('Ctrl Pts',(47.5209252782984,-41.7281059578637,-4.62896209536295));
#41850=CARTESIAN_POINT('Ctrl Pts',(50.3999796151832,-44.9034272465301,-4.82482465316824));
#41851=CARTESIAN_POINT('Ctrl Pts',(49.3478210201178,-49.058494204359,-5.02068721097353));
#41852=CARTESIAN_POINT('Ctrl Pts',(45.3045128337278,-50.4809139720657,-5.21654976877883));
#41853=CARTESIAN_POINT('Ctrl Pts',(41.8825957191635,-47.8998090611908,-5.41241232658412));
#41854=CARTESIAN_POINT('Ctrl Pts',(42.1394213564373,-43.6212976833329,-5.60827488438942));
#41855=CARTESIAN_POINT('Ctrl Pts',(45.8455257683553,-41.4680654970699,-5.80413744219471));
#41856=CARTESIAN_POINT('Ctrl Pts',(49.6896471516265,-43.3639429482889,-6.));
#41857=CARTESIAN_POINT('Ctrl Pts',(50.2372100484674,-47.6150360423544,-6.19586255780529));
#41858=CARTESIAN_POINT('Ctrl Pts',(46.9989891050268,-50.4231567570609,-6.39172511561059));
#41859=CARTESIAN_POINT('Ctrl Pts',(42.8682082517594,-49.2793559551702,-6.58758767341588));
#41860=CARTESIAN_POINT('Ctrl Pts',(41.5355661669926,-45.2055778964139,-6.78345023122117));
#41861=CARTESIAN_POINT('Ctrl Pts',(44.1917181841692,-41.8415825635829,-6.97931278902647));
#41862=CARTESIAN_POINT('Ctrl Pts',(48.4635132692535,-42.1929796222669,-7.17517534683176));
#41863=CARTESIAN_POINT('Ctrl Pts',(50.5342279103342,-45.9457910205032,-7.37103790463706));
#41864=CARTESIAN_POINT('Ctrl Pts',(48.5538368229528,-49.7470611301022,-7.56690046244235));
#41865=CARTESIAN_POINT('Ctrl Pts',(44.2915824239466,-50.200424683782,-7.76276302024764));
#41866=CARTESIAN_POINT('Ctrl Pts',(41.5559545523793,-46.9009747096407,-7.95862557805294));
#41867=CARTESIAN_POINT('Ctrl Pts',(42.7904590558158,-42.79632435712,-8.15448813585823));
#41868=CARTESIAN_POINT('Ctrl Pts',(46.8934884761126,-41.554472738295,-8.35035069366352));
#41869=CARTESIAN_POINT('Ctrl Pts',(50.1963327940828,-44.2836348061786,-8.54621325146883));
#41870=CARTESIAN_POINT('Ctrl Pts',(49.753789195966,-48.5481275234752,-8.7420758092741));
#41871=CARTESIAN_POINT('Ctrl Pts',(45.9494019193858,-50.5321870532849,-8.93793836707941));
#41872=CARTESIAN_POINT('Ctrl Pts',(43.4576053170538,-49.1595548364713,-9.06851340561627));
#41873=CARTESIAN_POINT('Ctrl Pts',(42.7687270241728,-48.0991451874963,-9.1338009248847));
#41874=CARTESIAN_POINT('Ctrl Pts',(49.1010141262202,-43.3408767631073,0.401402774654087));
#41875=CARTESIAN_POINT('Ctrl Pts',(49.9736609002034,-44.3585392526745,0.336115255385656));
#41876=CARTESIAN_POINT('Ctrl Pts',(50.6249357839467,-47.303330879551,0.205540216848794));
#41877=CARTESIAN_POINT('Ctrl Pts',(47.469658755269,-50.579786520798,0.00967765904349996));
#41878=CARTESIAN_POINT('Ctrl Pts',(42.999838843166,-49.7551352905006,-0.186184898761793));
#41879=CARTESIAN_POINT('Ctrl Pts',(41.2112450861611,-45.5799008480595,-0.382047456567087));
#41880=CARTESIAN_POINT('Ctrl Pts',(43.700874641208,-41.7778217753375,-0.577910014372381));
#41881=CARTESIAN_POINT('Ctrl Pts',(48.2448534714975,-41.7491667594488,-0.773772572177674));
#41882=CARTESIAN_POINT('Ctrl Pts',(50.7830591782025,-45.5179447043461,-0.969635129982967));
#41883=CARTESIAN_POINT('Ctrl Pts',(49.0478255306161,-49.7176766340539,-1.16549768778826));
#41884=CARTESIAN_POINT('Ctrl Pts',(44.5894569428605,-50.5956818776348,-1.36136024559355));
#41885=CARTESIAN_POINT('Ctrl Pts',(41.3913641290871,-47.3676830310895,-1.55722280339885));
#41886=CARTESIAN_POINT('Ctrl Pts',(42.3109058606407,-42.9176818937838,-1.75308536120414));
#41887=CARTESIAN_POINT('Ctrl Pts',(46.5265139467765,-41.2216283664815,-1.94894791900943));
#41888=CARTESIAN_POINT('Ctrl Pts',(50.2717008933508,-43.7948593340848,-2.14481047681473));
#41889=CARTESIAN_POINT('Ctrl Pts',(50.2002875828164,-48.338302371748,-2.34067303462002));
#41890=CARTESIAN_POINT('Ctrl Pts',(46.3760782410217,-50.7925602594573,-2.53653559242531));
#41891=CARTESIAN_POINT('Ctrl Pts',(42.2158575565662,-48.9648503213903,-2.73239815023061));
#41892=CARTESIAN_POINT('Ctrl Pts',(41.436622855328,-44.4881599926298,-2.9282607080359));
#41893=CARTESIAN_POINT('Ctrl Pts',(44.7345905347796,-41.3622408914429,-3.12412326584119));
#41894=CARTESIAN_POINT('Ctrl Pts',(49.1631529928913,-42.3799814708233,-3.31998582364649));
#41895=CARTESIAN_POINT('Ctrl Pts',(50.765559652625,-46.6320697278449,-3.51584838145178));
#41896=CARTESIAN_POINT('Ctrl Pts',(48.1101216480341,-50.3194279165342,-3.71171093925708));
#41897=CARTESIAN_POINT('Ctrl Pts',(43.5693709335647,-50.1475430411802,-3.90757349706237));
#41898=CARTESIAN_POINT('Ctrl Pts',(41.2002940079003,-46.2699876240602,-4.10343605486767));
#41899=CARTESIAN_POINT('Ctrl Pts',(43.1195701876843,-42.1512086292726,-4.29929861267295));
#41900=CARTESIAN_POINT('Ctrl Pts',(47.6123998603384,-41.4711770162521,-4.49516117047826));
#41901=CARTESIAN_POINT('Ctrl Pts',(50.6646121398881,-44.8374749372802,-4.69102372828354));
#41902=CARTESIAN_POINT('Ctrl Pts',(49.5491724822373,-49.2424443845602,-4.88688628608884));
#41903=CARTESIAN_POINT('Ctrl Pts',(45.2626834297744,-50.7504142155033,-5.08274884389412));
#41904=CARTESIAN_POINT('Ctrl Pts',(41.6349584150478,-48.0140712424484,-5.27861140169943));
#41905=CARTESIAN_POINT('Ctrl Pts',(41.9072305822478,-43.4782329297126,-5.47447395950471));
#41906=CARTESIAN_POINT('Ctrl Pts',(45.8362350648755,-41.1954966730761,-5.67033651731001));
#41907=CARTESIAN_POINT('Ctrl Pts',(49.9115574163095,-43.2053998426678,-5.86619907511531));
#41908=CARTESIAN_POINT('Ctrl Pts',(50.4920529547756,-47.7121708254118,-6.0620616329206));
#41909=CARTESIAN_POINT('Ctrl Pts',(47.0590723399817,-50.6891832485807,-6.25792419072589));
#41910=CARTESIAN_POINT('Ctrl Pts',(42.679849661568,-49.4765896520782,-6.45378674853119));
#41911=CARTESIAN_POINT('Ctrl Pts',(41.267057105603,-45.1577981462014,-6.64964930633648));
#41912=CARTESIAN_POINT('Ctrl Pts',(44.0829608206919,-41.591478562833,-6.84551186414177));
#41913=CARTESIAN_POINT('Ctrl Pts',(48.6116788957116,-41.9640100582522,-7.04137442194706));
#41914=CARTESIAN_POINT('Ctrl Pts',(50.8069346691015,-45.9425306737833,-7.23723697975236));
#41915=CARTESIAN_POINT('Ctrl Pts',(48.7074348723187,-49.9724245030734,-7.43309953755765));
#41916=CARTESIAN_POINT('Ctrl Pts',(44.1888312987275,-50.4530551698565,-7.62896209536294));
#41917=CARTESIAN_POINT('Ctrl Pts',(41.2886717307389,-46.9551629634418,-7.82482465316825));
#41918=CARTESIAN_POINT('Ctrl Pts',(42.5974243153202,-42.603642379507,-8.02068721097353));
#41919=CARTESIAN_POINT('Ctrl Pts',(46.947226477628,-41.2871007943775,-8.21654976877883));
#41920=CARTESIAN_POINT('Ctrl Pts',(50.4487171774031,-44.1804056791643,-8.41241232658412));
#41921=CARTESIAN_POINT('Ctrl Pts',(49.979557221961,-48.7013821925377,-8.60827488438941));
#41922=CARTESIAN_POINT('Ctrl Pts',(45.946358746692,-50.8047710666759,-8.80413744219471));
#41923=CARTESIAN_POINT('Ctrl Pts',(43.3046954441484,-49.3495832107922,-8.93471248073157));
#41924=CARTESIAN_POINT('Ctrl Pts',(42.5743852316216,-48.2253962475631,-9.));
#41925=CARTESIAN_POINT('Ctrl Pts',(48.5732344270147,-43.7934484719077,0.));
#41926=CARTESIAN_POINT('Ctrl Pts',(48.6498724033581,-43.8663851681741,3.87614628204605E-17));
#41927=CARTESIAN_POINT('Ctrl Pts',(48.7225776093513,-43.942957995891,-1.95539500540648E-17));
#41928=CARTESIAN_POINT('Ctrl Pts',(48.7913525374548,-44.022751380685,4.85722573273506E-17));
#41929=CARTESIAN_POINT('Ctrl Pts',(48.8618446331577,-44.1045370411351,1.1839943509454E-16));
#41930=CARTESIAN_POINT('Ctrl Pts',(48.9282081375236,-44.1897064969362,3.17350500352468E-16));
#41931=CARTESIAN_POINT('Ctrl Pts',(48.9904195836878,-44.2778605693834,3.05311331771918E-16));
#41932=CARTESIAN_POINT('Ctrl Pts',(49.0539465298674,-44.3678787149361,2.9301758742712E-16));
#41933=CARTESIAN_POINT('Ctrl Pts',(49.1131444138394,-44.4610095732985,3.8989011672772E-16));
#41934=CARTESIAN_POINT('Ctrl Pts',(49.1679548280974,-44.5568705359006,3.67761376907083E-16));
#41935=CARTESIAN_POINT('Ctrl Pts',(49.2206156820432,-44.6489720136768,3.4650048421955E-16));
#41936=CARTESIAN_POINT('Ctrl Pts',(49.2692265344368,-44.7435944760072,-5.92281301081711E-19));
#41937=CARTESIAN_POINT('Ctrl Pts',(49.3137017428961,-44.8404267203043,2.77555756156289E-17));
#41938=CARTESIAN_POINT('Ctrl Pts',(49.3201147960405,-44.8543893379128,3.18431632680741E-17));
#41939=CARTESIAN_POINT('Ctrl Pts',(49.3264418005973,-44.8683979386779,1.52397213062401E-16));
#41940=CARTESIAN_POINT('Ctrl Pts',(49.3326824371613,-44.8824516252654,1.66533453693773E-16));
#41941=CARTESIAN_POINT('Ctrl Pts',(49.3392327263543,-44.8972026383122,1.81371117013511E-16));
#41942=CARTESIAN_POINT('Ctrl Pts',(49.345684301834,-44.9119953356503,-6.93889390390723E-17));
#41943=CARTESIAN_POINT('Ctrl Pts',(49.3520358333759,-44.9268254977065,-6.93889390390723E-17));
#41944=CARTESIAN_POINT('Ctrl Pts',(49.3968932976766,-45.0315629867066,-6.93889390390723E-17));
#41945=CARTESIAN_POINT('Ctrl Pts',(49.4367846336838,-45.1382131707156,-9.08116252949891E-17));
#41946=CARTESIAN_POINT('Ctrl Pts',(49.4716807095004,-45.2463465785723,-1.2490009027033E-16));
#41947=CARTESIAN_POINT('Ctrl Pts',(49.5070983411891,-45.3560961456251,-1.59498040586468E-16));
#41948=CARTESIAN_POINT('Ctrl Pts',(49.5373707252924,-45.4673743159336,1.38995551510238E-16));
#41949=CARTESIAN_POINT('Ctrl Pts',(49.5624277251463,-45.5797685483207,1.2490009027033E-16));
#41950=CARTESIAN_POINT('Ctrl Pts',(49.5887043183169,-45.6976333181011,1.10118564041589E-16));
#41951=CARTESIAN_POINT('Ctrl Pts',(49.6092463289301,-45.8167261990927,-1.8576267690903E-16));
#41952=CARTESIAN_POINT('Ctrl Pts',(49.6239191637252,-45.9366000763245,-2.22044604925031E-16));
#41953=CARTESIAN_POINT('Ctrl Pts',(49.6349237898216,-46.0265054842483,-2.49256050937032E-16));
#41954=CARTESIAN_POINT('Ctrl Pts',(49.6426259276078,-46.1168509125721,-3.71444925944582E-16));
#41955=CARTESIAN_POINT('Ctrl Pts',(49.6469460860109,-46.2074531754375,-3.88578058618805E-16));
#41956=CARTESIAN_POINT('Ctrl Pts',(49.6478995072093,-46.2274483029239,-3.92359191244283E-16));
#41957=CARTESIAN_POINT('Ctrl Pts',(49.6486881115146,-46.2474583007511,3.11387392686402E-18));
#41958=CARTESIAN_POINT('Ctrl Pts',(49.6493104445425,-46.2674574556759,0.));
#41959=CARTESIAN_POINT('Ctrl Pts',(49.6529983798999,-46.3859721210812,-1.84527660266109E-17));
#41960=CARTESIAN_POINT('Ctrl Pts',(49.6508611272068,-46.5042818926988,-4.93086514076101E-16));
#41961=CARTESIAN_POINT('Ctrl Pts',(49.6428326820612,-46.6219591778934,-5.27355936696949E-16));
#41962=CARTESIAN_POINT('Ctrl Pts',(49.6348301571772,-46.7392565357239,-5.61514718667094E-16));
#41963=CARTESIAN_POINT('Ctrl Pts',(49.6209747430515,-46.8559263686311,3.35081433764176E-17));
#41964=CARTESIAN_POINT('Ctrl Pts',(49.6011528370971,-46.9715627523068,1.11022302462516E-16));
#41965=CARTESIAN_POINT('Ctrl Pts',(49.5985997294166,-46.9864569880065,1.21006306794016E-16));
#41966=CARTESIAN_POINT('Ctrl Pts',(49.5959475676709,-47.0013340919922,-3.9670406639623E-16));
#41967=CARTESIAN_POINT('Ctrl Pts',(49.5931960463113,-47.0161932062988,-4.16333634234434E-16));
#41968=CARTESIAN_POINT('Ctrl Pts',(49.5723030878064,-47.1290220082781,-5.94426135246255E-16));
#41969=CARTESIAN_POINT('Ctrl Pts',(49.5456857086921,-47.2408138147752,-1.38518759257453E-16));
#41970=CARTESIAN_POINT('Ctrl Pts',(49.5136421664862,-47.35130678912,-8.32667268468867E-17));
#41971=CARTESIAN_POINT('Ctrl Pts',(49.4934325244267,-47.4209939493983,-4.84196493640788E-17));
#41972=CARTESIAN_POINT('Ctrl Pts',(49.4710634035422,-47.4901644562924,-3.44816612477604E-16));
#41973=CARTESIAN_POINT('Ctrl Pts',(49.4465992519874,-47.5587510924403,-3.88578058618805E-16));
#41974=CARTESIAN_POINT('Ctrl Pts',(49.4379571492393,-47.5829797175535,-4.04037042066843E-16));
#41975=CARTESIAN_POINT('Ctrl Pts',(49.4290535388707,-47.6071354647896,-6.52106218683356E-16));
#41976=CARTESIAN_POINT('Ctrl Pts',(49.4198910389393,-47.6312153075406,-6.66133814775094E-16));
#41977=CARTESIAN_POINT('Ctrl Pts',(49.4140168574915,-47.646653164743,-6.75127063925236E-16));
#41978=CARTESIAN_POINT('Ctrl Pts',(49.4080376321108,-47.6620561076285,5.84477223823245E-17));
#41979=CARTESIAN_POINT('Ctrl Pts',(49.4019578356655,-47.6774144897037,5.55111512312578E-17));
#41980=CARTESIAN_POINT('Ctrl Pts',(49.3590826893517,-47.7857228655749,3.48022477513383E-17));
#41981=CARTESIAN_POINT('Ctrl Pts',(49.311160597646,-47.8919462670934,-4.80329790939922E-16));
#41982=CARTESIAN_POINT('Ctrl Pts',(49.2585457221187,-47.99582861299,-4.44089209850063E-16));
#41983=CARTESIAN_POINT('Ctrl Pts',(49.2040866933149,-48.1033520388407,-4.06578395091634E-16));
#41984=CARTESIAN_POINT('Ctrl Pts',(49.1446000346224,-48.2083681046694,-4.35125637352618E-16));
#41985=CARTESIAN_POINT('Ctrl Pts',(49.0804225521245,-48.3105894369623,-6.10622663543836E-16));
#41986=CARTESIAN_POINT('Ctrl Pts',(49.0155495073654,-48.4139186547353,-7.88021744842209E-16));
#41987=CARTESIAN_POINT('Ctrl Pts',(48.9458830288196,-48.5143929921466,2.12533168780725E-16));
#41988=CARTESIAN_POINT('Ctrl Pts',(48.8717189601,-48.6117011858697,3.88578058618805E-16));
#41989=CARTESIAN_POINT('Ctrl Pts',(48.819020255279,-48.680845393654,5.13670139528005E-16));
#41990=CARTESIAN_POINT('Ctrl Pts',(48.7640495726607,-48.7483907131672,2.85916815352541E-16));
#41991=CARTESIAN_POINT('Ctrl Pts',(48.7068990197081,-48.8142178472156,3.33066907387547E-16));
#41992=CARTESIAN_POINT('Ctrl Pts',(48.6896326846016,-48.8341055525284,3.47311901483314E-16));
#41993=CARTESIAN_POINT('Ctrl Pts',(48.6721673038657,-48.8538363742111,-2.93254321078155E-16));
#41994=CARTESIAN_POINT('Ctrl Pts',(48.6545052298657,-48.8734068741477,-2.77555756156289E-16));
#41995=CARTESIAN_POINT('Ctrl Pts',(48.6371213308794,-48.8926691416486,-2.62104441274986E-16));
#41996=CARTESIAN_POINT('Ctrl Pts',(48.6195431892455,-48.9117798961928,2.3663751342404E-16));
#41997=CARTESIAN_POINT('Ctrl Pts',(48.6017947545563,-48.9307129811787,2.22044604925031E-16));
#41998=CARTESIAN_POINT('Ctrl Pts',(48.5161347739284,-49.0220904869426,1.51614266632079E-16));
#41999=CARTESIAN_POINT('Ctrl Pts',(48.4264328955782,-49.1094220783965,-1.89444256750939E-16));
#42000=CARTESIAN_POINT('Ctrl Pts',(48.3330184543456,-49.1923915218619,-3.33066907387547E-16));
#42001=CARTESIAN_POINT('Ctrl Pts',(48.2522204472863,-49.2641552191059,-4.57292067725676E-16));
#42002=CARTESIAN_POINT('Ctrl Pts',(48.1686439750736,-49.3326555431842,-7.0435694103298E-16));
#42003=CARTESIAN_POINT('Ctrl Pts',(48.0824754422125,-49.3976719692188,-6.66133814775094E-16));
#42004=CARTESIAN_POINT('Ctrl Pts',(48.0430744318381,-49.4274010685969,-6.48656091246299E-16));
#42005=CARTESIAN_POINT('Ctrl Pts',(48.0031311516611,-49.4564015054461,-5.92672758068129E-16));
#42006=CARTESIAN_POINT('Ctrl Pts',(47.9626619300835,-49.4846508230087,-6.66133814775094E-16));
#42007=CARTESIAN_POINT('Ctrl Pts',(47.944142628871,-49.4975781193735,-6.99750656995116E-16));
#42008=CARTESIAN_POINT('Ctrl Pts',(47.9255112318031,-49.5103494157158,-7.97651143721192E-16));
#42009=CARTESIAN_POINT('Ctrl Pts',(47.9067755363185,-49.522958267244,-7.7715611723761E-16));
#42010=CARTESIAN_POINT('Ctrl Pts',(47.8018201646528,-49.5935917112763,-6.62345160598864E-16));
#42011=CARTESIAN_POINT('Ctrl Pts',(47.6937577817196,-49.659022014658,-1.03399818926308E-15));
#42012=CARTESIAN_POINT('Ctrl Pts',(47.5828994522725,-49.7189169737277,-9.43689570931383E-16));
#42013=CARTESIAN_POINT('Ctrl Pts',(47.4730678387123,-49.7782572148403,-8.54217347064921E-16));
#42014=CARTESIAN_POINT('Ctrl Pts',(47.360491247089,-49.8321648668083,-3.07975410823444E-16));
#42015=CARTESIAN_POINT('Ctrl Pts',(47.2454367515685,-49.8802809428291,-5.55111512312578E-17));
#42016=CARTESIAN_POINT('Ctrl Pts',(47.1845210132458,-49.9057560560156,2.0809105445999E-17));
#42017=CARTESIAN_POINT('Ctrl Pts',(47.122910127501,-49.9296070150102,-3.22723620147229E-16));
#42018=CARTESIAN_POINT('Ctrl Pts',(47.0606641786102,-49.9518499819597,-2.77555756156289E-16));
#42019=CARTESIAN_POINT('Ctrl Pts',(42.6120197259946,-46.0027475428216,-2.01601780324957));
#42020=CARTESIAN_POINT('Ctrl Pts',(42.6094248952187,-46.3290880655303,-1.99688706151736));
#42021=CARTESIAN_POINT('Ctrl Pts',(42.6528675733331,-46.654752224773,-1.97775631978515));
#42022=CARTESIAN_POINT('Ctrl Pts',(42.7452064887581,-46.965905306516,-1.95862557805294));
#42023=CARTESIAN_POINT('Ctrl Pts',(43.0603316838194,-48.0277780297008,-1.8933380587845));
#42024=CARTESIAN_POINT('Ctrl Pts',(43.944928592468,-48.9206469884994,-1.82805053951607));
#42025=CARTESIAN_POINT('Ctrl Pts',(45.0038225147786,-49.245652733732,-1.76276302024764));
#42026=CARTESIAN_POINT('Ctrl Pts',(46.0627164370892,-49.5706584789645,-1.69747550097921));
#42027=CARTESIAN_POINT('Ctrl Pts',(47.2959073730619,-49.3278010106308,-1.63218798171078));
#42028=CARTESIAN_POINT('Ctrl Pts',(48.1524868580578,-48.6255464376747,-1.56690046244235));
#42029=CARTESIAN_POINT('Ctrl Pts',(49.0090663430538,-47.9232918647185,-1.50161294317392));
#42030=CARTESIAN_POINT('Ctrl Pts',(49.489034377073,-46.7616401871398,-1.43632542390549));
#42031=CARTESIAN_POINT('Ctrl Pts',(49.3779827843599,-45.6595897445677,-1.37103790463706));
#42032=CARTESIAN_POINT('Ctrl Pts',(49.2669311916469,-44.5575393019956,-1.30575038536862));
#42033=CARTESIAN_POINT('Ctrl Pts',(48.5648599722015,-43.51509009443,-1.24046286610019));
#42034=CARTESIAN_POINT('Ctrl Pts',(47.5853889385713,-42.9978284992196,-1.17517534683176));
#42035=CARTESIAN_POINT('Ctrl Pts',(46.605917904941,-42.4805669040093,-1.10988782756333));
#42036=CARTESIAN_POINT('Ctrl Pts',(45.3490470571259,-42.488492921154,-1.0446003082949));
#42037=CARTESIAN_POINT('Ctrl Pts',(44.3762941389621,-43.0182861025848,-0.979312789026468));
#42038=CARTESIAN_POINT('Ctrl Pts',(43.4035412207983,-43.5480792840155,-0.914025269758037));
#42039=CARTESIAN_POINT('Ctrl Pts',(42.7149062322859,-44.5997396297324,-0.848737750489605));
#42040=CARTESIAN_POINT('Ctrl Pts',(42.6179524951822,-45.7030076218998,-0.783450231221174));
#42041=CARTESIAN_POINT('Ctrl Pts',(42.6093232857121,-45.8012021927373,-0.777639421897305));
#42042=CARTESIAN_POINT('Ctrl Pts',(42.6053811385124,-45.8998055787131,-0.771828612573435));
#42043=CARTESIAN_POINT('Ctrl Pts',(42.6059703323355,-45.9984546826137,-0.766017803249566));
#42044=CARTESIAN_POINT('Ctrl Pts',(44.942095577027,-49.9456385074984,5.55111512312578E-16));
#42045=CARTESIAN_POINT('Ctrl Pts',(43.6472519732776,-49.5984650974504,-0.0652875192684306));
#42046=CARTESIAN_POINT('Ctrl Pts',(41.4469671882449,-47.5357720342741,-0.195862557805293));
#42047=CARTESIAN_POINT('Ctrl Pts',(42.2010820840665,-43.0499891012353,-0.391725115610587));
#42048=CARTESIAN_POINT('Ctrl Pts',(46.3558078226787,-41.2067330502749,-0.58758767341588));
#42049=CARTESIAN_POINT('Ctrl Pts',(50.1895243958238,-43.6427681215851,-0.783450231221173));
#42050=CARTESIAN_POINT('Ctrl Pts',(50.2815817385072,-48.1865095580738,-0.979312789026466));
#42051=CARTESIAN_POINT('Ctrl Pts',(46.547466535547,-50.7759010051096,-1.17517534683176));
#42052=CARTESIAN_POINT('Ctrl Pts',(42.3245747925301,-49.0985935082275,-1.37103790463705));
#42053=CARTESIAN_POINT('Ctrl Pts',(41.3853564274817,-44.6526231071457,-1.56690046244235));
#42054=CARTESIAN_POINT('Ctrl Pts',(44.5692320816632,-41.4105744865513,-1.76276302024764));
#42055=CARTESIAN_POINT('Ctrl Pts',(49.0314013549138,-42.268956305567,-1.95862557805293));
#42056=CARTESIAN_POINT('Ctrl Pts',(50.7851507003408,-46.4609045572623,-2.15448813585823));
#42057=CARTESIAN_POINT('Ctrl Pts',(48.263541336862,-50.2410414729541,-2.35035069366352));
#42058=CARTESIAN_POINT('Ctrl Pts',(43.7195496474102,-50.2319758772438,-2.54621325146881));
#42059=CARTESIAN_POINT('Ctrl Pts',(41.2130503891591,-46.4417996610074,-2.74207580927411));
#42060=CARTESIAN_POINT('Ctrl Pts',(42.9835080927057,-42.2568936678579,-2.9379383670794));
#42061=CARTESIAN_POINT('Ctrl Pts',(47.4490849663269,-41.4163089133544,-3.13380092488469));
#42062=CARTESIAN_POINT('Ctrl Pts',(50.6199603203723,-44.6710765381374,-3.32966348268999));
#42063=CARTESIAN_POINT('Ctrl Pts',(49.6630782896489,-49.1131861274939,-3.52552604049528));
#42064=CARTESIAN_POINT('Ctrl Pts',(45.433376454472,-50.7737834599584,-3.72138859830057));
#42065=CARTESIAN_POINT('Ctrl Pts',(41.7099309782434,-48.1691884401856,-3.91725115610587));
#42066=CARTESIAN_POINT('Ctrl Pts',(41.8194975483498,-43.6265068139424,-4.11311371391116));
#42067=CARTESIAN_POINT('Ctrl Pts',(45.6641826146291,-41.204450252827,-4.30897627171645));
#42068=CARTESIAN_POINT('Ctrl Pts',(49.8089076312337,-43.0670333548852,-4.50483882952175));
#42069=CARTESIAN_POINT('Ctrl Pts',(50.5505198521649,-47.5501095932216,-4.70070138732704));
#42070=CARTESIAN_POINT('Ctrl Pts',(47.2264172239299,-50.6482223997432,-4.89656394513234));
#42071=CARTESIAN_POINT('Ctrl Pts',(42.8065578694184,-49.5933268780552,-5.09242650293763));
#42072=CARTESIAN_POINT('Ctrl Pts',(41.2399165089103,-45.3279316921833,-5.28828906074292));
#42073=CARTESIAN_POINT('Ctrl Pts',(43.9262270571184,-41.6630037489246,-5.48415161854821));
#42074=CARTESIAN_POINT('Ctrl Pts',(48.4653741677054,-41.8730155103115,-5.68001417635351));
#42075=CARTESIAN_POINT('Ctrl Pts',(50.8018040255352,-45.7703295385275,-5.8758767341588));
#42076=CARTESIAN_POINT('Ctrl Pts',(48.8480063650781,-49.8728452943253,-6.0717392919641));
#42077=CARTESIAN_POINT('Ctrl Pts',(44.349624114825,-50.5151224407608,-6.26760184976939));
#42078=CARTESIAN_POINT('Ctrl Pts',(41.3257897924298,-47.1233108990577,-6.46346440757468));
#42079=CARTESIAN_POINT('Ctrl Pts',(42.4781820663993,-42.7278643121404,-6.65932696537998));
#42080=CARTESIAN_POINT('Ctrl Pts',(46.777185224748,-41.255945113868,-6.85518952318527));
#42081=CARTESIAN_POINT('Ctrl Pts',(50.3817996987672,-44.0226574502926,-7.05105208099057));
#42082=CARTESIAN_POINT('Ctrl Pts',(50.071451482069,-48.5560483299491,-7.24691463879586));
#42083=CARTESIAN_POINT('Ctrl Pts',(46.1234029447301,-50.8057104508671,-7.44277719660115));
#42084=CARTESIAN_POINT('Ctrl Pts',(42.0651286013526,-48.7616499517032,-7.63863975440644));
#42085=CARTESIAN_POINT('Ctrl Pts',(41.522449548134,-44.2501709386981,-7.83450231221174));
#42086=CARTESIAN_POINT('Ctrl Pts',(44.9804152684286,-41.3020771440901,-8.03036487001703));
#42087=CARTESIAN_POINT('Ctrl Pts',(49.3490847557137,-42.5514377898613,-8.22622742782233));
#42088=CARTESIAN_POINT('Ctrl Pts',(50.7259989091243,-46.8818733140433,-8.42208998562761));
#42089=CARTESIAN_POINT('Ctrl Pts',(47.8793446557761,-50.4245587866615,-8.61795254343292));
#42090=CARTESIAN_POINT('Ctrl Pts',(43.3557549422264,-50.0137233751776,-8.8138151012382));
#42091=CARTESIAN_POINT('Ctrl Pts',(41.1902146341594,-46.0175034104326,-9.0096776590435));
#42092=CARTESIAN_POINT('Ctrl Pts',(43.3312750455412,-42.0041758492615,-9.20554021684879));
#42093=CARTESIAN_POINT('Ctrl Pts',(46.3331931919405,-41.7135846407914,-9.33611525538566));
#42094=CARTESIAN_POINT('Ctrl Pts',(47.5707104172798,-42.2290460377978,-9.40140277465409));
#42095=CARTESIAN_POINT('Ctrl Pts',(45.0021125537771,-49.7217947561856,0.133800924884696));
#42096=CARTESIAN_POINT('Ctrl Pts',(43.780727947621,-49.3943171693393,0.0685134056162651));
#42097=CARTESIAN_POINT('Ctrl Pts',(41.7052696005152,-47.4486446979355,-0.0620616329205971));
#42098=CARTESIAN_POINT('Ctrl Pts',(42.4166020906803,-43.2173489606696,-0.257924190725891));
#42099=CARTESIAN_POINT('Ctrl Pts',(46.3356221524447,-41.4786644127225,-0.453786748531184));
#42100=CARTESIAN_POINT('Ctrl Pts',(49.9518445234292,-43.7764984735613,-0.649649306336477));
#42101=CARTESIAN_POINT('Ctrl Pts',(50.0386792739052,-48.0624646155809,-0.84551186414177));
#42102=CARTESIAN_POINT('Ctrl Pts',(46.5164076935365,-50.5049548464966,-1.04137442194706));
#42103=CARTESIAN_POINT('Ctrl Pts',(42.5330888174582,-48.9228042681952,-1.23723697975236));
#42104=CARTESIAN_POINT('Ctrl Pts',(41.6471541381135,-44.7290624204674,-1.43309953755765));
#42105=CARTESIAN_POINT('Ctrl Pts',(44.6504023301515,-41.6709415276141,-1.62896209536294));
#42106=CARTESIAN_POINT('Ctrl Pts',(48.8594240565046,-42.4806256755021,-1.82482465316824));
#42107=CARTESIAN_POINT('Ctrl Pts',(50.5136797885161,-46.434756544742,-2.02068721097353));
#42108=CARTESIAN_POINT('Ctrl Pts',(48.1351262316434,-50.0004389365142,-2.21654976877883));
#42109=CARTESIAN_POINT('Ctrl Pts',(43.8489240339983,-49.9918876496915,-2.41241232658412));
#42110=CARTESIAN_POINT('Ctrl Pts',(41.4846233566774,-46.4167355064324,-2.60827488438941));
#42111=CARTESIAN_POINT('Ctrl Pts',(43.1546395491354,-42.4692473747058,-2.8041374421947));
#42112=CARTESIAN_POINT('Ctrl Pts',(47.3668755560586,-41.6763506292247,-3.));
#42113=CARTESIAN_POINT('Ctrl Pts',(50.3578609802875,-44.7464689524058,-3.19586255780529));
#42114=CARTESIAN_POINT('Ctrl Pts',(49.4552647293978,-48.9365690197714,-3.39172511561059));
#42115=CARTESIAN_POINT('Ctrl Pts',(45.465522110941,-50.5029574338028,-3.58758767341588));
#42116=CARTESIAN_POINT('Ctrl Pts',(41.9533149429416,-48.0461261584199,-3.78345023122117));
#42117=CARTESIAN_POINT('Ctrl Pts',(42.0566655882934,-43.761159701548,-3.97931278902647));
#42118=CARTESIAN_POINT('Ctrl Pts',(45.6832341884503,-41.4765111228166,-4.17517534683176));
#42119=CARTESIAN_POINT('Ctrl Pts',(49.5928208886295,-43.2334262606392,-4.37103790463705));
#42120=CARTESIAN_POINT('Ctrl Pts',(50.2923600049827,-47.4621688592611,-4.56690046244235));
#42121=CARTESIAN_POINT('Ctrl Pts',(47.1568401880312,-50.3845196968936,-4.76276302024764));
#42122=CARTESIAN_POINT('Ctrl Pts',(42.9877280563859,-49.38947045113,-4.95862557805294));
#42123=CARTESIAN_POINT('Ctrl Pts',(41.5099653091698,-45.3660594352277,-5.15448813585822));
#42124=CARTESIAN_POINT('Ctrl Pts',(44.0438762320297,-41.9090499866692,-5.35035069366353));
#42125=CARTESIAN_POINT('Ctrl Pts',(48.3255086931973,-42.1071473721194,-5.54621325146881));
#42126=CARTESIAN_POINT('Ctrl Pts',(50.5293883381624,-45.7833591907788,-5.74207580927411));
#42127=CARTESIAN_POINT('Ctrl Pts',(48.6864334213556,-49.6531312436619,-5.93793836707939));
#42128=CARTESIAN_POINT('Ctrl Pts',(44.4432531506607,-50.258970757616,-6.1338009248847));
#42129=CARTESIAN_POINT('Ctrl Pts',(41.5909668341935,-47.0595832856289,-6.32966348268998));
#42130=CARTESIAN_POINT('Ctrl Pts',(42.6779816517388,-42.9134989377614,-6.52552604049528));
#42131=CARTESIAN_POINT('Ctrl Pts',(46.7330939944334,-41.5250845801742,-6.72138859830057));
#42132=CARTESIAN_POINT('Ctrl Pts',(50.1332116742411,-44.1348359413317,-6.91725115610587));
#42133=CARTESIAN_POINT('Ctrl Pts',(49.8404701158586,-48.4110387337518,-7.11311371391116));
#42134=CARTESIAN_POINT('Ctrl Pts',(46.1164020555156,-50.5330731443828,-7.30897627171646));
#42135=CARTESIAN_POINT('Ctrl Pts',(42.2883615136259,-48.6049761753734,-7.50483882952175));
#42136=CARTESIAN_POINT('Ctrl Pts',(41.7764696992283,-44.3494421467659,-7.70070138732704));
#42137=CARTESIAN_POINT('Ctrl Pts',(45.0382582945098,-41.5685994505422,-7.89656394513233));
#42138=CARTESIAN_POINT('Ctrl Pts',(49.1590846597194,-42.7470814354426,-8.09242650293763));
#42139=CARTESIAN_POINT('Ctrl Pts',(50.4578837935332,-46.8318429246848,-8.28828906074292));
#42140=CARTESIAN_POINT('Ctrl Pts',(47.7727257759778,-50.1735449558638,-8.48415161854821));
#42141=CARTESIAN_POINT('Ctrl Pts',(43.5057681104367,-49.7860170368184,-8.68001417635351));
#42142=CARTESIAN_POINT('Ctrl Pts',(41.4630831185005,-46.0165104078946,-8.8758767341588));
#42143=CARTESIAN_POINT('Ctrl Pts',(43.4826770059318,-42.2308667297838,-9.0717392919641));
#42144=CARTESIAN_POINT('Ctrl Pts',(46.3142904937196,-41.9567613261026,-9.20231433050096));
#42145=CARTESIAN_POINT('Ctrl Pts',(47.4816009584782,-42.4429795948945,-9.26760184976939));
#42146=CARTESIAN_POINT('Ctrl Pts',(45.0621295305272,-49.4979510048728,0.267601849769392));
#42147=CARTESIAN_POINT('Ctrl Pts',(43.9142039219644,-49.1901692412281,0.202314330500961));
#42148=CARTESIAN_POINT('Ctrl Pts',(41.9635720127856,-47.361517361597,0.0717392919640984));
#42149=CARTESIAN_POINT('Ctrl Pts',(42.6321220972942,-43.3847088201037,-0.124123265841195));
#42150=CARTESIAN_POINT('Ctrl Pts',(46.3154364822107,-41.7505957751702,-0.319985823646489));
#42151=CARTESIAN_POINT('Ctrl Pts',(49.7141646510345,-43.9102288255375,-0.515848381451781));
#42152=CARTESIAN_POINT('Ctrl Pts',(49.7957768093032,-47.938419673088,-0.711710939257075));
#42153=CARTESIAN_POINT('Ctrl Pts',(46.4853488515259,-50.2340086878835,-0.907573497062368));
#42154=CARTESIAN_POINT('Ctrl Pts',(42.7416028423862,-48.747015028163,-1.10343605486766));
#42155=CARTESIAN_POINT('Ctrl Pts',(41.9089518487454,-44.805501733789,-1.29929861267296));
#42156=CARTESIAN_POINT('Ctrl Pts',(44.7315725786397,-41.931308568677,-1.49516117047825));
#42157=CARTESIAN_POINT('Ctrl Pts',(48.6874467580956,-42.6922950454372,-1.69102372828354));
#42158=CARTESIAN_POINT('Ctrl Pts',(50.2422088766913,-46.4086085322216,-1.88688628608884));
#42159=CARTESIAN_POINT('Ctrl Pts',(48.0067111264249,-49.7598364000743,-2.08274884389413));
#42160=CARTESIAN_POINT('Ctrl Pts',(43.9782984205864,-49.7517994221391,-2.27861140169942));
#42161=CARTESIAN_POINT('Ctrl Pts',(41.7561963241958,-46.3916713518576,-2.47447395950472));
#42162=CARTESIAN_POINT('Ctrl Pts',(43.3257710055652,-42.6816010815537,-2.67033651731001));
#42163=CARTESIAN_POINT('Ctrl Pts',(47.2846661457903,-41.936392345095,-2.8661990751153));
#42164=CARTESIAN_POINT('Ctrl Pts',(50.0957616402027,-44.8218613666743,-3.0620616329206));
#42165=CARTESIAN_POINT('Ctrl Pts',(49.2474511691466,-48.7599519120487,-3.25792419072589));
#42166=CARTESIAN_POINT('Ctrl Pts',(45.4976677674101,-50.2321314076473,-3.45378674853118));
#42167=CARTESIAN_POINT('Ctrl Pts',(42.1966989076398,-47.9230638766541,-3.64964930633647));
#42168=CARTESIAN_POINT('Ctrl Pts',(42.2938336282371,-43.8958125891536,-3.84551186414177));
#42169=CARTESIAN_POINT('Ctrl Pts',(45.7022857622716,-41.7485719928062,-4.04137442194706));
#42170=CARTESIAN_POINT('Ctrl Pts',(49.3767341460252,-43.3998191663933,-4.23723697975236));
#42171=CARTESIAN_POINT('Ctrl Pts',(50.0342001578005,-47.3742281253005,-4.43309953755765));
#42172=CARTESIAN_POINT('Ctrl Pts',(47.0872631521327,-50.1208169940441,-4.62896209536294));
#42173=CARTESIAN_POINT('Ctrl Pts',(43.1688982433533,-49.1856140242049,-4.82482465316824));
#42174=CARTESIAN_POINT('Ctrl Pts',(41.7800141094294,-45.4041871782722,-5.02068721097353));
#42175=CARTESIAN_POINT('Ctrl Pts',(44.161525406941,-42.1550962244138,-5.21654976877882));
#42176=CARTESIAN_POINT('Ctrl Pts',(48.1856432186892,-42.3412792339273,-5.41241232658412));
#42177=CARTESIAN_POINT('Ctrl Pts',(50.2569726507896,-45.79638884303,-5.60827488438941));
#42178=CARTESIAN_POINT('Ctrl Pts',(48.524860477633,-49.4334171929985,-5.80413744219471));
#42179=CARTESIAN_POINT('Ctrl Pts',(44.5368821864965,-50.0028190744713,-6.));
#42180=CARTESIAN_POINT('Ctrl Pts',(41.8561438759571,-46.9958556722001,-6.19586255780529));
#42181=CARTESIAN_POINT('Ctrl Pts',(42.8777812370783,-43.0991335633823,-6.39172511561059));
#42182=CARTESIAN_POINT('Ctrl Pts',(46.6890027641187,-41.7942240464804,-6.58758767341588));
#42183=CARTESIAN_POINT('Ctrl Pts',(49.8846236497149,-44.2470144323708,-6.78345023122117));
#42184=CARTESIAN_POINT('Ctrl Pts',(49.6094887496482,-48.2660291375546,-6.97931278902647));
#42185=CARTESIAN_POINT('Ctrl Pts',(46.1094011663011,-50.2604358378984,-7.17517534683175));
#42186=CARTESIAN_POINT('Ctrl Pts',(42.5115944258992,-48.4483023990436,-7.37103790463706));
#42187=CARTESIAN_POINT('Ctrl Pts',(42.0304898503225,-44.4487133548336,-7.56690046244234));
#42188=CARTESIAN_POINT('Ctrl Pts',(45.096101320591,-41.8351217569944,-7.76276302024765));
#42189=CARTESIAN_POINT('Ctrl Pts',(48.9690845637251,-42.9427250810239,-7.95862557805293));
#42190=CARTESIAN_POINT('Ctrl Pts',(50.1897686779422,-46.7818125353263,-8.15448813585822));
#42191=CARTESIAN_POINT('Ctrl Pts',(47.6661068961795,-49.922531125066,-8.35035069366353));
#42192=CARTESIAN_POINT('Ctrl Pts',(43.655781278647,-49.5583106984592,-8.54621325146881));
#42193=CARTESIAN_POINT('Ctrl Pts',(41.7359516028417,-46.0155174053566,-8.74207580927411));
#42194=CARTESIAN_POINT('Ctrl Pts',(43.6340789663225,-42.4575576103061,-8.9379383670794));
#42195=CARTESIAN_POINT('Ctrl Pts',(46.2953877954988,-42.1999380114139,-9.06851340561627));
#42196=CARTESIAN_POINT('Ctrl Pts',(47.3924914996766,-42.6569131519913,-9.1338009248847));
#42197=CARTESIAN_POINT('Ctrl Pts',(45.1221465072772,-49.27410725356,0.401402774654088));
#42198=CARTESIAN_POINT('Ctrl Pts',(44.0476798963079,-48.9860213131169,0.336115255385657));
#42199=CARTESIAN_POINT('Ctrl Pts',(42.2218744250559,-47.2743900252584,0.205540216848794));
#42200=CARTESIAN_POINT('Ctrl Pts',(42.8476421039081,-43.5520686795379,0.00967765904350066));
#42201=CARTESIAN_POINT('Ctrl Pts',(46.2952508119767,-42.0225271376179,-0.186184898761793));
#42202=CARTESIAN_POINT('Ctrl Pts',(49.4764847786399,-44.0439591775136,-0.382047456567085));
#42203=CARTESIAN_POINT('Ctrl Pts',(49.5528743447013,-47.814374730595,-0.57791001437238));
#42204=CARTESIAN_POINT('Ctrl Pts',(46.4542900095154,-49.9630625292705,-0.773772572177672));
#42205=CARTESIAN_POINT('Ctrl Pts',(42.9501168673143,-48.5712257881308,-0.969635129982967));
#42206=CARTESIAN_POINT('Ctrl Pts',(42.1707495593773,-44.8819410471107,-1.16549768778826));
#42207=CARTESIAN_POINT('Ctrl Pts',(44.812742827128,-42.1916756097399,-1.36136024559355));
#42208=CARTESIAN_POINT('Ctrl Pts',(48.5154694596864,-42.9039644153723,-1.55722280339885));
#42209=CARTESIAN_POINT('Ctrl Pts',(49.9707379648667,-46.3824605197014,-1.75308536120414));
#42210=CARTESIAN_POINT('Ctrl Pts',(47.8782960212063,-49.5192338636343,-1.94894791900943));
#42211=CARTESIAN_POINT('Ctrl Pts',(44.1076728071747,-49.5117111945868,-2.14481047681473));
#42212=CARTESIAN_POINT('Ctrl Pts',(42.027769291714,-46.3666071972827,-2.34067303462002));
#42213=CARTESIAN_POINT('Ctrl Pts',(43.4969024619949,-42.8939547884017,-2.53653559242531));
#42214=CARTESIAN_POINT('Ctrl Pts',(47.2024567355219,-42.1964340609653,-2.73239815023061));
#42215=CARTESIAN_POINT('Ctrl Pts',(49.833662300118,-44.8972537809427,-2.9282607080359));
#42216=CARTESIAN_POINT('Ctrl Pts',(49.0396376088954,-48.5833348043262,-3.12412326584119));
#42217=CARTESIAN_POINT('Ctrl Pts',(45.5298134238792,-49.9613053814918,-3.31998582364649));
#42218=CARTESIAN_POINT('Ctrl Pts',(42.440082872338,-47.8000015948883,-3.51584838145178));
#42219=CARTESIAN_POINT('Ctrl Pts',(42.5310016681808,-44.0304654767592,-3.71171093925708));
#42220=CARTESIAN_POINT('Ctrl Pts',(45.7213373360928,-42.0206328627957,-3.90757349706236));
#42221=CARTESIAN_POINT('Ctrl Pts',(49.1606474034209,-43.5662120721474,-4.10343605486766));
#42222=CARTESIAN_POINT('Ctrl Pts',(49.7760403106183,-47.2862873913398,-4.29929861267295));
#42223=CARTESIAN_POINT('Ctrl Pts',(47.0176861162341,-49.8571142911945,-4.49516117047825));
#42224=CARTESIAN_POINT('Ctrl Pts',(43.3500684303209,-48.9817575972797,-4.69102372828354));
#42225=CARTESIAN_POINT('Ctrl Pts',(42.0500629096888,-45.4423149213166,-4.88688628608883));
#42226=CARTESIAN_POINT('Ctrl Pts',(44.2791745818524,-42.4011424621584,-5.08274884389413));
#42227=CARTESIAN_POINT('Ctrl Pts',(48.0457777441811,-42.5754110957352,-5.27861140169942));
#42228=CARTESIAN_POINT('Ctrl Pts',(49.9845569634168,-45.8094184952813,-5.47447395950472));
#42229=CARTESIAN_POINT('Ctrl Pts',(48.3632875339104,-49.2137031423351,-5.67033651731001));
#42230=CARTESIAN_POINT('Ctrl Pts',(44.6305112223323,-49.7466673913265,-5.86619907511531));
#42231=CARTESIAN_POINT('Ctrl Pts',(42.1213209177207,-46.9321280587713,-6.06206163292059));
#42232=CARTESIAN_POINT('Ctrl Pts',(43.0775808224178,-43.2847681890032,-6.25792419072589));
#42233=CARTESIAN_POINT('Ctrl Pts',(46.6449115338041,-42.0633635127868,-6.45378674853118));
#42234=CARTESIAN_POINT('Ctrl Pts',(49.6360356251888,-44.3591929234098,-6.64964930633648));
#42235=CARTESIAN_POINT('Ctrl Pts',(49.3785073834378,-48.1210195413575,-6.84551186414177));
#42236=CARTESIAN_POINT('Ctrl Pts',(46.1024002770866,-49.9877985314141,-7.04137442194706));
#42237=CARTESIAN_POINT('Ctrl Pts',(42.7348273381726,-48.2916286227139,-7.23723697975236));
#42238=CARTESIAN_POINT('Ctrl Pts',(42.2845100014167,-44.5479845629013,-7.43309953755765));
#42239=CARTESIAN_POINT('Ctrl Pts',(45.1539443466722,-42.1016440634466,-7.62896209536294));
#42240=CARTESIAN_POINT('Ctrl Pts',(48.7790844677308,-43.1383687266052,-7.82482465316824));
#42241=CARTESIAN_POINT('Ctrl Pts',(49.9216535623511,-46.7317821459677,-8.02068721097353));
#42242=CARTESIAN_POINT('Ctrl Pts',(47.5594880163812,-49.6715172942683,-8.21654976877883));
#42243=CARTESIAN_POINT('Ctrl Pts',(43.8057944468573,-49.3306043600999,-8.41241232658412));
#42244=CARTESIAN_POINT('Ctrl Pts',(42.0088200871828,-46.0145244028186,-8.60827488438941));
#42245=CARTESIAN_POINT('Ctrl Pts',(43.7854809267131,-42.6842484908284,-8.80413744219471));
#42246=CARTESIAN_POINT('Ctrl Pts',(46.2764850972779,-42.4431146967252,-8.93471248073157));
#42247=CARTESIAN_POINT('Ctrl Pts',(47.3033820408749,-42.8708467090881,-9.));
#42248=CARTESIAN_POINT('Ctrl Pts',(42.6118898788522,-45.9972329038001,-1.10898219675043));
#42249=CARTESIAN_POINT('Ctrl Pts',(42.6093014257603,-45.675906530902,-1.12782069376304));
#42250=CARTESIAN_POINT('Ctrl Pts',(42.6514005654697,-45.35524393637,-1.14665919077564));
#42251=CARTESIAN_POINT('Ctrl Pts',(42.7409763219919,-45.0484442643856,-1.16549768778825));
#42252=CARTESIAN_POINT('Ctrl Pts',(43.0514139819609,-43.9851859013204,-1.23078520705669));
#42253=CARTESIAN_POINT('Ctrl Pts',(43.9320784045444,-43.0884307555301,-1.29607272632512));
#42254=CARTESIAN_POINT('Ctrl Pts',(44.9895317212626,-42.7587679835737,-1.36136024559355));
#42255=CARTESIAN_POINT('Ctrl Pts',(46.0469850379808,-42.4291052116173,-1.42664776486198));
#42256=CARTESIAN_POINT('Ctrl Pts',(47.2812272488336,-42.6665348134948,-1.49193528413041));
#42257=CARTESIAN_POINT('Ctrl Pts',(48.1408931051234,-43.3649989651551,-1.55722280339884));
#42258=CARTESIAN_POINT('Ctrl Pts',(49.0005589614132,-44.0634631168153,-1.62251032266727));
#42259=CARTESIAN_POINT('Ctrl Pts',(49.4856484631399,-45.2229618182583,-1.68779784193571));
#42260=CARTESIAN_POINT('Ctrl Pts',(49.3794528900599,-46.325506726302,-1.75308536120414));
#42261=CARTESIAN_POINT('Ctrl Pts',(49.2732573169799,-47.4280516343457,-1.81837288047257));
#42262=CARTESIAN_POINT('Ctrl Pts',(48.5757766690931,-48.47364274899,-1.883660399741));
#42263=CARTESIAN_POINT('Ctrl Pts',(47.5985991428111,-48.9951845281376,-1.94894791900943));
#42264=CARTESIAN_POINT('Ctrl Pts',(46.6214216165291,-49.5167263072851,-2.01423543827786));
#42265=CARTESIAN_POINT('Ctrl Pts',(45.3645472118519,-49.514218750936,-2.0795229575463));
#42266=CARTESIAN_POINT('Ctrl Pts',(44.3894594236032,-48.9887809732107,-2.14481047681473));
#42267=CARTESIAN_POINT('Ctrl Pts',(43.4143716353545,-48.4633431954854,-2.21009799608316));
#42268=CARTESIAN_POINT('Ctrl Pts',(42.7210704635343,-47.4149751963841,-2.27538551535159));
#42269=CARTESIAN_POINT('Ctrl Pts',(42.6192754060043,-46.3120157953532,-2.34067303462002));
#42270=CARTESIAN_POINT('Ctrl Pts',(42.6097596402894,-46.2089115434583,-2.34677608866349));
#42271=CARTESIAN_POINT('Ctrl Pts',(42.6054127175106,-46.1053302476658,-2.35287914270696));
#42272=CARTESIAN_POINT('Ctrl Pts',(42.6060559323604,-46.0016943206056,-2.35898219675043));
#42273=CARTESIAN_POINT('Ctrl Pts',(44.942095577027,-49.9456385074984,5.55111512312578E-16));
#42274=CARTESIAN_POINT('Ctrl Pts',(44.82663061034,-49.9039985139974,5.42846940041275E-16));
#42275=CARTESIAN_POINT('Ctrl Pts',(44.7135212423861,-49.8568503832162,-2.95193080891787E-17));
#42276=CARTESIAN_POINT('Ctrl Pts',(44.6029921165273,-49.8045482654284,1.38777878078145E-16));
#42277=CARTESIAN_POINT('Ctrl Pts',(44.4901063321701,-49.7511309824801,3.10663430578551E-16));
#42278=CARTESIAN_POINT('Ctrl Pts',(44.3799113698433,-49.6923370368737,-1.16889976070159E-16));
#42279=CARTESIAN_POINT('Ctrl Pts',(44.2726738374971,-49.6284969638907,-6.93889390390723E-18));
#42280=CARTESIAN_POINT('Ctrl Pts',(44.160705472714,-49.5618405570977,1.07862730181961E-16));
#42281=CARTESIAN_POINT('Ctrl Pts',(44.0519603129653,-49.4896824522167,5.85955431398957E-16));
#42282=CARTESIAN_POINT('Ctrl Pts',(43.9467834035794,-49.412356585367,5.48172618408671E-16));
#42283=CARTESIAN_POINT('Ctrl Pts',(43.8547536078667,-49.3446964518735,5.15112657042171E-16));
#42284=CARTESIAN_POINT('Ctrl Pts',(43.7654561119054,-49.2730787482686,1.19154455589423E-15));
#42285=CARTESIAN_POINT('Ctrl Pts',(43.679154686656,-49.1977078017425,1.36002320516582E-15));
#42286=CARTESIAN_POINT('Ctrl Pts',(43.6621944745782,-49.1828956797654,1.39313312906316E-15));
#42287=CARTESIAN_POINT('Ctrl Pts',(43.6453500786238,-49.1679385594659,5.1622689728816E-16));
#42288=CARTESIAN_POINT('Ctrl Pts',(43.6286236576442,-49.152837933438,5.13478148889135E-16));
#42289=CARTESIAN_POINT('Ctrl Pts',(43.6160017913096,-49.1414429025748,5.11403925424206E-16));
#42290=CARTESIAN_POINT('Ctrl Pts',(43.6034471475502,-49.1299661133717,1.00052068254941E-15));
#42291=CARTESIAN_POINT('Ctrl Pts',(43.5909710847022,-49.1184180804733,9.99200722162641E-16));
#42292=CARTESIAN_POINT('Ctrl Pts',(43.5004959172789,-49.034672893981,9.89628500666128E-16));
#42293=CARTESIAN_POINT('Ctrl Pts',(43.4140089081737,-48.9470574449428,1.70135956276898E-16));
#42294=CARTESIAN_POINT('Ctrl Pts',(43.3317676836786,-48.8558861730966,3.19189119579733E-16));
#42295=CARTESIAN_POINT('Ctrl Pts',(43.249852288359,-48.7650761101272,4.67651753381386E-16));
#42296=CARTESIAN_POINT('Ctrl Pts',(43.1721486259969,-48.6707376107984,1.09689163767266E-15));
#42297=CARTESIAN_POINT('Ctrl Pts',(43.0989537517469,-48.5731525014645,1.346145417358E-15));
#42298=CARTESIAN_POINT('Ctrl Pts',(43.0268380871154,-48.4770062195034,1.59172411625057E-15));
#42299=CARTESIAN_POINT('Ctrl Pts',(42.9590988800379,-48.3777076637844,9.41922024275774E-16));
#42300=CARTESIAN_POINT('Ctrl Pts',(42.8960675550739,-48.2755089103244,9.71445146547012E-16));
#42301=CARTESIAN_POINT('Ctrl Pts',(42.8445085118557,-48.1919112713806,9.95594788617647E-16));
#42302=CARTESIAN_POINT('Ctrl Pts',(42.7961003109415,-48.1063726153879,5.70479466357528E-16));
#42303=CARTESIAN_POINT('Ctrl Pts',(42.7510509740316,-48.0190267661575,5.55111512312578E-16));
#42304=CARTESIAN_POINT('Ctrl Pts',(42.7404166838962,-47.9984080142168,5.51483772298812E-16));
#42305=CARTESIAN_POINT('Ctrl Pts',(42.7299696743251,-47.9776885519846,5.63921738060297E-16));
#42306=CARTESIAN_POINT('Ctrl Pts',(42.7197128936464,-47.9568701328682,5.55111512312578E-16));
#42307=CARTESIAN_POINT('Ctrl Pts',(42.7124710693496,-47.9421712387317,5.48891031551775E-16));
#42308=CARTESIAN_POINT('Ctrl Pts',(42.705324800963,-47.9274243606889,3.80345069376565E-16));
#42309=CARTESIAN_POINT('Ctrl Pts',(42.6982802017053,-47.9126412259157,3.88578058618805E-16));
#42310=CARTESIAN_POINT('Ctrl Pts',(42.6476410529925,-47.8063746615825,4.47759787959845E-16));
#42311=CARTESIAN_POINT('Ctrl Pts',(42.6021744956729,-47.6980810220835,2.79773749468683E-16));
#42312=CARTESIAN_POINT('Ctrl Pts',(42.5621516727626,-47.5880163403607,1.94289029309402E-16));
#42313=CARTESIAN_POINT('Ctrl Pts',(42.5229349918356,-47.4801685877389,1.10526147262437E-16));
#42314=CARTESIAN_POINT('Ctrl Pts',(42.4889447313643,-47.3706197849924,1.994436682046E-16));
#42315=CARTESIAN_POINT('Ctrl Pts',(42.4604848736845,-47.2596000187875,1.94289029309402E-16));
#42316=CARTESIAN_POINT('Ctrl Pts',(42.4550245237132,-47.2382996038655,1.93300052742487E-16));
#42317=CARTESIAN_POINT('Ctrl Pts',(42.4497679053429,-47.2169450250228,4.20536784643823E-16));
#42318=CARTESIAN_POINT('Ctrl Pts',(42.4447173875259,-47.1955378899826,4.16333634234434E-16));
#42319=CARTESIAN_POINT('Ctrl Pts',(42.4175094478094,-47.080214261639,3.67266964756074E-16));
#42320=CARTESIAN_POINT('Ctrl Pts',(42.3962787129898,-46.9633646502898,-2.91090424899702E-16));
#42321=CARTESIAN_POINT('Ctrl Pts',(42.380940596355,-46.845425615413,-2.4980018054066E-16));
#42322=CARTESIAN_POINT('Ctrl Pts',(42.3724302191523,-46.7799869636134,-2.26890226036143E-16));
#42323=CARTESIAN_POINT('Ctrl Pts',(42.3657348704511,-46.7142130564285,9.61593993794892E-16));
#42324=CARTESIAN_POINT('Ctrl Pts',(42.3608466945119,-46.6481804853459,1.0547118733939E-15));
#42325=CARTESIAN_POINT('Ctrl Pts',(42.3589204350846,-46.6221593551456,1.09140637777708E-15));
#42326=CARTESIAN_POINT('Ctrl Pts',(42.3572748561029,-46.5960980794369,9.6891319473525E-16));
#42327=CARTESIAN_POINT('Ctrl Pts',(42.3559096667242,-46.5700014398623,9.99200722162641E-16));
#42328=CARTESIAN_POINT('Ctrl Pts',(42.355035272559,-46.5532867263352,1.01859966979129E-15));
#42329=CARTESIAN_POINT('Ctrl Pts',(42.3542759514787,-46.5365570378457,1.12141472518015E-16));
#42330=CARTESIAN_POINT('Ctrl Pts',(42.3536320498877,-46.5198290668053,1.11022302462516E-16));
#42331=CARTESIAN_POINT('Ctrl Pts',(42.3490547833004,-46.4009158912789,1.03066521995632E-16));
#42332=CARTESIAN_POINT('Ctrl Pts',(42.350294234656,-46.2819004401008,3.95995902974907E-17));
#42333=CARTESIAN_POINT('Ctrl Pts',(42.3571972740339,-46.163217984259,5.55111512312578E-17));
#42334=CARTESIAN_POINT('Ctrl Pts',(42.3639584195197,-46.0469750792689,7.10956456095611E-17));
#42335=CARTESIAN_POINT('Ctrl Pts',(42.3761532498072,-45.9310507101419,5.29470641973068E-16));
#42336=CARTESIAN_POINT('Ctrl Pts',(42.3936902278642,-45.815863702484,4.9960036108132E-16));
#42337=CARTESIAN_POINT('Ctrl Pts',(42.4110239463115,-45.7020117518776,4.70076287022706E-16));
#42338=CARTESIAN_POINT('Ctrl Pts',(42.4335770963145,-45.5888793559188,1.28993477976455E-16));
#42339=CARTESIAN_POINT('Ctrl Pts',(42.4613061905346,-45.4768933497828,1.11022302462516E-16));
#42340=CARTESIAN_POINT('Ctrl Pts',(42.4793959127936,-45.4038366631192,9.92983863787067E-17));
#42341=CARTESIAN_POINT('Ctrl Pts',(42.4996893681797,-45.331268353669,-2.62013610217355E-17));
#42342=CARTESIAN_POINT('Ctrl Pts',(42.522183785235,-45.2593146281972,-5.55111512312578E-17));
#42343=CARTESIAN_POINT('Ctrl Pts',(42.5314102394662,-45.2298016271181,-6.75330425844794E-17));
#42344=CARTESIAN_POINT('Ctrl Pts',(42.5410070574239,-45.2003921034647,5.52363651431842E-16));
#42345=CARTESIAN_POINT('Ctrl Pts',(42.5509743800709,-45.1710951322748,5.55111512312578E-16));
#42346=CARTESIAN_POINT('Ctrl Pts',(42.5570610432268,-45.1532045912102,5.56789525975078E-16));
#42347=CARTESIAN_POINT('Ctrl Pts',(42.5632831769561,-45.1353640243178,1.12910067832828E-16));
#42348=CARTESIAN_POINT('Ctrl Pts',(42.5696389447263,-45.1175795122746,1.11022302462516E-16));
#42349=CARTESIAN_POINT('Ctrl Pts',(42.6078193744145,-45.0107442193322,9.96821000518763E-17));
#42350=CARTESIAN_POINT('Ctrl Pts',(42.6508354931777,-44.9058800578143,1.89284020183184E-16));
#42351=CARTESIAN_POINT('Ctrl Pts',(42.6986279931034,-44.8033979085955,2.22044604925031E-16));
#42352=CARTESIAN_POINT('Ctrl Pts',(42.7370196795508,-44.7210740597619,2.48361162945569E-16));
#42353=CARTESIAN_POINT('Ctrl Pts',(42.7784944303779,-44.6402876042849,-1.09142067611465E-17));
#42354=CARTESIAN_POINT('Ctrl Pts',(42.8230401863722,-44.5612683184574,2.77555756156289E-16));
#42355=CARTESIAN_POINT('Ctrl Pts',(42.8451166911604,-44.5221070200802,4.2051906153628E-16));
#42356=CARTESIAN_POINT('Ctrl Pts',(42.8679477140259,-44.4833800189724,1.95633996835777E-17));
#42357=CARTESIAN_POINT('Ctrl Pts',(42.8915331690334,-44.4451169825572,0.));
#42358=CARTESIAN_POINT('Ctrl Pts',(42.9049285238735,-44.4233854980522,-1.11110292574829E-17));
#42359=CARTESIAN_POINT('Ctrl Pts',(42.9185690339628,-44.4018011557844,2.38874525753449E-17));
#42360=CARTESIAN_POINT('Ctrl Pts',(42.9324410403483,-44.3803901775881,5.55111512312578E-17));
#42361=CARTESIAN_POINT('Ctrl Pts',(42.9909913459386,-44.2900197379023,1.88986956298474E-16));
#42362=CARTESIAN_POINT('Ctrl Pts',(43.0537086663914,-44.2026583110029,-7.69983934686249E-16));
#42363=CARTESIAN_POINT('Ctrl Pts',(43.120561083899,-44.1186870123308,-1.11022302462516E-16));
#42364=CARTESIAN_POINT('Ctrl Pts',(43.1787980554028,-44.0455373146802,4.63017219645686E-16));
#42365=CARTESIAN_POINT('Ctrl Pts',(43.2401736532957,-43.9749604886065,-2.51258776215073E-17));
#42366=CARTESIAN_POINT('Ctrl Pts',(43.304686291877,-43.9072342474385,-1.11022302462516E-16));
#42367=CARTESIAN_POINT('Ctrl Pts',(43.3427056719154,-43.8673209876779,-2.14685645937026E-16));
#42368=CARTESIAN_POINT('Ctrl Pts',(43.3818149876739,-43.8283983093625,3.12743896641743E-16));
#42369=CARTESIAN_POINT('Ctrl Pts',(43.4219651657257,-43.7904875258606,2.77555756156289E-16));
#42370=CARTESIAN_POINT('Origin',(46.,-46.,-5.));
#42371=CARTESIAN_POINT('Origin',(-46.,-46.,-9.));
#42372=CARTESIAN_POINT('Ctrl Pts',(-44.696617959125,-42.8708467090881,-9.));
#42373=CARTESIAN_POINT('Ctrl Pts',(-44.7904997272541,-42.8200479292046,
-9.));
#42374=CARTESIAN_POINT('Ctrl Pts',(-44.886738796863,-42.7741603751026,-9.));
#42375=CARTESIAN_POINT('Ctrl Pts',(-44.9849439731347,-42.733071165152,-9.));
#42376=CARTESIAN_POINT('Ctrl Pts',(-45.0854084189225,-42.6910366730583,
-9.));
#42377=CARTESIAN_POINT('Ctrl Pts',(-45.1879310497138,-42.6540235798679,
-9.));
#42378=CARTESIAN_POINT('Ctrl Pts',(-45.2921276331192,-42.6219533204472,
-9.));
#42379=CARTESIAN_POINT('Ctrl Pts',(-45.3228379835846,-42.6125011016303,
-9.));
#42380=CARTESIAN_POINT('Ctrl Pts',(-45.3536939396971,-42.6034785481757,
-9.));
#42381=CARTESIAN_POINT('Ctrl Pts',(-45.3846861010656,-42.5948843786566,
-9.));
#42382=CARTESIAN_POINT('Ctrl Pts',(-45.4054440163549,-42.5891281798314,
-9.));
#42383=CARTESIAN_POINT('Ctrl Pts',(-45.4262630376611,-42.5835641629292,
-9.));
#42384=CARTESIAN_POINT('Ctrl Pts',(-45.4471403803258,-42.5781920278371,
-9.));
#42385=CARTESIAN_POINT('Ctrl Pts',(-45.4677328861357,-42.5728931866545,
-9.));
#42386=CARTESIAN_POINT('Ctrl Pts',(-45.4883746116549,-42.567782998565,-9.));
#42387=CARTESIAN_POINT('Ctrl Pts',(-45.5090571442629,-42.5628620679155,
-9.));
#42388=CARTESIAN_POINT('Ctrl Pts',(-45.6183973166331,-42.5368471008109,
-9.));
#42389=CARTESIAN_POINT('Ctrl Pts',(-45.7289240905594,-42.5161052932284,
-9.));
#42390=CARTESIAN_POINT('Ctrl Pts',(-45.8402228698817,-42.5005440545346,
-9.));
#42391=CARTESIAN_POINT('Ctrl Pts',(-45.9357752888625,-42.4871843931926,
-9.));
#42392=CARTESIAN_POINT('Ctrl Pts',(-46.0318975830046,-42.4776438143453,
-9.));
#42393=CARTESIAN_POINT('Ctrl Pts',(-46.128341200326,-42.4718911713871,-9.));
#42394=CARTESIAN_POINT('Ctrl Pts',(-46.1610020619997,-42.4699430250905,
-9.));
#42395=CARTESIAN_POINT('Ctrl Pts',(-46.1936998545402,-42.4684295178701,
-9.));
#42396=CARTESIAN_POINT('Ctrl Pts',(-46.2264251288074,-42.4673501149057,
-9.));
#42397=CARTESIAN_POINT('Ctrl Pts',(-46.2453983262225,-42.4667243073,-9.));
#42398=CARTESIAN_POINT('Ctrl Pts',(-46.2643828408655,-42.4662443894445,
-9.));
#42399=CARTESIAN_POINT('Ctrl Pts',(-46.2833702123848,-42.4659104209501,
-9.));
#42400=CARTESIAN_POINT('Ctrl Pts',(-46.3983318693734,-42.4638883626863,
-9.));
#42401=CARTESIAN_POINT('Ctrl Pts',(-46.5131366913024,-42.4672161609136,
-9.));
#42402=CARTESIAN_POINT('Ctrl Pts',(-46.6273657132139,-42.4757916011297,
-9.));
#42403=CARTESIAN_POINT('Ctrl Pts',(-46.7431939697372,-42.4844870996338,
-9.));
#42404=CARTESIAN_POINT('Ctrl Pts',(-46.8584310337364,-42.4985780118847,
-9.));
#42405=CARTESIAN_POINT('Ctrl Pts',(-46.9726595897454,-42.5180074306283,
-9.));
#42406=CARTESIAN_POINT('Ctrl Pts',(-47.0865463926996,-42.5373787197462,
-9.));
#42407=CARTESIAN_POINT('Ctrl Pts',(-47.1994316277292,-42.5620565574636,
-9.));
#42408=CARTESIAN_POINT('Ctrl Pts',(-47.3109076528104,-42.5920352736768,
-9.));
#42409=CARTESIAN_POINT('Ctrl Pts',(-47.3774374342275,-42.6099268107619,
-9.));
#42410=CARTESIAN_POINT('Ctrl Pts',(-47.4434653340186,-42.6297073870142,
-9.));
#42411=CARTESIAN_POINT('Ctrl Pts',(-47.5089036506937,-42.6513845973822,
-9.));
#42412=CARTESIAN_POINT('Ctrl Pts',(-47.5540019340407,-42.6663239330042,
-9.));
#42413=CARTESIAN_POINT('Ctrl Pts',(-47.5988201695549,-42.682164228417,-9.));
#42414=CARTESIAN_POINT('Ctrl Pts',(-47.6433291058402,-42.698909822974,-9.));
#42415=CARTESIAN_POINT('Ctrl Pts',(-47.6570944305462,-42.7040887503021,
-9.));
#42416=CARTESIAN_POINT('Ctrl Pts',(-47.6708276202054,-42.7093533588747,
-9.));
#42417=CARTESIAN_POINT('Ctrl Pts',(-47.684519940033,-42.7147005149645,-9.));
#42418=CARTESIAN_POINT('Ctrl Pts',(-47.7954788044728,-42.7580324247633,
-9.));
#42419=CARTESIAN_POINT('Ctrl Pts',(-47.9039046508829,-42.8068376390484,
-9.));
#42420=CARTESIAN_POINT('Ctrl Pts',(-48.0093701191363,-42.861056455776,-9.));
#42421=CARTESIAN_POINT('Ctrl Pts',(-48.0319897960043,-42.872685021361,-9.));
#42422=CARTESIAN_POINT('Ctrl Pts',(-48.0544733077876,-42.8845627997616,
-9.));
#42423=CARTESIAN_POINT('Ctrl Pts',(-48.0768164393444,-42.8966895147212,
-9.));
#42424=CARTESIAN_POINT('Ctrl Pts',(-48.1769659944078,-42.9510455974617,
-9.));
#42425=CARTESIAN_POINT('Ctrl Pts',(-48.2742962894481,-43.0103990269558,
-9.));
#42426=CARTESIAN_POINT('Ctrl Pts',(-48.3686669704147,-43.0743603461825,
-9.));
#42427=CARTESIAN_POINT('Ctrl Pts',(-48.4650739604994,-43.1397018082269,
-9.));
#42428=CARTESIAN_POINT('Ctrl Pts',(-48.5583927895653,-43.2098525452832,
-9.));
#42429=CARTESIAN_POINT('Ctrl Pts',(-48.6484540229757,-43.2844481095684,
-9.));
#42430=CARTESIAN_POINT('Ctrl Pts',(-48.6989515653842,-43.3262740154365,
-9.));
#42431=CARTESIAN_POINT('Ctrl Pts',(-48.7484245615551,-43.3694981915471,
-9.));
#42432=CARTESIAN_POINT('Ctrl Pts',(-48.7968394888843,-43.4140624125384,
-9.));
#42433=CARTESIAN_POINT('Ctrl Pts',(-48.8170272914924,-43.4326445678031,
-9.));
#42434=CARTESIAN_POINT('Ctrl Pts',(-48.8370310947172,-43.4514597614807,
-9.00000000000001));
#42435=CARTESIAN_POINT('Ctrl Pts',(-48.8568483097048,-43.4705039675987,
-9.00000000000001));
#42436=CARTESIAN_POINT('Ctrl Pts',(-48.8675797536332,-43.4808168107629,
-9.00000000000001));
#42437=CARTESIAN_POINT('Ctrl Pts',(-48.8782549321768,-43.4911953739355,
-9.));
#42438=CARTESIAN_POINT('Ctrl Pts',(-48.888867064305,-43.5016325280181,-9.));
#42439=CARTESIAN_POINT('Ctrl Pts',(-48.9743463294842,-43.5857023690979,
-9.));
#42440=CARTESIAN_POINT('Ctrl Pts',(-49.0558569064676,-43.6736845088744,
-9.));
#42441=CARTESIAN_POINT('Ctrl Pts',(-49.1332523820262,-43.7651463951702,
-9.));
#42442=CARTESIAN_POINT('Ctrl Pts',(-49.2120673577358,-43.8582857717904,
-9.));
#42443=CARTESIAN_POINT('Ctrl Pts',(-49.286615490809,-43.9550342143835,-9.));
#42444=CARTESIAN_POINT('Ctrl Pts',(-49.3567182741951,-44.0549849707905,
-9.));
#42445=CARTESIAN_POINT('Ctrl Pts',(-49.4273892475969,-44.1557458379964,
-9.));
#42446=CARTESIAN_POINT('Ctrl Pts',(-49.4935431267415,-44.2597617819432,
-9.));
#42447=CARTESIAN_POINT('Ctrl Pts',(-49.5549639159556,-44.3666576234218,
-9.));
#42448=CARTESIAN_POINT('Ctrl Pts',(-49.5912272721098,-44.4297698370639,
-9.));
#42449=CARTESIAN_POINT('Ctrl Pts',(-49.6258400878192,-44.4938866701378,
-9.));
#42450=CARTESIAN_POINT('Ctrl Pts',(-49.6587512269125,-44.5589362078444,
-9.));
#42451=CARTESIAN_POINT('Ctrl Pts',(-49.6760912942311,-44.5932092045848,
-9.));
#42452=CARTESIAN_POINT('Ctrl Pts',(-49.6929588912015,-44.6277411762725,
-9.));
#42453=CARTESIAN_POINT('Ctrl Pts',(-49.7093459082312,-44.6625219515001,
-9.));
#42454=CARTESIAN_POINT('Ctrl Pts',(-49.7168943224581,-44.6785431528006,
-9.));
#42455=CARTESIAN_POINT('Ctrl Pts',(-49.7243415069159,-44.6946187938948,
-9.));
#42456=CARTESIAN_POINT('Ctrl Pts',(-49.7316842773234,-44.7107427074915,
-9.));
#42457=CARTESIAN_POINT('Ctrl Pts',(-49.7841002776772,-44.8258424605655,
-9.));
#42458=CARTESIAN_POINT('Ctrl Pts',(-49.8310341812553,-44.9430352874127,
-9.));
#42459=CARTESIAN_POINT('Ctrl Pts',(-49.8723050335951,-45.0618934597966,
-9.));
#42460=CARTESIAN_POINT('Ctrl Pts',(-49.9136557204705,-45.1809815520019,
-9.));
#42461=CARTESIAN_POINT('Ctrl Pts',(-49.9493220045472,-45.3017421809313,
-9.));
#42462=CARTESIAN_POINT('Ctrl Pts',(-49.9790839449739,-45.4237811307975,
-9.));
#42463=CARTESIAN_POINT('Ctrl Pts',(-50.0083331061446,-45.5437174273752,
-9.));
#42464=CARTESIAN_POINT('Ctrl Pts',(-50.0318800488967,-45.664889160174,-9.));
#42465=CARTESIAN_POINT('Ctrl Pts',(-50.0494721954982,-45.78694540661,-9.));
#42466=CARTESIAN_POINT('Ctrl Pts',(-50.0603641529683,-45.862515004525,-9.));
#42467=CARTESIAN_POINT('Ctrl Pts',(-50.0689725651408,-45.9384240776739,
-9.));
#42468=CARTESIAN_POINT('Ctrl Pts',(-50.0752277437256,-46.0145919640507,
-9.));
#42469=CARTESIAN_POINT('Ctrl Pts',(-50.0806292004451,-46.080364273521,-9.));
#42470=CARTESIAN_POINT('Ctrl Pts',(-50.0842757987835,-46.1463296239162,
-9.));
#42471=CARTESIAN_POINT('Ctrl Pts',(-50.0861960634202,-46.2124371387131,
-9.));
#42472=CARTESIAN_POINT('Ctrl Pts',(-49.4256147683784,-48.2253962475631,
-9.));
#42473=CARTESIAN_POINT('Ctrl Pts',(-49.3489157903097,-48.32416642034,-9.));
#42474=CARTESIAN_POINT('Ctrl Pts',(-49.2674580358364,-48.4189429185709,
-9.));
#42475=CARTESIAN_POINT('Ctrl Pts',(-49.181649358739,-48.509586461748,-9.));
#42476=CARTESIAN_POINT('Ctrl Pts',(-49.0946357246301,-48.6015028549048,
-9.));
#42477=CARTESIAN_POINT('Ctrl Pts',(-49.0031473218947,-48.6891698089487,
-9.));
#42478=CARTESIAN_POINT('Ctrl Pts',(-48.9075793351274,-48.7723981712024,
-9.));
#42479=CARTESIAN_POINT('Ctrl Pts',(-48.8671612794576,-48.8075974957113,
-9.));
#42480=CARTESIAN_POINT('Ctrl Pts',(-48.8260132332562,-48.8420023423363,
-9.));
#42481=CARTESIAN_POINT('Ctrl Pts',(-48.7841640395052,-48.8755958163019,
-9.));
#42482=CARTESIAN_POINT('Ctrl Pts',(-48.7601546692882,-48.8948687838556,
-9.));
#42483=CARTESIAN_POINT('Ctrl Pts',(-48.7359100930681,-48.9138778990817,
-9.));
#42484=CARTESIAN_POINT('Ctrl Pts',(-48.7114611111693,-48.9326007103251,
-9.));
#42485=CARTESIAN_POINT('Ctrl Pts',(-48.6120344070545,-49.0087407893434,
-9.));
#42486=CARTESIAN_POINT('Ctrl Pts',(-48.5091640540545,-49.0802045044556,
-9.));
#42487=CARTESIAN_POINT('Ctrl Pts',(-48.4032434739676,-49.146819885912,-9.));
#42488=CARTESIAN_POINT('Ctrl Pts',(-48.315219738108,-49.2021796161617,-9.));
#42489=CARTESIAN_POINT('Ctrl Pts',(-48.2250887079674,-49.2541902643244,
-9.00000000000001));
#42490=CARTESIAN_POINT('Ctrl Pts',(-48.1330675829928,-49.3027271284968,
-9.00000000000001));
#42491=CARTESIAN_POINT('Ctrl Pts',(-48.0928083408164,-49.3239620065723,
-9.00000000000001));
#42492=CARTESIAN_POINT('Ctrl Pts',(-48.0521872566217,-49.3445316646075,
-9.00000000000001));
#42493=CARTESIAN_POINT('Ctrl Pts',(-48.0112223219151,-49.3644241467311,
-9.00000000000001));
#42494=CARTESIAN_POINT('Ctrl Pts',(-47.9888528780583,-49.3752866994295,
-9.00000000000001));
#42495=CARTESIAN_POINT('Ctrl Pts',(-47.966380902054,-49.3859473119928,-9.));
#42496=CARTESIAN_POINT('Ctrl Pts',(-47.9438093210079,-49.3964039173489,
-9.));
#42497=CARTESIAN_POINT('Ctrl Pts',(-47.9276093772253,-49.403908771288,-9.));
#42498=CARTESIAN_POINT('Ctrl Pts',(-47.9113666692195,-49.4113045751474,
-9.));
#42499=CARTESIAN_POINT('Ctrl Pts',(-47.8950830669899,-49.4185906009187,
-9.));
#42500=CARTESIAN_POINT('Ctrl Pts',(-47.7833615965889,-49.4685798785413,
-9.));
#42501=CARTESIAN_POINT('Ctrl Pts',(-47.6697055328393,-49.5134106633889,
-9.));
#42502=CARTESIAN_POINT('Ctrl Pts',(-47.5544816880324,-49.5529248054346,
-9.));
#42503=CARTESIAN_POINT('Ctrl Pts',(-47.440121123448,-49.5921428995799,-9.));
#42504=CARTESIAN_POINT('Ctrl Pts',(-47.3242153616244,-49.6261239014414,
-9.00000000000001));
#42505=CARTESIAN_POINT('Ctrl Pts',(-47.207114055994,-49.6546628848245,-9.00000000000001));
#42506=CARTESIAN_POINT('Ctrl Pts',(-47.093156836174,-49.6824356170355,-9.00000000000001));
#42507=CARTESIAN_POINT('Ctrl Pts',(-46.9780667128225,-49.7050546341585,
-9.));
#42508=CARTESIAN_POINT('Ctrl Pts',(-46.8621684928363,-49.7222822072425,
-9.));
#42509=CARTESIAN_POINT('Ctrl Pts',(-46.7940349211499,-49.7324098527391,
-9.));
#42510=CARTESIAN_POINT('Ctrl Pts',(-46.725622175006,-49.7406733115846,-9.));
#42511=CARTESIAN_POINT('Ctrl Pts',(-46.6569980993869,-49.7470160499487,
-9.));
#42512=CARTESIAN_POINT('Ctrl Pts',(-46.6091444604989,-49.751439032823,-9.));
#42513=CARTESIAN_POINT('Ctrl Pts',(-46.5611880896396,-49.754927900429,-9.00000000000001));
#42514=CARTESIAN_POINT('Ctrl Pts',(-46.5131526151167,-49.7574616543188,
-9.00000000000001));
#42515=CARTESIAN_POINT('Ctrl Pts',(-46.4976743750253,-49.7582780936572,
-9.00000000000001));
#42516=CARTESIAN_POINT('Ctrl Pts',(-46.4821913582372,-49.7589951350126,
-9.));
#42517=CARTESIAN_POINT('Ctrl Pts',(-46.4667128228249,-49.7596119474122,
-9.));
#42518=CARTESIAN_POINT('Ctrl Pts',(-46.3509652583505,-49.7642244337419,
-9.));
#42519=CARTESIAN_POINT('Ctrl Pts',(-46.2353273954703,-49.7632440066829,
-9.00000000000001));
#42520=CARTESIAN_POINT('Ctrl Pts',(-46.1201129558431,-49.7564872215625,
-9.00000000000001));
#42521=CARTESIAN_POINT('Ctrl Pts',(-46.0928431815546,-49.754887977529,-9.00000000000001));
#42522=CARTESIAN_POINT('Ctrl Pts',(-46.0655971479505,-49.7529649092835,
-9.));
#42523=CARTESIAN_POINT('Ctrl Pts',(-46.0383790696643,-49.7507151556099,
-9.));
#42524=CARTESIAN_POINT('Ctrl Pts',(-45.9217046490404,-49.7410712452773,
-9.));
#42525=CARTESIAN_POINT('Ctrl Pts',(-45.8055425487772,-49.7254282959812,
-9.));
#42526=CARTESIAN_POINT('Ctrl Pts',(-45.6902555581451,-49.7040295749359,
-9.));
#42527=CARTESIAN_POINT('Ctrl Pts',(-45.574018295102,-49.6824544713332,-9.));
#42528=CARTESIAN_POINT('Ctrl Pts',(-45.4586698083806,-49.6550277949428,
-9.));
#42529=CARTESIAN_POINT('Ctrl Pts',(-45.3446065975032,-49.6219525163758,
-9.));
#42530=CARTESIAN_POINT('Ctrl Pts',(-45.2880020256639,-49.6055387054077,
-9.));
#42531=CARTESIAN_POINT('Ctrl Pts',(-45.2317144362182,-49.587733147565,-9.));
#42532=CARTESIAN_POINT('Ctrl Pts',(-45.1757954701078,-49.5685570750744,
-9.));
#42533=CARTESIAN_POINT('Ctrl Pts',(-45.1531748577313,-49.5607998768841,
-9.));
#42534=CARTESIAN_POINT('Ctrl Pts',(-45.130614594322,-49.5528183825136,-9.00000000000001));
#42535=CARTESIAN_POINT('Ctrl Pts',(-45.1081182151183,-49.5446139009718,
-9.00000000000001));
#42536=CARTESIAN_POINT('Ctrl Pts',(-45.0928980597617,-49.5390630751009,
-9.00000000000001));
#42537=CARTESIAN_POINT('Ctrl Pts',(-45.0777075162266,-49.5334102502331,
-9.));
#42538=CARTESIAN_POINT('Ctrl Pts',(-45.0625604546644,-49.5276608672583,
-9.));
#42539=CARTESIAN_POINT('Ctrl Pts',(-44.9540999893991,-49.4864924366765,
-9.));
#42540=CARTESIAN_POINT('Ctrl Pts',(-44.847696747572,-49.4403157932029,-9.));
#42541=CARTESIAN_POINT('Ctrl Pts',(-44.7436925895056,-49.3893796291663,
-9.));
#42542=CARTESIAN_POINT('Ctrl Pts',(-44.6397899691822,-49.338493193364,-9.));
#42543=CARTESIAN_POINT('Ctrl Pts',(-44.538281011366,-49.2828559183071,-9.));
#42544=CARTESIAN_POINT('Ctrl Pts',(-44.4395357151276,-49.2226729043818,
-9.));
#42545=CARTESIAN_POINT('Ctrl Pts',(-44.3421823782594,-49.1633382580584,
-9.));
#42546=CARTESIAN_POINT('Ctrl Pts',(-44.2475147356571,-49.0995845005203,
-9.));
#42547=CARTESIAN_POINT('Ctrl Pts',(-44.1559255117573,-49.0315757708794,
-9.));
#42548=CARTESIAN_POINT('Ctrl Pts',(-44.1056634674231,-48.9942541555324,
-9.));
#42549=CARTESIAN_POINT('Ctrl Pts',(-44.0563292320097,-48.9556506133514,
-9.));
#42550=CARTESIAN_POINT('Ctrl Pts',(-44.0079936818957,-48.9157890410837,
-9.));
#42551=CARTESIAN_POINT('Ctrl Pts',(-43.9809707187663,-48.8935036259983,
-9.));
#42552=CARTESIAN_POINT('Ctrl Pts',(-43.9542599849663,-48.8708249647296,
-9.));
#42553=CARTESIAN_POINT('Ctrl Pts',(-43.9278745179484,-48.8477569807897,
-9.));
#42554=CARTESIAN_POINT('Ctrl Pts',(-43.9114578068069,-48.833404366576,-9.));
#42555=CARTESIAN_POINT('Ctrl Pts',(-43.8951635188026,-48.8188977346138,
-9.));
#42556=CARTESIAN_POINT('Ctrl Pts',(-43.8790167509615,-48.8042581930767,
-9.));
#42557=CARTESIAN_POINT('Ctrl Pts',(-43.7964009707645,-48.7293542149109,
-9.));
#42558=CARTESIAN_POINT('Ctrl Pts',(-43.7175410737808,-48.6508864608485,
-9.));
#42559=CARTESIAN_POINT('Ctrl Pts',(-43.6427713171281,-48.5690422853087,
-9.));
#42560=CARTESIAN_POINT('Ctrl Pts',(-43.5691131678398,-48.488414893029,-9.));
#42561=CARTESIAN_POINT('Ctrl Pts',(-43.4994239498864,-48.4045101397136,
-9.));
#42562=CARTESIAN_POINT('Ctrl Pts',(-43.4340655377993,-48.3174806252745,
-9.));
#42563=CARTESIAN_POINT('Ctrl Pts',(-43.3705929531023,-48.232962228178,-9.));
#42564=CARTESIAN_POINT('Ctrl Pts',(-43.3112045665986,-48.1454962597952,
-9.));
#42565=CARTESIAN_POINT('Ctrl Pts',(-43.256277583738,-48.0552054878722,-9.));
#42566=CARTESIAN_POINT('Ctrl Pts',(-43.2286235921166,-48.0097469514626,
-9.));
#42567=CARTESIAN_POINT('Ctrl Pts',(-43.2021012370726,-47.9635721597901,
-9.));
#42568=CARTESIAN_POINT('Ctrl Pts',(-43.1767635963711,-47.9166956970799,
-9.));
#42569=CARTESIAN_POINT('Ctrl Pts',(-43.1505634206932,-47.8682234824552,
-9.));
#42570=CARTESIAN_POINT('Ctrl Pts',(-43.1256300485181,-47.8190009337087,
-9.));
#42571=CARTESIAN_POINT('Ctrl Pts',(-43.1019720879322,-47.7690801693092,
-9.));
#42572=CARTESIAN_POINT('Origin',(-46.,-46.,2.76038497140452));
#42573=CARTESIAN_POINT('Ctrl Pts',(-50.0901578141997,-45.9981376217778,
-0.364615028595479));
#42574=CARTESIAN_POINT('Ctrl Pts',(-50.0908678443317,-45.8792552045722,
-0.370425837919348));
#42575=CARTESIAN_POINT('Ctrl Pts',(-50.0327404569368,-44.4253400287511,
-0.441524166511649));
#42576=CARTESIAN_POINT('Ctrl Pts',(-48.2991257101273,-41.7778216414365,
-0.577910014372381));
#42577=CARTESIAN_POINT('Ctrl Pts',(-43.7551462487284,-41.7491661756407,
-0.773772572177673));
#42578=CARTESIAN_POINT('Ctrl Pts',(-41.2169403724754,-45.5179447459126,
-0.969635129982968));
#42579=CARTESIAN_POINT('Ctrl Pts',(-42.9521741545416,-49.7176769546074,
-1.16549768778826));
#42580=CARTESIAN_POINT('Ctrl Pts',(-47.4105432027648,-50.5956823608512,
-1.36136024559355));
#42581=CARTESIAN_POINT('Ctrl Pts',(-49.8549768496287,-48.1283902680758,
-1.51106602586263));
#42582=CARTESIAN_POINT('Ctrl Pts',(-50.0859947420446,-46.3965852541406,
-1.59548428686327));
#42583=CARTESIAN_POINT('Ctrl Pts',(-50.0828677018166,-46.0033110698502,
-1.61461502859548));
#42584=CARTESIAN_POINT('Ctrl Pts',(-50.0805802565567,-46.0038346370175,
-0.260384971404518));
#42585=CARTESIAN_POINT('Ctrl Pts',(-50.0745370386142,-45.103146971309,-0.304165019473208));
#42586=CARTESIAN_POINT('Ctrl Pts',(-49.3426919586741,-42.8475836408644,
-0.413232586810328));
#42587=CARTESIAN_POINT('Ctrl Pts',(-45.6441921539078,-41.2067322013831,
-0.58758767341588));
#42588=CARTESIAN_POINT('Ctrl Pts',(-41.8104753331013,-43.6427683056469,
-0.783450231221174));
#42589=CARTESIAN_POINT('Ctrl Pts',(-41.7184180535194,-48.1865095079258,
-0.979312789026466));
#42590=CARTESIAN_POINT('Ctrl Pts',(-45.4525334082598,-50.7759013692154,
-1.17517534683176));
#42591=CARTESIAN_POINT('Ctrl Pts',(-49.2692582722498,-49.2599208265826,
-1.35219940762444));
#42592=CARTESIAN_POINT('Ctrl Pts',(-50.0753327932863,-46.9514405162048,
-1.4639359491487));
#42593=CARTESIAN_POINT('Ctrl Pts',(-50.0830240067876,-45.9966653604899,
-1.51038497140452));
#42594=CARTESIAN_POINT('Ctrl Pts',(-43.4267655729853,-43.7934484719077,
0.));
#42595=CARTESIAN_POINT('Ctrl Pts',(-42.7026396483563,-44.6379090408209,
-0.0652875192684312));
#42596=CARTESIAN_POINT('Ctrl Pts',(-42.1622118099361,-47.0815123730999,
-0.195862557805293));
#42597=CARTESIAN_POINT('Ctrl Pts',(-44.7804699456593,-49.8003252158879,
-0.391725115610587));
#42598=CARTESIAN_POINT('Ctrl Pts',(-48.4895469401944,-49.1160278933692,
-0.58758767341588));
#42599=CARTESIAN_POINT('Ctrl Pts',(-49.9737289311609,-45.6513995309775,
-0.783450231221174));
#42600=CARTESIAN_POINT('Ctrl Pts',(-47.9078240822286,-42.4964188271871,
-0.979312789026467));
#42601=CARTESIAN_POINT('Ctrl Pts',(-44.1372110150862,-42.4726404024181,
-1.17517534683176));
#42602=CARTESIAN_POINT('Ctrl Pts',(-42.0309972160583,-45.5999885440531,
-1.37103790463705));
#42603=CARTESIAN_POINT('Ctrl Pts',(-43.4709014297081,-49.0849438082939,
-1.56690046244235));
#42604=CARTESIAN_POINT('Ctrl Pts',(-47.1704746197239,-49.813516348273,-1.76276302024764));
#42605=CARTESIAN_POINT('Ctrl Pts',(-49.824265602867,-47.1349091719286,-1.95862557805294));
#42606=CARTESIAN_POINT('Ctrl Pts',(-49.0612259744186,-43.4422793602443,
-2.15448813585823));
#42607=CARTESIAN_POINT('Ctrl Pts',(-45.5630964920078,-42.0348869356059,
-2.35035069366352));
#42608=CARTESIAN_POINT('Ctrl Pts',(-42.4553244696169,-44.1701649184598,
-2.54621325146881));
#42609=CARTESIAN_POINT('Ctrl Pts',(-42.5145835375169,-47.9403332310127,
-2.74207580927411));
#42610=CARTESIAN_POINT('Ctrl Pts',(-45.6879286795441,-49.9768868435812,
-2.9379383670794));
#42611=CARTESIAN_POINT('Ctrl Pts',(-49.1400974595928,-48.4602453793828,
-3.13380092488469));
#42612=CARTESIAN_POINT('Ctrl Pts',(-49.7867097218029,-44.7454687457041,
-3.32966348268999));
#42613=CARTESIAN_POINT('Ctrl Pts',(-47.050042144684,-42.1515678088258,-3.52552604049528));
#42614=CARTESIAN_POINT('Ctrl Pts',(-43.3752022219567,-42.996093261025,-3.72138859830058));
#42615=CARTESIAN_POINT('Ctrl Pts',(-42.0455183750331,-46.5244941426766,
-3.91725115610587));
#42616=CARTESIAN_POINT('Ctrl Pts',(-44.2490121010238,-49.5842796169672,
-4.11311371391116));
#42617=CARTESIAN_POINT('Ctrl Pts',(-48.0169463150116,-49.4416488178989,
-4.30897627171646));
#42618=CARTESIAN_POINT('Ctrl Pts',(-49.9828164023805,-46.2240368762855,
-4.50483882952175));
#42619=CARTESIAN_POINT('Ctrl Pts',(-48.3901928829157,-42.8062565861503,
-4.70070138732704));
#42620=CARTESIAN_POINT('Ctrl Pts',(-44.6620237528019,-42.2419634675882,
-4.89656394513234));
#42621=CARTESIAN_POINT('Ctrl Pts',(-42.1292850495319,-45.0353317691525,
-5.09242650293763));
#42622=CARTESIAN_POINT('Ctrl Pts',(-43.0548816114063,-48.6905941113693,
-5.28828906074292));
#42623=CARTESIAN_POINT('Ctrl Pts',(-46.6118284191898,-49.9419138769607,
-5.48415161854822));
#42624=CARTESIAN_POINT('Ctrl Pts',(-49.6221300325651,-47.6712848647882,
-5.68001417635351));
#42625=CARTESIAN_POINT('Ctrl Pts',(-49.3961974327852,-43.9074269825829,
-5.87587673415881));
#42626=CARTESIAN_POINT('Ctrl Pts',(-46.1358928380674,-42.0132027488516,
-6.0717392919641));
#42627=CARTESIAN_POINT('Ctrl Pts',(-42.7541730553862,-43.6810289290001,
-6.26760184976939));
#42628=CARTESIAN_POINT('Ctrl Pts',(-42.2724753932177,-47.4207666175459,
-6.46346440757469));
#42629=CARTESIAN_POINT('Ctrl Pts',(-45.121177278434,-49.8911041605667,-6.65932696537998));
#42630=CARTESIAN_POINT('Ctrl Pts',(-48.7550748399576,-48.8848888483899,
-6.85518952318527));
#42631=CARTESIAN_POINT('Ctrl Pts',(-49.9274161038516,-45.3011373268432,
-7.05105208099057));
#42632=CARTESIAN_POINT('Ctrl Pts',(-47.5907672407131,-42.3417902023858,
-7.24691463879586));
#42633=CARTESIAN_POINT('Ctrl Pts',(-43.8328177801406,-42.6509184160841,
-7.44277719660115));
#42634=CARTESIAN_POINT('Ctrl Pts',(-42.0111851884223,-45.9523117110681,
-7.63863975440645));
#42635=CARTESIAN_POINT('Ctrl Pts',(-43.753359094242,-49.2963347098191,-7.83450231221174));
#42636=CARTESIAN_POINT('Ctrl Pts',(-47.5029153976546,-49.6951640790793,
-8.03036487001703));
#42637=CARTESIAN_POINT('Ctrl Pts',(-49.9094803345903,-46.7925982881772,
-8.22622742782233));
#42638=CARTESIAN_POINT('Ctrl Pts',(-48.8234714875911,-43.1816880013063,
-8.42208998562762));
#42639=CARTESIAN_POINT('Ctrl Pts',(-45.2139879040286,-42.0892163329667,
-8.61795254343291));
#42640=CARTESIAN_POINT('Ctrl Pts',(-42.3084348061939,-44.4900926453702,
-8.81381510123821));
#42641=CARTESIAN_POINT('Ctrl Pts',(-42.6977478369022,-48.2416190468656,
-9.0096776590435));
#42642=CARTESIAN_POINT('Ctrl Pts',(-46.0445080898354,-49.9870172102589,
-9.2055402168488));
#42643=CARTESIAN_POINT('Ctrl Pts',(-48.2365749371353,-48.7794980878294,
-9.33611525538566));
#42644=CARTESIAN_POINT('Ctrl Pts',(-48.8425893907247,-47.8466430673628,
-9.40140277465409));
#42645=CARTESIAN_POINT('Ctrl Pts',(-43.2508390065835,-43.6425912356409,
0.133800924884696));
#42646=CARTESIAN_POINT('Ctrl Pts',(-42.4772061321698,-44.5447857781054,
0.0685134056162645));
#42647=CARTESIAN_POINT('Ctrl Pts',(-41.8998303915285,-47.155453074469,-0.0620616329205977));
#42648=CARTESIAN_POINT('Ctrl Pts',(-44.6970932688856,-50.0601453704073,
-0.257924190725891));
#42649=CARTESIAN_POINT('Ctrl Pts',(-48.659751971064,-49.329064094944,-0.453786748531184));
#42650=CARTESIAN_POINT('Ctrl Pts',(-50.2454043289916,-45.6275664581267,
-0.649649306336479));
#42651=CARTESIAN_POINT('Ctrl Pts',(-48.0382579581949,-42.2568864319368,
-0.845511864141771));
#42652=CARTESIAN_POINT('Ctrl Pts',(-44.0098560929669,-42.2314823268256,
-1.04137442194707));
#42653=CARTESIAN_POINT('Ctrl Pts',(-41.759644934864,-45.5726406113396,-1.23723697975236));
#42654=CARTESIAN_POINT('Ctrl Pts',(-43.2979923379859,-49.2958548570651,
-1.43309953755765));
#42655=CARTESIAN_POINT('Ctrl Pts',(-47.2504974807376,-50.0742383524657,
-1.62896209536295));
#42656=CARTESIAN_POINT('Ctrl Pts',(-50.0857225107405,-47.212500498898,-1.82482465316824));
#42657=CARTESIAN_POINT('Ctrl Pts',(-49.2705154853181,-43.267413438491,-2.02068721097353));
#42658=CARTESIAN_POINT('Ctrl Pts',(-45.5332263281381,-41.7638005862665,
-2.21654976877883));
#42659=CARTESIAN_POINT('Ctrl Pts',(-42.2129825405171,-44.0450629846456,
-2.41241232658412));
#42660=CARTESIAN_POINT('Ctrl Pts',(-42.2762930248891,-48.0729896883583,
-2.60827488438941));
#42661=CARTESIAN_POINT('Ctrl Pts',(-45.6665930269102,-50.2487781411695,
-2.80413744219471));
#42662=CARTESIAN_POINT('Ctrl Pts',(-49.3547792462321,-48.6284471248425,
-3.));
#42663=CARTESIAN_POINT('Ctrl Pts',(-50.0455990139418,-44.6596991113113,
-3.19586255780529));
#42664=CARTESIAN_POINT('Ctrl Pts',(-47.1218312934503,-41.8884586826942,
-3.39172511561059));
#42665=CARTESIAN_POINT('Ctrl Pts',(-43.1957503788823,-42.790722544377,-3.58758767341588));
#42666=CARTESIAN_POINT('Ctrl Pts',(-41.775158874602,-46.5603526919989,-3.78345023122118));
#42667=CARTESIAN_POINT('Ctrl Pts',(-44.1293007814315,-49.8293291932581,
-3.97931278902646));
#42668=CARTESIAN_POINT('Ctrl Pts',(-48.1548406460106,-49.6769470297281,
-4.17517534683177));
#42669=CARTESIAN_POINT('Ctrl Pts',(-50.2551130912961,-46.2393538011558,
-4.37103790463705));
#42670=CARTESIAN_POINT('Ctrl Pts',(-48.5536052881419,-42.5879071396839,
-4.56690046244235));
#42671=CARTESIAN_POINT('Ctrl Pts',(-44.5705491616704,-41.9850345004413,
-4.76276302024764));
#42672=CARTESIAN_POINT('Ctrl Pts',(-41.8646524985264,-44.9693794533479,
-4.95862557805293));
#42673=CARTESIAN_POINT('Ctrl Pts',(-42.8535301292744,-48.8745443098529,
-5.15448813585823));
#42674=CARTESIAN_POINT('Ctrl Pts',(-46.6536578273016,-50.2114141471829,
-5.35035069366352));
#42675=CARTESIAN_POINT('Ctrl Pts',(-49.8697673612905,-47.7855470574026,
-5.54621325146882));
#42676=CARTESIAN_POINT('Ctrl Pts',(-49.6283882300557,-43.7643622147427,
-5.74207580927411));
#42677=CARTESIAN_POINT('Ctrl Pts',(-46.1451835424621,-41.7406338977701,
-5.9379383670794));
#42678=CARTESIAN_POINT('Ctrl Pts',(-42.5322627686646,-43.5224858076182,
-6.1338009248847));
#42679=CARTESIAN_POINT('Ctrl Pts',(-42.0176324615496,-47.5179014102639,
-6.32966348268999));
#42680=CARTESIAN_POINT('Ctrl Pts',(-45.0610940375688,-50.1571306785139,
-6.52552604049528));
#42681=CARTESIAN_POINT('Ctrl Pts',(-48.9434334487518,-49.0821225649218,
-6.72138859830058));
#42682=CARTESIAN_POINT('Ctrl Pts',(-50.1959251921524,-45.2533575718454,
-6.91725115610588));
#42683=CARTESIAN_POINT('Ctrl Pts',(-47.6995246145712,-42.0916861768389,
-7.11311371391116));
#42684=CARTESIAN_POINT('Ctrl Pts',(-43.6846521397682,-42.4219488292201,
-7.30897627171646));
#42685=CARTESIAN_POINT('Ctrl Pts',(-41.7384784010241,-45.9490513641516,
-7.50483882952175));
#42686=CARTESIAN_POINT('Ctrl Pts',(-43.5997610324648,-49.521698105055,-7.70070138732705));
#42687=CARTESIAN_POINT('Ctrl Pts',(-47.6056665277988,-49.9477945902752,
-7.89656394513234));
#42688=CARTESIAN_POINT('Ctrl Pts',(-50.1767631924828,-46.8467865478674,
-8.09242650293763));
#42689=CARTESIAN_POINT('Ctrl Pts',(-49.0165062297547,-42.9890060024281,
-8.28828906074293));
#42690=CARTESIAN_POINT('Ctrl Pts',(-45.1602499282955,-41.8218443690062,
-8.48415161854821));
#42691=CARTESIAN_POINT('Ctrl Pts',(-42.0560503431317,-44.3868634899944,
-8.68001417635352));
#42692=CARTESIAN_POINT('Ctrl Pts',(-42.4719798779679,-48.3948737748281,
-8.8758767341588));
#42693=CARTESIAN_POINT('Ctrl Pts',(-46.0475510133015,-50.2596010994772,
-9.0717392919641));
#42694=CARTESIAN_POINT('Ctrl Pts',(-48.3894848100407,-48.9695264621503,
-9.20231433050096));
#42695=CARTESIAN_POINT('Ctrl Pts',(-49.036931183276,-47.9728941274296,-9.2676018497694));
#42696=CARTESIAN_POINT('Ctrl Pts',(-43.0749124401816,-43.4917339993741,
0.267601849769391));
#42697=CARTESIAN_POINT('Ctrl Pts',(-42.2517726159832,-44.45166251539,0.20231433050096));
#42698=CARTESIAN_POINT('Ctrl Pts',(-41.6374489731208,-47.2293937758381,
0.0717392919640981));
#42699=CARTESIAN_POINT('Ctrl Pts',(-44.613716592112,-50.3199655249267,-0.124123265841196));
#42700=CARTESIAN_POINT('Ctrl Pts',(-48.8299570019335,-49.5421002965189,
-0.319985823646488));
#42701=CARTESIAN_POINT('Ctrl Pts',(-50.5170797268223,-45.603733385276,-0.515848381451784));
#42702=CARTESIAN_POINT('Ctrl Pts',(-48.1686918341611,-42.0173540366867,
-0.711710939257075));
#42703=CARTESIAN_POINT('Ctrl Pts',(-43.8825011708477,-41.9903242512331,
-0.907573497062371));
#42704=CARTESIAN_POINT('Ctrl Pts',(-41.4882926536697,-45.545292678626,-1.10343605486766));
#42705=CARTESIAN_POINT('Ctrl Pts',(-43.1250832462638,-49.5067659058363,
-1.29929861267296));
#42706=CARTESIAN_POINT('Ctrl Pts',(-47.3305203417512,-50.3349603566584,
-1.49516117047825));
#42707=CARTESIAN_POINT('Ctrl Pts',(-50.3471794186141,-47.2900918258674,
-1.69102372828354));
#42708=CARTESIAN_POINT('Ctrl Pts',(-49.4798049962175,-43.0925475167376,
-1.88688628608884));
#42709=CARTESIAN_POINT('Ctrl Pts',(-45.5033561642685,-41.4927142369271,
-2.08274884389413));
#42710=CARTESIAN_POINT('Ctrl Pts',(-41.9706406114172,-43.9199610508312,
-2.27861140169943));
#42711=CARTESIAN_POINT('Ctrl Pts',(-42.0380025122611,-48.2056461457039,
-2.47447395950472));
#42712=CARTESIAN_POINT('Ctrl Pts',(-45.6452573742764,-50.5206694387578,
-2.67033651731001));
#42713=CARTESIAN_POINT('Ctrl Pts',(-49.5694610328715,-48.7966488703022,
-2.8661990751153));
#42714=CARTESIAN_POINT('Ctrl Pts',(-50.3044883060807,-44.5739294769185,
-3.0620616329206));
#42715=CARTESIAN_POINT('Ctrl Pts',(-47.1936204422165,-41.6253495565626,
-3.25792419072589));
#42716=CARTESIAN_POINT('Ctrl Pts',(-43.0162985358079,-42.585351827729,-3.45378674853118));
#42717=CARTESIAN_POINT('Ctrl Pts',(-41.5047993741709,-46.5962112413212,
-3.64964930633648));
#42718=CARTESIAN_POINT('Ctrl Pts',(-44.0095894618394,-50.074378769549,-3.84551186414177));
#42719=CARTESIAN_POINT('Ctrl Pts',(-48.2927349770096,-49.9122452415573,
-4.04137442194707));
#42720=CARTESIAN_POINT('Ctrl Pts',(-50.5274097802118,-46.2546707260261,
-4.23723697975236));
#42721=CARTESIAN_POINT('Ctrl Pts',(-48.7170176933682,-42.3695576932174,
-4.43309953755765));
#42722=CARTESIAN_POINT('Ctrl Pts',(-44.4790745705388,-41.7281055332943,
-4.62896209536295));
#42723=CARTESIAN_POINT('Ctrl Pts',(-41.6000199475209,-44.9034271375432,
-4.82482465316824));
#42724=CARTESIAN_POINT('Ctrl Pts',(-42.6521786471426,-49.0584945083365,
-5.02068721097354));
#42725=CARTESIAN_POINT('Ctrl Pts',(-46.6954872354135,-50.480914417405,-5.21654976877883));
#42726=CARTESIAN_POINT('Ctrl Pts',(-50.1174046900159,-47.8998092500169,
-5.41241232658412));
#42727=CARTESIAN_POINT('Ctrl Pts',(-49.8605790273263,-43.6212974469025,
-5.60827488438941));
#42728=CARTESIAN_POINT('Ctrl Pts',(-46.1544742468569,-41.4680650466885,
-5.80413744219471));
#42729=CARTESIAN_POINT('Ctrl Pts',(-42.3103524819431,-43.3639426862363,
-6.));
#42730=CARTESIAN_POINT('Ctrl Pts',(-41.7627895298816,-47.6150362029821,
-6.1958625578053));
#42731=CARTESIAN_POINT('Ctrl Pts',(-45.0010107967036,-50.423157196461,-6.39172511561059));
#42732=CARTESIAN_POINT('Ctrl Pts',(-49.131792057546,-49.2793562814538,-6.58758767341588));
#42733=CARTESIAN_POINT('Ctrl Pts',(-50.4644342804531,-45.2055778168475,
-6.78345023122118));
#42734=CARTESIAN_POINT('Ctrl Pts',(-47.8082819884292,-41.8415821512922,
-6.97931278902647));
#42735=CARTESIAN_POINT('Ctrl Pts',(-43.5364864993957,-42.1929792423559,
-7.17517534683176));
#42736=CARTESIAN_POINT('Ctrl Pts',(-41.4657716136258,-45.9457910172352,
-7.37103790463706));
#42737=CARTESIAN_POINT('Ctrl Pts',(-43.4461629706875,-49.7470615002908,
-7.56690046244235));
#42738=CARTESIAN_POINT('Ctrl Pts',(-47.7084176579431,-50.2004251014713,
-7.76276302024765));
#42739=CARTESIAN_POINT('Ctrl Pts',(-50.4440460503753,-46.9009748075577,
-7.95862557805293));
#42740=CARTESIAN_POINT('Ctrl Pts',(-49.2095409719184,-42.79632400355,-8.15448813585823));
#42741=CARTESIAN_POINT('Ctrl Pts',(-45.1065119525624,-41.5544724050458,
-8.35035069366352));
#42742=CARTESIAN_POINT('Ctrl Pts',(-41.8036658800697,-44.2836343346184,
-8.54621325146882));
#42743=CARTESIAN_POINT('Ctrl Pts',(-42.2462119190335,-48.5481285027907,
-8.74207580927411));
#42744=CARTESIAN_POINT('Ctrl Pts',(-46.0505939367677,-50.5321849886954,
-8.93793836707941));
#42745=CARTESIAN_POINT('Ctrl Pts',(-48.5423946829461,-49.1595548364713,
-9.06851340561627));
#42746=CARTESIAN_POINT('Ctrl Pts',(-49.2312729758272,-48.0991451874963,
-9.1338009248847));
#42747=CARTESIAN_POINT('Ctrl Pts',(-42.8989858737798,-43.3408767631073,
0.401402774654087));
#42748=CARTESIAN_POINT('Ctrl Pts',(-42.0263390997967,-44.3585392526745,
0.336115255385656));
#42749=CARTESIAN_POINT('Ctrl Pts',(-41.3750675547132,-47.3033344772072,
0.205540216848794));
#42750=CARTESIAN_POINT('Ctrl Pts',(-44.5303399153384,-50.5797856794461,
0.00967765904350008));
#42751=CARTESIAN_POINT('Ctrl Pts',(-49.0001620328031,-49.7551364980937,
-0.186184898761793));
#42752=CARTESIAN_POINT('Ctrl Pts',(-50.7887551246529,-45.5799003124252,
-0.382047456567087));
#42753=CARTESIAN_POINT('Ctrl Pts',(-48.2991257101273,-41.7778216414365,
-0.577910014372381));
#42754=CARTESIAN_POINT('Ctrl Pts',(-43.7551462487284,-41.7491661756407,
-0.773772572177673));
#42755=CARTESIAN_POINT('Ctrl Pts',(-41.2169403724754,-45.5179447459126,
-0.969635129982968));
#42756=CARTESIAN_POINT('Ctrl Pts',(-42.9521741545416,-49.7176769546074,
-1.16549768778826));
#42757=CARTESIAN_POINT('Ctrl Pts',(-47.4105432027648,-50.5956823608512,
-1.36136024559355));
#42758=CARTESIAN_POINT('Ctrl Pts',(-50.6086363264877,-47.3676831528367,
-1.55722280339885));
#42759=CARTESIAN_POINT('Ctrl Pts',(-49.6890945071171,-42.9176815949843,
-1.75308536120414));
#42760=CARTESIAN_POINT('Ctrl Pts',(-45.4734860003987,-41.2216278875877,
-1.94894791900943));
#42761=CARTESIAN_POINT('Ctrl Pts',(-41.7282986823175,-43.794859117017,-2.14481047681473));
#42762=CARTESIAN_POINT('Ctrl Pts',(-41.7997119996332,-48.3383026030494,
-2.34067303462002));
#42763=CARTESIAN_POINT('Ctrl Pts',(-45.6239217216425,-50.7925607363461,
-2.53653559242531));
#42764=CARTESIAN_POINT('Ctrl Pts',(-49.7841428195107,-48.9648506157619,
-2.73239815023061));
#42765=CARTESIAN_POINT('Ctrl Pts',(-50.5633775982196,-44.4881598425256,
-2.9282607080359));
#42766=CARTESIAN_POINT('Ctrl Pts',(-47.2654095909828,-41.362240430431,-3.1241232658412));
#42767=CARTESIAN_POINT('Ctrl Pts',(-42.8368466927335,-42.379981111081,-3.31998582364649));
#42768=CARTESIAN_POINT('Ctrl Pts',(-41.2344398737399,-46.6320697906436,
-3.51584838145178));
#42769=CARTESIAN_POINT('Ctrl Pts',(-43.8898781422471,-50.3194283458399,
-3.71171093925708));
#42770=CARTESIAN_POINT('Ctrl Pts',(-48.4306293080085,-50.1475434533866,
-3.90757349706237));
#42771=CARTESIAN_POINT('Ctrl Pts',(-50.7997064691274,-46.2699876508964,
-4.10343605486766));
#42772=CARTESIAN_POINT('Ctrl Pts',(-48.8804300985944,-42.151208246751,-4.29929861267296));
#42773=CARTESIAN_POINT('Ctrl Pts',(-44.3875999794073,-41.4711765661473,
-4.49516117047825));
#42774=CARTESIAN_POINT('Ctrl Pts',(-41.3353873965154,-44.8374748217385,
-4.69102372828354));
#42775=CARTESIAN_POINT('Ctrl Pts',(-42.4508271650107,-49.2424447068201,
-4.88688628608884));
#42776=CARTESIAN_POINT('Ctrl Pts',(-46.7373166435254,-50.7504146876272,
-5.08274884389413));
#42777=CARTESIAN_POINT('Ctrl Pts',(-50.3650420187413,-48.0140714426314,
-5.27861140169942));
#42778=CARTESIAN_POINT('Ctrl Pts',(-50.0927698245969,-43.4782326790622,
-5.47447395950472));
#42779=CARTESIAN_POINT('Ctrl Pts',(-46.1637649512516,-41.195496195607,-5.67033651731001));
#42780=CARTESIAN_POINT('Ctrl Pts',(-42.0884421952216,-43.2053995648544,
-5.86619907511531));
#42781=CARTESIAN_POINT('Ctrl Pts',(-41.5079465982135,-47.7121709957002,
-6.0620616329206));
#42782=CARTESIAN_POINT('Ctrl Pts',(-44.9409275558383,-50.6891837144081,
-6.25792419072589));
#42783=CARTESIAN_POINT('Ctrl Pts',(-49.3201506663402,-49.4765899979858,
-6.45378674853118));
#42784=CARTESIAN_POINT('Ctrl Pts',(-50.7329433687539,-45.1577980618496,
-6.64964930633648));
#42785=CARTESIAN_POINT('Ctrl Pts',(-47.9170393622873,-41.5914781257455,
-6.84551186414177));
#42786=CARTESIAN_POINT('Ctrl Pts',(-43.3883208590233,-41.9640096554919,
-7.04137442194707));
#42787=CARTESIAN_POINT('Ctrl Pts',(-41.1930648262276,-45.9425306703187,
-7.23723697975236));
#42788=CARTESIAN_POINT('Ctrl Pts',(-43.2925649089103,-49.9724248955266,
-7.43309953755766));
#42789=CARTESIAN_POINT('Ctrl Pts',(-47.8111687880873,-50.4530556126673,
-7.62896209536294));
#42790=CARTESIAN_POINT('Ctrl Pts',(-50.7113289082679,-46.9551630672479,
-7.82482465316824));
#42791=CARTESIAN_POINT('Ctrl Pts',(-49.4025757140821,-42.6036420046718,
-8.02068721097354));
#42792=CARTESIAN_POINT('Ctrl Pts',(-45.0527739768292,-41.2871004410853,
-8.21654976877883));
#42793=CARTESIAN_POINT('Ctrl Pts',(-41.5512814170077,-44.1804051792425,
-8.41241232658412));
#42794=CARTESIAN_POINT('Ctrl Pts',(-42.020443960099,-48.7013832307533,-8.60827488438941));
#42795=CARTESIAN_POINT('Ctrl Pts',(-46.0536368602338,-50.8047688779136,
-8.80413744219471));
#42796=CARTESIAN_POINT('Ctrl Pts',(-48.6953045558515,-49.3495832107922,
-8.93471248073157));
#42797=CARTESIAN_POINT('Ctrl Pts',(-49.4256147683784,-48.2253962475631,
-9.));
#42798=CARTESIAN_POINT('Ctrl Pts',(-43.4267655729853,-43.7934484719077,
0.));
#42799=CARTESIAN_POINT('Ctrl Pts',(-43.3501276807105,-43.8663850881657,
-7.04753096378064E-18));
#42800=CARTESIAN_POINT('Ctrl Pts',(-43.2774225625484,-43.9429578412532,
2.53724992624095E-17));
#42801=CARTESIAN_POINT('Ctrl Pts',(-43.2086477236659,-44.0227511556538,
-4.5102810375397E-17));
#42802=CARTESIAN_POINT('Ctrl Pts',(-43.1381557104546,-44.104536754345,-1.17337751798334E-16));
#42803=CARTESIAN_POINT('Ctrl Pts',(-43.0717922910936,-44.1897061536963,
3.43486518888929E-16));
#42804=CARTESIAN_POINT('Ctrl Pts',(-43.0095809299478,-44.2778601735959,
2.84494650060196E-16));
#42805=CARTESIAN_POINT('Ctrl Pts',(-42.946054054693,-44.3678782880081,2.24255346127592E-16));
#42806=CARTESIAN_POINT('Ctrl Pts',(-42.8868562438295,-44.461009120855,7.85372393156655E-16));
#42807=CARTESIAN_POINT('Ctrl Pts',(-42.8320459022356,-44.5568700617774,
9.78384040450919E-16));
#42808=CARTESIAN_POINT('Ctrl Pts',(-42.7793850615827,-44.648971617578,1.16382633668118E-15));
#42809=CARTESIAN_POINT('Ctrl Pts',(-42.7307742307634,-44.7435941668825,
3.30656683784562E-17));
#42810=CARTESIAN_POINT('Ctrl Pts',(-42.6862990500763,-44.8404265045392,
1.11022302462516E-16));
#42811=CARTESIAN_POINT('Ctrl Pts',(-42.679886056326,-44.8543890150141,1.22263075393663E-16));
#42812=CARTESIAN_POINT('Ctrl Pts',(-42.6735591098059,-44.8683975079843,
-7.82688482717754E-16));
#42813=CARTESIAN_POINT('Ctrl Pts',(-42.6673185299068,-44.8824510861312,
-7.91033905045424E-16));
#42814=CARTESIAN_POINT('Ctrl Pts',(-42.6607681147427,-44.8972024029786,
-7.99793664851382E-16));
#42815=CARTESIAN_POINT('Ctrl Pts',(-42.6543164169337,-44.9119954067526,
-1.21324678104633E-16));
#42816=CARTESIAN_POINT('Ctrl Pts',(-42.6479647673033,-44.9268258764304,
-1.2490009027033E-16));
#42817=CARTESIAN_POINT('Ctrl Pts',(-42.6031073987511,-45.0315633671385,
-1.50150787424036E-16));
#42818=CARTESIAN_POINT('Ctrl Pts',(-42.5632161545331,-45.1382135540035,
-3.07907070874353E-16));
#42819=CARTESIAN_POINT('Ctrl Pts',(-42.528320163891,-45.2463469640437,-2.08166817117217E-16));
#42820=CARTESIAN_POINT('Ctrl Pts',(-42.4929026061891,-45.3560965719249,
-1.06935812418896E-16));
#42821=CARTESIAN_POINT('Ctrl Pts',(-42.4626302928821,-45.4673747834446,
-2.85605705579807E-16));
#42822=CARTESIAN_POINT('Ctrl Pts',(-42.4375733579101,-45.5797690551028,
-4.9960036108132E-16));
#42823=CARTESIAN_POINT('Ctrl Pts',(-42.4112968134939,-45.6976339525716,
-7.24010891595492E-16));
#42824=CARTESIAN_POINT('Ctrl Pts',(-42.3907548535477,-45.8167269609219,
-4.47609461766868E-17));
#42825=CARTESIAN_POINT('Ctrl Pts',(-42.376082068452,-45.9366009615454,-5.55111512312578E-17));
#42826=CARTESIAN_POINT('Ctrl Pts',(-42.3650774796302,-46.0265064620131,
-6.35738050221861E-17));
#42827=CARTESIAN_POINT('Ctrl Pts',(-42.357375378577,-46.1168519806525,6.6117506257439E-16));
#42828=CARTESIAN_POINT('Ctrl Pts',(-42.3530552551646,-46.2074543300699,
7.21644966006352E-16));
#42829=CARTESIAN_POINT('Ctrl Pts',(-42.3521018391375,-46.2274495301548,
7.3499018084909E-16));
#42830=CARTESIAN_POINT('Ctrl Pts',(-42.3513132407974,-46.2474596005774,
-3.23104951562236E-16));
#42831=CARTESIAN_POINT('Ctrl Pts',(-42.3506909145217,-46.2674588278385,
-3.05311331771918E-16));
#42832=CARTESIAN_POINT('Ctrl Pts',(-42.3470030310376,-46.3859735407681,
-1.99866970652492E-16));
#42833=CARTESIAN_POINT('Ctrl Pts',(-42.3491403257791,-46.5042833521836,
-9.63231096175936E-16));
#42834=CARTESIAN_POINT('Ctrl Pts',(-42.3571688004525,-46.621960666869,-8.60422844084496E-16));
#42835=CARTESIAN_POINT('Ctrl Pts',(-42.3651713582012,-46.7392581044026,
-7.57946469943304E-16));
#42836=CARTESIAN_POINT('Ctrl Pts',(-42.3790267977734,-46.8559280062375,
-2.07758591149402E-16));
#42837=CARTESIAN_POINT('Ctrl Pts',(-42.3988487192012,-46.9715644449789,
-2.4980018054066E-16));
#42838=CARTESIAN_POINT('Ctrl Pts',(-42.4014018331404,-46.9864587126565,
-2.55215244276644E-16));
#42839=CARTESIAN_POINT('Ctrl Pts',(-42.4040540013104,-47.0013358483328,
-4.57968684642233E-16));
#42840=CARTESIAN_POINT('Ctrl Pts',(-42.406805529256,-47.0161949940318,-4.71844785465692E-16));
#42841=CARTESIAN_POINT('Ctrl Pts',(-42.4276985069981,-47.1290238682075,
-5.79779039420077E-16));
#42842=CARTESIAN_POINT('Ctrl Pts',(-42.4543158977961,-47.2408157327732,
-3.25103491011084E-16));
#42843=CARTESIAN_POINT('Ctrl Pts',(-42.486359445728,-47.3513087526731,-4.16333634234434E-16));
#42844=CARTESIAN_POINT('Ctrl Pts',(-42.5065690808814,-47.4209959054168,
-4.73871829238813E-16));
#42845=CARTESIAN_POINT('Ctrl Pts',(-42.5289381902425,-47.4901664003336,
-2.57699975902937E-16));
#42846=CARTESIAN_POINT('Ctrl Pts',(-42.5534023261536,-47.5587530205468,
-3.33066907387547E-16));
#42847=CARTESIAN_POINT('Ctrl Pts',(-42.5620444221668,-47.5829816366427,
-3.59690707242276E-16));
#42848=CARTESIAN_POINT('Ctrl Pts',(-42.5709480252132,-47.607137374388,-1.17515466282303E-15));
#42849=CARTESIAN_POINT('Ctrl Pts',(-42.5801105172574,-47.631217207197,-1.22124532708767E-15));
#42850=CARTESIAN_POINT('Ctrl Pts',(-42.5859847085885,-47.6466550972885,
-1.25079464392915E-15));
#42851=CARTESIAN_POINT('Ctrl Pts',(-42.5919639441197,-47.6620580726081,
-1.28683390958385E-16));
#42852=CARTESIAN_POINT('Ctrl Pts',(-42.598043751014,-47.6774164867468,-1.38777878078145E-16));
#42853=CARTESIAN_POINT('Ctrl Pts',(-42.6409188983819,-47.7857249052508,
-2.09964780949104E-16));
#42854=CARTESIAN_POINT('Ctrl Pts',(-42.6888409885308,-47.8919483371788,
-6.43124410407582E-16));
#42855=CARTESIAN_POINT('Ctrl Pts',(-42.741455861339,-47.9958307028328,-5.55111512312578E-16));
#42856=CARTESIAN_POINT('Ctrl Pts',(-42.7959148678593,-48.1033541106933,
-4.64013791546623E-16));
#42857=CARTESIAN_POINT('Ctrl Pts',(-42.8554014994299,-48.2083701489123,
3.64463956063111E-16));
#42858=CARTESIAN_POINT('Ctrl Pts',(-42.9195789519365,-48.3105914458752,
3.88578058618805E-16));
#42859=CARTESIAN_POINT('Ctrl Pts',(-42.98445195249,-48.4139206058127,4.12953507118863E-16));
#42860=CARTESIAN_POINT('Ctrl Pts',(-43.054118381845,-48.5143948787197,-3.61504930637615E-16));
#42861=CARTESIAN_POINT('Ctrl Pts',(-43.1282823985727,-48.61170300331,-3.33066907387547E-16));
#42862=CARTESIAN_POINT('Ctrl Pts',(-43.1809810456532,-48.6808471346839,
-3.1285973122524E-16));
#42863=CARTESIAN_POINT('Ctrl Pts',(-43.2359516673225,-48.7483923767087,
-1.30566376976968E-16));
#42864=CARTESIAN_POINT('Ctrl Pts',(-43.2931021569972,-48.8142194330436,
-5.55111512312578E-17));
#42865=CARTESIAN_POINT('Ctrl Pts',(-43.3103693212538,-48.8341080919287,
-3.28343392102748E-17));
#42866=CARTESIAN_POINT('Ctrl Pts',(-43.3278355504843,-48.8538398517485,
-4.86517584915369E-16));
#42867=CARTESIAN_POINT('Ctrl Pts',(-43.345498492003,-48.873411273902,-4.9960036108132E-16));
#42868=CARTESIAN_POINT('Ctrl Pts',(-43.3628813133451,-48.8926723088969,
-5.124756548431E-16));
#42869=CARTESIAN_POINT('Ctrl Pts',(-43.3804583525997,-48.9117818491587,
-2.10886016998155E-16));
#42870=CARTESIAN_POINT('Ctrl Pts',(-43.3982056633207,-48.9307137415863,
-2.22044604925031E-16));
#42871=CARTESIAN_POINT('Ctrl Pts',(-43.4838655638276,-49.0220911929223,
-2.75903104764051E-16));
#42872=CARTESIAN_POINT('Ctrl Pts',(-43.5735673629197,-49.1094227285799,
1.55779886598745E-16));
#42873=CARTESIAN_POINT('Ctrl Pts',(-43.6669817278709,-49.1923921170496,
-5.55111512312578E-17));
#42874=CARTESIAN_POINT('Ctrl Pts',(-43.7477796843816,-49.2641557804304,
-2.38265528404594E-16));
#42875=CARTESIAN_POINT('Ctrl Pts',(-43.8313561093309,-49.3326560699961,
-5.06042579863952E-16));
#42876=CARTESIAN_POINT('Ctrl Pts',(-43.9175245994745,-49.3976724621237,
-7.21644966006352E-16));
#42877=CARTESIAN_POINT('Ctrl Pts',(-43.9569256379766,-49.4274015819587,
-8.20230399073553E-16));
#42878=CARTESIAN_POINT('Ctrl Pts',(-43.9968689485439,-49.4564020376285,
-5.36268313194471E-16));
#42879=CARTESIAN_POINT('Ctrl Pts',(-44.0373382028386,-49.4846513724122,
-5.55111512312578E-16));
#42880=CARTESIAN_POINT('Ctrl Pts',(-44.0558574998406,-49.4975786632676,
-5.63734423878843E-16));
#42881=CARTESIAN_POINT('Ctrl Pts',(-44.0744888929508,-49.5103499540868,
3.11047644558593E-16));
#42882=CARTESIAN_POINT('Ctrl Pts',(-44.093224584765,-49.5229588001047,2.77555756156289E-16));
#42883=CARTESIAN_POINT('Ctrl Pts',(-44.1981798849433,-49.5935921789969,
8.99378536162834E-17));
#42884=CARTESIAN_POINT('Ctrl Pts',(-44.3062422017772,-49.6590224223094,
-6.83717929618714E-16));
#42885=CARTESIAN_POINT('Ctrl Pts',(-44.4171004727898,-49.7189173286392,
-4.9960036108132E-16));
#42886=CARTESIAN_POINT('Ctrl Pts',(-44.5269320414255,-49.7782575245074,
-3.17187978305053E-16));
#42887=CARTESIAN_POINT('Ctrl Pts',(-44.6395085962919,-49.8321651371395,
-3.46914076603539E-16));
#42888=CARTESIAN_POINT('Ctrl Pts',(-44.7545630653622,-49.880281181818,-2.77555756156289E-16));
#42889=CARTESIAN_POINT('Ctrl Pts',(-44.8154787832058,-49.9057562757025,
-2.40833915513258E-16));
#42890=CARTESIAN_POINT('Ctrl Pts',(-44.8770896512138,-49.9296072179812,
-2.58827617428343E-16));
#42891=CARTESIAN_POINT('Ctrl Pts',(-44.9393355849193,-49.9518501705994,
-2.77555756156289E-16));
#42892=CARTESIAN_POINT('Ctrl Pts',(-49.3879806100937,-46.0027475395409,
-2.01601780324957));
#42893=CARTESIAN_POINT('Ctrl Pts',(-49.3905754410883,-46.3290880943019,
-1.99688706151736));
#42894=CARTESIAN_POINT('Ctrl Pts',(-49.3471327586953,-46.6547522859376,
-1.97775631978515));
#42895=CARTESIAN_POINT('Ctrl Pts',(-49.2547938342684,-46.965905399372,-1.95862557805294));
#42896=CARTESIAN_POINT('Ctrl Pts',(-48.9396686084859,-48.0277782307101,
-1.8933380587845));
#42897=CARTESIAN_POINT('Ctrl Pts',(-48.0550716141049,-48.9206472894915,
-1.82805053951607));
#42898=CARTESIAN_POINT('Ctrl Pts',(-46.9961775852451,-49.2456530622191,
-1.76276302024764));
#42899=CARTESIAN_POINT('Ctrl Pts',(-45.9372835563853,-49.5706588349466,
-1.69747550097921));
#42900=CARTESIAN_POINT('Ctrl Pts',(-44.7040924930467,-49.3278013216202,
-1.63218798171078));
#42901=CARTESIAN_POINT('Ctrl Pts',(-43.8475129257691,-48.6255466875836,
-1.56690046244235));
#42902=CARTESIAN_POINT('Ctrl Pts',(-42.9909333584915,-47.923292053547,-1.50161294317392));
#42903=CARTESIAN_POINT('Ctrl Pts',(-42.5109652872749,-46.7616402988001,
-1.43632542390549));
#42904=CARTESIAN_POINT('Ctrl Pts',(-42.6220168848379,-45.6595897311541,
-1.37103790463705));
#42905=CARTESIAN_POINT('Ctrl Pts',(-42.733068482401,-44.5575391635081,-1.30575038536862));
#42906=CARTESIAN_POINT('Ctrl Pts',(-43.4351397487436,-43.5150897829631,
-1.24046286610019));
#42907=CARTESIAN_POINT('Ctrl Pts',(-44.4146108931053,-42.9978281634854,
-1.17517534683176));
#42908=CARTESIAN_POINT('Ctrl Pts',(-45.394082037467,-42.4805665440078,-1.10988782756333));
#42909=CARTESIAN_POINT('Ctrl Pts',(-46.6509530598478,-42.4884926855974,
-1.0446003082949));
#42910=CARTESIAN_POINT('Ctrl Pts',(-47.6237060458603,-43.0182858736907,
-0.979312789026467));
#42911=CARTESIAN_POINT('Ctrl Pts',(-48.5964590318727,-43.5480790617839,
-0.914025269758036));
#42912=CARTESIAN_POINT('Ctrl Pts',(-49.2850939815168,-44.5997392963807,
-0.848737750489605));
#42913=CARTESIAN_POINT('Ctrl Pts',(-49.3820477911778,-45.7030074740777,
-0.783450231221174));
#42914=CARTESIAN_POINT('Ctrl Pts',(-49.3906770071057,-45.8012020614281,
-0.777639421897305));
#42915=CARTESIAN_POINT('Ctrl Pts',(-49.3946191616459,-45.8998054662665,
-0.771828612573436));
#42916=CARTESIAN_POINT('Ctrl Pts',(-49.3940299756876,-45.9984545908008,
-0.766017803249567));
#42917=CARTESIAN_POINT('Ctrl Pts',(-47.0579044229729,-49.9456385074984,
5.55111512312578E-16));
#42918=CARTESIAN_POINT('Ctrl Pts',(-48.3527480267224,-49.5984650974504,
-0.0652875192684306));
#42919=CARTESIAN_POINT('Ctrl Pts',(-50.5530323995854,-47.5357692714295,
-0.195862557805293));
#42920=CARTESIAN_POINT('Ctrl Pts',(-49.798918270059,-43.0499899242987,-0.391725115610586));
#42921=CARTESIAN_POINT('Ctrl Pts',(-45.6441921539078,-41.2067322013831,
-0.58758767341588));
#42922=CARTESIAN_POINT('Ctrl Pts',(-41.8104753331013,-43.6427683056469,
-0.783450231221174));
#42923=CARTESIAN_POINT('Ctrl Pts',(-41.7184180535194,-48.1865095079258,
-0.979312789026466));
#42924=CARTESIAN_POINT('Ctrl Pts',(-45.4525334082598,-50.7759013692154,
-1.17517534683176));
#42925=CARTESIAN_POINT('Ctrl Pts',(-49.6754254318228,-49.098593633004,-1.37103790463705));
#42926=CARTESIAN_POINT('Ctrl Pts',(-50.6146438233287,-44.6526230577962,
-1.56690046244235));
#42927=CARTESIAN_POINT('Ctrl Pts',(-47.4307680051951,-41.41057421285,-1.76276302024764));
#42928=CARTESIAN_POINT('Ctrl Pts',(-42.9685984702712,-42.2689561020525,
-1.95862557805293));
#42929=CARTESIAN_POINT('Ctrl Pts',(-41.2148490309835,-46.4609045794214,
-2.15448813585823));
#42930=CARTESIAN_POINT('Ctrl Pts',(-43.7364585340961,-50.2410417148001,
-2.35035069366352));
#42931=CARTESIAN_POINT('Ctrl Pts',(-48.2804504821097,-50.2319761154881,
-2.54621325146882));
#42932=CARTESIAN_POINT('Ctrl Pts',(-50.7869498812151,-46.4417996865353,
-2.74207580927411));
#42933=CARTESIAN_POINT('Ctrl Pts',(-49.0164920780277,-42.2568934559197,
-2.9379383670794));
#42934=CARTESIAN_POINT('Ctrl Pts',(-44.5509149516467,-41.4163086543115,
-3.1338009248847));
#42935=CARTESIAN_POINT('Ctrl Pts',(-41.3800394184348,-44.6710764629181,
-3.32966348268999));
#42936=CARTESIAN_POINT('Ctrl Pts',(-42.3369215031958,-49.1131863035692,
-3.52552604049529));
#42937=CARTESIAN_POINT('Ctrl Pts',(-46.5666235775808,-50.7737837298756,
-3.72138859830058));
#42938=CARTESIAN_POINT('Ctrl Pts',(-50.2900692643348,-48.1691885628536,
-3.91725115610587));
#42939=CARTESIAN_POINT('Ctrl Pts',(-50.180502688043,-43.6265066797266,-4.11311371391116));
#42940=CARTESIAN_POINT('Ctrl Pts',(-46.3358174043579,-41.204449981662,-4.30897627171646));
#42941=CARTESIAN_POINT('Ctrl Pts',(-42.1910921533903,-43.0670331890375,
-4.50483882952175));
#42942=CARTESIAN_POINT('Ctrl Pts',(-41.4494798905217,-47.5501096808741,
-4.70070138732705));
#42943=CARTESIAN_POINT('Ctrl Pts',(-44.7735827067234,-50.6482226625802,
-4.89656394513233));
#42944=CARTESIAN_POINT('Ctrl Pts',(-49.1934423111539,-49.5933270812414,
-5.09242650293764));
#42945=CARTESIAN_POINT('Ctrl Pts',(-50.7600837602575,-45.3279316541825,
-5.28828906074292));
#42946=CARTESIAN_POINT('Ctrl Pts',(-48.0737730601331,-41.6630035036824,
-5.48415161854822));
#42947=CARTESIAN_POINT('Ctrl Pts',(-43.5346256929101,-41.8730152769562,
-5.68001417635351));
#42948=CARTESIAN_POINT('Ctrl Pts',(-41.1981957029014,-45.7703295255252,
-5.87587673415881));
#42949=CARTESIAN_POINT('Ctrl Pts',(-43.1519934739611,-49.8728455133488,
-6.0717392919641));
#42950=CARTESIAN_POINT('Ctrl Pts',(-47.6503759783394,-50.5151226960096,
-6.26760184976939));
#42951=CARTESIAN_POINT('Ctrl Pts',(-50.6742104721782,-47.1233109626991,
-6.46346440757469));
#42952=CARTESIAN_POINT('Ctrl Pts',(-49.5218181321677,-42.7278641268702,
-6.65932696537998));
#42953=CARTESIAN_POINT('Ctrl Pts',(-45.2228147324014,-41.2559448461001,
-6.85518952318528));
#42954=CARTESIAN_POINT('Ctrl Pts',(-41.6182000513892,-44.022657337512,-7.05105208099056));
#42955=CARTESIAN_POINT('Ctrl Pts',(-41.9285482915987,-48.5560484764118,
-7.24691463879586));
#42956=CARTESIAN_POINT('Ctrl Pts',(-45.8765970410433,-50.8057107187776,
-7.44277719660115));
#42957=CARTESIAN_POINT('Ctrl Pts',(-49.9348716345255,-48.761650115466,-7.63863975440645));
#42958=CARTESIAN_POINT('Ctrl Pts',(-50.4775506806467,-44.2501708246775,
-7.83450231221174));
#42959=CARTESIAN_POINT('Ctrl Pts',(-47.0195848331003,-41.3020769083036,
-8.03036487001704));
#42960=CARTESIAN_POINT('Ctrl Pts',(-42.6509149775089,-42.5514375357737,
-8.22622742782233));
#42961=CARTESIAN_POINT('Ctrl Pts',(-41.2740009567628,-46.8818734807212,
-8.42208998562762));
#42962=CARTESIAN_POINT('Ctrl Pts',(-44.1206550171574,-50.4245588063534,
-8.61795254343291));
#42963=CARTESIAN_POINT('Ctrl Pts',(-48.6442455574373,-50.0137240618373,
-8.81381510123821));
#42964=CARTESIAN_POINT('Ctrl Pts',(-50.8097851438853,-46.0175025423462,
-9.0096776590435));
#42965=CARTESIAN_POINT('Ctrl Pts',(-48.6687263145852,-42.0041782891898,
-9.2055402168488));
#42966=CARTESIAN_POINT('Ctrl Pts',(-45.6668068080595,-41.7135846407913,
-9.33611525538566));
#42967=CARTESIAN_POINT('Ctrl Pts',(-44.4292895827202,-42.2290460377978,
-9.40140277465409));
#42968=CARTESIAN_POINT('Ctrl Pts',(-46.9978874462229,-49.7217947561856,
0.133800924884696));
#42969=CARTESIAN_POINT('Ctrl Pts',(-48.219272052379,-49.3943171693393,0.0685134056162651));
#42970=CARTESIAN_POINT('Ctrl Pts',(-50.2947300106983,-47.4486420918325,
-0.0620616329205972));
#42971=CARTESIAN_POINT('Ctrl Pts',(-49.5833982433549,-43.2173497370389,
-0.257924190725891));
#42972=CARTESIAN_POINT('Ctrl Pts',(-45.6643778254701,-41.4786636119901,
-0.453786748531184));
#42973=CARTESIAN_POINT('Ctrl Pts',(-42.0481552208745,-43.7764986471809,
-0.649649306336477));
#42974=CARTESIAN_POINT('Ctrl Pts',(-41.9613205299201,-48.0624645682778,
-0.845511864141771));
#42975=CARTESIAN_POINT('Ctrl Pts',(-45.4835922534583,-50.504955189946,-1.04137442194706));
#42976=CARTESIAN_POINT('Ctrl Pts',(-49.4669113941667,-48.922804385893,-1.23723697975236));
#42977=CARTESIAN_POINT('Ctrl Pts',(-50.352846098468,-44.7290623739175,-1.43309953755765));
#42978=CARTESIAN_POINT('Ctrl Pts',(-47.3495977517792,-41.6709412694405,
-1.62896209536294));
#42979=CARTESIAN_POINT('Ctrl Pts',(-43.140575778598,-42.4806254835333,-1.82482465316824));
#42980=CARTESIAN_POINT('Ctrl Pts',(-41.4863199580507,-46.434756565644,-2.02068721097353));
#42981=CARTESIAN_POINT('Ctrl Pts',(-43.8648736466354,-50.0004391646398,
-2.21654976877883));
#42982=CARTESIAN_POINT('Ctrl Pts',(-48.1510760881736,-49.9918878744197,
-2.41241232658412));
#42983=CARTESIAN_POINT('Ctrl Pts',(-50.5153768983579,-46.4167355305122,
-2.60827488438941));
#42984=CARTESIAN_POINT('Ctrl Pts',(-48.845360611912,-42.4692471747913,-2.80413744219471));
#42985=CARTESIAN_POINT('Ctrl Pts',(-44.6331243665686,-41.6763503848778,
-3.));
#42986=CARTESIAN_POINT('Ctrl Pts',(-41.6421387733376,-44.7464688814539,
-3.19586255780529));
#42987=CARTESIAN_POINT('Ctrl Pts',(-42.5447350751993,-48.9365691858576,
-3.39172511561059));
#42988=CARTESIAN_POINT('Ctrl Pts',(-46.5344779192933,-50.5029576884072,
-3.58758767341588));
#42989=CARTESIAN_POINT('Ctrl Pts',(-50.0466852858747,-48.0461262741287,
-3.78345023122117));
#42990=CARTESIAN_POINT('Ctrl Pts',(-49.9433346346883,-43.7611595749465,
-3.97931278902647));
#42991=CARTESIAN_POINT('Ctrl Pts',(-46.3167658294595,-41.4765108670353,
-4.17517534683176));
#42992=CARTESIAN_POINT('Ctrl Pts',(-42.4071789082133,-43.2334261042004,
-4.37103790463705));
#42993=CARTESIAN_POINT('Ctrl Pts',(-41.7076397523018,-47.4621689419408,
-4.56690046244235));
#42994=CARTESIAN_POINT('Ctrl Pts',(-44.8431597465561,-50.3845199448194,
-4.76276302024764));
#42995=CARTESIAN_POINT('Ctrl Pts',(-49.0122721139422,-49.3894706427891,
-4.95862557805293));
#42996=CARTESIAN_POINT('Ctrl Pts',(-50.4900349447276,-45.3660593993828,
-5.15448813585823));
#42997=CARTESIAN_POINT('Ctrl Pts',(-47.95612387857,-41.9090497553401,-5.35035069366352));
#42998=CARTESIAN_POINT('Ctrl Pts',(-43.6744911753258,-42.1071471520028,
-5.54621325146882));
#42999=CARTESIAN_POINT('Ctrl Pts',(-41.4706114056805,-45.7833591785141,
-5.7420758092741));
#43000=CARTESIAN_POINT('Ctrl Pts',(-43.3135664268153,-49.6531314502598,
-5.93793836707941));
#43001=CARTESIAN_POINT('Ctrl Pts',(-47.5567469372182,-50.2589709983841,
-6.13380092488469));
#43002=CARTESIAN_POINT('Ctrl Pts',(-50.4090334154029,-47.0595833456598,
-6.32966348269));
#43003=CARTESIAN_POINT('Ctrl Pts',(-49.3220185355631,-42.9134987630019,
-6.52552604049528));
#43004=CARTESIAN_POINT('Ctrl Pts',(-45.2669059651471,-41.5250843275974,
-6.72138859830058));
#43005=CARTESIAN_POINT('Ctrl Pts',(-41.8667880900894,-44.1348358349494,
-6.91725115610587));
#43006=CARTESIAN_POINT('Ctrl Pts',(-42.1595296706494,-48.4110388719054,
-7.11311371391116));
#43007=CARTESIAN_POINT('Ctrl Pts',(-45.8835979310649,-50.5330733970942,
-7.30897627171647));
#43008=CARTESIAN_POINT('Ctrl Pts',(-49.7116387088703,-48.6049763298456,
-7.50483882952174));
#43009=CARTESIAN_POINT('Ctrl Pts',(-50.2235305165733,-44.3494420392139,
-7.70070138732705));
#43010=CARTESIAN_POINT('Ctrl Pts',(-46.9617418012592,-41.5685992281323,
-7.89656394513233));
#43011=CARTESIAN_POINT('Ctrl Pts',(-42.840915088638,-42.7470811957699,-8.09242650293763));
#43012=CARTESIAN_POINT('Ctrl Pts',(-41.5421160799624,-46.8318430819068,
-8.28828906074292));
#43013=CARTESIAN_POINT('Ctrl Pts',(-44.2272739155108,-50.1735449744385,
-8.48415161854822));
#43014=CARTESIAN_POINT('Ctrl Pts',(-48.4942323608801,-49.7860176845225,
-8.68001417635351));
#43015=CARTESIAN_POINT('Ctrl Pts',(-50.5369166721361,-46.0165095890564,
-8.8758767341588));
#43016=CARTESIAN_POINT('Ctrl Pts',(-48.5173242770319,-42.2308690312902,
-9.0717392919641));
#43017=CARTESIAN_POINT('Ctrl Pts',(-45.6857095062803,-41.9567613261026,
-9.20231433050096));
#43018=CARTESIAN_POINT('Ctrl Pts',(-44.5183990415218,-42.4429795948946,
-9.26760184976939));
#43019=CARTESIAN_POINT('Ctrl Pts',(-46.9378704694728,-49.4979510048728,
0.267601849769392));
#43020=CARTESIAN_POINT('Ctrl Pts',(-48.0857960780355,-49.1901692412281,
0.202314330500961));
#43021=CARTESIAN_POINT('Ctrl Pts',(-50.0364276218112,-47.3615149122355,
0.0717392919640985));
#43022=CARTESIAN_POINT('Ctrl Pts',(-49.3678782166508,-43.3847095497791,
-0.124123265841195));
#43023=CARTESIAN_POINT('Ctrl Pts',(-45.6845634970324,-41.750595022597,-0.319985823646488));
#43024=CARTESIAN_POINT('Ctrl Pts',(-42.2858351086478,-43.9102289887149,
-0.515848381451782));
#43025=CARTESIAN_POINT('Ctrl Pts',(-42.2042230063208,-47.9384196286299,
-0.711710939257077));
#43026=CARTESIAN_POINT('Ctrl Pts',(-45.5146510986568,-50.2340090106765,
-0.907573497062368));
#43027=CARTESIAN_POINT('Ctrl Pts',(-49.2583973565106,-48.7470151387819,
-1.10343605486766));
#43028=CARTESIAN_POINT('Ctrl Pts',(-50.0910483736072,-44.8055016900389,
-1.29929861267296));
#43029=CARTESIAN_POINT('Ctrl Pts',(-47.2684274983633,-41.9313083260309,
-1.49516117047825));
#43030=CARTESIAN_POINT('Ctrl Pts',(-43.3125530869246,-42.6922948650142,
-1.69102372828354));
#43031=CARTESIAN_POINT('Ctrl Pts',(-41.757790885118,-46.4086085518666,-1.88688628608884));
#43032=CARTESIAN_POINT('Ctrl Pts',(-43.9932887591747,-49.7598366144794,
-2.08274884389413));
#43033=CARTESIAN_POINT('Ctrl Pts',(-48.0217016942375,-49.7517996333514,
-2.27861140169942));
#43034=CARTESIAN_POINT('Ctrl Pts',(-50.2438039155007,-46.391671374489,-2.47447395950472));
#43035=CARTESIAN_POINT('Ctrl Pts',(-48.6742291457962,-42.681600893663,-2.67033651731001));
#43036=CARTESIAN_POINT('Ctrl Pts',(-44.7153337814905,-41.936392115444,-2.8661990751153));
#43037=CARTESIAN_POINT('Ctrl Pts',(-41.9042381282403,-44.8218612999897,
-3.0620616329206));
#43038=CARTESIAN_POINT('Ctrl Pts',(-42.7525486472029,-48.7599520681459,
-3.25792419072589));
#43039=CARTESIAN_POINT('Ctrl Pts',(-46.5023322610058,-50.2321316469387,
-3.45378674853119));
#43040=CARTESIAN_POINT('Ctrl Pts',(-49.8033013074145,-47.9230639854038,
-3.64964930633647));
#43041=CARTESIAN_POINT('Ctrl Pts',(-49.7061665813336,-43.8958124701664,
-3.84551186414177));
#43042=CARTESIAN_POINT('Ctrl Pts',(-46.2977142545611,-41.7485717524086,
-4.04137442194706));
#43043=CARTESIAN_POINT('Ctrl Pts',(-42.6232656630362,-43.3998190193633,
-4.23723697975236));
#43044=CARTESIAN_POINT('Ctrl Pts',(-41.9657996140819,-47.3742282030075,
-4.43309953755765));
#43045=CARTESIAN_POINT('Ctrl Pts',(-44.9127367863888,-50.1208172270585,
-4.62896209536295));
#43046=CARTESIAN_POINT('Ctrl Pts',(-48.8311019167305,-49.1856142043368,
-4.82482465316824));
#43047=CARTESIAN_POINT('Ctrl Pts',(-50.2199861291977,-45.4041871445831,
-5.02068721097353));
#43048=CARTESIAN_POINT('Ctrl Pts',(-47.8384746970067,-42.1550960069977,
-5.21654976877883));
#43049=CARTESIAN_POINT('Ctrl Pts',(-43.8143566577415,-42.3412790270494,
-5.41241232658412));
#43050=CARTESIAN_POINT('Ctrl Pts',(-41.7430271084595,-45.7963888315029,
-5.60827488438941));
#43051=CARTESIAN_POINT('Ctrl Pts',(-43.4751393796696,-49.4334173871708,
-5.80413744219471));
#43052=CARTESIAN_POINT('Ctrl Pts',(-47.463117896097,-50.0028193007586,-6.));
#43053=CARTESIAN_POINT('Ctrl Pts',(-50.1438563586276,-46.9958557286205,
-6.19586255780529));
#43054=CARTESIAN_POINT('Ctrl Pts',(-49.1222189389585,-43.0991333991335,
-6.39172511561059));
#43055=CARTESIAN_POINT('Ctrl Pts',(-45.3109971978927,-41.7942238090946,
-6.58758767341588));
#43056=CARTESIAN_POINT('Ctrl Pts',(-42.1153761287897,-44.2470143323867,
-6.78345023122118));
#43057=CARTESIAN_POINT('Ctrl Pts',(-42.3905110497,-48.266029267399,-6.97931278902647));
#43058=CARTESIAN_POINT('Ctrl Pts',(-45.8905988210865,-50.2604360754108,
-7.17517534683176));
#43059=CARTESIAN_POINT('Ctrl Pts',(-49.4884057832152,-48.4483025442253,
-7.37103790463705));
#43060=CARTESIAN_POINT('Ctrl Pts',(-49.9695103524998,-44.4487132537502,
-7.56690046244235));
#43061=CARTESIAN_POINT('Ctrl Pts',(-46.9038987694181,-41.8351215479612,
-7.76276302024765));
#43062=CARTESIAN_POINT('Ctrl Pts',(-43.030915199767,-42.942724855766,-7.95862557805293));
#43063=CARTESIAN_POINT('Ctrl Pts',(-41.8102312031619,-46.7818126830923,
-8.15448813585824));
#43064=CARTESIAN_POINT('Ctrl Pts',(-44.3338928138642,-49.9225311425236,
-8.35035069366352));
#43065=CARTESIAN_POINT('Ctrl Pts',(-48.3442191643229,-49.5583113072078,
-8.54621325146882));
#43066=CARTESIAN_POINT('Ctrl Pts',(-50.2640482003868,-46.0155166357666,
-8.74207580927411));
#43067=CARTESIAN_POINT('Ctrl Pts',(-48.3659222394787,-42.4575597733907,
-8.93793836707941));
#43068=CARTESIAN_POINT('Ctrl Pts',(-45.7046122045012,-42.1999380114139,
-9.06851340561627));
#43069=CARTESIAN_POINT('Ctrl Pts',(-44.6075085003234,-42.6569131519913,
-9.1338009248847));
#43070=CARTESIAN_POINT('Ctrl Pts',(-46.8778534927228,-49.27410725356,0.401402774654088));
#43071=CARTESIAN_POINT('Ctrl Pts',(-47.9523201036921,-48.9860213131169,
0.336115255385657));
#43072=CARTESIAN_POINT('Ctrl Pts',(-49.7781252329241,-47.2743877326385,
0.205540216848794));
#43073=CARTESIAN_POINT('Ctrl Pts',(-49.1523581899468,-43.5520693625194,
0.00967765904350067));
#43074=CARTESIAN_POINT('Ctrl Pts',(-45.7047491685946,-42.0225264332039,
-0.186184898761793));
#43075=CARTESIAN_POINT('Ctrl Pts',(-42.5235149964211,-44.0439593302489,
-0.382047456567086));
#43076=CARTESIAN_POINT('Ctrl Pts',(-42.4471254827216,-47.814374688982,-0.57791001437238));
#43077=CARTESIAN_POINT('Ctrl Pts',(-45.5457099438552,-49.963062831407,-0.773772572177673));
#43078=CARTESIAN_POINT('Ctrl Pts',(-49.0498833188546,-48.5712258916709,
-0.969635129982967));
#43079=CARTESIAN_POINT('Ctrl Pts',(-49.8292506487463,-44.8819410061602,
-1.16549768778826));
#43080=CARTESIAN_POINT('Ctrl Pts',(-47.1872572449474,-42.1916753826214,
-1.36136024559355));
#43081=CARTESIAN_POINT('Ctrl Pts',(-43.4845303952514,-42.9039642464951,
-1.55722280339885));
#43082=CARTESIAN_POINT('Ctrl Pts',(-42.0292618121851,-46.3824605380891,
-1.75308536120414));
#43083=CARTESIAN_POINT('Ctrl Pts',(-44.1217038717141,-49.5192340643191,
-1.94894791900943));
#43084=CARTESIAN_POINT('Ctrl Pts',(-47.8923273003014,-49.5117113922829,
-2.14481047681473));
#43085=CARTESIAN_POINT('Ctrl Pts',(-49.9722309326436,-46.3666072184659,
-2.34067303462002));
#43086=CARTESIAN_POINT('Ctrl Pts',(-48.5030976796804,-42.8939546125346,
-2.53653559242531));
#43087=CARTESIAN_POINT('Ctrl Pts',(-44.7975431964124,-42.1964338460104,
-2.73239815023061));
#43088=CARTESIAN_POINT('Ctrl Pts',(-42.166337483143,-44.8972537185255,-2.9282607080359));
#43089=CARTESIAN_POINT('Ctrl Pts',(-42.9603622192064,-48.5833349504342,
-3.1241232658412));
#43090=CARTESIAN_POINT('Ctrl Pts',(-46.4701866027183,-49.9613056054703,
-3.31998582364649));
#43091=CARTESIAN_POINT('Ctrl Pts',(-49.5599173289544,-47.8000016966788,
-3.51584838145178));
#43092=CARTESIAN_POINT('Ctrl Pts',(-49.4689985279789,-44.0304653653864,
-3.71171093925708));
#43093=CARTESIAN_POINT('Ctrl Pts',(-46.2786626796627,-42.0206326377818,
-3.90757349706237));
#43094=CARTESIAN_POINT('Ctrl Pts',(-42.8393524178592,-43.5662119345263,
-4.10343605486766));
#43095=CARTESIAN_POINT('Ctrl Pts',(-42.2239594758619,-47.2862874640742,
-4.29929861267296));
#43096=CARTESIAN_POINT('Ctrl Pts',(-44.9823138262216,-49.8571145092977,
-4.49516117047825));
#43097=CARTESIAN_POINT('Ctrl Pts',(-48.6499317195187,-48.9817577658845,
-4.69102372828354));
#43098=CARTESIAN_POINT('Ctrl Pts',(-49.9499373136678,-45.4423148897834,
-4.88688628608884));
#43099=CARTESIAN_POINT('Ctrl Pts',(-47.7208255154434,-42.4011422586555,
-5.08274884389413));
#43100=CARTESIAN_POINT('Ctrl Pts',(-43.9542221401571,-42.575410902096,-5.27861140169943));
#43101=CARTESIAN_POINT('Ctrl Pts',(-42.0154428112387,-45.8094184844919,
-5.47447395950472));
#43102=CARTESIAN_POINT('Ctrl Pts',(-43.6367123325237,-49.2137033240818,
-5.67033651731001));
#43103=CARTESIAN_POINT('Ctrl Pts',(-47.3694888549758,-49.7466676031331,
-5.86619907511531));
#43104=CARTESIAN_POINT('Ctrl Pts',(-49.8786793018522,-46.9321281115812,
-6.0620616329206));
#43105=CARTESIAN_POINT('Ctrl Pts',(-48.9224193423538,-43.2847680352652,
-6.25792419072589));
#43106=CARTESIAN_POINT('Ctrl Pts',(-45.3550884306384,-42.0633632905919,
-6.45378674853118));
#43107=CARTESIAN_POINT('Ctrl Pts',(-42.3639641674899,-44.3591928298241,
-6.64964930633648));
#43108=CARTESIAN_POINT('Ctrl Pts',(-42.6214924287507,-48.1210196628927,
-6.84551186414177));
#43109=CARTESIAN_POINT('Ctrl Pts',(-45.8975997111081,-49.9877987537274,
-7.04137442194707));
#43110=CARTESIAN_POINT('Ctrl Pts',(-49.2651728575601,-48.2916287586049,
-7.23723697975236));
#43111=CARTESIAN_POINT('Ctrl Pts',(-49.7154901884265,-44.5479844682866,
-7.43309953755765));
#43112=CARTESIAN_POINT('Ctrl Pts',(-46.8460557375769,-42.1016438677899,
-7.62896209536295));
#43113=CARTESIAN_POINT('Ctrl Pts',(-43.2209153108962,-43.1383685157623,
-7.82482465316823));
#43114=CARTESIAN_POINT('Ctrl Pts',(-42.0783463263615,-46.7317822842778,
-8.02068721097354));
#43115=CARTESIAN_POINT('Ctrl Pts',(-44.4405117122176,-49.6715173106087,
-8.21654976877882));
#43116=CARTESIAN_POINT('Ctrl Pts',(-48.1942059677658,-49.330604929893,-8.41241232658413));
#43117=CARTESIAN_POINT('Ctrl Pts',(-49.9911797286376,-46.0145236824768,
-8.60827488438941));
#43118=CARTESIAN_POINT('Ctrl Pts',(-48.2145202019254,-42.6842505154911,
-8.80413744219471));
#43119=CARTESIAN_POINT('Ctrl Pts',(-45.723514902722,-42.4431146967252,-8.93471248073157));
#43120=CARTESIAN_POINT('Ctrl Pts',(-44.696617959125,-42.8708467090881,-9.));
#43121=CARTESIAN_POINT('Ctrl Pts',(-49.3881103126091,-45.9972329022571,
-1.10898219675043));
#43122=CARTESIAN_POINT('Ctrl Pts',(-49.3906987648108,-45.6759065142304,
-1.12782069376304));
#43123=CARTESIAN_POINT('Ctrl Pts',(-49.348599621807,-45.3552439043751,-1.14665919077565));
#43124=CARTESIAN_POINT('Ctrl Pts',(-49.2590238597979,-45.0484442164888,
-1.16549768778826));
#43125=CARTESIAN_POINT('Ctrl Pts',(-48.9485861808133,-43.9851857983139,
-1.23078520705669));
#43126=CARTESIAN_POINT('Ctrl Pts',(-48.0679217128803,-43.0884305904677,
-1.29607272632512));
#43127=CARTESIAN_POINT('Ctrl Pts',(-47.0104683372979,-42.7587677971901,
-1.36136024559355));
#43128=CARTESIAN_POINT('Ctrl Pts',(-45.9530149617154,-42.4291050039126,
-1.42664776486198));
#43129=CARTESIAN_POINT('Ctrl Pts',(-44.7187726784834,-42.6665346252038,
-1.49193528413041));
#43130=CARTESIAN_POINT('Ctrl Pts',(-43.859106773023,-43.3649988177818,-1.55722280339884));
#43131=CARTESIAN_POINT('Ctrl Pts',(-42.9994408675627,-44.0634630103597,
-1.62251032266727));
#43132=CARTESIAN_POINT('Ctrl Pts',(-42.5143513398739,-45.2229617742244,
-1.6877978419357));
#43133=CARTESIAN_POINT('Ctrl Pts',(-42.6205469192844,-46.3255067438617,
-1.75308536120414));
#43134=CARTESIAN_POINT('Ctrl Pts',(-42.7267424986948,-47.4280517134991,
-1.81837288047257));
#43135=CARTESIAN_POINT('Ctrl Pts',(-43.4242231852045,-48.4736428889091,
-1.883660399741));
#43136=CARTESIAN_POINT('Ctrl Pts',(-44.4014007665572,-48.9951846979414,
-1.94894791900943));
#43137=CARTESIAN_POINT('Ctrl Pts',(-45.3785783479099,-49.5167265069737,
-2.01423543827786));
#43138=CARTESIAN_POINT('Ctrl Pts',(-46.6354528241056,-49.5142189496283,
-2.07952295754629));
#43139=CARTESIAN_POINT('Ctrl Pts',(-47.6105406675939,-48.9887811419861,
-2.14481047681472));
#43140=CARTESIAN_POINT('Ctrl Pts',(-48.5856285110821,-48.4633433343439,
-2.21009799608315));
#43141=CARTESIAN_POINT('Ctrl Pts',(-49.2789297218628,-47.4149752764049,
-2.27538551535158));
#43142=CARTESIAN_POINT('Ctrl Pts',(-49.3807247850927,-46.3120158131135,
-2.34067303462002));
#43143=CARTESIAN_POINT('Ctrl Pts',(-49.3902405513404,-46.2089115553985,
-2.34677608866349));
#43144=CARTESIAN_POINT('Ctrl Pts',(-49.3945874743613,-46.105330253756,-2.35287914270696));
#43145=CARTESIAN_POINT('Ctrl Pts',(-49.393944259473,-46.0016943208402,-2.35898219675043));
#43146=CARTESIAN_POINT('Ctrl Pts',(-47.0579044229729,-49.9456385074984,
5.55111512312578E-16));
#43147=CARTESIAN_POINT('Ctrl Pts',(-47.1733693372504,-49.9039985328978,
5.66013349383169E-16));
#43148=CARTESIAN_POINT('Ctrl Pts',(-47.2864786532175,-49.8568504145239,
5.21146057028503E-16));
#43149=CARTESIAN_POINT('Ctrl Pts',(-47.3970077281708,-49.804548304315,4.47558656802016E-16));
#43150=CARTESIAN_POINT('Ctrl Pts',(-47.5098934841488,-49.7511310179344,
3.72402239284464E-16));
#43151=CARTESIAN_POINT('Ctrl Pts',(-47.620088418098,-49.6923370616094,4.47268168963809E-16));
#43152=CARTESIAN_POINT('Ctrl Pts',(-47.7273259226398,-49.6284969725913,
5.48172618408671E-16));
#43153=CARTESIAN_POINT('Ctrl Pts',(-47.8392942950329,-49.561840527243,6.53528547939391E-16));
#43154=CARTESIAN_POINT('Ctrl Pts',(-47.9480394609077,-49.4896823744086,
7.20663869194476E-16));
#43155=CARTESIAN_POINT('Ctrl Pts',(-48.0532163752826,-49.4123564527643,
7.42461647718073E-16));
#43156=CARTESIAN_POINT('Ctrl Pts',(-48.1452461753606,-49.3446962713255,
7.61534703926221E-16));
#43157=CARTESIAN_POINT('Ctrl Pts',(-48.2345436748161,-49.2730785145345,
1.00926389872883E-15));
#43158=CARTESIAN_POINT('Ctrl Pts',(-48.3208451029165,-49.1977075112963,
1.01307850997046E-15));
#43159=CARTESIAN_POINT('Ctrl Pts',(-48.3378049250329,-49.1828957192345,
1.01382815142513E-15));
#43160=CARTESIAN_POINT('Ctrl Pts',(-48.3546489363343,-49.1679389353915,
5.86365414716671E-16));
#43161=CARTESIAN_POINT('Ctrl Pts',(-48.3713749781207,-49.1528386522715,
5.82867087928207E-16));
#43162=CARTESIAN_POINT('Ctrl Pts',(-48.3839971030697,-49.1414433883627,
5.80227113784865E-16));
#43163=CARTESIAN_POINT('Ctrl Pts',(-48.3965520031907,-49.1299663623313,
3.88578058618805E-16));
#43164=CARTESIAN_POINT('Ctrl Pts',(-48.4090283192252,-49.1184180896672,
3.88578058618805E-16));
#43165=CARTESIAN_POINT('Ctrl Pts',(-48.4995034915464,-49.034672859391,3.88578058618805E-16));
#43166=CARTESIAN_POINT('Ctrl Pts',(-48.585990505988,-48.9470573638322,2.49245464307548E-16));
#43167=CARTESIAN_POINT('Ctrl Pts',(-48.6682317367018,-48.8558860449089,
3.05311331771918E-16));
#43168=CARTESIAN_POINT('Ctrl Pts',(-48.7501471507582,-48.7650759211444,
3.61155082016356E-16));
#43169=CARTESIAN_POINT('Ctrl Pts',(-48.8278508314432,-48.6707373593851,
2.40491596001199E-16));
#43170=CARTESIAN_POINT('Ctrl Pts',(-48.9010457239218,-48.573152188254,4.16333634234434E-17));
#43171=CARTESIAN_POINT('Ctrl Pts',(-48.9731614105922,-48.4770058399686,
-1.54292848184616E-16));
#43172=CARTESIAN_POINT('Ctrl Pts',(-49.0409006391222,-48.3777072181801,
1.86597674064836E-16));
#43173=CARTESIAN_POINT('Ctrl Pts',(-49.1039319851986,-48.2755084011431,
8.32667268468867E-17));
#43174=CARTESIAN_POINT('Ctrl Pts',(-49.1554910626096,-48.191910682755,-1.25706390486376E-18));
#43175=CARTESIAN_POINT('Ctrl Pts',(-49.2038992954219,-48.1063719477112,
5.41938973494124E-16));
#43176=CARTESIAN_POINT('Ctrl Pts',(-49.2489486618552,-48.0190260212161,
5.55111512312578E-16));
#43177=CARTESIAN_POINT('Ctrl Pts',(-49.2595828404022,-47.998407480907,5.58220970686877E-16));
#43178=CARTESIAN_POINT('Ctrl Pts',(-49.270029742428,-47.9776882326517,9.06864741724049E-16));
#43179=CARTESIAN_POINT('Ctrl Pts',(-49.2802864197024,-47.9568700298176,
9.15933995315754E-16));
#43180=CARTESIAN_POINT('Ctrl Pts',(-49.287528246751,-47.9421711346146,9.2233743028929E-16));
#43181=CARTESIAN_POINT('Ctrl Pts',(-49.2946745182361,-47.9274242550742,
-3.81840268582438E-17));
#43182=CARTESIAN_POINT('Ctrl Pts',(-49.3017191206196,-47.9126411190135,
-2.77555756156289E-17));
#43183=CARTESIAN_POINT('Ctrl Pts',(-49.3523583097563,-47.8063745077476,
4.72079618742721E-17));
#43184=CARTESIAN_POINT('Ctrl Pts',(-49.3978249076527,-47.6980808260915,
-4.96970061520271E-16));
#43185=CARTESIAN_POINT('Ctrl Pts',(-49.4378477716308,-47.5880161091457,
-4.9960036108132E-16));
#43186=CARTESIAN_POINT('Ctrl Pts',(-49.4770644924164,-47.4801683230611,
-5.02177680973382E-16));
#43187=CARTESIAN_POINT('Ctrl Pts',(-49.5110547933194,-47.3706194935391,
4.57968148600611E-17));
#43188=CARTESIAN_POINT('Ctrl Pts',(-49.5395146923287,-47.2595997093103,
2.77555756156289E-17));
#43189=CARTESIAN_POINT('Ctrl Pts',(-49.544975138073,-47.2382989482596,2.42941013489102E-17));
#43190=CARTESIAN_POINT('Ctrl Pts',(-49.5502318456946,-47.2169440218678,
-4.52064932513013E-16));
#43191=CARTESIAN_POINT('Ctrl Pts',(-49.5552824461283,-47.1955365379506,
-4.71844785465692E-16));
#43192=CARTESIAN_POINT('Ctrl Pts',(-49.5824903881121,-47.0802129070123,
-6.35243347783829E-16));
#43193=CARTESIAN_POINT('Ctrl Pts',(-49.6037211273402,-46.9633633041741,
-3.31089260042331E-16));
#43194=CARTESIAN_POINT('Ctrl Pts',(-49.6190592501821,-46.8454242871399,
-4.16333634234434E-16));
#43195=CARTESIAN_POINT('Ctrl Pts',(-49.6275696309687,-46.7799856441651,
-4.63631604903081E-16));
#43196=CARTESIAN_POINT('Ctrl Pts',(-49.634264983748,-46.7142117486677,-2.27956851258612E-16));
#43197=CARTESIAN_POINT('Ctrl Pts',(-49.6391531642022,-46.6481791918392,
-2.22044604925031E-16));
#43198=CARTESIAN_POINT('Ctrl Pts',(-49.6410794249398,-46.6221580735902,
-2.1971479568619E-16));
#43199=CARTESIAN_POINT('Ctrl Pts',(-49.6427250054364,-46.596096810251,4.98233321211434E-16));
#43200=CARTESIAN_POINT('Ctrl Pts',(-49.6440901965306,-46.5700001834423,
5.27355936696949E-16));
#43201=CARTESIAN_POINT('Ctrl Pts',(-49.6449645924009,-46.553285466503,5.46008779378254E-16));
#43202=CARTESIAN_POINT('Ctrl Pts',(-49.6457239151094,-46.5365557747368,
6.58486149275759E-16));
#43203=CARTESIAN_POINT('Ctrl Pts',(-49.646367818249,-46.5198278005682,6.66133814775094E-16));
#43204=CARTESIAN_POINT('Ctrl Pts',(-49.6509450937801,-46.4009146564497,
7.20498314655799E-16));
#43205=CARTESIAN_POINT('Ctrl Pts',(-49.6497056526231,-46.2818992441625,
-3.44821266031896E-16));
#43206=CARTESIAN_POINT('Ctrl Pts',(-49.6428026243385,-46.1632168328176,
-3.88578058618805E-16));
#43207=CARTESIAN_POINT('Ctrl Pts',(-49.6360414897975,-46.0469739727774,
-4.31435417673498E-16));
#43208=CARTESIAN_POINT('Ctrl Pts',(-49.6238466714416,-45.9310496539742,
5.18747692508596E-16));
#43209=CARTESIAN_POINT('Ctrl Pts',(-49.6063097059683,-45.8158627002793,
5.55111512312578E-16));
#43210=CARTESIAN_POINT('Ctrl Pts',(-49.5889759985516,-45.7020107937674,
5.91053865851183E-16));
#43211=CARTESIAN_POINT('Ctrl Pts',(-49.56642285937,-45.5888784455779,2.91334207310992E-16));
#43212=CARTESIAN_POINT('Ctrl Pts',(-49.5386937754477,-45.4768924893138,
4.44089209850063E-16));
#43213=CARTESIAN_POINT('Ctrl Pts',(-49.5206040613618,-45.4038358410619,
5.43742495507627E-16));
#43214=CARTESIAN_POINT('Ctrl Pts',(-49.5003106142802,-45.3312675708399,
3.37381644489328E-17));
#43215=CARTESIAN_POINT('Ctrl Pts',(-49.4778162055683,-45.2593138849385,
5.55111512312578E-17));
#43216=CARTESIAN_POINT('Ctrl Pts',(-49.4685898053458,-45.2298010619024,
6.44416500351063E-17));
#43217=CARTESIAN_POINT('Ctrl Pts',(-49.4589930454642,-45.2003917152151,
5.1904603637396E-16));
#43218=CARTESIAN_POINT('Ctrl Pts',(-49.4490257849573,-45.171094919731,5.55111512312578E-16));
#43219=CARTESIAN_POINT('Ctrl Pts',(-49.4429390810481,-45.1532042546404,
5.77135605415197E-16));
#43220=CARTESIAN_POINT('Ctrl Pts',(-49.4367169044357,-45.1353635641357,
-3.8949053638378E-16));
#43221=CARTESIAN_POINT('Ctrl Pts',(-49.430361091836,-45.1175789294473,-3.33066907387547E-16));
#43222=CARTESIAN_POINT('Ctrl Pts',(-49.3921806745662,-45.0107436880449,
5.87916208435275E-18));
#43223=CARTESIAN_POINT('Ctrl Pts',(-49.3491645674419,-44.9058795780642,
7.07363767081224E-16));
#43224=CARTESIAN_POINT('Ctrl Pts',(-49.3013720780751,-44.8033974788009,
3.88578058618805E-16));
#43225=CARTESIAN_POINT('Ctrl Pts',(-49.2629804005143,-44.7210736709641,
1.3249769343093E-16));
#43226=CARTESIAN_POINT('Ctrl Pts',(-49.2215056579415,-44.6402872554315,
-1.03620088217595E-16));
#43227=CARTESIAN_POINT('Ctrl Pts',(-49.1769599094038,-44.5612680076514,
-2.22044604925031E-16));
#43228=CARTESIAN_POINT('Ctrl Pts',(-49.1548834013714,-44.5221067158202,
-2.80734825207282E-16));
#43229=CARTESIAN_POINT('Ctrl Pts',(-49.1320523745914,-44.4833797210652,
-9.37977106089326E-17));
#43230=CARTESIAN_POINT('Ctrl Pts',(-49.1084669149778,-44.4451166907322,
-1.66533453693773E-16));
#43231=CARTESIAN_POINT('Ctrl Pts',(-49.0950715621271,-44.4233852171529,
-2.07843691418425E-16));
#43232=CARTESIAN_POINT('Ctrl Pts',(-49.0814310539731,-44.4018008856244,
5.69071523681598E-16));
#43233=CARTESIAN_POINT('Ctrl Pts',(-49.0675590494629,-44.3803899179501,
5.55111512312578E-16));
#43234=CARTESIAN_POINT('Ctrl Pts',(-49.0090087392671,-44.2900195033499,
4.96189746868475E-16));
#43235=CARTESIAN_POINT('Ctrl Pts',(-48.9462914113485,-44.2026580989667,
1.12926594395583E-15));
#43236=CARTESIAN_POINT('Ctrl Pts',(-48.8794389832423,-44.1186868190207,
1.0547118733939E-15));
#43237=CARTESIAN_POINT('Ctrl Pts',(-48.8212020338695,-44.0455371770777,
9.89765815997824E-16));
#43238=CARTESIAN_POINT('Ctrl Pts',(-48.7598264591088,-43.9749604010674,
8.04362549974418E-16));
#43239=CARTESIAN_POINT('Ctrl Pts',(-48.6953138444556,-43.9072342030353,
9.99200722162641E-16));
#43240=CARTESIAN_POINT('Ctrl Pts',(-48.6572944668562,-43.8673209564524,
1.05974870095357E-15));
#43241=CARTESIAN_POINT('Ctrl Pts',(-48.6181851531445,-43.8283982895143,
2.13352833165291E-16));
#43242=CARTESIAN_POINT('Ctrl Pts',(-48.5780349767684,-43.7904875157198,
2.77555756156289E-16));
#43243=CARTESIAN_POINT('Origin',(-46.,-46.,-5.));
#43244=CARTESIAN_POINT('Origin',(0.,0.,0.));
#43245=CARTESIAN_POINT('',(-40.,-4.89858719658941E-15,4.));
#43246=CARTESIAN_POINT('Origin',(0.,0.,4.));
#43247=CARTESIAN_POINT('',(-40.,-4.89858719658941E-15,0.));
#43248=CARTESIAN_POINT('',(-40.,-4.89858719658941E-15,0.));
#43249=CARTESIAN_POINT('Origin',(0.,0.,0.));
#43250=CARTESIAN_POINT('Origin',(0.,0.,4.));
#43251=CARTESIAN_POINT('',(-20.,-2.44929359829471E-15,4.));
#43252=CARTESIAN_POINT('Origin',(0.,0.,4.));
#43253=CARTESIAN_POINT('Origin',(0.,0.,-10.));
#43254=CARTESIAN_POINT('',(-20.,-2.44929359829471E-15,-10.));
#43255=CARTESIAN_POINT('',(-20.,-2.44929359829471E-15,-10.));
#43256=CARTESIAN_POINT('Origin',(0.,0.,-10.));
#43257=CARTESIAN_POINT('Origin',(0.,0.,-10.));
#43258=CARTESIAN_POINT('',(-110.,1.34711147906209E-14,0.));
#43259=CARTESIAN_POINT('Origin',(0.,0.,0.));
#43260=CARTESIAN_POINT('',(-110.,1.34711147906209E-14,-10.));
#43261=CARTESIAN_POINT('',(-110.,-1.34711147906209E-14,-10.));
#43262=CARTESIAN_POINT('Origin',(0.,0.,-10.));
#43263=CARTESIAN_POINT('Origin',(0.,0.,0.));
#43264=CARTESIAN_POINT('Origin',(0.,0.,-10.));
#43265=CARTESIAN_POINT('',(0.,0.,0.));
#43266=CARTESIAN_POINT('Origin',(25.,0.,20.));
#43267=CARTESIAN_POINT('',(1.67595849469688,-5.1370281214151,20.0000980417081));
#43268=CARTESIAN_POINT('',(1.19904150530312,-5.13642988889554,19.9999056069319));
#43269=CARTESIAN_POINT('',(25.,-5.13675,20.));
#43270=CARTESIAN_POINT('',(0.,2.03511426366965,15.2835913560943));
#43271=CARTESIAN_POINT('Ctrl Pts',(1.19904150530312,-5.13642988889554,19.9999056069319));
#43272=CARTESIAN_POINT('Ctrl Pts',(1.16979164483845,-5.13607337989701,20.5394453457191));
#43273=CARTESIAN_POINT('Ctrl Pts',(1.14054178437377,-5.05144972646588,21.0790942532312));
#43274=CARTESIAN_POINT('Ctrl Pts',(1.1112919239091,-4.88433464596569,21.591857523604));
#43275=CARTESIAN_POINT('Ctrl Pts',(1.06498809374622,-4.61978404017791,22.4035845885512));
#43276=CARTESIAN_POINT('Ctrl Pts',(1.01868426358334,-4.14850745767332,23.147935444906));
#43277=CARTESIAN_POINT('Ctrl Pts',(0.972380433420454,-3.5279135019224,23.7342406241061));
#43278=CARTESIAN_POINT('Ctrl Pts',(0.926076603257575,-2.90731954617152,
24.3205458033061));
#43279=CARTESIAN_POINT('Ctrl Pts',(0.879772773094695,-2.13740821717434,
24.7488053053514));
#43280=CARTESIAN_POINT('Ctrl Pts',(0.833468942931815,-1.31196997330618,
24.9668393096929));
#43281=CARTESIAN_POINT('Ctrl Pts',(0.787165112768935,-0.486531729438019,
25.1848733140344));
#43282=CARTESIAN_POINT('Ctrl Pts',(0.740861282606054,0.394433429301118,
25.1926818206721));
#43283=CARTESIAN_POINT('Ctrl Pts',(0.694557452443174,1.22361266905245,24.9893341571924));
#43284=CARTESIAN_POINT('Ctrl Pts',(0.648253622280297,2.05279190880373,24.7859864937127));
#43285=CARTESIAN_POINT('Ctrl Pts',(0.60194979211742,2.83018522956722,24.3714826601157));
#43286=CARTESIAN_POINT('Ctrl Pts',(0.555645961954543,3.4610850284195,23.7962758976919));
#43287=CARTESIAN_POINT('Ctrl Pts',(0.509342131791666,4.09198482727179,23.2210691352681));
#43288=CARTESIAN_POINT('Ctrl Pts',(0.463038301628789,4.57639110421287,22.4851594440176));
#43289=CARTESIAN_POINT('Ctrl Pts',(0.416734471465911,4.85530994747718,21.6782733986309));
#43290=CARTESIAN_POINT('Ctrl Pts',(0.370430641303029,5.13422879074152,20.8713873532441));
#43291=CARTESIAN_POINT('Ctrl Pts',(0.324126811140146,5.20766020032903,19.993524953721));
#43292=CARTESIAN_POINT('Ctrl Pts',(0.277822980977266,5.06662947414752,19.1514626743736));
#43293=CARTESIAN_POINT('Ctrl Pts',(0.23151915081439,4.92559874796603,18.3094003950264));
#43294=CARTESIAN_POINT('Ctrl Pts',(0.185215320651517,4.57010588601557,17.5031382358548));
#43295=CARTESIAN_POINT('Ctrl Pts',(0.138911490488641,4.04350918221108,16.8312698444277));
#43296=CARTESIAN_POINT('Ctrl Pts',(0.0926076603257671,3.51691247840663,
16.1594014530006));
#43297=CARTESIAN_POINT('Ctrl Pts',(0.0463038301628913,2.81921193274818,
15.621926829318));
#43298=CARTESIAN_POINT('Ctrl Pts',(1.67921232474555E-14,2.03511426366992,
15.2835913560944));
#43299=CARTESIAN_POINT('',(8.67361737988404E-17,-4.95671627827806,18.6504206457069));
#43300=CARTESIAN_POINT('Origin',(0.,0.,20.));
#43301=CARTESIAN_POINT('Ctrl Pts',(8.67361737988404E-17,-4.95671627827806,
18.6504206457069));
#43302=CARTESIAN_POINT('Ctrl Pts',(0.0435916381931696,-4.74515587227111,
17.8749982094656));
#43303=CARTESIAN_POINT('Ctrl Pts',(0.087183276386337,-4.34884798055575,
17.1496924532122));
#43304=CARTESIAN_POINT('Ctrl Pts',(0.130774914579507,-3.80964413227746,
16.5536547957343));
#43305=CARTESIAN_POINT('Ctrl Pts',(0.177078744742386,-3.23689200712882,
15.9205327657653));
#43306=CARTESIAN_POINT('Ctrl Pts',(0.223382574905267,-2.50290931084975,
15.4332648935754));
#43307=CARTESIAN_POINT('Ctrl Pts',(0.269686405068148,-1.69709307475199,
15.1512235477709));
#43308=CARTESIAN_POINT('Ctrl Pts',(0.315990235231029,-0.891276838654234,
14.8691822019664));
#43309=CARTESIAN_POINT('Ctrl Pts',(0.362294065393908,-0.0136270627378211,
14.7923673825474));
#43310=CARTESIAN_POINT('Ctrl Pts',(0.408597895556788,0.828935910813523,
14.9301289758831));
#43311=CARTESIAN_POINT('Ctrl Pts',(0.454901725719665,1.67149888436482,15.0678905692187));
#43312=CARTESIAN_POINT('Ctrl Pts',(0.501205555882542,2.47897505555102,15.4202285753089));
#43313=CARTESIAN_POINT('Ctrl Pts',(0.54750938604542,3.15300369865065,15.944225949857));
#43314=CARTESIAN_POINT('Ctrl Pts',(0.593813216208297,3.82703234175028,16.4682233244052));
#43315=CARTESIAN_POINT('Ctrl Pts',(0.640117046371173,4.36761345676332,17.1638800674114));
#43316=CARTESIAN_POINT('Ctrl Pts',(0.686420876534051,4.70889301949145,17.9464512664084));
#43317=CARTESIAN_POINT('Ctrl Pts',(0.732724706696928,5.05017258221958,18.7290224654053));
#43318=CARTESIAN_POINT('Ctrl Pts',(0.779028536859813,5.19215059266281,19.5985081203932));
#43319=CARTESIAN_POINT('Ctrl Pts',(0.825332367022691,5.11753265898529,20.448990868539));
#43320=CARTESIAN_POINT('Ctrl Pts',(0.871636197185571,5.04291472530777,21.2994736166849));
#43321=CARTESIAN_POINT('Ctrl Pts',(0.917940027348451,4.75170084750951,22.1309534579889));
#43322=CARTESIAN_POINT('Ctrl Pts',(0.964243857511331,4.27936539996342,22.8421413166637));
#43323=CARTESIAN_POINT('Ctrl Pts',(1.01054768767421,3.80702995241733,23.5533291753386));
#43324=CARTESIAN_POINT('Ctrl Pts',(1.05685151783709,3.15357293512343,24.1442250513843));
#43325=CARTESIAN_POINT('Ctrl Pts',(1.10315534799997,2.3985969297664,24.5428478929248));
#43326=CARTESIAN_POINT('Ctrl Pts',(1.14945917816285,1.64362092440936,24.9414707344653));
#43327=CARTESIAN_POINT('Ctrl Pts',(1.19576300832573,0.787125930989224,25.1478205415004));
#43328=CARTESIAN_POINT('Ctrl Pts',(1.24206683848861,-0.0665523229436308,
25.1367602221083));
#43329=CARTESIAN_POINT('Ctrl Pts',(1.28837066865149,-0.920230576876437,
25.1256999027162));
#43330=CARTESIAN_POINT('Ctrl Pts',(1.33467449881437,-1.77109209132193,24.8972294568967));
#43331=CARTESIAN_POINT('Ctrl Pts',(1.38097832897724,-2.51548720074908,24.4791805886385));
#43332=CARTESIAN_POINT('Ctrl Pts',(1.42728215914012,-3.25988231017623,24.0611317203803));
#43333=CARTESIAN_POINT('Ctrl Pts',(1.473585989303,-3.89781101458502,23.4535044296833));
#43334=CARTESIAN_POINT('Ctrl Pts',(1.51988981946587,-4.35156263339055,22.7303181625132));
#43335=CARTESIAN_POINT('Ctrl Pts',(1.56619364962876,-4.80531425219613,22.007131895343));
#43336=CARTESIAN_POINT('Ctrl Pts',(1.61249747979164,-5.07488878539839,21.1683866516996));
#43337=CARTESIAN_POINT('Ctrl Pts',(1.65880130995452,-5.12744739087817,20.316256078288));
#43338=CARTESIAN_POINT('Ctrl Pts',(1.66452037153531,-5.13393898995932,20.2110080414178));
#43339=CARTESIAN_POINT('Ctrl Pts',(1.6702394331161,-5.13711998437662,20.1055558096961));
#43340=CARTESIAN_POINT('Ctrl Pts',(1.67595849469688,-5.1370281214151,20.0000980417081));
#43341=CARTESIAN_POINT('Origin',(25.,0.,20.));
#43342=CARTESIAN_POINT('',(3.42595849469688,-5.13662475218558,19.9998702837641));
#43343=CARTESIAN_POINT('',(2.94904150530311,-5.13675306620054,20.0001330755183));
#43344=CARTESIAN_POINT('',(25.,-5.13675,20.));
#43345=CARTESIAN_POINT('Ctrl Pts',(2.94904150530311,-5.13675306620054,20.0001330755183));
#43346=CARTESIAN_POINT('Ctrl Pts',(2.93840810362253,-5.1369545100676,20.1962400809989));
#43347=CARTESIAN_POINT('Ctrl Pts',(2.92777470194195,-5.12593941290559,20.3923245889008));
#43348=CARTESIAN_POINT('Ctrl Pts',(2.91714130026136,-5.10353305157791,20.5870986720596));
#43349=CARTESIAN_POINT('Ctrl Pts',(2.87083747009849,-5.00596311294013,21.4352549194799));
#43350=CARTESIAN_POINT('Ctrl Pts',(2.82453363993561,-4.69238941147243,22.2585625924748));
#43351=CARTESIAN_POINT('Ctrl Pts',(2.77822980977273,-4.2010106299116,22.956728622548));
#43352=CARTESIAN_POINT('Ctrl Pts',(2.73192597960986,-3.70963184835079,23.6548946526213));
#43353=CARTESIAN_POINT('Ctrl Pts',(2.68562214944698,-3.0404479866969,24.2279190397728));
#43354=CARTESIAN_POINT('Ctrl Pts',(2.6393183192841,-2.27497717516906,24.6059975367511));
#43355=CARTESIAN_POINT('Ctrl Pts',(2.59301448912122,-1.50950636364119,24.9840760337294));
#43356=CARTESIAN_POINT('Ctrl Pts',(2.54671065895834,-0.647748602239379,
25.1672086405343));
#43357=CARTESIAN_POINT('Ctrl Pts',(2.50040682879546,0.205319157132801,25.1330866455296));
#43358=CARTESIAN_POINT('Ctrl Pts',(2.45410299863258,1.05838691650498,25.0989646505249));
#43359=CARTESIAN_POINT('Ctrl Pts',(2.4077991684697,1.9027646738475,24.8475880537104));
#43360=CARTESIAN_POINT('Ctrl Pts',(2.36149533830682,2.6355926631063,24.4095788641542));
#43361=CARTESIAN_POINT('Ctrl Pts',(2.31519150814394,3.36842065236505,23.971569674598));
#43362=CARTESIAN_POINT('Ctrl Pts',(2.26888767798107,3.98969887354006,23.3469278923001));
#43363=CARTESIAN_POINT('Ctrl Pts',(2.22258384781819,4.42374492670835,22.6117456427229));
#43364=CARTESIAN_POINT('Ctrl Pts',(2.17628001765531,4.85779097987664,21.8765633931457));
#43365=CARTESIAN_POINT('Ctrl Pts',(2.12997618749244,5.10460486503819,21.0308406762892));
#43366=CARTESIAN_POINT('Ctrl Pts',(2.08367235732956,5.13412040058503,20.1776011220843));
#43367=CARTESIAN_POINT('Ctrl Pts',(2.03736852716668,5.16363593613188,19.3243615678793));
#43368=CARTESIAN_POINT('Ctrl Pts',(1.99106469700379,4.97585312206397,18.4636051763258));
#43369=CARTESIAN_POINT('Ctrl Pts',(1.94476086684092,4.593647133555,17.7001868684259));
#43370=CARTESIAN_POINT('Ctrl Pts',(1.89845703667804,4.21144114504601,16.936768560526));
#43371=CARTESIAN_POINT('Ctrl Pts',(1.85215320651516,3.63481198209594,16.2706883362796));
#43372=CARTESIAN_POINT('Ctrl Pts',(1.80584937635228,2.93400303467477,15.7830863406323));
#43373=CARTESIAN_POINT('Ctrl Pts',(1.75954554618939,2.23319408725357,15.2954843449849));
#43374=CARTESIAN_POINT('Ctrl Pts',(1.71324171602651,1.40820535536131,14.9863605779366));
#43375=CARTESIAN_POINT('Ctrl Pts',(1.66693788586363,0.559534654553702,14.8933714642486));
#43376=CARTESIAN_POINT('Ctrl Pts',(1.62063405570075,-0.289136046253805,
14.8003823505606));
#43377=CARTESIAN_POINT('Ctrl Pts',(1.57433022553787,-1.16148871597661,14.9235278902329));
#43378=CARTESIAN_POINT('Ctrl Pts',(1.528026395375,-1.95125569367861,15.2478071862158));
#43379=CARTESIAN_POINT('Ctrl Pts',(1.48172256521212,-2.74102267138062,15.5720864821987));
#43380=CARTESIAN_POINT('Ctrl Pts',(1.43541873504924,-3.4482039570618,16.0974995344921));
#43381=CARTESIAN_POINT('Ctrl Pts',(1.38911490488637,-3.98665281109446,16.7600412814375));
#43382=CARTESIAN_POINT('Ctrl Pts',(1.34281107472349,-4.52510166512713,17.422583028383));
#43383=CARTESIAN_POINT('Ctrl Pts',(1.29650724456061,-4.89481808751126,18.2222534699804));
#43384=CARTESIAN_POINT('Ctrl Pts',(1.25020341439773,-5.05076398416784,19.0616403275488));
#43385=CARTESIAN_POINT('Ctrl Pts',(1.23314944469953,-5.10819976403283,19.3707913844634));
#43386=CARTESIAN_POINT('Ctrl Pts',(1.21609547500132,-5.13663774949937,19.6853299402422));
#43387=CARTESIAN_POINT('Ctrl Pts',(1.19904150530312,-5.13642988889554,19.9999056069319));
#43388=CARTESIAN_POINT('Ctrl Pts',(1.67595849469688,-5.1370281214151,20.0000980417081));
#43389=CARTESIAN_POINT('Ctrl Pts',(1.71654326327897,-5.13637622477403,19.25172716853));
#43390=CARTESIAN_POINT('Ctrl Pts',(1.75712803186106,-4.9709066914377,18.5030774948426));
#43391=CARTESIAN_POINT('Ctrl Pts',(1.79771280044315,-4.65410916960248,17.8251431180106));
#43392=CARTESIAN_POINT('Ctrl Pts',(1.84401663060603,-4.29266966508966,17.0516766343244));
#43393=CARTESIAN_POINT('Ctrl Pts',(1.89032046076891,-3.73424797830663,16.3702595701316));
#43394=CARTESIAN_POINT('Ctrl Pts',(1.93662429093179,-3.04686949311008,15.8639002752298));
#43395=CARTESIAN_POINT('Ctrl Pts',(1.98292812109466,-2.35949100791349,15.3575409803279));
#43396=CARTESIAN_POINT('Ctrl Pts',(2.02923195125755,-1.54315572430333,15.026239454717));
#43397=CARTESIAN_POINT('Ctrl Pts',(2.07553578142043,-0.697307354947416,
14.9103539333822));
#43398=CARTESIAN_POINT('Ctrl Pts',(2.12183961158331,0.148541014408493,14.7944684120474));
#43399=CARTESIAN_POINT('Ctrl Pts',(2.16814344174618,1.02390246951018,14.8939988949887));
#43400=CARTESIAN_POINT('Ctrl Pts',(2.21444727190906,1.82214289574261,15.1968208546759));
#43401=CARTESIAN_POINT('Ctrl Pts',(2.26075110207194,2.62038332197499,15.4996428143631));
#43402=CARTESIAN_POINT('Ctrl Pts',(2.30705493223482,3.34150271933815,16.0057562507961));
#43403=CARTESIAN_POINT('Ctrl Pts',(2.3533587623977,3.89765631317662,16.6535078218819));
#43404=CARTESIAN_POINT('Ctrl Pts',(2.39966259256058,4.45380990701512,17.3012593929677));
#43405=CARTESIAN_POINT('Ctrl Pts',(2.44596642272346,4.84499769732893,18.0906490987062));
#43406=CARTESIAN_POINT('Ctrl Pts',(2.49227025288633,5.02356626779578,18.9255156648107));
#43407=CARTESIAN_POINT('Ctrl Pts',(2.53857408304922,5.20213483826264,19.7603822309153));
#43408=CARTESIAN_POINT('Ctrl Pts',(2.58487791321209,5.16808418888255,20.6407256573858));
#43409=CARTESIAN_POINT('Ctrl Pts',(2.63118174337498,4.92556227560906,21.459304938352));
#43410=CARTESIAN_POINT('Ctrl Pts',(2.67748557353785,4.68304036233561,22.2778842193182));
#43411=CARTESIAN_POINT('Ctrl Pts',(2.72378940370073,4.23204718516878,23.0346993547799));
#43412=CARTESIAN_POINT('Ctrl Pts',(2.77009323386361,3.62752148790459,23.6375572144555));
#43413=CARTESIAN_POINT('Ctrl Pts',(2.81639706402649,3.0229957906404,24.240415074131));
#43414=CARTESIAN_POINT('Ctrl Pts',(2.86270089418936,2.26493757327881,24.6893156580203));
#43415=CARTESIAN_POINT('Ctrl Pts',(2.90900472435224,1.44569139494332,24.9295751362994));
#43416=CARTESIAN_POINT('Ctrl Pts',(2.95530855451512,0.626445216607834,25.1698346145785));
#43417=CARTESIAN_POINT('Ctrl Pts',(3.001612384678,-0.253988922701738,25.2014529872475));
#43418=CARTESIAN_POINT('Ctrl Pts',(3.04791621484087,-1.08835896685382,25.0205785914601));
#43419=CARTESIAN_POINT('Ctrl Pts',(3.09422004500375,-1.92272901100601,24.8397041956727));
#43420=CARTESIAN_POINT('Ctrl Pts',(3.14052387516663,-2.71103496000072,24.4463370314289));
#43421=CARTESIAN_POINT('Ctrl Pts',(3.18682770532951,-3.35724755952852,23.8883960006432));
#43422=CARTESIAN_POINT('Ctrl Pts',(3.23313153549239,-4.00346015905632,23.3304549698574));
#43423=CARTESIAN_POINT('Ctrl Pts',(3.27943536565528,-4.50757940911709,22.6079400725296));
#43424=CARTESIAN_POINT('Ctrl Pts',(3.32573919581816,-4.80819489445646,21.8088660787087));
#43425=CARTESIAN_POINT('Ctrl Pts',(3.35914562877773,-5.02507740767993,21.2323649186445));
#43426=CARTESIAN_POINT('Ctrl Pts',(3.3925520617373,-5.13603483479161,20.6160142309818));
#43427=CARTESIAN_POINT('Ctrl Pts',(3.42595849469688,-5.13662475218558,19.9998702837641));
#43428=CARTESIAN_POINT('Origin',(25.,0.,20.));
#43429=CARTESIAN_POINT('',(5.17595849469686,-5.13652742584517,20.0001179802973));
#43430=CARTESIAN_POINT('',(4.6990415053031,-5.13690701511421,19.999878736315));
#43431=CARTESIAN_POINT('',(25.,-5.13675,20.));
#43432=CARTESIAN_POINT('Ctrl Pts',(4.6990415053031,-5.13690701511421,19.999878736315));
#43433=CARTESIAN_POINT('Ctrl Pts',(4.66072073224373,-5.13619931580811,20.7065503462862));
#43434=CARTESIAN_POINT('Ctrl Pts',(4.62239995918437,-4.98918393518755,21.4135072640234));
#43435=CARTESIAN_POINT('Ctrl Pts',(4.584079186125,-4.70575595787938,22.0607268921647));
#43436=CARTESIAN_POINT('Ctrl Pts',(4.53777535596212,-4.36328371953613,22.8427765573191));
#43437=CARTESIAN_POINT('Ctrl Pts',(4.49147152579924,-3.821643378755,23.5376072786038));
#43438=CARTESIAN_POINT('Ctrl Pts',(4.44516769563637,-3.14681606646729,24.0605766958687));
#43439=CARTESIAN_POINT('Ctrl Pts',(4.39886386547349,-2.47198875417958,24.5835461131336));
#43440=CARTESIAN_POINT('Ctrl Pts',(4.35256003531062,-1.66397447038526,24.9346542263786));
#43441=CARTESIAN_POINT('Ctrl Pts',(4.30625620514774,-0.821203284337316,
25.0711300146023));
#43442=CARTESIAN_POINT('Ctrl Pts',(4.25995237498486,0.0215679017106736,
25.2076058028261));
#43443=CARTESIAN_POINT('Ctrl Pts',(4.21364854482198,0.899095990012317,25.1294492660285));
#43444=CARTESIAN_POINT('Ctrl Pts',(4.1673447146591,1.70448293156581,24.8461812177436));
#43445=CARTESIAN_POINT('Ctrl Pts',(4.12104088449621,2.50986987311931,24.5629131694588));
#43446=CARTESIAN_POINT('Ctrl Pts',(4.07473705433334,3.2431156679247,24.0745336096866));
#43447=CARTESIAN_POINT('Ctrl Pts',(4.02843322417046,3.81489833763396,23.4405355880622));
#43448=CARTESIAN_POINT('Ctrl Pts',(3.98212939400758,4.38668100734326,22.8065375664377));
#43449=CARTESIAN_POINT('Ctrl Pts',(3.93582556384469,4.79700055195643,22.026921082961));
#43450=CARTESIAN_POINT('Ctrl Pts',(3.88952173368181,4.99587297737494,21.1966568652486));
#43451=CARTESIAN_POINT('Ctrl Pts',(3.84321790351893,5.19474540279343,20.3663926475364));
#43452=CARTESIAN_POINT('Ctrl Pts',(3.79691407335605,5.18217070901731,19.4854806955885));
#43453=CARTESIAN_POINT('Ctrl Pts',(3.75061024319318,4.95968071052699,18.6612312713407));
#43454=CARTESIAN_POINT('Ctrl Pts',(3.7043064130303,4.73719071203664,17.8369818470928));
#43455=CARTESIAN_POINT('Ctrl Pts',(3.65800258286743,4.30478540883215,17.069394950545));
#43456=CARTESIAN_POINT('Ctrl Pts',(3.61169875270455,3.71513922114496,16.4519758982357));
#43457=CARTESIAN_POINT('Ctrl Pts',(3.56539492254167,3.1254930334578,15.8345568459265));
#43458=CARTESIAN_POINT('Ctrl Pts',(3.51909109237879,2.37860596128802,15.3673056378559));
#43459=CARTESIAN_POINT('Ctrl Pts',(3.47278726221591,1.56546172573618,15.1071415262117));
#43460=CARTESIAN_POINT('Ctrl Pts',(3.42648343205303,0.752317490184298,14.8469774145675));
#43461=CARTESIAN_POINT('Ctrl Pts',(3.38017960189015,-0.12708390874967,14.7939003993497));
#43462=CARTESIAN_POINT('Ctrl Pts',(3.33387577172727,-0.965616220544838,
14.9543761759623));
#43463=CARTESIAN_POINT('Ctrl Pts',(3.28757194156439,-1.80414853234001,15.1148519525748));
#43464=CARTESIAN_POINT('Ctrl Pts',(3.24126811140151,-2.6018117569964,15.4888805210176));
#43465=CARTESIAN_POINT('Ctrl Pts',(3.19496428123863,-3.2614367626877,16.0308987538203));
#43466=CARTESIAN_POINT('Ctrl Pts',(3.14866045107576,-3.92106176837896,16.572916986623));
#43467=CARTESIAN_POINT('Ctrl Pts',(3.10235662091288,-4.44264855510516,17.2829248837855));
#43468=CARTESIAN_POINT('Ctrl Pts',(3.05605279075,-4.76265886056433,18.0744312432895));
#43469=CARTESIAN_POINT('Ctrl Pts',(3.02038236226771,-5.00918068552627,18.6841728324984));
#43470=CARTESIAN_POINT('Ctrl Pts',(2.98471193378541,-5.13607730981806,19.3422795377697));
#43471=CARTESIAN_POINT('Ctrl Pts',(2.94904150530311,-5.13675306620054,20.0001330755183));
#43472=CARTESIAN_POINT('Ctrl Pts',(3.42595849469688,-5.13662475218558,19.9998702837641));
#43473=CARTESIAN_POINT('Ctrl Pts',(3.43885589190018,-5.13685250469529,19.7619923507535));
#43474=CARTESIAN_POINT('Ctrl Pts',(3.45175328910349,-5.12062952689274,19.5241452332548));
#43475=CARTESIAN_POINT('Ctrl Pts',(3.46465068630679,-5.08770017461725,19.2886340133428));
#43476=CARTESIAN_POINT('Ctrl Pts',(3.51095451646967,-4.9694782488207,18.4431090321117));
#43477=CARTESIAN_POINT('Ctrl Pts',(3.55725834663255,-4.63592267660959,17.6276921599634));
#43478=CARTESIAN_POINT('Ctrl Pts',(3.60356217679543,-4.12766627689558,16.9417152290282));
#43479=CARTESIAN_POINT('Ctrl Pts',(3.6498660069583,-3.61940987718164,16.2557382980931));
#43480=CARTESIAN_POINT('Ctrl Pts',(3.69616983712118,-2.93645264996485,15.6992013083712));
#43481=CARTESIAN_POINT('Ctrl Pts',(3.74247366728406,-2.16199055912924,15.3399000594395));
#43482=CARTESIAN_POINT('Ctrl Pts',(3.78877749744694,-1.3875284682935,14.9805988105078));
#43483=CARTESIAN_POINT('Ctrl Pts',(3.83508132760981,-0.521561513839056,
14.8185333023666));
#43484=CARTESIAN_POINT('Ctrl Pts',(3.88138515777269,0.330420600639911,14.8734459077808));
#43485=CARTESIAN_POINT('Ctrl Pts',(3.92768898793557,1.18240271511878,14.9283585131949));
#43486=CARTESIAN_POINT('Ctrl Pts',(3.97399281809846,2.02039998962215,15.2002492321646));
#43487=CARTESIAN_POINT('Ctrl Pts',(4.02029664826134,2.74232990974664,15.6559970879515));
#43488=CARTESIAN_POINT('Ctrl Pts',(4.06660047842422,3.46425982987117,16.1117449437385));
#43489=CARTESIAN_POINT('Ctrl Pts',(4.11290430858709,4.07012239561694,16.7513499363429));
#43490=CARTESIAN_POINT('Ctrl Pts',(4.15920813874997,4.48611310191496,17.4968971514132));
#43491=CARTESIAN_POINT('Ctrl Pts',(4.20551196891285,4.90210380821297,18.2424443664834));
#43492=CARTESIAN_POINT('Ctrl Pts',(4.25181579907574,5.12822265506323,19.0939338040197));
#43493=CARTESIAN_POINT('Ctrl Pts',(4.29811962923862,5.13692446882051,19.9476393715678));
#43494=CARTESIAN_POINT('Ctrl Pts',(4.34442345940149,5.14562628257779,20.8013449391159));
#43495=CARTESIAN_POINT('Ctrl Pts',(4.39072728956437,4.93691106324213,21.657266636676));
#43496=CARTESIAN_POINT('Ctrl Pts',(4.43703111972725,4.53620392260352,22.4111384461148));
#43497=CARTESIAN_POINT('Ctrl Pts',(4.48333494989012,4.13549678196491,23.1650102555536));
#43498=CARTESIAN_POINT('Ctrl Pts',(4.529638780053,3.54279772002336,23.8168321768712));
#43499=CARTESIAN_POINT('Ctrl Pts',(4.57594261021588,2.83030770015685,24.2872010631891));
#43500=CARTESIAN_POINT('Ctrl Pts',(4.62224644037876,2.1178176802903,24.757569949507));
#43501=CARTESIAN_POINT('Ctrl Pts',(4.66855027054164,1.28553670249876,25.0464858008252));
#43502=CARTESIAN_POINT('Ctrl Pts',(4.71485410070452,0.434850937701575,25.1187536857869));
#43503=CARTESIAN_POINT('Ctrl Pts',(4.7611579308674,-0.415834827095611,25.1910215707485));
#43504=CARTESIAN_POINT('Ctrl Pts',(4.80746176103028,-1.28492537889845,25.0466414893536));
#43505=CARTESIAN_POINT('Ctrl Pts',(4.85376559119316,-2.06655050610693,24.7032014245071));
#43506=CARTESIAN_POINT('Ctrl Pts',(4.90006942135603,-2.84817563331536,24.3597613596607));
#43507=CARTESIAN_POINT('Ctrl Pts',(4.94637325151891,-3.54233533592946,23.8172613113628));
#43508=CARTESIAN_POINT('Ctrl Pts',(4.99267708168179,-4.06446899544116,23.1417871377409));
#43509=CARTESIAN_POINT('Ctrl Pts',(5.03898091184467,-4.5866026549529,22.4663129641189));
#43510=CARTESIAN_POINT('Ctrl Pts',(5.08528474200755,-4.93671027136222,21.6578646651729));
#43511=CARTESIAN_POINT('Ctrl Pts',(5.13158857217043,-5.07214270142953,20.8149251806834));
#43512=CARTESIAN_POINT('Ctrl Pts',(5.14637854634591,-5.11540137217387,20.5456806459821));
#43513=CARTESIAN_POINT('Ctrl Pts',(5.16116852052139,-5.1367580897038,20.2729171934918));
#43514=CARTESIAN_POINT('Ctrl Pts',(5.17595849469686,-5.13652742584517,20.0001179802973));
#43515=CARTESIAN_POINT('Origin',(25.,0.,20.));
#43516=CARTESIAN_POINT('',(6.92595849469687,-5.13711149676084,19.9999295065412));
#43517=CARTESIAN_POINT('',(6.4490415053031,-5.13634995705138,20.0000574179808));
#43518=CARTESIAN_POINT('',(25.,-5.13675,20.));
#43519=CARTESIAN_POINT('Ctrl Pts',(6.4490415053031,-5.13634995705138,20.0000574179808));
#43520=CARTESIAN_POINT('Ctrl Pts',(6.42933719102783,-5.13649271790615,20.3635369867805));
#43521=CARTESIAN_POINT('Ctrl Pts',(6.40963287675255,-5.09845241040451,20.7269871071621));
#43522=CARTESIAN_POINT('Ctrl Pts',(6.38992856247728,-5.02192199172085,21.0821432290962));
#43523=CARTESIAN_POINT('Ctrl Pts',(6.3436247323144,-4.8420805895022,21.9167365329586));
#43524=CARTESIAN_POINT('Ctrl Pts',(6.29732090215152,-4.44968956026618,22.7055288187839));
#43525=CARTESIAN_POINT('Ctrl Pts',(6.25101707198864,-3.89254889586517,23.3524315880428));
#43526=CARTESIAN_POINT('Ctrl Pts',(6.20471324182576,-3.33540823146419,23.9993343573016));
#43527=CARTESIAN_POINT('Ctrl Pts',(6.15840941166288,-2.61351793189824,24.504347609994));
#43528=CARTESIAN_POINT('Ctrl Pts',(6.11210558150001,-1.81481668043628,24.8059520259381));
#43529=CARTESIAN_POINT('Ctrl Pts',(6.06580175133713,-1.01611542897428,25.1075564418822));
#43530=CARTESIAN_POINT('Ctrl Pts',(6.01949792117425,-0.140603225616253,
25.2057520210781));
#43531=CARTESIAN_POINT('Ctrl Pts',(5.97319409101137,0.70506745017449,25.0885768491704));
#43532=CARTESIAN_POINT('Ctrl Pts',(5.92689026084849,1.55073812596523,24.9714016772627));
#43533=CARTESIAN_POINT('Ctrl Pts',(5.88058643068561,2.3665672741887,24.6388557542514));
#43534=CARTESIAN_POINT('Ctrl Pts',(5.83428260052273,3.05317284038265,24.1314489063715));
#43535=CARTESIAN_POINT('Ctrl Pts',(5.78797877035985,3.73977840657657,23.6240420584916));
#43536=CARTESIAN_POINT('Ctrl Pts',(5.74167494019697,4.297160390741,22.941774285743));
#43537=CARTESIAN_POINT('Ctrl Pts',(5.6953711100341,4.65742005840793,22.1677575645694));
#43538=CARTESIAN_POINT('Ctrl Pts',(5.64906727987122,5.01767972607487,21.3937408433957));
#43539=CARTESIAN_POINT('Ctrl Pts',(5.60276344970835,5.1808170772443,20.527975173797));
#43540=CARTESIAN_POINT('Ctrl Pts',(5.55645961954547,5.12695917019303,19.6759257394025));
#43541=CARTESIAN_POINT('Ctrl Pts',(5.51015578938259,5.07310126314176,18.8238763050079));
#43542=CARTESIAN_POINT('Ctrl Pts',(5.4638519592197,4.80224809786972,17.9855431058176));
#43543=CARTESIAN_POINT('Ctrl Pts',(5.41754812905682,4.34739425918792,17.2630495776525));
#43544=CARTESIAN_POINT('Ctrl Pts',(5.37124429889395,3.89254042050617,16.5405560494875));
#43545=CARTESIAN_POINT('Ctrl Pts',(5.32494046873107,3.25368590841469,15.9339021923476));
#43546=CARTESIAN_POINT('Ctrl Pts',(5.27863663856819,2.50865421580088,15.5169889042349));
#43547=CARTESIAN_POINT('Ctrl Pts',(5.23233280840532,1.76362252318708,15.1000756161223));
#43548=CARTESIAN_POINT('Ctrl Pts',(5.18602897824244,0.912413650050945,14.8729028970369));
#43549=CARTESIAN_POINT('Ctrl Pts',(5.13972514807956,0.0587195112657737,
14.86314430043));
#43550=CARTESIAN_POINT('Ctrl Pts',(5.09342131791668,-0.794974627519446,
14.8533857038231));
#43551=CARTESIAN_POINT('Ctrl Pts',(5.0471174877538,-1.6511540319537,15.0610412296947));
#43552=CARTESIAN_POINT('Ctrl Pts',(5.00081365759092,-2.40552129076381,15.4608148551871));
#43553=CARTESIAN_POINT('Ctrl Pts',(4.95450982742804,-3.15988854957393,15.8605884806794));
#43554=CARTESIAN_POINT('Ctrl Pts',(4.90820599726516,-3.81244366275989,16.4524802057925));
#43555=CARTESIAN_POINT('Ctrl Pts',(4.86190216710228,-4.28369416803413,17.1643874146917));
#43556=CARTESIAN_POINT('Ctrl Pts',(4.8155983369394,-4.75494467330841,17.8762946235911));
#43557=CARTESIAN_POINT('Ctrl Pts',(4.76929450677652,-5.04489057067094,18.7082173162766));
#43558=CARTESIAN_POINT('Ctrl Pts',(4.72299067661363,-5.11821145139949,19.5588129671315));
#43559=CARTESIAN_POINT('Ctrl Pts',(4.71500761951012,-5.13085240951628,19.7054607418163));
#43560=CARTESIAN_POINT('Ctrl Pts',(4.70702456240661,-5.13705444439399,19.8526635481691));
#43561=CARTESIAN_POINT('Ctrl Pts',(4.6990415053031,-5.13690701511421,19.999878736315));
#43562=CARTESIAN_POINT('Ctrl Pts',(5.17595849469686,-5.13652742584517,20.0001179802973));
#43563=CARTESIAN_POINT('Ctrl Pts',(5.20747235068426,-5.13603593698008,19.4188488708258));
#43564=CARTESIAN_POINT('Ctrl Pts',(5.23898620667166,-5.03753493650671,18.8374174031187));
#43565=CARTESIAN_POINT('Ctrl Pts',(5.27050006265906,-4.84406756639821,18.2895193523615));
#43566=CARTESIAN_POINT('Ctrl Pts',(5.31680389282194,-4.55980275757426,17.4844836785621));
#43567=CARTESIAN_POINT('Ctrl Pts',(5.36310772298482,-4.07051589620105,16.7518430009963));
#43568=CARTESIAN_POINT('Ctrl Pts',(5.4094115531477,-3.43581055688794,16.1808455843009));
#43569=CARTESIAN_POINT('Ctrl Pts',(5.45571538331058,-2.80110521757488,15.6098481676055));
#43570=CARTESIAN_POINT('Ctrl Pts',(5.50201921347345,-2.02098140032195,15.2004940117805));
#43571=CARTESIAN_POINT('Ctrl Pts',(5.54832304363632,-1.19047163474926,15.0026495099269));
#43572=CARTESIAN_POINT('Ctrl Pts',(5.5946268737992,-0.35996186917647,14.8048050080732));
#43573=CARTESIAN_POINT('Ctrl Pts',(5.64093070396209,0.520933844716072,14.818470160191));
#43574=CARTESIAN_POINT('Ctrl Pts',(5.68723453412497,1.34490722307478,15.0419803151764));
#43575=CARTESIAN_POINT('Ctrl Pts',(5.73353836428785,2.16888060143339,15.2654904701619));
#43576=CARTESIAN_POINT('Ctrl Pts',(5.77984219445072,2.93593164425815,15.698845628015));
#43577=CARTESIAN_POINT('Ctrl Pts',(5.8261460246136,3.55262031121797,16.2892556598307));
#43578=CARTESIAN_POINT('Ctrl Pts',(5.87244985477648,4.16930897817779,16.8796656916465));
#43579=CARTESIAN_POINT('Ctrl Pts',(5.91875368493936,4.63563526927263,17.6271305974248));
#43580=CARTESIAN_POINT('Ctrl Pts',(5.96505751510224,4.89479260317398,18.4405962659754));
#43581=CARTESIAN_POINT('Ctrl Pts',(6.01136134526512,5.15394993707534,19.254061934526));
#43582=CARTESIAN_POINT('Ctrl Pts',(6.057665175428,5.20593831378318,20.133528365849));
#43583=CARTESIAN_POINT('Ctrl Pts',(6.10396900559087,5.04442465277859,20.9718613873471));
#43584=CARTESIAN_POINT('Ctrl Pts',(6.15027283575375,4.88291099177398,21.8101944088453));
#43585=CARTESIAN_POINT('Ctrl Pts',(6.19657666591664,4.50789529305694,22.6073940205188));
#43586=CARTESIAN_POINT('Ctrl Pts',(6.24288049607952,3.96506093368653,23.2663475666147));
#43587=CARTESIAN_POINT('Ctrl Pts',(6.2891843262424,3.42222657431609,23.9253011127106));
#43588=CARTESIAN_POINT('Ctrl Pts',(6.33548815640528,2.71157355429229,24.4460085932289));
#43589=CARTESIAN_POINT('Ctrl Pts',(6.38179198656816,1.91967166251458,24.7650388604832));
#43590=CARTESIAN_POINT('Ctrl Pts',(6.42809581673104,1.12776977073697,25.0840691277375));
#43591=CARTESIAN_POINT('Ctrl Pts',(6.47439964689391,0.254619007205502,25.2014221817279));
#43592=CARTESIAN_POINT('Ctrl Pts',(6.52070347705679,-0.593415812696665,
25.1028023974105));
#43593=CARTESIAN_POINT('Ctrl Pts',(6.56700730721967,-1.44145063259883,25.004182613093));
#43594=CARTESIAN_POINT('Ctrl Pts',(6.61331113738255,-2.26436950887167,24.6895899904676));
#43595=CARTESIAN_POINT('Ctrl Pts',(6.65961496754543,-2.96192673595563,24.1973473342824));
#43596=CARTESIAN_POINT('Ctrl Pts',(6.70591879770831,-3.65948396303959,23.7051046780972));
#43597=CARTESIAN_POINT('Ctrl Pts',(6.75222262787118,-4.23167954093465,23.0352119883522));
#43598=CARTESIAN_POINT('Ctrl Pts',(6.79852645803406,-4.60881018408253,22.2692737430451));
#43599=CARTESIAN_POINT('Ctrl Pts',(6.84100380358832,-4.95477527145751,21.566631577058));
#43600=CARTESIAN_POINT('Ctrl Pts',(6.8834811491426,-5.1365830919474,20.7831620910917));
#43601=CARTESIAN_POINT('Ctrl Pts',(6.92595849469687,-5.13711149676084,19.9999295065412));
#43602=CARTESIAN_POINT('Origin',(25.,0.,20.));
#43603=CARTESIAN_POINT('',(8.67595849469684,-5.13631265723153,19.9999878238786));
#43604=CARTESIAN_POINT('',(8.19904150530309,-5.13718402169266,20.000021201249));
#43605=CARTESIAN_POINT('',(25.,-5.13675,20.));
#43606=CARTESIAN_POINT('Ctrl Pts',(8.19904150530309,-5.13718402169266,20.000021201249));
#43607=CARTESIAN_POINT('Ctrl Pts',(8.19795364981191,-5.13718867916289,20.0200791611231));
#43608=CARTESIAN_POINT('Ctrl Pts',(8.19686579432073,-5.13707366050557,20.0401370673822));
#43609=CARTESIAN_POINT('Ctrl Pts',(8.19577793882955,-5.13683863807768,20.0601935674349));
#43610=CARTESIAN_POINT('Ctrl Pts',(8.14947410866668,-5.12683506805018,20.9138848707705));
#43611=CARTESIAN_POINT('Ctrl Pts',(8.1031702785038,-4.89941809766086,21.7650285199751));
#43612=CARTESIAN_POINT('Ctrl Pts',(8.05686644834092,-4.48229103438051,22.5099405455748));
#43613=CARTESIAN_POINT('Ctrl Pts',(8.01056261817804,-4.06516397110018,23.2548525711745));
#43614=CARTESIAN_POINT('Ctrl Pts',(7.96425878801516,-3.45832681492884,23.8935329731693));
#43615=CARTESIAN_POINT('Ctrl Pts',(7.91795495785228,-2.73570279285051,24.348179468283));
#43616=CARTESIAN_POINT('Ctrl Pts',(7.87165112768941,-2.01307877077215,24.8028259633968));
#43617=CARTESIAN_POINT('Ctrl Pts',(7.82534729752653,-1.17466788278679,25.0734385516296));
#43618=CARTESIAN_POINT('Ctrl Pts',(7.77904346736365,-0.322603028549861,
25.1270519546011));
#43619=CARTESIAN_POINT('Ctrl Pts',(7.73273963720077,0.529461825687064,25.1806653575726));
#43620=CARTESIAN_POINT('Ctrl Pts',(7.68643580703788,1.39518064617555,25.0172795752827));
#43621=CARTESIAN_POINT('Ctrl Pts',(7.640131976875,2.1690939563155,24.6567978126481));
#43622=CARTESIAN_POINT('Ctrl Pts',(7.59382814671212,2.9430072664554,24.2963160500134));
#43623=CARTESIAN_POINT('Ctrl Pts',(7.54752431654925,3.62511506624678,23.7387383070339));
#43624=CARTESIAN_POINT('Ctrl Pts',(7.50122048638637,4.13232486671005,23.051987164976));
#43625=CARTESIAN_POINT('Ctrl Pts',(7.4549166562235,4.63953466717333,22.365236022918));
#43626=CARTESIAN_POINT('Ctrl Pts',(7.40861282606061,4.97184646830851,21.5493114817816));
#43627=CARTESIAN_POINT('Ctrl Pts',(7.36230899589774,5.08877896396127,20.7036072165303));
#43628=CARTESIAN_POINT('Ctrl Pts',(7.31600516573486,5.20571145961404,19.8579029512789));
#43629=CARTESIAN_POINT('Ctrl Pts',(7.26970133557198,5.10726464978438,18.9824189619126));
#43630=CARTESIAN_POINT('Ctrl Pts',(7.22339750540911,4.80543105304975,18.183804290944));
#43631=CARTESIAN_POINT('Ctrl Pts',(7.17709367524623,4.50359745631513,17.3851896199754));
#43632=CARTESIAN_POINT('Ctrl Pts',(7.13078984508334,3.99837707267555,16.6634442674047));
#43633=CARTESIAN_POINT('Ctrl Pts',(7.08448601492046,3.35131445443296,16.1064892594579));
#43634=CARTESIAN_POINT('Ctrl Pts',(7.03818218475758,2.70425183619038,15.5495342515111));
#43635=CARTESIAN_POINT('Ctrl Pts',(6.9918783545947,1.91534698334479,15.1573695881882));
#43636=CARTESIAN_POINT('Ctrl Pts',(6.94557452443182,1.08070210702917,14.9777676860712));
#43637=CARTESIAN_POINT('Ctrl Pts',(6.89927069426894,0.24605723071356,14.7981657839541));
#43638=CARTESIAN_POINT('Ctrl Pts',(6.85296686410606,-0.63432766907208,14.8311266430428));
#43639=CARTESIAN_POINT('Ctrl Pts',(6.80666303394318,-1.45320653443837,15.0726350624828));
#43640=CARTESIAN_POINT('Ctrl Pts',(6.7603592037803,-2.27208539980461,15.3141434819228));
#43641=CARTESIAN_POINT('Ctrl Pts',(6.71405537361743,-3.0294582307515,15.764199461714));
#43642=CARTESIAN_POINT('Ctrl Pts',(6.66775154345455,-3.63306395999889,16.3679784249312));
#43643=CARTESIAN_POINT('Ctrl Pts',(6.62144771329168,-4.23666968924627,16.9717573881484));
#43644=CARTESIAN_POINT('Ctrl Pts',(6.57514388312879,-4.68650831679415,17.7292593347915));
#43645=CARTESIAN_POINT('Ctrl Pts',(6.52884005296591,-4.92778174296745,18.5482074690628));
#43646=CARTESIAN_POINT('Ctrl Pts',(6.50224053707831,-5.06638272500672,19.0186571884932));
#43647=CARTESIAN_POINT('Ctrl Pts',(6.4756410211907,-5.13615723937687,19.5093841354682));
#43648=CARTESIAN_POINT('Ctrl Pts',(6.4490415053031,-5.13634995705138,20.0000574179808));
#43649=CARTESIAN_POINT('Ctrl Pts',(6.92595849469687,-5.13711149676084,19.9999295065412));
#43650=CARTESIAN_POINT('Ctrl Pts',(6.92978497930548,-5.13715909702539,19.9293736045506));
#43651=CARTESIAN_POINT('Ctrl Pts',(6.93361146391409,-5.13573562608275,19.8588196250004));
#43652=CARTESIAN_POINT('Ctrl Pts',(6.9374379485227,-5.13282856734164,19.788326827259));
#43653=CARTESIAN_POINT('Ctrl Pts',(6.98374177868558,-5.09765059905217,18.9353019576494));
#43654=CARTESIAN_POINT('Ctrl Pts',(7.03004560884846,-4.84522895407254,18.0912360192996));
#43655=CARTESIAN_POINT('Ctrl Pts',(7.07634943901133,-4.40631294029821,17.3589507944877));
#43656=CARTESIAN_POINT('Ctrl Pts',(7.12265326917421,-3.96739692652388,16.6266655696758));
#43657=CARTESIAN_POINT('Ctrl Pts',(7.1689570993371,-3.34198654395484,16.0061610584017));
#43658=CARTESIAN_POINT('Ctrl Pts',(7.21526092949998,-2.60626755873719,15.5730254071148));
#43659=CARTESIAN_POINT('Ctrl Pts',(7.26156475966286,-1.87054857351955,15.139889755828));
#43660=CARTESIAN_POINT('Ctrl Pts',(7.30786858982574,-1.02452098565328,14.8941229645282));
#43661=CARTESIAN_POINT('Ctrl Pts',(7.35417241998862,-0.171245540144829,
14.8656636652088));
#43662=CARTESIAN_POINT('Ctrl Pts',(7.40047625015149,0.68202990536357,14.8372043658894));
#43663=CARTESIAN_POINT('Ctrl Pts',(7.44678008031437,1.54255320851417,15.0260525585502));
#43664=CARTESIAN_POINT('Ctrl Pts',(7.49308391047725,2.30549779628496,15.4092032777412));
#43665=CARTESIAN_POINT('Ctrl Pts',(7.53938774064013,3.06844238405575,15.7923539969322));
#43666=CARTESIAN_POINT('Ctrl Pts',(7.58569157080301,3.73380825644674,16.3698072426534));
#43667=CARTESIAN_POINT('Ctrl Pts',(7.63199540096588,4.22054237985248,17.0712192547673));
#43668=CARTESIAN_POINT('Ctrl Pts',(7.67829923112877,4.70727650325828,17.7726312668813));
#43669=CARTESIAN_POINT('Ctrl Pts',(7.72460306129164,5.0153788776788,18.5980020453883));
#43670=CARTESIAN_POINT('Ctrl Pts',(7.77090689145452,5.10731732248371,19.4467872007676));
#43671=CARTESIAN_POINT('Ctrl Pts',(7.8172107216174,5.19925576728861,20.2955723561469));
#43672=CARTESIAN_POINT('Ctrl Pts',(7.86351455178028,5.07503028247796,21.1677718883985));
#43673=CARTESIAN_POINT('Ctrl Pts',(7.90981838194316,4.74977367364457,21.9571368585078));
#43674=CARTESIAN_POINT('Ctrl Pts',(7.95612221210604,4.42451706481121,22.746501828617));
#43675=CARTESIAN_POINT('Ctrl Pts',(8.00242604226892,3.89822933195513,23.4530322365837));
#43676=CARTESIAN_POINT('Ctrl Pts',(8.04872987243179,3.23502139369626,23.9906604987275));
#43677=CARTESIAN_POINT('Ctrl Pts',(8.09503370259467,2.57181345543735,24.5282887608713));
#43678=CARTESIAN_POINT('Ctrl Pts',(8.14133753275755,1.7716853117756,24.8970148771921));
#43679=CARTESIAN_POINT('Ctrl Pts',(8.18764136292043,0.932106364145535,25.0519216501937));
#43680=CARTESIAN_POINT('Ctrl Pts',(8.23394519308331,0.0925274165154677,
25.2068284231954));
#43681=CARTESIAN_POINT('Ctrl Pts',(8.28024902324619,-0.786502335082951,
25.1479158528779));
#43682=CARTESIAN_POINT('Ctrl Pts',(8.32655285340907,-1.59790191317113,24.8823605059091));
#43683=CARTESIAN_POINT('Ctrl Pts',(8.37285668357194,-2.40930149125927,24.6168051589403));
#43684=CARTESIAN_POINT('Ctrl Pts',(8.41916051373481,-3.15307089583721,24.1446070353203));
#43685=CARTESIAN_POINT('Ctrl Pts',(8.46546434389769,-3.73860619146813,23.5232880068046));
#43686=CARTESIAN_POINT('Ctrl Pts',(8.51176817406057,-4.32414148709909,22.9019689782888));
#43687=CARTESIAN_POINT('Ctrl Pts',(8.55807200422345,-4.75144267378303,22.1315290448773));
#43688=CARTESIAN_POINT('Ctrl Pts',(8.60437583438634,-4.96845710066864,21.3058210721964));
#43689=CARTESIAN_POINT('Ctrl Pts',(8.6282367211565,-5.08028708642134,20.8803244259781));
#43690=CARTESIAN_POINT('Ctrl Pts',(8.65209760792667,-5.13627632047532,20.4401515877795));
#43691=CARTESIAN_POINT('Ctrl Pts',(8.67595849469684,-5.13631265723153,19.9999878238786));
#43692=CARTESIAN_POINT('Origin',(25.,0.,20.));
#43693=CARTESIAN_POINT('',(10.4259584946969,-5.13705094320386,20.000091771118));
#43694=CARTESIAN_POINT('',(9.94904150530308,-5.13641270033522,19.9999113248429));
#43695=CARTESIAN_POINT('',(25.,-5.13675,20.));
#43696=CARTESIAN_POINT('Ctrl Pts',(9.94904150530308,-5.13641270033522,19.9999113248429));
#43697=CARTESIAN_POINT('Ctrl Pts',(9.92026627843311,-5.13608567565037,20.530700733121));
#43698=CARTESIAN_POINT('Ctrl Pts',(9.89149105156315,-5.05423141803617,21.061588697543));
#43699=CARTESIAN_POINT('Ctrl Pts',(9.86271582469318,-4.89240905155667,21.5668657030692));
#43700=CARTESIAN_POINT('Ctrl Pts',(9.81641199453031,-4.63201161288895,22.3799352491347));
#43701=CARTESIAN_POINT('Ctrl Pts',(9.77010816436743,-4.16454609932103,23.1266882093746));
#43702=CARTESIAN_POINT('Ctrl Pts',(9.72380433420456,-3.54695786911788,23.7161571998384));
#43703=CARTESIAN_POINT('Ctrl Pts',(9.67750050404168,-2.92936963891474,24.3056261903022));
#43704=CARTESIAN_POINT('Ctrl Pts',(9.6311966738788,-2.16165869207638,24.73781121099));
#43705=CARTESIAN_POINT('Ctrl Pts',(9.58489284371592,-1.33734545661897,24.9600646758756));
#43706=CARTESIAN_POINT('Ctrl Pts',(9.53858901355304,-0.51303222116157,25.1823181407612));
#43707=CARTESIAN_POINT('Ctrl Pts',(9.49228518339017,0.367883302914878,25.1946400498445));
#43708=CARTESIAN_POINT('Ctrl Pts',(9.44598135322729,1.19809041853487,24.99552938218));
#43709=CARTESIAN_POINT('Ctrl Pts',(9.39967752306441,2.02829753415495,24.7964187145154));
#43710=CARTESIAN_POINT('Ctrl Pts',(9.35337369290152,2.80779624131857,24.3858754701028));
#43711=CARTESIAN_POINT('Ctrl Pts',(9.30706986273864,3.44163015959083,23.8139108935321));
#43712=CARTESIAN_POINT('Ctrl Pts',(9.26076603257576,4.07546407786306,23.2419463169615));
#43713=CARTESIAN_POINT('Ctrl Pts',(9.21446220241288,4.56363320724394,22.5085604082327));
#43714=CARTESIAN_POINT('Ctrl Pts',(9.16815837225,4.84667013214954,21.7030922139854));
#43715=CARTESIAN_POINT('Ctrl Pts',(9.12185454208712,5.12970705705514,20.8976240197382));
#43716=CARTESIAN_POINT('Ctrl Pts',(9.07555071192424,5.20761177748545,20.0200735399724));
#43717=CARTESIAN_POINT('Ctrl Pts',(9.02924688176136,5.07089415548018,19.1773415513561));
#43718=CARTESIAN_POINT('Ctrl Pts',(8.98294305159848,4.93417653347491,18.3346095627398));
#43719=CARTESIAN_POINT('Ctrl Pts',(8.93663922143561,4.58283656903409,17.526696065273));
#43720=CARTESIAN_POINT('Ctrl Pts',(8.89033539127273,4.05967352663219,16.8520188506965));
#43721=CARTESIAN_POINT('Ctrl Pts',(8.84403156110985,3.5365104842303,16.1773416361201));
#43722=CARTESIAN_POINT('Ctrl Pts',(8.79772773094698,2.84152436386732,15.6359007044339));
#43723=CARTESIAN_POINT('Ctrl Pts',(8.7514239007841,2.05937645597988,15.2936528951039));
#43724=CARTESIAN_POINT('Ctrl Pts',(8.70512007062122,1.27722854809239,14.9514050857739));
#43725=CARTESIAN_POINT('Ctrl Pts',(8.65881624045834,0.407918852680429,14.8083503988));
#43726=CARTESIAN_POINT('Ctrl Pts',(8.61251241029546,-0.442655723186566,
14.8819153611983));
#43727=CARTESIAN_POINT('Ctrl Pts',(8.56620858013258,-1.29323029905356,14.9554803235965));
#43728=CARTESIAN_POINT('Ctrl Pts',(8.5199047499697,-2.12506975537558,15.2456649353669));
#43729=CARTESIAN_POINT('Ctrl Pts',(8.47360091980682,-2.83684170615976,15.717119708257));
#43730=CARTESIAN_POINT('Ctrl Pts',(8.42729708964395,-3.54861365694389,16.1885744811471));
#43731=CARTESIAN_POINT('Ctrl Pts',(8.38099325948107,-4.14031810219019,16.8412994151569));
#43732=CARTESIAN_POINT('Ctrl Pts',(8.33468942931819,-4.5398752399805,17.5957813608949));
#43733=CARTESIAN_POINT('Ctrl Pts',(8.28947345464649,-4.93004524014409,18.3325376168839));
#43734=CARTESIAN_POINT('Ctrl Pts',(8.24425747997479,-5.13699043710604,19.1663257214849));
#43735=CARTESIAN_POINT('Ctrl Pts',(8.19904150530309,-5.13718402169266,20.000021201249));
#43736=CARTESIAN_POINT('Ctrl Pts',(8.67595849469684,-5.13631265723153,19.9999878238786));
#43737=CARTESIAN_POINT('Ctrl Pts',(8.69840143808955,-5.13634683466049,19.5859809794599));
#43738=CARTESIAN_POINT('Ctrl Pts',(8.72084438148226,-5.08688057336706,19.1719821628957));
#43739=CARTESIAN_POINT('Ctrl Pts',(8.74328732487497,-4.98782055609996,18.7702111018865));
#43740=CARTESIAN_POINT('Ctrl Pts',(8.78959115503785,-4.78344191755838,17.9412851162078));
#43741=CARTESIAN_POINT('Ctrl Pts',(8.83589498520072,-4.36795697338792,17.164409156801));
#43742=CARTESIAN_POINT('Ctrl Pts',(8.8821988153636,-3.79197895239965,16.5342201082102));
#43743=CARTESIAN_POINT('Ctrl Pts',(8.92850264552648,-3.21600093141144,15.9040310596194));
#43744=CARTESIAN_POINT('Ctrl Pts',(8.97480647568936,-2.47952983360547,15.4205289218445));
#43745=CARTESIAN_POINT('Ctrl Pts',(9.02111030585223,-1.67228053483701,15.1426125904369));
#43746=CARTESIAN_POINT('Ctrl Pts',(9.06741413601512,-0.86503123606842,14.8646962590293));
#43747=CARTESIAN_POINT('Ctrl Pts',(9.113717966178,0.0129962636626844,14.7923657339889));
#43748=CARTESIAN_POINT('Ctrl Pts',(9.16002179634088,0.854843078433148,14.9344321201832));
#43749=CARTESIAN_POINT('Ctrl Pts',(9.20632562650376,1.69668989320356,15.0764985063775));
#43750=CARTESIAN_POINT('Ctrl Pts',(9.25262945666664,2.50235602301334,15.4329618038064));
#43751=CARTESIAN_POINT('Ctrl Pts',(9.29893328682952,3.17369744424494,15.9603986377156));
#43752=CARTESIAN_POINT('Ctrl Pts',(9.3452371169924,3.84503886547653,16.4878354716248));
#43753=CARTESIAN_POINT('Ctrl Pts',(9.39154094715527,4.38205557812995,17.1862458420142));
#43754=CARTESIAN_POINT('Ctrl Pts',(9.43784477731815,4.71932968888737,17.9705513257629));
#43755=CARTESIAN_POINT('Ctrl Pts',(9.48414860748104,5.05660379964479,18.7548568095115));
#43756=CARTESIAN_POINT('Ctrl Pts',(9.53045243764392,5.19413530850622,19.6250574066194));
#43757=CARTESIAN_POINT('Ctrl Pts',(9.5767562678068,5.11517050676475,20.475147682832));
#43758=CARTESIAN_POINT('Ctrl Pts',(9.62306009796968,5.03620570502329,21.3252379590446));
#43759=CARTESIAN_POINT('Ctrl Pts',(9.66936392813255,4.74074459267895,22.1552179143621));
#43760=CARTESIAN_POINT('Ctrl Pts',(9.71566775829543,4.26477942671644,22.86398168207));
#43761=CARTESIAN_POINT('Ctrl Pts',(9.76197158845831,3.78881426075394,23.572745449778));
#43762=CARTESIAN_POINT('Ctrl Pts',(9.80827541862118,3.13234504117326,24.1602930298765));
#43763=CARTESIAN_POINT('Ctrl Pts',(9.85457924878406,2.37534103589674,24.5550509982833));
#43764=CARTESIAN_POINT('Ctrl Pts',(9.90088307894694,1.61833703062018,24.9498089666901));
#43765=CARTESIAN_POINT('Ctrl Pts',(9.94718690910982,0.76079823964778,25.1517773234051));
#43766=CARTESIAN_POINT('Ctrl Pts',(9.9934907392727,-0.092812329032254,25.1363528408158));
#43767=CARTESIAN_POINT('Ctrl Pts',(10.0397945694356,-0.946422897712288,
25.1209283582265));
#43768=CARTESIAN_POINT('Ctrl Pts',(10.0860983995985,-1.79610524409995,24.8881110363328));
#43769=CARTESIAN_POINT('Ctrl Pts',(10.1324022297613,-2.53835341059595,24.4662620385164));
#43770=CARTESIAN_POINT('Ctrl Pts',(10.1787060599242,-3.28060157709191,24.0444130407));
#43771=CARTESIAN_POINT('Ctrl Pts',(10.2250098900871,-3.91541556369621,23.4335323669608));
#43772=CARTESIAN_POINT('Ctrl Pts',(10.27131372025,-4.36546408318106,22.7080358144295));
#43773=CARTESIAN_POINT('Ctrl Pts',(10.3176175504128,-4.81551260266596,21.9825392618981));
#43774=CARTESIAN_POINT('Ctrl Pts',(10.3639213805757,-5.08079565503136,21.1424268305745));
#43775=CARTESIAN_POINT('Ctrl Pts',(10.4102252107386,-5.12899719124236,20.290038697426));
#43776=CARTESIAN_POINT('Ctrl Pts',(10.4154696387247,-5.13445655571799,20.1934961832375));
#43777=CARTESIAN_POINT('Ctrl Pts',(10.4207140667108,-5.13713117626548,20.0967961950884));
#43778=CARTESIAN_POINT('Ctrl Pts',(10.4259584946969,-5.13705094320386,20.000091771118));
#43779=CARTESIAN_POINT('Origin',(25.,0.,20.));
#43780=CARTESIAN_POINT('',(12.1759584946968,-5.13659925691256,19.9998724976161));
#43781=CARTESIAN_POINT('',(11.6990415053031,-5.13678078662753,20.0001322193276));
#43782=CARTESIAN_POINT('',(25.,-5.13675,20.));
#43783=CARTESIAN_POINT('Ctrl Pts',(11.6990415053031,-5.13678078662753,20.0001322193276));
#43784=CARTESIAN_POINT('Ctrl Pts',(11.6888827372172,-5.13697407873776,20.1874828625214));
#43785=CARTESIAN_POINT('Ctrl Pts',(11.6787239691313,-5.12692244990169,20.3748128764519));
#43786=CARTESIAN_POINT('Ctrl Pts',(11.6685652010455,-5.10646780565129,20.5610000080705));
#43787=CARTESIAN_POINT('Ctrl Pts',(11.6222613708826,-5.01323520447304,21.4096439822325));
#43788=CARTESIAN_POINT('Ctrl Pts',(11.5759575407197,-4.70387462893425,22.234543990903));
#43789=CARTESIAN_POINT('Ctrl Pts',(11.5296537105568,-4.21607153025175,22.9352129924435));
#43790=CARTESIAN_POINT('Ctrl Pts',(11.483349880394,-3.72826843156924,23.6358819939839));
#43791=CARTESIAN_POINT('Ctrl Pts',(11.4370460502311,-3.062022809743,24.2123199883943));
#43792=CARTESIAN_POINT('Ctrl Pts',(11.3907422200682,-2.29849486702586,24.5943068906489));
#43793=CARTESIAN_POINT('Ctrl Pts',(11.3444383899053,-1.53496692430872,24.9762937929036));
#43794=CARTESIAN_POINT('Ctrl Pts',(11.2981345597424,-0.674156660700671,
25.1638296030025));
#43795=CARTESIAN_POINT('Ctrl Pts',(11.2518307295796,0.179074394045612,25.134069226316));
#43796=CARTESIAN_POINT('Ctrl Pts',(11.2055268994167,1.0323054487919,25.1043088496296));
#43797=CARTESIAN_POINT('Ctrl Pts',(11.1592230692538,1.87795729467641,24.8572522861577));
#43798=CARTESIAN_POINT('Ctrl Pts',(11.1129192390909,2.61301495854358,24.4229952843787));
#43799=CARTESIAN_POINT('Ctrl Pts',(11.066615408928,3.34807262241072,23.9887382825997));
#43800=CARTESIAN_POINT('Ctrl Pts',(11.0203115787652,3.97253610426052,23.3672808425136));
#43801=CARTESIAN_POINT('Ctrl Pts',(10.9740077486023,4.41033498677829,22.6343271937266));
#43802=CARTESIAN_POINT('Ctrl Pts',(10.9277039184394,4.84813386929609,21.9013735449396));
#43803=CARTESIAN_POINT('Ctrl Pts',(10.8814000882765,5.09926815248184,21.0569236874518));
#43804=CARTESIAN_POINT('Ctrl Pts',(10.8350962581136,5.1331453512996,20.2038461715107));
#43805=CARTESIAN_POINT('Ctrl Pts',(10.7887924279508,5.16702255011737,19.3507686555696));
#43806=CARTESIAN_POINT('Ctrl Pts',(10.7424885977879,4.98364266456715,18.4890634811753));
#43807=CARTESIAN_POINT('Ctrl Pts',(10.696184767625,4.60534452602403,17.7237011936416));
#43808=CARTESIAN_POINT('Ctrl Pts',(10.6498809374621,4.22704638748092,16.9583389061079));
#43809=CARTESIAN_POINT('Ctrl Pts',(10.6035771072993,3.65382999594493,16.289319505435));
#43810=CARTESIAN_POINT('Ctrl Pts',(10.5572732771364,2.95552298967378,15.7981410879567));
#43811=CARTESIAN_POINT('Ctrl Pts',(10.5109694469735,2.25721598340259,15.3069626704783));
#43812=CARTESIAN_POINT('Ctrl Pts',(10.4646656168106,1.43381836239623,14.9936252361946));
#43813=CARTESIAN_POINT('Ctrl Pts',(10.4183617866477,0.58563415157598,14.8962986862752));
#43814=CARTESIAN_POINT('Ctrl Pts',(10.3720579564849,-0.262550059244267,
14.7989721363558));
#43815=CARTESIAN_POINT('Ctrl Pts',(10.325754126322,-1.1355208598784,14.9176564708008));
#43816=CARTESIAN_POINT('Ctrl Pts',(10.2794502961591,-1.92693535752653,15.2378938916565));
#43817=CARTESIAN_POINT('Ctrl Pts',(10.2331464659962,-2.71834985517461,15.5581313125122));
#43818=CARTESIAN_POINT('Ctrl Pts',(10.1868426358333,-3.4282080498367,16.0799218197787));
#43819=CARTESIAN_POINT('Ctrl Pts',(10.1405388056705,-3.9700369760445,16.7397023344413));
#43820=CARTESIAN_POINT('Ctrl Pts',(10.0942349755076,-4.51186590225237,17.3994828491039));
#43821=CARTESIAN_POINT('Ctrl Pts',(10.0479311453447,-4.88566556000591,18.1972533711626));
#43822=CARTESIAN_POINT('Ctrl Pts',(10.0016273151818,-5.04590070699891,19.0358316981376));
#43823=CARTESIAN_POINT('Ctrl Pts',(9.9840987118889,-5.10655871985318,19.3532807465613));
#43824=CARTESIAN_POINT('Ctrl Pts',(9.96657010859599,-5.1366119093977,19.6765777500346));
#43825=CARTESIAN_POINT('Ctrl Pts',(9.94904150530308,-5.13641270033522,19.9999113248429));
#43826=CARTESIAN_POINT('Ctrl Pts',(10.4259584946969,-5.13705094320386,20.000091771118));
#43827=CARTESIAN_POINT('Ctrl Pts',(10.4670178968737,-5.1364227867007,19.2429785365343));
#43828=CARTESIAN_POINT('Ctrl Pts',(10.5080772990505,-4.96693434567107,18.4855934058136));
#43829=CARTESIAN_POINT('Ctrl Pts',(10.5491367012273,-4.6429297443183,17.8013781536833));
#43830=CARTESIAN_POINT('Ctrl Pts',(10.5954405313901,-4.27754074112656,17.0297695780623));
#43831=CARTESIAN_POINT('Ctrl Pts',(10.641744361553,-3.71564271468642,16.3512162617936));
#43832=CARTESIAN_POINT('Ctrl Pts',(10.6880481917159,-3.02568453126784,15.8483776964874));
#43833=CARTESIAN_POINT('Ctrl Pts',(10.7343520218788,-2.3357263478493,15.3455391311813));
#43834=CARTESIAN_POINT('Ctrl Pts',(10.7806558520416,-1.51770800745234,15.0184153168377));
#43835=CARTESIAN_POINT('Ctrl Pts',(10.8269596822045,-0.671278245885745,
14.9068555733833));
#43836=CARTESIAN_POINT('Ctrl Pts',(10.8732635123674,0.175151515680903,14.7952958299288));
#43837=CARTESIAN_POINT('Ctrl Pts',(10.9195673425303,1.0499926984172,14.8993001573634));
#43838=CARTESIAN_POINT('Ctrl Pts',(10.9658711726932,1.84667456473939,15.2061990356585));
#43839=CARTESIAN_POINT('Ctrl Pts',(11.012175002856,2.64335643106154,15.5130979139536));
#43840=CARTESIAN_POINT('Ctrl Pts',(11.0584788330189,3.3618789809696,16.0228913431091));
#43841=CARTESIAN_POINT('Ctrl Pts',(11.1047826631818,3.91471378116012,16.6734776950437));
#43842=CARTESIAN_POINT('Ctrl Pts',(11.1510864933447,4.46754858135067,17.3240640469784));
#43843=CARTESIAN_POINT('Ctrl Pts',(11.1973903235076,4.85469563182366,18.1154433216923));
#43844=CARTESIAN_POINT('Ctrl Pts',(11.2436941536704,5.02899374774183,18.9512118808118));
#43845=CARTESIAN_POINT('Ctrl Pts',(11.2899979838333,5.20329186365999,19.7869804399314));
#43846=CARTESIAN_POINT('Ctrl Pts',(11.3363018139962,5.16474104502332,20.6671382834566));
#43847=CARTESIAN_POINT('Ctrl Pts',(11.3826056441591,4.91803744612548,21.484467012865));
#43848=CARTESIAN_POINT('Ctrl Pts',(11.4289094743219,4.67133384722765,22.3017957422732));
#43849=CARTESIAN_POINT('Ctrl Pts',(11.4752133044848,4.21647746806867,23.0562953575646));
#43850=CARTESIAN_POINT('Ctrl Pts',(11.5215171346477,3.60887765697164,23.6560547986576));
#43851=CARTESIAN_POINT('Ctrl Pts',(11.5678209648106,3.00127784587458,24.2558142397507));
#43852=CARTESIAN_POINT('Ctrl Pts',(11.6141247949735,2.24093460283946,24.7008335066453));
#43853=CARTESIAN_POINT('Ctrl Pts',(11.6604286251363,1.42047084254621,24.9369015808757));
#43854=CARTESIAN_POINT('Ctrl Pts',(11.7067324552992,0.600007082252954,25.1729696551061));
#43855=CARTESIAN_POINT('Ctrl Pts',(11.7530362854621,-0.280577195298433,
25.2000865366723));
#43856=CARTESIAN_POINT('Ctrl Pts',(11.799340115625,-1.1140116445696,25.0149489219273));
#43857=CARTESIAN_POINT('Ctrl Pts',(11.8456439457879,-1.94744609384073,24.8298113071824));
#43858=CARTESIAN_POINT('Ctrl Pts',(11.8919477759507,-2.73373071483164,24.4324191961262));
#43859=CARTESIAN_POINT('Ctrl Pts',(11.9382516061136,-3.37708248581986,23.8711817985914));
#43860=CARTESIAN_POINT('Ctrl Pts',(11.9845554362765,-4.02043425680805,23.3099444010566));
#43861=CARTESIAN_POINT('Ctrl Pts',(12.0308592664394,-4.52085317779356,22.5848617170433));
#43862=CARTESIAN_POINT('Ctrl Pts',(12.0771630966022,-4.81737959739892,21.7842613172799));
#43863=CARTESIAN_POINT('Ctrl Pts',(12.1100948959671,-5.02827248730623,21.2148654024344));
#43864=CARTESIAN_POINT('Ctrl Pts',(12.143026695332,-5.13603221298305,20.6072710206123));
#43865=CARTESIAN_POINT('Ctrl Pts',(12.1759584946968,-5.13659925691256,19.9998724976161));
#43866=CARTESIAN_POINT('Origin',(25.,0.,20.));
#43867=CARTESIAN_POINT('',(13.9259584946968,-5.13655067277195,20.0001216380244));
#43868=CARTESIAN_POINT('',(13.4490415053031,-5.13687989532564,19.9998753684823));
#43869=CARTESIAN_POINT('',(25.,-5.13675,20.));
#43870=CARTESIAN_POINT('Ctrl Pts',(13.4490415053031,-5.13687989532564,19.9998753684823));
#43871=CARTESIAN_POINT('Ctrl Pts',(13.4111953658384,-5.13617111687111,20.6978049124174));
#43872=CARTESIAN_POINT('Ctrl Pts',(13.3733492263738,-4.99287560925193,21.3960165694796));
#43873=CARTESIAN_POINT('Ctrl Pts',(13.3355030869091,-4.71622959740109,22.0366425419808));
#43874=CARTESIAN_POINT('Ctrl Pts',(13.2891992567462,-4.37775993763722,22.820432821471));
#43875=CARTESIAN_POINT('Ctrl Pts',(13.2428954265833,-3.83967888536099,23.5180235117641));
#43876=CARTESIAN_POINT('Ctrl Pts',(13.1965915964205,-3.16753398880461,24.0444360409056));
#43877=CARTESIAN_POINT('Ctrl Pts',(13.1502877662576,-2.49538909224818,24.570848570047));
#43878=CARTESIAN_POINT('Ctrl Pts',(13.1039839360947,-1.68918035141157,24.9260829380368));
#43879=CARTESIAN_POINT('Ctrl Pts',(13.0576801059318,-0.847117889289556,
25.0668654749119));
#43880=CARTESIAN_POINT('Ctrl Pts',(13.0113762757689,-0.00505542716753793,
25.2076480117869));
#43881=CARTESIAN_POINT('Ctrl Pts',(12.9650724456061,0.872860756239892,25.1339787175473));
#43882=CARTESIAN_POINT('Ctrl Pts',(12.9187686154432,1.67968533525682,24.854831782228));
#43883=CARTESIAN_POINT('Ctrl Pts',(12.8724647852803,2.4865099142737,24.5756848469088));
#43884=CARTESIAN_POINT('Ctrl Pts',(12.8261609551174,3.22224288890008,24.0910602705099));
#43885=CARTESIAN_POINT('Ctrl Pts',(12.7798571249545,3.79725929940857,23.4599936809571));
#43886=CARTESIAN_POINT('Ctrl Pts',(12.7335532947917,4.37227570991707,22.8289270914043));
#43887=CARTESIAN_POINT('Ctrl Pts',(12.6872494646288,4.78657555630767,22.0514184886975));
#43888=CARTESIAN_POINT('Ctrl Pts',(12.6409456344659,4.98968997510898,21.2221818242411));
#43889=CARTESIAN_POINT('Ctrl Pts',(12.594641804303,5.1928043939103,20.3929451597845));
#43890=CARTESIAN_POINT('Ctrl Pts',(12.5483379741402,5.18473338512231,19.5119804335783));
#43891=CARTESIAN_POINT('Ctrl Pts',(12.5020341439773,4.96646013675279,18.6866043363656));
#43892=CARTESIAN_POINT('Ctrl Pts',(12.4557303138144,4.74818688838326,17.8612282391528));
#43893=CARTESIAN_POINT('Ctrl Pts',(12.4094264836515,4.31971140043221,17.0914407709334));
#43894=CARTESIAN_POINT('Ctrl Pts',(12.3631226534886,3.73322937388923,16.4710153158254));
#43895=CARTESIAN_POINT('Ctrl Pts',(12.3168188233258,3.14674734734626,15.8505898607174));
#43896=CARTESIAN_POINT('Ctrl Pts',(12.2705149931629,2.40225878221136,15.3795264187206));
#43897=CARTESIAN_POINT('Ctrl Pts',(12.224211163,1.5904552200749,15.1152086378081));
#43898=CARTESIAN_POINT('Ctrl Pts',(12.1779073328371,0.778651657938445,14.8508908568955));
#43899=CARTESIAN_POINT('Ctrl Pts',(12.1316035026742,-0.100466901199574,
14.7933187370672));
#43900=CARTESIAN_POINT('Ctrl Pts',(12.0852996725114,-0.939808661571305,
14.9495055550131));
#43901=CARTESIAN_POINT('Ctrl Pts',(12.0389958423485,-1.77915042194299,15.1056923729589));
#43902=CARTESIAN_POINT('Ctrl Pts',(11.9926920121856,-2.57871538354839,15.475638128679));
#43903=CARTESIAN_POINT('Ctrl Pts',(11.9463881820227,-3.24110275023627,16.0142770515728));
#43904=CARTESIAN_POINT('Ctrl Pts',(11.9000843518599,-3.90349011692416,16.5529159744666));
#43905=CARTESIAN_POINT('Ctrl Pts',(11.853780521697,-4.42869988869453,17.2602480645341));
#43906=CARTESIAN_POINT('Ctrl Pts',(11.8074766915341,-4.75275246117088,18.0501080793945));
#43907=CARTESIAN_POINT('Ctrl Pts',(11.7713316294571,-5.00570994454042,18.6666777922856));
#43908=CARTESIAN_POINT('Ctrl Pts',(11.7351865673801,-5.13609305015553,19.3335355836762));
#43909=CARTESIAN_POINT('Ctrl Pts',(11.6990415053031,-5.13678078662753,20.0001322193276));
#43910=CARTESIAN_POINT('Ctrl Pts',(12.1759584946968,-5.13659925691256,19.9998724976161));
#43911=CARTESIAN_POINT('Ctrl Pts',(12.1893305254949,-5.13682950636858,19.7532369686496));
#43912=CARTESIAN_POINT('Ctrl Pts',(12.2027025562929,-5.11938599591789,19.5066337325767));
#43913=CARTESIAN_POINT('Ctrl Pts',(12.2160745870909,-5.08399694390373,19.2626332607487));
#43914=CARTESIAN_POINT('Ctrl Pts',(12.2623784172538,-4.96145395257798,18.4177237194945));
#43915=CARTESIAN_POINT('Ctrl Pts',(12.3086822474166,-4.62373405170133,17.6040227524996));
#43916=CARTESIAN_POINT('Ctrl Pts',(12.3549860775795,-4.1119773472077,16.9206531650645));
#43917=CARTESIAN_POINT('Ctrl Pts',(12.4012899077424,-3.60022064271406,16.2372835776294));
#43918=CARTESIAN_POINT('Ctrl Pts',(12.4475937379053,-2.91442713460346,15.6842453697541));
#43919=CARTESIAN_POINT('Ctrl Pts',(12.4938975680682,-2.13813829466724,15.3289081290715));
#43920=CARTESIAN_POINT('Ctrl Pts',(12.540201398231,-1.36184945473103,14.973570888389));
#43921=CARTESIAN_POINT('Ctrl Pts',(12.5865052283939,-0.495065282969215,
14.8159346148992));
#43922=CARTESIAN_POINT('Ctrl Pts',(12.6328090585568,0.35662496586725,14.87520212423));
#43923=CARTESIAN_POINT('Ctrl Pts',(12.6791128887197,1.20831521470367,14.9344696335608));
#43924=CARTESIAN_POINT('Ctrl Pts',(12.7254167188826,2.04491154061474,15.2106409257122));
#43925=CARTESIAN_POINT('Ctrl Pts',(12.7717205490454,2.76450208888721,15.6700735763393));
#43926=CARTESIAN_POINT('Ctrl Pts',(12.8180243792083,3.48409263715968,16.1295062269664));
#43927=CARTESIAN_POINT('Ctrl Pts',(12.8643282093712,4.08667740779355,16.7722002360692));
#43928=CARTESIAN_POINT('Ctrl Pts',(12.9106320395341,4.49885118767081,17.5198643938346));
#43929=CARTESIAN_POINT('Ctrl Pts',(12.9569358696969,4.91102496754808,18.2675285515999));
#43930=CARTESIAN_POINT('Ctrl Pts',(13.0032396998598,5.13278775666873,19.1201628580279));
#43931=CARTESIAN_POINT('Ctrl Pts',(13.0495435300227,5.13712502431383,19.973901755897));
#43932=CARTESIAN_POINT('Ctrl Pts',(13.0958473601856,5.14146229195894,20.8276406537662));
#43933=CARTESIAN_POINT('Ctrl Pts',(13.1421511903485,4.92837403812845,21.6824841430764));
#43934=CARTESIAN_POINT('Ctrl Pts',(13.1884550205113,4.52381808560127,22.4342975500467));
#43935=CARTESIAN_POINT('Ctrl Pts',(13.2347588506742,4.11926213307414,23.1861109570169));
#43936=CARTESIAN_POINT('Ctrl Pts',(13.2810626808371,3.52323848185035,23.8348942816473));
#43937=CARTESIAN_POINT('Ctrl Pts',(13.327366511,2.8083530875956,24.3016145305186));
#43938=CARTESIAN_POINT('Ctrl Pts',(13.3736703411629,2.09346769334081,24.76833477939));
#43939=CARTESIAN_POINT('Ctrl Pts',(13.4199741713257,1.25972055605504,25.0529919525024));
#43940=CARTESIAN_POINT('Ctrl Pts',(13.4662780014886,0.408676450159372,25.1209098989205));
#43941=CARTESIAN_POINT('Ctrl Pts',(13.5125818316515,-0.442367655736295,
25.1888278453385));
#43942=CARTESIAN_POINT('Ctrl Pts',(13.5588856618144,-1.31070873024186,25.0400065650622));
#43943=CARTESIAN_POINT('Ctrl Pts',(13.6051894919772,-2.09056786101249,24.6925750555829));
#43944=CARTESIAN_POINT('Ctrl Pts',(13.6514933221401,-2.87042699178307,24.3451435461035));
#43945=CARTESIAN_POINT('Ctrl Pts',(13.697797152303,-3.56180417881871,23.7991018074213));
#43946=CARTESIAN_POINT('Ctrl Pts',(13.7441009824659,-4.08047776197707,23.120967136608));
#43947=CARTESIAN_POINT('Ctrl Pts',(13.7904048126288,-4.59915134513546,22.4428324657947));
#43948=CARTESIAN_POINT('Ctrl Pts',(13.8367086427916,-4.94512132441653,21.6326048628505));
#43949=CARTESIAN_POINT('Ctrl Pts',(13.8830124729545,-5.07624259211229,20.7889840174565));
#43950=CARTESIAN_POINT('Ctrl Pts',(13.8973278135353,-5.11678018042506,20.5281693142155));
#43951=CARTESIAN_POINT('Ctrl Pts',(13.9116431541161,-5.13678241017023,20.2641628664098));
#43952=CARTESIAN_POINT('Ctrl Pts',(13.9259584946968,-5.13655067277195,20.0001216380244));
#43953=CARTESIAN_POINT('Origin',(25.,0.,20.));
#43954=CARTESIAN_POINT('',(15.6759584946968,-5.13709264059427,19.9999219868719));
#43955=CARTESIAN_POINT('',(15.1990415053031,-5.1363612583734,20.0000647015142));
#43956=CARTESIAN_POINT('',(25.,-5.13675,20.));
#43957=CARTESIAN_POINT('Ctrl Pts',(15.1990415053031,-5.1363612583734,20.0000647015142));
#43958=CARTESIAN_POINT('Ctrl Pts',(15.1798118246225,-5.13651868439003,20.3547866133449));
#43959=CARTESIAN_POINT('Ctrl Pts',(15.1605821439419,-5.10030269833592,20.7094768313789));
#43960=CARTESIAN_POINT('Ctrl Pts',(15.1413524632614,-5.02738864798306,21.0564553191401));
#43961=CARTESIAN_POINT('Ctrl Pts',(15.0950486330985,-4.85181631997047,21.8919571267025));
#43962=CARTESIAN_POINT('Ctrl Pts',(15.0487448029356,-4.46346299222078,22.6827451405394));
#43963=CARTESIAN_POINT('Ctrl Pts',(15.0024409727727,-3.90963679493877,23.3324877480449));
#43964=CARTESIAN_POINT('Ctrl Pts',(14.9561371426099,-3.35581059765675,23.9822303555503));
#43965=CARTESIAN_POINT('Ctrl Pts',(14.909833312447,-2.63651153084241,24.4909275567245));
#43966=CARTESIAN_POINT('Ctrl Pts',(14.8635294822841,-1.83936262094488,24.7966112629521));
#43967=CARTESIAN_POINT('Ctrl Pts',(14.8172256521212,-1.04221371104731,25.1022949691798));
#43968=CARTESIAN_POINT('Ctrl Pts',(14.7709218219583,-0.167214958066531,
25.204965180461));
#43969=CARTESIAN_POINT('Ctrl Pts',(14.7246179917955,0.679043705641541,25.0921148951135));
#43970=CARTESIAN_POINT('Ctrl Pts',(14.6783141616326,1.52530236934961,24.979264609766));
#43971=CARTESIAN_POINT('Ctrl Pts',(14.6320103314697,2.34282094378498,24.6508938277899));
#43972=CARTESIAN_POINT('Ctrl Pts',(14.5857065013068,3.03201157324853,24.1470037712661));
#43973=CARTESIAN_POINT('Ctrl Pts',(14.5394026711439,3.72120220271208,23.6431137147422));
#43974=CARTESIAN_POINT('Ctrl Pts',(14.4930988409811,4.2820648872038,22.9637043836706));
#43975=CARTESIAN_POINT('Ctrl Pts',(14.4467950108182,4.64627688295148,22.1915395470214));
#43976=CARTESIAN_POINT('Ctrl Pts',(14.4004911806553,5.01048887869915,21.4193747103723));
#43977=CARTESIAN_POINT('Ctrl Pts',(14.3541873504924,5.17805018570278,20.5544543681455));
#43978=CARTESIAN_POINT('Ctrl Pts',(14.3078835203295,5.12854894815326,19.7021407285239));
#43979=CARTESIAN_POINT('Ctrl Pts',(14.2615796901667,5.07904771060375,18.8498270889023));
#43980=CARTESIAN_POINT('Ctrl Pts',(14.2152758600038,4.81248392850112,18.0101201518859));
#43981=CARTESIAN_POINT('Ctrl Pts',(14.1689720298409,4.36132966584095,17.2853106982448));
#43982=CARTESIAN_POINT('Ctrl Pts',(14.122668199678,3.91017540318078,16.5605012446038));
#43983=CARTESIAN_POINT('Ctrl Pts',(14.0763643695151,3.27443065996308,15.9505892743381));
#43984=CARTESIAN_POINT('Ctrl Pts',(14.0300605393523,2.53154010561662,15.5298725797956));
#43985=CARTESIAN_POINT('Ctrl Pts',(13.9837567091894,1.78864955127012,15.1091558852532));
#43986=CARTESIAN_POINT('Ctrl Pts',(13.9374528790265,0.938613185794851,14.8776344664341));
#43987=CARTESIAN_POINT('Ctrl Pts',(13.8911490488637,0.0849800924179688,
14.863511623385));
#43988=CARTESIAN_POINT('Ctrl Pts',(13.8448452187008,-0.768653000958913,
14.849388780336));
#43989=CARTESIAN_POINT('Ctrl Pts',(13.7985413885379,-1.62588282223741,15.052664513057));
#43990=CARTESIAN_POINT('Ctrl Pts',(13.752237558375,-2.38228400126439,15.448576333));
#43991=CARTESIAN_POINT('Ctrl Pts',(13.7059337282121,-3.13868518029134,15.8444881529429));
#43992=CARTESIAN_POINT('Ctrl Pts',(13.6596298980493,-3.79425771706679,16.4330360601078));
#43993=CARTESIAN_POINT('Ctrl Pts',(13.6133260678864,-4.26914157509214,17.1425247733308));
#43994=CARTESIAN_POINT('Ctrl Pts',(13.5670222377235,-4.74402543311751,17.8520134865539));
#43995=CARTESIAN_POINT('Ctrl Pts',(13.5207184075606,-5.03822061239277,18.6824430058351));
#43996=CARTESIAN_POINT('Ctrl Pts',(13.4744145773977,-5.11588906840463,19.5326526998193));
#43997=CARTESIAN_POINT('Ctrl Pts',(13.4659568866995,-5.13007570859501,19.6879489376263));
#43998=CARTESIAN_POINT('Ctrl Pts',(13.4574991960013,-5.137038290053,19.8439051084966));
#43999=CARTESIAN_POINT('Ctrl Pts',(13.4490415053031,-5.13687989532564,19.9998753684823));
#44000=CARTESIAN_POINT('Ctrl Pts',(13.9259584946968,-5.13655067277195,20.0001216380244));
#44001=CARTESIAN_POINT('Ctrl Pts',(13.9579469842789,-5.13603284161668,19.4101056313638));
#44002=CARTESIAN_POINT('Ctrl Pts',(13.989935473861,-5.03448157070668,18.8199159562585));
#44003=CARTESIAN_POINT('Ctrl Pts',(14.0219239634432,-4.83525970650011,18.2647771888103));
#44004=CARTESIAN_POINT('Ctrl Pts',(14.068227793606,-4.54688299708175,17.4612052934018));
#44005=CARTESIAN_POINT('Ctrl Pts',(14.1145316237689,-4.05385702213458,16.7310755904285));
#44006=CARTESIAN_POINT('Ctrl Pts',(14.1608354539318,-3.41624084476046,16.1633304645348));
#44007=CARTESIAN_POINT('Ctrl Pts',(14.2071392840947,-2.77862466738633,15.595585338641));
#44008=CARTESIAN_POINT('Ctrl Pts',(14.2534431142576,-1.99641828758527,15.1902247898268));
#44009=CARTESIAN_POINT('Ctrl Pts',(14.2997469444204,-1.16490792699735,14.9966287210127));
#44010=CARTESIAN_POINT('Ctrl Pts',(14.3460507745833,-0.333397566409359,
14.8030326521985));
#44011=CARTESIAN_POINT('Ctrl Pts',(14.3923546047462,0.54741677496555,14.8212010633846));
#44012=CARTESIAN_POINT('Ctrl Pts',(14.4386584349091,1.37023672584908,15.0489207288803));
#44013=CARTESIAN_POINT('Ctrl Pts',(14.4849622650719,2.19305667673255,15.276640394376));
#44014=CARTESIAN_POINT('Ctrl Pts',(14.5312660952348,2.95788223712471,15.7139113141812));
#44015=CARTESIAN_POINT('Ctrl Pts',(14.5775699253977,3.57154446882019,16.3074663520807));
#44016=CARTESIAN_POINT('Ctrl Pts',(14.6238737555606,4.18520670051574,16.9010213899802));
#44017=CARTESIAN_POINT('Ctrl Pts',(14.6701775857235,4.64770560351457,17.650860545974));
#44018=CARTESIAN_POINT('Ctrl Pts',(14.7164814158864,4.90270083833917,18.4656404842655));
#44019=CARTESIAN_POINT('Ctrl Pts',(14.7627852460492,5.15769607316375,19.2804204225568));
#44020=CARTESIAN_POINT('Ctrl Pts',(14.8090890762121,5.20518763981414,20.1601411431458));
#44021=CARTESIAN_POINT('Ctrl Pts',(14.855392906375,5.03939024675767,20.9976374966191));
#44022=CARTESIAN_POINT('Ctrl Pts',(14.9016967365379,4.87359285370119,21.8351338500923));
#44023=CARTESIAN_POINT('Ctrl Pts',(14.9480005667007,4.49450650093785,22.6304058364498));
#44024=CARTESIAN_POINT('Ctrl Pts',(14.9943043968636,3.94831044136419,23.2865756179329));
#44025=CARTESIAN_POINT('Ctrl Pts',(15.0406082270265,3.40211438179051,23.942745399416));
#44026=CARTESIAN_POINT('Ctrl Pts',(15.0869120571894,2.68880861540652,24.4598129760247));
#44027=CARTESIAN_POINT('Ctrl Pts',(15.1332158873523,1.89528608134946,24.7747906031176));
#44028=CARTESIAN_POINT('Ctrl Pts',(15.1795197175151,1.10176354729244,25.0897682302105));
#44029=CARTESIAN_POINT('Ctrl Pts',(15.225823547678,0.228024245562298,25.2026559077876));
#44030=CARTESIAN_POINT('Ctrl Pts',(15.2721273778409,-0.619495314359142,
25.0997019706316));
#44031=CARTESIAN_POINT('Ctrl Pts',(15.3184312080038,-1.46701487428056,24.9967480334755));
#44032=CARTESIAN_POINT('Ctrl Pts',(15.3647350381666,-2.28831469239333,24.6779524815862));
#44033=CARTESIAN_POINT('Ctrl Pts',(15.4110388683295,-2.98334629233299,24.1821501089511));
#44034=CARTESIAN_POINT('Ctrl Pts',(15.4573426984924,-3.6783778922727,23.6863477363159));
#44035=CARTESIAN_POINT('Ctrl Pts',(15.5036465286553,-4.24714127403926,23.0135385429349));
#44036=CARTESIAN_POINT('Ctrl Pts',(15.5499503588182,-4.62035125273102,22.2456822872266));
#44037=CARTESIAN_POINT('Ctrl Pts',(15.5919530707777,-4.95889411582207,21.5491514598327));
#44038=CARTESIAN_POINT('Ctrl Pts',(15.6339557827373,-5.13652580276168,20.7744111288028));
#44039=CARTESIAN_POINT('Ctrl Pts',(15.6759584946968,-5.13709264059427,19.9999219868719));
#44040=CARTESIAN_POINT('Origin',(25.,0.,20.));
#44041=CARTESIAN_POINT('',(17.4259584946968,-5.13631117261779,19.999995970574));
#44042=CARTESIAN_POINT('',(16.9490415053031,-5.13718894078376,20.0000119941014));
#44043=CARTESIAN_POINT('',(25.,-5.13675,20.));
#44044=CARTESIAN_POINT('Ctrl Pts',(16.9490415053031,-5.13718894078376,20.0000119941014));
#44045=CARTESIAN_POINT('Ctrl Pts',(16.9484282834066,-5.1371904673118,20.0113185931481));
#44046=CARTESIAN_POINT('Ctrl Pts',(16.9478150615101,-5.13715392013654,20.0226251822843));
#44047=CARTESIAN_POINT('Ctrl Pts',(16.9472018396137,-5.13707923933338,20.0339315195396));
#44048=CARTESIAN_POINT('Ctrl Pts',(16.9008980094508,-5.1314401595061,20.8876628084021));
#44049=CARTESIAN_POINT('Ctrl Pts',(16.8545941792879,-4.90837749602317,21.7399579674652));
#44050=CARTESIAN_POINT('Ctrl Pts',(16.808290349125,-4.49506412670956,22.4869927535031));
#44051=CARTESIAN_POINT('Ctrl Pts',(16.7619865189621,-4.08175075739599,23.234027539541));
#44052=CARTESIAN_POINT('Ctrl Pts',(16.7156826887993,-3.47818668225178,23.8758019525536));
#44053=CARTESIAN_POINT('Ctrl Pts',(16.6693788586364,-2.7578964105667,24.3341368053848));
#44054=CARTESIAN_POINT('Ctrl Pts',(16.6230750284735,-2.03760613888161,24.792471658216));
#44055=CARTESIAN_POINT('Ctrl Pts',(16.5767711983106,-1.20058967065567,25.0673669508658));
#44056=CARTESIAN_POINT('Ctrl Pts',(16.5304673681477,-0.348810041178962,
25.1253356977257));
#44057=CARTESIAN_POINT('Ctrl Pts',(16.4841635379848,0.502969588297676,25.1833044445855));
#44058=CARTESIAN_POINT('Ctrl Pts',(16.437859707822,1.36951237902513,25.0243466456554));
#44059=CARTESIAN_POINT('Ctrl Pts',(16.3915558776591,2.14525848062353,24.667826101144));
#44060=CARTESIAN_POINT('Ctrl Pts',(16.3452520474962,2.92100458222195,24.3113055566325));
#44061=CARTESIAN_POINT('Ctrl Pts',(16.2989482173333,3.60595399469137,23.7572222665397));
#44062=CARTESIAN_POINT('Ctrl Pts',(16.2526443871705,4.11666807164104,23.0730731275288));
#44063=CARTESIAN_POINT('Ctrl Pts',(16.2063405570076,4.62738214859073,22.3889239885178));
#44064=CARTESIAN_POINT('Ctrl Pts',(16.1600367268447,4.96386089002065,21.5747090005889));
#44065=CARTESIAN_POINT('Ctrl Pts',(16.1137328966818,5.08511538461402,20.7296135856535));
#44066=CARTESIAN_POINT('Ctrl Pts',(16.067429066519,5.20636987920738,19.884518170718));
#44067=CARTESIAN_POINT('Ctrl Pts',(16.0211252363561,5.1124001269642,19.0085423287761));
#44068=CARTESIAN_POINT('Ctrl Pts',(15.9748214061932,4.81465326366721,18.2083950184634));
#44069=CARTESIAN_POINT('Ctrl Pts',(15.9285175760303,4.51690640037024,17.4082477081506));
#44070=CARTESIAN_POINT('Ctrl Pts',(15.8822137458674,4.01538242601949,16.683928929467));
#44071=CARTESIAN_POINT('Ctrl Pts',(15.8359099157046,3.37117560654253,16.1236731963029));
#44072=CARTESIAN_POINT('Ctrl Pts',(15.7896060855417,2.72696878706553,15.5634174631387));
#44073=CARTESIAN_POINT('Ctrl Pts',(15.7433022553788,1.94007912246231,15.1672247754941));
#44074=CARTESIAN_POINT('Ctrl Pts',(15.6969984252159,1.10636333919777,14.983358232753));
#44075=CARTESIAN_POINT('Ctrl Pts',(15.650694595053,0.272647555933252,14.7994916900119));
#44076=CARTESIAN_POINT('Ctrl Pts',(15.6043907648902,-0.607894345992638,
14.8279512921742));
#44077=CARTESIAN_POINT('Ctrl Pts',(15.5580869347273,-1.42799718312314,15.0652701690771));
#44078=CARTESIAN_POINT('Ctrl Pts',(15.5117831045644,-2.24810002025363,15.3025890459799));
#44079=CARTESIAN_POINT('Ctrl Pts',(15.4654792744015,-3.00776379258878,15.7487671976232));
#44080=CARTESIAN_POINT('Ctrl Pts',(15.4191754442386,-3.61444835669347,16.3494524334007));
#44081=CARTESIAN_POINT('Ctrl Pts',(15.3728716140758,-4.22113292079819,16.9501376691782));
#44082=CARTESIAN_POINT('Ctrl Pts',(15.3265677839129,-4.67483827667241,17.7053299890898));
#44083=CARTESIAN_POINT('Ctrl Pts',(15.28026395375,-4.92029529047178,18.5230339496896));
#44084=CARTESIAN_POINT('Ctrl Pts',(15.2531898042677,-5.06381559666912,19.001150753066));
#44085=CARTESIAN_POINT('Ctrl Pts',(15.2261156547854,-5.13613961270089,19.5006391403159));
#44086=CARTESIAN_POINT('Ctrl Pts',(15.1990415053031,-5.1363612583734,20.0000647015142));
#44087=CARTESIAN_POINT('Ctrl Pts',(15.6759584946968,-5.13709264059427,19.9999219868719));
#44088=CARTESIAN_POINT('Ctrl Pts',(15.6802596129002,-5.13715068533487,19.9206135519823));
#44089=CARTESIAN_POINT('Ctrl Pts',(15.6845607311035,-5.13535203559877,19.8413077510508));
#44090=CARTESIAN_POINT('Ctrl Pts',(15.6888618493068,-5.13167934602173,19.7620888329847));
#44091=CARTESIAN_POINT('Ctrl Pts',(15.7351656794697,-5.09214088500373,18.9092549524864));
#44092=CARTESIAN_POINT('Ctrl Pts',(15.7814695096325,-4.83540738735081,18.0664905095254));
#44093=CARTESIAN_POINT('Ctrl Pts',(15.8277733397954,-4.39275341894673,17.3364587418047));
#44094=CARTESIAN_POINT('Ctrl Pts',(15.8740771699583,-3.95009945054265,16.606426974084));
#44095=CARTESIAN_POINT('Ctrl Pts',(15.9203810001212,-3.32152501138741,15.9891278816036));
#44096=CARTESIAN_POINT('Ctrl Pts',(15.9666848302841,-2.58360130426497,15.5597591355449));
#44097=CARTESIAN_POINT('Ctrl Pts',(16.012988660447,-1.8456775971425,15.1303903894862));
#44098=CARTESIAN_POINT('Ctrl Pts',(16.0592924906098,-0.9984046220528,14.8889519898493));
#44099=CARTESIAN_POINT('Ctrl Pts',(16.1055963207727,-0.144994833635566,
14.8648552959049));
#44100=CARTESIAN_POINT('Ctrl Pts',(16.1519001509356,0.708414954781668,14.8407586019606));
#44101=CARTESIAN_POINT('Ctrl Pts',(16.1982039810985,1.56796155652645,15.0340036137088));
#44102=CARTESIAN_POINT('Ctrl Pts',(16.2445078112613,2.32893737764552,15.4210497573371));
#44103=CARTESIAN_POINT('Ctrl Pts',(16.2908116414242,3.08991319876458,15.8080959009655));
#44104=CARTESIAN_POINT('Ctrl Pts',(16.3371154715871,3.75231823925793,16.3889431764739));
#44105=CARTESIAN_POINT('Ctrl Pts',(16.38341930175,4.2354601458875,17.0928343723869));
#44106=CARTESIAN_POINT('Ctrl Pts',(16.4297231319129,4.71860205251706,17.7967255682998));
#44107=CARTESIAN_POINT('Ctrl Pts',(16.4760269620757,5.02248082528284,18.6236606846172));
#44108=CARTESIAN_POINT('Ctrl Pts',(16.5223307922386,5.1100787910474,19.4729047685055));
#44109=CARTESIAN_POINT('Ctrl Pts',(16.5686346224015,5.19767675681196,20.3221488523938));
#44110=CARTESIAN_POINT('Ctrl Pts',(16.6149384525644,5.06899391557534,21.193701903853));
#44111=CARTESIAN_POINT('Ctrl Pts',(16.6612422827273,4.73970605578413,21.9813937363734));
#44112=CARTESIAN_POINT('Ctrl Pts',(16.7075461128901,4.41041819599293,22.7690855688939));
#44113=CARTESIAN_POINT('Ctrl Pts',(16.753849943053,3.88052531764715,23.4729161824757));
#44114=CARTESIAN_POINT('Ctrl Pts',(16.8001537732159,3.21457750823702,24.0071468749365));
#44115=CARTESIAN_POINT('Ctrl Pts',(16.8464576033788,2.54862969882685,24.5413775673973));
#44116=CARTESIAN_POINT('Ctrl Pts',(16.8927614335417,1.74662695835231,24.9060083387372));
#44117=CARTESIAN_POINT('Ctrl Pts',(16.9390652637045,0.90626704645616,25.056620875079));
#44118=CARTESIAN_POINT('Ctrl Pts',(16.9853690938674,0.0659071345600125,
25.2072334114207));
#44119=CARTESIAN_POINT('Ctrl Pts',(17.0316729240303,-0.812809948757753,
25.1438277127643));
#44120=CARTESIAN_POINT('Ctrl Pts',(17.0779767541932,-1.62284131440529,24.8741276862671));
#44121=CARTESIAN_POINT('Ctrl Pts',(17.124280584356,-2.43287268005278,24.60442765977));
#44122=CARTESIAN_POINT('Ctrl Pts',(17.1705844145189,-3.17421832803005,24.128433305432));
#44123=CARTESIAN_POINT('Ctrl Pts',(17.2168882446818,-3.7565695782378,23.504128941354));
#44124=CARTESIAN_POINT('Ctrl Pts',(17.2631920748447,-4.33892082844559,22.879824577276));
#44125=CARTESIAN_POINT('Ctrl Pts',(17.3094959050076,-4.76227768088384,22.1072102034581));
#44126=CARTESIAN_POINT('Ctrl Pts',(17.3557997351704,-4.97506797260937,21.2804035698533));
#44127=CARTESIAN_POINT('Ctrl Pts',(17.3791859883459,-5.08254002444763,20.8628158845016));
#44128=CARTESIAN_POINT('Ctrl Pts',(17.4025722415214,-5.13629939103057,20.4314044857201));
#44129=CARTESIAN_POINT('Ctrl Pts',(17.4259584946968,-5.13631117261779,19.999995970574));
#44130=CARTESIAN_POINT('Origin',(25.,0.,20.));
#44131=CARTESIAN_POINT('',(19.1759584946968,-5.13707257898892,20.0000850551338));
#44132=CARTESIAN_POINT('',(18.6990415053031,-5.13639668367057,19.9999176386971));
#44133=CARTESIAN_POINT('',(25.,-5.13675,20.));
#44134=CARTESIAN_POINT('Ctrl Pts',(18.6990415053031,-5.13639668367057,19.9999176386971));
#44135=CARTESIAN_POINT('Ctrl Pts',(18.6707409120278,-5.13609916331192,20.5219565910637));
#44136=CARTESIAN_POINT('Ctrl Pts',(18.6424403187525,-5.05696603051791,21.0440837186712));
#44137=CARTESIAN_POINT('Ctrl Pts',(18.6141397254773,-4.90035546598673,21.54183357279));
#44138=CARTESIAN_POINT('Ctrl Pts',(18.5678358953144,-4.64411811748906,22.356223733609));
#44139=CARTESIAN_POINT('Ctrl Pts',(18.5215320651515,-4.18047636719759,23.1053567774596));
#44140=CARTESIAN_POINT('Ctrl Pts',(18.4752282349886,-3.56590977309181,23.6979753851772));
#44141=CARTESIAN_POINT('Ctrl Pts',(18.4289244048258,-2.95134317898598,24.2905939928948));
#44142=CARTESIAN_POINT('Ctrl Pts',(18.3826205746629,-2.18585174106585,24.7266981644793));
#44143=CARTESIAN_POINT('Ctrl Pts',(18.3363167445,-1.36268551289881,24.9531628937623));
#44144=CARTESIAN_POINT('Ctrl Pts',(18.2900129143371,-0.539519284731791,
25.1796276230454));
#44145=CARTESIAN_POINT('Ctrl Pts',(18.2437090841742,0.341321733682111,25.196452910027));
#44146=CARTESIAN_POINT('Ctrl Pts',(18.1974052540114,1.17253592134146,25.0015891446991));
#44147=CARTESIAN_POINT('Ctrl Pts',(18.1511014238485,2.00375010900077,24.8067253793712));
#44148=CARTESIAN_POINT('Ctrl Pts',(18.1047975936856,2.78533746590556,24.4001725617338));
#44149=CARTESIAN_POINT('Ctrl Pts',(18.0584937635227,3.4220871780759,23.8314558336038));
#44150=CARTESIAN_POINT('Ctrl Pts',(18.0121899333599,4.05883689024629,23.2627391054738));
#44151=CARTESIAN_POINT('Ctrl Pts',(17.965886103197,4.55074895768223,22.5318584668512));
#44152=CARTESIAN_POINT('Ctrl Pts',(17.9195822730341,4.83790001041956,21.7278477792881));
#44153=CARTESIAN_POINT('Ctrl Pts',(17.8732784428712,5.12505106315689,20.9238370917249));
#44154=CARTESIAN_POINT('Ctrl Pts',(17.8269746127083,5.20744110119561,20.0466963552211));
#44155=CARTESIAN_POINT('Ctrl Pts',(17.7806707825455,5.07503359756761,19.2032764326517));
#44156=CARTESIAN_POINT('Ctrl Pts',(17.7343669523826,4.94262609393962,18.3598565100823));
#44157=CARTESIAN_POINT('Ctrl Pts',(17.6880631222197,4.59542104864494,17.5501574014474));
#44158=CARTESIAN_POINT('Ctrl Pts',(17.6417592920568,4.07571402172354,16.8728144167104));
#44159=CARTESIAN_POINT('Ctrl Pts',(17.595455461894,3.5560069948021,16.1954714319734));
#44160=CARTESIAN_POINT('Ctrl Pts',(17.5491516317311,2.8637979862539,15.6504845711344));
#44161=CARTESIAN_POINT('Ctrl Pts',(17.5028478015682,2.08340998642146,15.3042426289588));
#44162=CARTESIAN_POINT('Ctrl Pts',(17.4565439714053,1.30302198658901,14.9580006867833));
#44163=CARTESIAN_POINT('Ctrl Pts',(17.4102401412424,0.434454995472302,14.8105036632712));
#44164=CARTESIAN_POINT('Ctrl Pts',(17.3639363110796,-0.416484554045956,
14.8797192386111));
#44165=CARTESIAN_POINT('Ctrl Pts',(17.3176324809167,-1.26742410356419,14.9489348139509));
#44166=CARTESIAN_POINT('Ctrl Pts',(17.2713286507538,-2.10073621148394,15.2348629881427));
#44167=CARTESIAN_POINT('Ctrl Pts',(17.2250248205909,-2.81490909746055,15.7026727804085));
#44168=CARTESIAN_POINT('Ctrl Pts',(17.178720990428,-3.52908198343714,16.1704825726743));
#44169=CARTESIAN_POINT('Ctrl Pts',(17.1324171602652,-4.12411564747056,16.8201739830141));
#44170=CARTESIAN_POINT('Ctrl Pts',(17.0861133301023,-4.52752473140143,17.5726033975148));
#44171=CARTESIAN_POINT('Ctrl Pts',(17.0404227218359,-4.92559129220556,18.3150680598363));
#44172=CARTESIAN_POINT('Ctrl Pts',(16.9947321135695,-5.13707520056159,19.1575675366546));
#44173=CARTESIAN_POINT('Ctrl Pts',(16.9490415053031,-5.13718894078376,20.0000119941014));
#44174=CARTESIAN_POINT('Ctrl Pts',(17.4259584946968,-5.13631117261779,19.999995970574));
#44175=CARTESIAN_POINT('Ctrl Pts',(17.4488760716842,-5.1363227180941,19.577233171219));
#44176=CARTESIAN_POINT('Ctrl Pts',(17.4717936486717,-5.08471936726895,19.1544731410777));
#44177=CARTESIAN_POINT('Ctrl Pts',(17.4947112256591,-4.9814682768752,18.7447277425743));
#44178=CARTESIAN_POINT('Ctrl Pts',(17.5410150558219,-4.7728545584027,17.9168574422915));
#44179=CARTESIAN_POINT('Ctrl Pts',(17.5873188859848,-4.3534033904449,17.1421157351172));
#44180=CARTESIAN_POINT('Ctrl Pts',(17.6336227161477,-3.77421115624452,16.5148795168809));
#44181=CARTESIAN_POINT('Ctrl Pts',(17.6799265463106,-3.19501892204413,15.8876432986447));
#44182=CARTESIAN_POINT('Ctrl Pts',(17.7262303764735,-2.45608562160116,15.4079125693465));
#44183=CARTESIAN_POINT('Ctrl Pts',(17.7725342066363,-1.6474260694984,15.1341268019693));
#44184=CARTESIAN_POINT('Ctrl Pts',(17.8188380367992,-0.838766517395638,
14.8603410345921));
#44185=CARTESIAN_POINT('Ctrl Pts',(17.8651418669621,0.0396192863669109,
14.7925002291359));
#44186=CARTESIAN_POINT('Ctrl Pts',(17.911445697125,0.880728808258228,14.9388685652237));
#44187=CARTESIAN_POINT('Ctrl Pts',(17.9577495272879,1.72183833014957,15.0852369013115));
#44188=CARTESIAN_POINT('Ctrl Pts',(18.0040533574507,2.52567157016968,15.4458143789434));
#44189=CARTESIAN_POINT('Ctrl Pts',(18.0503571876136,3.19430778227486,15.9766764452912));
#44190=CARTESIAN_POINT('Ctrl Pts',(18.0966610177765,3.86294399438003,16.5075385116389));
#44191=CARTESIAN_POINT('Ctrl Pts',(18.1429648479394,4.39638317857029,17.2086851667026));
#44192=CARTESIAN_POINT('Ctrl Pts',(18.1892686781023,4.72964324616823,17.9947046607166));
#44193=CARTESIAN_POINT('Ctrl Pts',(18.2355725082651,5.06290331376618,18.7807241547306));
#44194=CARTESIAN_POINT('Ctrl Pts',(18.281876338428,5.19598426477179,19.6516164876949));
#44195=CARTESIAN_POINT('Ctrl Pts',(18.3281801685909,5.11267454514886,20.5012919600029));
#44196=CARTESIAN_POINT('Ctrl Pts',(18.3744839987538,5.02936482552594,21.3509674323108));
#44197=CARTESIAN_POINT('Ctrl Pts',(18.4207878289167,4.72966443527452,22.1794260439624));
#44198=CARTESIAN_POINT('Ctrl Pts',(18.4670916590795,4.25008204850996,22.8857472541285));
#44199=CARTESIAN_POINT('Ctrl Pts',(18.5133954892424,3.77049966174541,23.5920684642946));
#44200=CARTESIAN_POINT('Ctrl Pts',(18.5596993194053,3.11103527846767,24.1762522729753));
#44201=CARTESIAN_POINT('Ctrl Pts',(18.6060031495682,2.35202302917159,24.5671350214355));
#44202=CARTESIAN_POINT('Ctrl Pts',(18.652306979731,1.59301077987547,24.9580177698958));
#44203=CARTESIAN_POINT('Ctrl Pts',(18.6986108098939,0.734450664561022,25.1555994581356));
#44204=CARTESIAN_POINT('Ctrl Pts',(18.7449146400568,-0.119069893872046,
25.1358112303851));
#44205=CARTESIAN_POINT('Ctrl Pts',(18.7912184702197,-0.972590452305114,
25.1160230026347));
#44206=CARTESIAN_POINT('Ctrl Pts',(18.8375223003826,-1.82107145385673,24.8788648588939));
#44207=CARTESIAN_POINT('Ctrl Pts',(18.8838261305454,-2.5611532854388,24.4532267494776));
#44208=CARTESIAN_POINT('Ctrl Pts',(18.9301299607083,-3.30123511702085,24.0275886400612));
#44209=CARTESIAN_POINT('Ctrl Pts',(18.9764337908712,-3.93291777863336,23.4134705649693));
#44210=CARTESIAN_POINT('Ctrl Pts',(19.0227376210341,-4.37925143241393,22.6856826926272));
#44211=CARTESIAN_POINT('Ctrl Pts',(19.069041451197,-4.82558508619451,21.9578948202851));
#44212=CARTESIAN_POINT('Ctrl Pts',(19.1153452813598,-5.08656973214315,21.1164371506928));
#44213=CARTESIAN_POINT('Ctrl Pts',(19.1616491115227,-5.13041294122744,20.2638137340296));
#44214=CARTESIAN_POINT('Ctrl Pts',(19.1664189059141,-5.13492926508348,20.1759843174035));
#44215=CARTESIAN_POINT('Ctrl Pts',(19.1711887003055,-5.13714145250432,20.0880364185337));
#44216=CARTESIAN_POINT('Ctrl Pts',(19.1759584946968,-5.13707257898892,20.0000850551338));
#44217=CARTESIAN_POINT('Origin',(25.,0.,20.));
#44218=CARTESIAN_POINT('',(20.9259584946969,-5.13657443916938,19.9998752094656));
#44219=CARTESIAN_POINT('',(20.4490415053031,-5.13680856920626,20.000130812524));
#44220=CARTESIAN_POINT('',(25.,-5.13675,20.));
#44221=CARTESIAN_POINT('Ctrl Pts',(20.4490415053031,-5.13680856920626,20.000130812524));
#44222=CARTESIAN_POINT('Ctrl Pts',(20.4393573708119,-5.13699294951738,20.1787253578794));
#44223=CARTESIAN_POINT('Ctrl Pts',(20.4296732363207,-5.12786043275759,20.3573011391577));
#44224=CARTESIAN_POINT('Ctrl Pts',(20.4199891018296,-5.10926909616917,20.5348866815868));
#44225=CARTESIAN_POINT('Ctrl Pts',(20.3736852716667,-5.02037626917714,21.3839962022691));
#44226=CARTESIAN_POINT('Ctrl Pts',(20.3273814415038,-4.71523690500024,22.2104669872532));
#44227=CARTESIAN_POINT('Ctrl Pts',(20.2810776113409,-4.23102223854131,22.9136206472664));
#44228=CARTESIAN_POINT('Ctrl Pts',(20.234773781178,-3.74680757208241,23.6167743072796));
#44229=CARTESIAN_POINT('Ctrl Pts',(20.1884699510152,-3.08351760334145,24.1966108423221));
#44230=CARTESIAN_POINT('Ctrl Pts',(20.1421661208523,-2.32195248507256,24.5824961665313));
#44231=CARTESIAN_POINT('Ctrl Pts',(20.0958622906894,-1.56038736680363,24.9683814907404));
#44232=CARTESIAN_POINT('Ctrl Pts',(20.0495584605265,-0.700547099006791,
25.1603156041162));
#44233=CARTESIAN_POINT('Ctrl Pts',(20.0032546303637,0.152824950777143,25.1349176228668));
#44234=CARTESIAN_POINT('Ctrl Pts',(19.9569508002008,1.00619700056105,25.1095196416174));
#44235=CARTESIAN_POINT('Ctrl Pts',(19.9106469700379,1.85310083233197,24.8667895657428));
#44236=CARTESIAN_POINT('Ctrl Pts',(19.864343139875,2.59036895947021,24.4362961029469));
#44237=CARTESIAN_POINT('Ctrl Pts',(19.8180393097121,3.32763708660844,24.0058026401509));
#44238=CARTESIAN_POINT('Ctrl Pts',(19.7717354795493,3.95526950911397,23.3875457904338));
#44239=CARTESIAN_POINT('Ctrl Pts',(19.7254316493864,4.39680977807037,22.6568398963191));
#44240=CARTESIAN_POINT('Ctrl Pts',(19.6791278192235,4.83835004702677,21.9261340022045));
#44241=CARTESIAN_POINT('Ctrl Pts',(19.6328239890606,5.09379816243402,21.0829790636924));
#44242=CARTESIAN_POINT('Ctrl Pts',(19.5865201588977,5.13203614012476,20.2300858875759));
#44243=CARTESIAN_POINT('Ctrl Pts',(19.5402163287349,5.17027411781551,19.3771927114594));
#44244=CARTESIAN_POINT('Ctrl Pts',(19.493912498572,4.99130195778974,18.5145612977385));
#44245=CARTESIAN_POINT('Ctrl Pts',(19.4476086684091,4.6169215544682,17.7472750236447));
#44246=CARTESIAN_POINT('Ctrl Pts',(19.4013048382462,4.24254115114665,16.9799887495508));
#44247=CARTESIAN_POINT('Ctrl Pts',(19.3550010080833,3.67275250452931,16.3080476150841));
#44248=CARTESIAN_POINT('Ctrl Pts',(19.3086971779205,2.97696569445138,15.8133056341228));
#44249=CARTESIAN_POINT('Ctrl Pts',(19.2623933477576,2.28117888437348,15.3185636531615));
#44250=CARTESIAN_POINT('Ctrl Pts',(19.2160895175947,1.45939391083502,15.0010208257055));
#44251=CARTESIAN_POINT('Ctrl Pts',(19.1697856874318,0.611718350494981,14.8993593423104));
#44252=CARTESIAN_POINT('Ctrl Pts',(19.123481857269,-0.235957209845108,14.7976978589153));
#44253=CARTESIAN_POINT('Ctrl Pts',(19.0771780271061,-1.10952335698676,14.9119177195811));
#44254=CARTESIAN_POINT('Ctrl Pts',(19.0308741969432,-1.90256467466223,15.2281049762243));
#44255=CARTESIAN_POINT('Ctrl Pts',(18.9845703667803,-2.69560599233769,15.5442922328674));
#44256=CARTESIAN_POINT('Ctrl Pts',(18.9382665366174,-3.40812248054695,16.0624468854881));
#44257=CARTESIAN_POINT('Ctrl Pts',(18.8919627064546,-3.95331734784091,16.7194487648463));
#44258=CARTESIAN_POINT('Ctrl Pts',(18.8456588762917,-4.49851221513488,17.3764506442046));
#44259=CARTESIAN_POINT('Ctrl Pts',(18.7993550461288,-4.87638546151354,18.1722997503005));
#44260=CARTESIAN_POINT('Ctrl Pts',(18.7530512159659,-5.04090561135092,19.0100479422421));
#44261=CARTESIAN_POINT('Ctrl Pts',(18.7350479790783,-5.10487213895543,19.3357700066727));
#44262=CARTESIAN_POINT('Ctrl Pts',(18.7170447421907,-5.13658594929633,19.6678259813736));
#44263=CARTESIAN_POINT('Ctrl Pts',(18.6990415053031,-5.13639668367057,19.9999176386971));
#44264=CARTESIAN_POINT('Ctrl Pts',(19.1759584946968,-5.13707257898892,20.0000850551338));
#44265=CARTESIAN_POINT('Ctrl Pts',(19.2174925304683,-5.13647284767606,19.2342291766898));
#44266=CARTESIAN_POINT('Ctrl Pts',(19.2590265662398,-4.96291305319095,18.4681106023481));
#44267=CARTESIAN_POINT('Ctrl Pts',(19.3005606020113,-4.63162896954659,17.7776706539684));
#44268=CARTESIAN_POINT('Ctrl Pts',(19.3468644321742,-4.26230001656154,17.0079401543048));
#44269=CARTESIAN_POINT('Ctrl Pts',(19.3931682623371,-3.69694033837151,16.332268318712));
#44270=CARTESIAN_POINT('Ctrl Pts',(19.4394720925,-3.00442049010556,15.8329636247795));
#44271=CARTESIAN_POINT('Ctrl Pts',(19.4857759226629,-2.31190064183958,15.333658930847));
#44272=CARTESIAN_POINT('Ctrl Pts',(19.5320797528257,-1.49222062349769,15.0107213785748));
#44273=CARTESIAN_POINT('Ctrl Pts',(19.5783835829886,-0.645231591908269,
14.9034903290016));
#44274=CARTESIAN_POINT('Ctrl Pts',(19.6246874131515,0.20175743968115,14.7962592794284));
#44275=CARTESIAN_POINT('Ctrl Pts',(19.6709912433144,1.07605548451817,14.9047347325541));
#44276=CARTESIAN_POINT('Ctrl Pts',(19.7172950734773,1.87115796857826,15.2157025081625));
#44277=CARTESIAN_POINT('Ctrl Pts',(19.7635989036401,2.66626045263838,15.5266702837709));
#44278=CARTESIAN_POINT('Ctrl Pts',(19.809902733803,3.38216737592161,16.0401303818618));
#44279=CARTESIAN_POINT('Ctrl Pts',(19.8562065639659,3.93166893353869,16.6935345108676));
#44280=CARTESIAN_POINT('Ctrl Pts',(19.9025103941288,4.48117049115577,17.3469386398734));
#44281=CARTESIAN_POINT('Ctrl Pts',(19.9488142242917,4.86426668310665,18.1402867997939));
#44282=CARTESIAN_POINT('Ctrl Pts',(19.9951180544545,5.03428978895545,18.9769355080957));
#44283=CARTESIAN_POINT('Ctrl Pts',(20.0414218846174,5.20431289480425,19.8135842163973));
#44284=CARTESIAN_POINT('Ctrl Pts',(20.0877257147803,5.16126291455098,20.6935334730801));
#44285=CARTESIAN_POINT('Ctrl Pts',(20.1340295449432,4.91038407793598,21.5095902890948));
#44286=CARTESIAN_POINT('Ctrl Pts',(20.180333375106,4.65950524132096,22.3256471051096));
#44287=CARTESIAN_POINT('Ctrl Pts',(20.2266372052689,4.20079754834418,23.0778114804561));
#44288=CARTESIAN_POINT('Ctrl Pts',(20.2729410354318,3.59013950374517,23.6744568275359));
#44289=CARTESIAN_POINT('Ctrl Pts',(20.3192448655947,2.97948145914616,24.2711021746156));
#44290=CARTESIAN_POINT('Ctrl Pts',(20.3655486957576,2.21687306292492,24.7122284934286));
#44291=CARTESIAN_POINT('Ctrl Pts',(20.4118525259204,1.39521316446878,24.9440989936964));
#44292=CARTESIAN_POINT('Ctrl Pts',(20.4581563560833,0.57355326601265,25.1759694939642));
#44293=CARTESIAN_POINT('Ctrl Pts',(20.5044601862462,-0.307158134678377,
25.198584175687));
#44294=CARTESIAN_POINT('Ctrl Pts',(20.5507640164091,-1.13963520627605,25.0091881807727));
#44295=CARTESIAN_POINT('Ctrl Pts',(20.5970678465719,-1.97211227787367,24.8197921858584));
#44296=CARTESIAN_POINT('Ctrl Pts',(20.6433716767348,-2.75635502037793,24.4183855143072));
#44297=CARTESIAN_POINT('Ctrl Pts',(20.6896755068977,-3.39682914806631,23.8538664186274));
#44298=CARTESIAN_POINT('Ctrl Pts',(20.7359793370606,-4.03730327575471,23.2893473229476));
#44299=CARTESIAN_POINT('Ctrl Pts',(20.7822831672235,-4.53400878862721,22.5617158031392));
#44300=CARTESIAN_POINT('Ctrl Pts',(20.8285869973863,-4.82643839243051,21.7596099220706));
#44301=CARTESIAN_POINT('Ctrl Pts',(20.8610441631565,-5.03142005579099,21.1973652123891));
#44302=CARTESIAN_POINT('Ctrl Pts',(20.8935013289267,-5.13603158465629,20.5985278291506));
#44303=CARTESIAN_POINT('Ctrl Pts',(20.9259584946969,-5.13657443916938,19.9998752094656));
#44304=CARTESIAN_POINT('Origin',(25.,0.,20.));
#44305=CARTESIAN_POINT('',(22.6759584946968,-5.1365747461539,20.0001248276021));
#44306=CARTESIAN_POINT('',(22.1990415053031,-5.13685244596756,19.9998725425992));
#44307=CARTESIAN_POINT('',(25.,-5.13675,20.));
#44308=CARTESIAN_POINT('Ctrl Pts',(22.1990415053031,-5.13685244596756,19.9998725425992));
#44309=CARTESIAN_POINT('Ctrl Pts',(22.1616699994331,-5.13614579389918,20.6890598759674));
#44310=CARTESIAN_POINT('Ctrl Pts',(22.1242984935631,-4.99651893549095,21.3785248624566));
#44311=CARTESIAN_POINT('Ctrl Pts',(22.0869269876932,-4.72657997268596,22.012504961736));
#44312=CARTESIAN_POINT('Ctrl Pts',(22.0406231575303,-4.39212173780621,22.7980153702763));
#44313=CARTESIAN_POINT('Ctrl Pts',(21.9943193273674,-3.85761403741936,23.4983477972205));
#44314=CARTESIAN_POINT('Ctrl Pts',(21.9480154972046,-3.18816912389587,24.0281896798246));
#44315=CARTESIAN_POINT('Ctrl Pts',(21.9017116670417,-2.51872421037239,24.5580315624287));
#44316=CARTESIAN_POINT('Ctrl Pts',(21.8554078368788,-1.71434208371228,24.9173829006927));
#44317=CARTESIAN_POINT('Ctrl Pts',(21.8091040067159,-0.87301035381432,25.0624685067012));
#44318=CARTESIAN_POINT('Ctrl Pts',(21.762800176553,-0.031678623916381,25.2075541127096));
#44319=CARTESIAN_POINT('Ctrl Pts',(21.7164963463902,0.846602709219399,25.1383739864625));
#44320=CARTESIAN_POINT('Ctrl Pts',(21.6701925162273,1.65484383838534,24.8633554599439));
#44321=CARTESIAN_POINT('Ctrl Pts',(21.6238886860644,2.46308496755134,24.5883369334253));
#44322=CARTESIAN_POINT('Ctrl Pts',(21.5775848559015,3.20128589274747,24.1074800066352));
#44323=CARTESIAN_POINT('Ctrl Pts',(21.5312810257386,3.77952101532157,23.4793613428259));
#44324=CARTESIAN_POINT('Ctrl Pts',(21.4849771955758,4.35775613789566,22.8512426790165));
#44325=CARTESIAN_POINT('Ctrl Pts',(21.4386733654129,4.77602545784771,22.0758622781877));
#44326=CARTESIAN_POINT('Ctrl Pts',(21.39236953525,4.98337656139613,21.2476748400669));
#44327=CARTESIAN_POINT('Ctrl Pts',(21.3460657050871,5.19072766494455,20.419487401946));
#44328=CARTESIAN_POINT('Ctrl Pts',(21.2997618749242,5.18716055208937,19.538492926533));
#44329=CARTESIAN_POINT('Ctrl Pts',(21.2534580447614,4.97310975867039,18.7120117285372));
#44330=CARTESIAN_POINT('Ctrl Pts',(21.2071542145985,4.75905896525139,17.8855305305414));
#44331=CARTESIAN_POINT('Ctrl Pts',(21.1608503844356,4.33452449126856,17.1135626099627));
#44332=CARTESIAN_POINT('Ctrl Pts',(21.1145465542728,3.7512219542704,16.4901469676056));
#44333=CARTESIAN_POINT('Ctrl Pts',(21.0682427241099,3.16791941727224,15.8667313252485));
#44334=CARTESIAN_POINT('Ctrl Pts',(21.021938893947,2.42584881725878,15.391867961113));
#44335=CARTESIAN_POINT('Ctrl Pts',(20.9756350637841,1.61540714598487,15.123403419196));
#44336=CARTESIAN_POINT('Ctrl Pts',(20.9293312336212,0.804965474710955,14.8549388772789));
#44337=CARTESIAN_POINT('Ctrl Pts',(20.8830274034583,-0.0738472678233812,
14.7928731575803));
#44338=CARTESIAN_POINT('Ctrl Pts',(20.8367235732955,-0.913976539584659,
14.9447669347203));
#44339=CARTESIAN_POINT('Ctrl Pts',(20.7904197431326,-1.75410581134589,15.0966607118603));
#44340=CARTESIAN_POINT('Ctrl Pts',(20.7441159129697,-2.55555161233405,15.4625139858388));
#44341=CARTESIAN_POINT('Ctrl Pts',(20.6978120828068,-3.22068402773702,15.9977595208823));
#44342=CARTESIAN_POINT('Ctrl Pts',(20.6515082526439,-3.88581644314001,16.533005055926));
#44343=CARTESIAN_POINT('Ctrl Pts',(20.6052044224811,-4.41463547295778,17.2376428520347));
#44344=CARTESIAN_POINT('Ctrl Pts',(20.5589005923182,-4.74272184296308,18.0258358782793));
#44345=CARTESIAN_POINT('Ctrl Pts',(20.5222808966465,-5.00219115643817,18.6491836369876));
#44346=CARTESIAN_POINT('Ctrl Pts',(20.4856612009748,-5.13611135141281,19.3247913791957));
#44347=CARTESIAN_POINT('Ctrl Pts',(20.4490415053031,-5.13680856920626,20.000130812524));
#44348=CARTESIAN_POINT('Ctrl Pts',(20.9259584946969,-5.13657443916938,19.9998752094656));
#44349=CARTESIAN_POINT('Ctrl Pts',(20.9398051590896,-5.13680602822155,19.7444819329456));
#44350=CARTESIAN_POINT('Ctrl Pts',(20.9536518234823,-5.11809721635881,19.4891222832186));
#44351=CARTESIAN_POINT('Ctrl Pts',(20.967498487875,-5.08016083691862,19.2366517801062));
#44352=CARTESIAN_POINT('Ctrl Pts',(21.0138023180379,-4.95329998286932,18.3923797615392));
#44353=CARTESIAN_POINT('Ctrl Pts',(21.0601061482008,-4.61142458003661,17.5804159667339));
#44354=CARTESIAN_POINT('Ctrl Pts',(21.1064099783636,-4.09618094613004,16.8996715834709));
#44355=CARTESIAN_POINT('Ctrl Pts',(21.1527138085265,-3.58093731222347,16.2189272002079));
#44356=CARTESIAN_POINT('Ctrl Pts',(21.1990176386894,-2.89232544724305,15.6694022284871));
#44357=CARTESIAN_POINT('Ctrl Pts',(21.2453214688522,-2.11423014743298,15.3180382832127));
#44358=CARTESIAN_POINT('Ctrl Pts',(21.2916252990151,-1.3361348476229,14.9666743379382));
#44359=CARTESIAN_POINT('Ctrl Pts',(21.337929129178,-0.468556112983181,14.8134714191101));
#44360=CARTESIAN_POINT('Ctrl Pts',(21.3842329593409,0.382820010279116,14.877092283331));
#44361=CARTESIAN_POINT('Ctrl Pts',(21.4305367895038,1.23419613354144,14.940713147552));
#44362=CARTESIAN_POINT('Ctrl Pts',(21.4768406196667,2.06936964542633,15.221157794822));
#44363=CARTESIAN_POINT('Ctrl Pts',(21.5231444498295,2.78660201449705,15.6842632324738));
#44364=CARTESIAN_POINT('Ctrl Pts',(21.5694482799924,3.50383438356776,16.1473686701255));
#44365=CARTESIAN_POINT('Ctrl Pts',(21.6157521101553,4.10312560982429,16.7931348981589));
#44366=CARTESIAN_POINT('Ctrl Pts',(21.6620559403182,4.51147169063172,17.5428964575327));
#44367=CARTESIAN_POINT('Ctrl Pts',(21.708359770481,4.91981777143912,18.2926580169065));
#44368=CARTESIAN_POINT('Ctrl Pts',(21.7546636006439,5.13721870679744,19.1464149076206));
#44369=CARTESIAN_POINT('Ctrl Pts',(21.8009674308068,5.13719131497069,20.0001648223351));
#44370=CARTESIAN_POINT('Ctrl Pts',(21.8472712609697,5.13716392314393,20.8539147370496));
#44371=CARTESIAN_POINT('Ctrl Pts',(21.8935750911326,4.91970820413208,21.7076576757646));
#44372=CARTESIAN_POINT('Ctrl Pts',(21.9398789212954,4.51131401326454,22.4573930307339));
#44373=CARTESIAN_POINT('Ctrl Pts',(21.9861827514583,4.10291982239703,23.2071283857032));
#44374=CARTESIAN_POINT('Ctrl Pts',(22.0324865816212,3.50358715967385,23.852856156927));
#44375=CARTESIAN_POINT('Ctrl Pts',(22.0787904117841,2.7863250754059,24.3159155700663));
#44376=CARTESIAN_POINT('Ctrl Pts',(22.125094241947,2.06906299113791,24.7789749832056));
#44377=CARTESIAN_POINT('Ctrl Pts',(22.1713980721098,1.23387148532514,25.0593660382605));
#44378=CARTESIAN_POINT('Ctrl Pts',(22.2177019022727,0.382491281374938,25.1229322710191));
#44379=CARTESIAN_POINT('Ctrl Pts',(22.2640057324356,-0.468888922575259,
25.1864985037777));
#44380=CARTESIAN_POINT('Ctrl Pts',(22.3103095625985,-1.33645782466288,25.0332399142401));
#44381=CARTESIAN_POINT('Ctrl Pts',(22.3566133927614,-2.11453057645518,24.6818260406611));
#44382=CARTESIAN_POINT('Ctrl Pts',(22.4029172229242,-2.89260332824749,24.3304121670822));
#44383=CARTESIAN_POINT('Ctrl Pts',(22.4492210530871,-3.58117992974448,23.780843009462));
#44384=CARTESIAN_POINT('Ctrl Pts',(22.49552488325,-4.09637988040214,23.1000655653088));
#44385=CARTESIAN_POINT('Ctrl Pts',(22.5418287134129,-4.61157983105977,22.4192881211556));
#44386=CARTESIAN_POINT('Ctrl Pts',(22.5881325435757,-4.95340313087809,21.6073023904696));
#44387=CARTESIAN_POINT('Ctrl Pts',(22.6344363737386,-5.08020980919293,20.7630222331994));
#44388=CARTESIAN_POINT('Ctrl Pts',(22.6482770807247,-5.11811367313376,20.510657920575));
#44389=CARTESIAN_POINT('Ctrl Pts',(22.6621177877108,-5.13680632573211,20.2554081796058));
#44390=CARTESIAN_POINT('Ctrl Pts',(22.6759584946968,-5.1365747461539,20.0001248276021));
#44391=CARTESIAN_POINT('Origin',(25.,0.,20.));
#44392=CARTESIAN_POINT('',(24.4259584946968,-5.13707231536035,19.9999148579252));
#44393=CARTESIAN_POINT('',(23.9490415053031,-5.13637392180183,20.0000717483683));
#44394=CARTESIAN_POINT('',(25.,-5.13675,20.));
#44395=CARTESIAN_POINT('Ctrl Pts',(23.9490415053031,-5.13637392180183,20.0000717483683));
#44396=CARTESIAN_POINT('Ctrl Pts',(23.9302864582172,-5.13654471386954,20.3460358505988));
#44397=CARTESIAN_POINT('Ctrl Pts',(23.9115314111314,-5.10210725044954,20.6919664138276));
#44398=CARTESIAN_POINT('Ctrl Pts',(23.8927763640455,-5.03272390749879,21.0307397974748));
#44399=CARTESIAN_POINT('Ctrl Pts',(23.8464725338826,-4.86142524248265,21.8671282719098));
#44400=CARTESIAN_POINT('Ctrl Pts',(23.8001687037197,-4.47711976629267,22.6598913455785));
#44401=CARTESIAN_POINT('Ctrl Pts',(23.7538648735568,-3.9266225110321,23.3124568095394));
#44402=CARTESIAN_POINT('Ctrl Pts',(23.7075610433939,-3.37612525577151,23.9650222735004));
#44403=CARTESIAN_POINT('Ctrl Pts',(23.6612572132311,-2.65943622144031,24.4773901277534));
#44404=CARTESIAN_POINT('Ctrl Pts',(23.6149533830682,-1.86386048753644,24.7871451348595));
#44405=CARTESIAN_POINT('Ctrl Pts',(23.5686495529053,-1.06828475363257,25.0969001419655));
#44406=CARTESIAN_POINT('Ctrl Pts',(23.5223457227424,-0.193822320156021,
25.2040423019247));
#44407=CARTESIAN_POINT('Ctrl Pts',(23.4760418925795,0.65300221349861,25.0955198526131));
#44408=CARTESIAN_POINT('Ctrl Pts',(23.4297380624166,1.49982674715322,24.9869974033015));
#44409=CARTESIAN_POINT('Ctrl Pts',(23.3834342322538,2.31901338098592,24.6628103447192));
#44410=CARTESIAN_POINT('Ctrl Pts',(23.3371304020909,3.01077106090705,24.1624502493138));
#44411=CARTESIAN_POINT('Ctrl Pts',(23.2908265719281,3.7025287408282,23.6620901539085));
#44412=CARTESIAN_POINT('Ctrl Pts',(23.2445227417652,4.26685746683774,22.9855570216801));
#44413=CARTESIAN_POINT('Ctrl Pts',(23.1982189116023,4.63501227155502,22.2152642509964));
#44414=CARTESIAN_POINT('Ctrl Pts',(23.1519150814394,5.00316707627228,21.4449714803128));
#44415=CARTESIAN_POINT('Ctrl Pts',(23.1056112512765,5.17514795969726,20.5809190711738));
#44416=CARTESIAN_POINT('Ctrl Pts',(23.0593074211136,5.13000468542294,19.7283635025498));
#44417=CARTESIAN_POINT('Ctrl Pts',(23.0130035909508,5.08486141114861,18.8758079339259));
#44418=CARTESIAN_POINT('Ctrl Pts',(22.9666997607879,4.822593979175,18.0347492058169));
#44419=CARTESIAN_POINT('Ctrl Pts',(22.920395930625,4.37515108398647,17.3076427704518));
#44420=CARTESIAN_POINT('Ctrl Pts',(22.8740921004621,3.92770818879797,16.5805363350868));
#44421=CARTESIAN_POINT('Ctrl Pts',(22.8277882702993,3.2950898303946,15.9673821924658));
#44422=CARTESIAN_POINT('Ctrl Pts',(22.7814844401364,2.55435983063849,15.5428730874218));
#44423=CARTESIAN_POINT('Ctrl Pts',(22.7351806099735,1.81362983088237,15.1183639823779));
#44424=CARTESIAN_POINT('Ctrl Pts',(22.6888767798106,0.964788189773507,14.882499914911));
#44425=CARTESIAN_POINT('Ctrl Pts',(22.6425729496478,0.11123845251519,14.864013194537));
#44426=CARTESIAN_POINT('Ctrl Pts',(22.5962691194849,-0.742311284743175,
14.8455264741629));
#44427=CARTESIAN_POINT('Ctrl Pts',(22.549965289322,-1.60056911815101,15.0444171008817));
#44428=CARTESIAN_POINT('Ctrl Pts',(22.5036614591591,-2.35898444795574,15.4364567676518));
#44429=CARTESIAN_POINT('Ctrl Pts',(22.4573576289962,-3.11739977776043,15.8284964344218));
#44430=CARTESIAN_POINT('Ctrl Pts',(22.4110537988333,-3.77597260396205,16.4136851412431));
#44431=CARTESIAN_POINT('Ctrl Pts',(22.3647499686705,-4.25447740308742,17.1207368154636));
#44432=CARTESIAN_POINT('Ctrl Pts',(22.3184461385076,-4.73298220221278,17.827788489684));
#44433=CARTESIAN_POINT('Ctrl Pts',(22.2721423083447,-5.0314189742619,18.6567031313036));
#44434=CARTESIAN_POINT('Ctrl Pts',(22.2258384781818,-5.11343297560014,19.5065046471815));
#44435=CARTESIAN_POINT('Ctrl Pts',(22.2169061538889,-5.12925403519577,19.6704371490444));
#44436=CARTESIAN_POINT('Ctrl Pts',(22.207973829596,-5.1370213459166,19.8351469149609));
#44437=CARTESIAN_POINT('Ctrl Pts',(22.1990415053031,-5.13685244596756,19.9998725425992));
#44438=CARTESIAN_POINT('Ctrl Pts',(22.6759584946968,-5.1365747461539,20.0001248276021));
#44439=CARTESIAN_POINT('Ctrl Pts',(22.7084216178736,-5.13603158052079,19.4013624298848));
#44440=CARTESIAN_POINT('Ctrl Pts',(22.7408847410504,-5.03138084291631,18.802415128328));
#44441=CARTESIAN_POINT('Ctrl Pts',(22.7733478642272,-4.82632547137258,18.240080377359));
#44442=CARTESIAN_POINT('Ctrl Pts',(22.8196516943901,-4.53384439842607,17.437993262643));
#44443=CARTESIAN_POINT('Ctrl Pts',(22.865955524553,-4.0370921957217,16.7103936170653));
#44444=CARTESIAN_POINT('Ctrl Pts',(22.9122593547159,-3.39658184513919,16.1459156206632));
#44445=CARTESIAN_POINT('Ctrl Pts',(22.9585631848788,-2.75607149455666,15.5814376242612));
#44446=CARTESIAN_POINT('Ctrl Pts',(23.0048670150417,-1.97180299609605,15.180081277035));
#44447=CARTESIAN_POINT('Ctrl Pts',(23.0511708452045,-1.13931377299928,14.9907387011226));
#44448=CARTESIAN_POINT('Ctrl Pts',(23.0974746753674,-0.306824549902529,
14.8013961252102));
#44449=CARTESIAN_POINT('Ctrl Pts',(23.1437785055303,0.57388539783039,14.8240673206118));
#44450=CARTESIAN_POINT('Ctrl Pts',(23.1900823356932,1.39553041586644,15.0559905448949));
#44451=CARTESIAN_POINT('Ctrl Pts',(23.236386165856,2.21717543390246,15.2879137691781));
#44452=CARTESIAN_POINT('Ctrl Pts',(23.2826899960189,2.9797555222417,15.7290890223429));
#44453=CARTESIAN_POINT('Ctrl Pts',(23.3289938261818,3.59037527988484,16.3257735530634));
#44454=CARTESIAN_POINT('Ctrl Pts',(23.3752976563447,4.20099503752802,16.9224580837839));
#44455=CARTESIAN_POINT('Ctrl Pts',(23.4216014865076,4.6596544644751,17.6746518920602));
#44456=CARTESIAN_POINT('Ctrl Pts',(23.4679053166704,4.91048093562102,18.4907248048553));
#44457=CARTESIAN_POINT('Ctrl Pts',(23.5142091468333,5.16130740676694,19.3067977176504));
#44458=CARTESIAN_POINT('Ctrl Pts',(23.5605129769962,5.20430092211171,20.1867497349642));
#44459=CARTESIAN_POINT('Ctrl Pts',(23.6068168071591,5.0342241303143,21.0233875314552));
#44460=CARTESIAN_POINT('Ctrl Pts',(23.653120637322,4.86414733851688,21.8600253279462));
#44461=CARTESIAN_POINT('Ctrl Pts',(23.6994244674848,4.48100023957725,22.6533489036142));
#44462=CARTESIAN_POINT('Ctrl Pts',(23.7457282976477,3.93145675528012,23.3067177707115));
#44463=CARTESIAN_POINT('Ctrl Pts',(23.7920321278106,3.38191327098302,23.9600866378087));
#44464=CARTESIAN_POINT('Ctrl Pts',(23.8383359579735,2.66597340132842,24.4735007963352));
#44465=CARTESIAN_POINT('Ctrl Pts',(23.8846397881363,1.87085096464169,24.7844175509539));
#44466=CARTESIAN_POINT('Ctrl Pts',(23.9309436182992,1.07572852795493,25.0953343055727));
#44467=CARTESIAN_POINT('Ctrl Pts',(23.9772474484621,0.201423524236018,25.2037536562837));
#44468=CARTESIAN_POINT('Ctrl Pts',(24.023551278625,-0.645558624778892,25.096468257112));
#44469=CARTESIAN_POINT('Ctrl Pts',(24.0698551087879,-1.49254077379385,24.9891828579403));
#44470=CARTESIAN_POINT('Ctrl Pts',(24.1161589389507,-2.31220006810482,24.6661927088857));
#44471=CARTESIAN_POINT('Ctrl Pts',(24.1624627691136,-3.00468787542759,24.1668435781818));
#44472=CARTESIAN_POINT('Ctrl Pts',(24.2087665992765,-3.69717568275031,23.667494447478));
#44473=CARTESIAN_POINT('Ctrl Pts',(24.2550704294394,-4.26249200308487,22.9917863351248));
#44474=CARTESIAN_POINT('Ctrl Pts',(24.3013742596023,-4.63177156303645,22.2220321378467));
#44475=CARTESIAN_POINT('Ctrl Pts',(24.3429023379671,-4.96296383050694,21.5316699688036));
#44476=CARTESIAN_POINT('Ctrl Pts',(24.384430416332,-5.13647219728032,20.7656610002149));
#44477=CARTESIAN_POINT('Ctrl Pts',(24.4259584946968,-5.13707231536035,19.9999148579252));
#44478=CARTESIAN_POINT('Origin',(25.,0.,20.));
#44479=CARTESIAN_POINT('',(26.1759584946969,-5.13631118199777,20.0000041318326));
#44480=CARTESIAN_POINT('',(25.6990415053031,-5.13719123497192,20.0000027154119));
#44481=CARTESIAN_POINT('',(25.,-5.13675,20.));
#44482=CARTESIAN_POINT('Ctrl Pts',(25.6990415053031,-5.1371911776762,20.0000027150593));
#44483=CARTESIAN_POINT('Ctrl Pts',(25.6525990868384,-5.13721811325437,20.8563079779957));
#44484=CARTESIAN_POINT('Ctrl Pts',(25.6061566683738,-4.9184342166288,21.71259975382));
#44485=CARTESIAN_POINT('Ctrl Pts',(25.5597142499091,-4.50771973522286,22.4639799609353));
#44486=CARTESIAN_POINT('Ctrl Pts',(25.5134104197462,-4.09823086230967,23.2131179827739));
#44487=CARTESIAN_POINT('Ctrl Pts',(25.4671065895833,-3.49795564305339,23.8579696332713));
#44488=CARTESIAN_POINT('Ctrl Pts',(25.4208027594205,-2.78001794739953,24.3199808646966));
#44489=CARTESIAN_POINT('Ctrl Pts',(25.3744989292576,-2.06208025174567,24.7819920961219));
#44490=CARTESIAN_POINT('Ctrl Pts',(25.3281950990947,-1.22648007969423,25.0611629084752));
#44491=CARTESIAN_POINT('Ctrl Pts',(25.2818912689318,-0.375007937245508,
25.1234854841417));
#44492=CARTESIAN_POINT('Ctrl Pts',(25.235587438769,0.476464205203244,25.1858080598083));
#44493=CARTESIAN_POINT('Ctrl Pts',(25.1892836086061,1.34380831804928,25.031282398788));
#44494=CARTESIAN_POINT('Ctrl Pts',(25.1429797784432,2.12136693606468,24.6787323904857));
#44495=CARTESIAN_POINT('Ctrl Pts',(25.0966759482803,2.89892555408006,24.3261823821834));
#44496=CARTESIAN_POINT('Ctrl Pts',(25.0503721181174,3.5866986772648,23.7756080265991));
#44497=CARTESIAN_POINT('Ctrl Pts',(25.0040682879546,4.10090368258461,23.0940787716819));
#44498=CARTESIAN_POINT('Ctrl Pts',(24.9577644577917,4.61510868790441,22.4125495167647));
#44499=CARTESIAN_POINT('Ctrl Pts',(24.9114606276288,4.95574557535929,21.6000653625146));
#44500=CARTESIAN_POINT('Ctrl Pts',(24.8651567974659,5.08131889976369,20.755600885463));
#44501=CARTESIAN_POINT('Ctrl Pts',(24.818852967303,5.20689222416809,19.9111364084115));
#44502=CARTESIAN_POINT('Ctrl Pts',(24.7725491371402,5.11740198552201,19.0346916085584));
#44503=CARTESIAN_POINT('Ctrl Pts',(24.7262453069773,4.82374963762902,18.2330325716974));
#44504=CARTESIAN_POINT('Ctrl Pts',(24.6799414768144,4.53009728973603,17.4313735348365));
#44505=CARTESIAN_POINT('Ctrl Pts',(24.6336376466515,4.03228283259613,16.7045002609676));
#44506=CARTESIAN_POINT('Ctrl Pts',(24.5873338164887,3.39094864899165,16.1409584455321));
#44507=CARTESIAN_POINT('Ctrl Pts',(24.5410299863258,2.74961446538713,15.5774166300966));
#44508=CARTESIAN_POINT('Ctrl Pts',(24.4947261561629,1.96476055531803,15.1772062730945));
#44509=CARTESIAN_POINT('Ctrl Pts',(24.448422326,1.13199565525229,14.9890798952989));
#44510=CARTESIAN_POINT('Ctrl Pts',(24.4021184958371,0.299230755186634,14.8009535175032));
#44511=CARTESIAN_POINT('Ctrl Pts',(24.3558146656743,-0.581445134875576,
14.8249111189138));
#44512=CARTESIAN_POINT('Ctrl Pts',(24.3095108355114,-1.40275050941299,15.0580342506701));
#44513=CARTESIAN_POINT('Ctrl Pts',(24.2632070053485,-2.22405588395042,15.2911573824264));
#44514=CARTESIAN_POINT('Ctrl Pts',(24.2169031751856,-2.98599074296305,15.7334460445283));
#44515=CARTESIAN_POINT('Ctrl Pts',(24.1705993450227,-3.59573828550665,16.3310218532472));
#44516=CARTESIAN_POINT('Ctrl Pts',(24.1242955148599,-4.20548582805026,16.928597661966));
#44517=CARTESIAN_POINT('Ctrl Pts',(24.077991684697,-4.66304605412489,17.6814606173018));
#44518=CARTESIAN_POINT('Ctrl Pts',(24.0316878545341,-4.91268024024106,18.4978990325703));
#44519=CARTESIAN_POINT('Ctrl Pts',(24.0041390714571,-5.06120182080424,18.9836446980768));
#44520=CARTESIAN_POINT('Ctrl Pts',(23.9765902883801,-5.13612304993768,19.4918944048967));
#44521=CARTESIAN_POINT('Ctrl Pts',(23.9490415053031,-5.13637392180183,20.0000717483683));
#44522=CARTESIAN_POINT('Ctrl Pts',(24.4259584946968,-5.13707231536035,19.9999148579252));
#44523=CARTESIAN_POINT('Ctrl Pts',(24.4307342464949,-5.13714132926883,19.9118536314043));
#44524=CARTESIAN_POINT('Ctrl Pts',(24.4355099982929,-5.13492360976748,19.8237958807944));
#44525=CARTESIAN_POINT('Ctrl Pts',(24.4402857500909,-5.13039600219461,19.7358570568002));
#44526=CARTESIAN_POINT('Ctrl Pts',(24.4865895802538,-5.08649808183254,18.8832364552351));
#44527=CARTESIAN_POINT('Ctrl Pts',(24.5328934104167,-4.82545944153983,18.041795534308));
#44528=CARTESIAN_POINT('Ctrl Pts',(24.5791972405795,-4.3790790877908,17.3140363039218));
#44529=CARTESIAN_POINT('Ctrl Pts',(24.6255010707424,-3.93269873404178,16.5862770735357));
#44530=CARTESIAN_POINT('Ctrl Pts',(24.6718049009053,-3.30097666683647,15.9721995336905));
#44531=CARTESIAN_POINT('Ctrl Pts',(24.7181087310681,-2.56086752431778,15.5466089149199));
#44532=CARTESIAN_POINT('Ctrl Pts',(24.764412561231,-1.82075838179906,15.1210182961492));
#44533=CARTESIAN_POINT('Ctrl Pts',(24.8107163913939,-0.972262163966955,
14.8839145984532));
#44534=CARTESIAN_POINT('Ctrl Pts',(24.8570202215568,-0.118740337514819,
14.8641811396795));
#44535=CARTESIAN_POINT('Ctrl Pts',(24.9033240517197,0.734781488937317,14.8444476809058));
#44536=CARTESIAN_POINT('Ctrl Pts',(24.9496278818825,1.59332892400947,15.0420844610545));
#44537=CARTESIAN_POINT('Ctrl Pts',(24.9959317120454,2.35231608947392,15.4330159132116));
#44538=CARTESIAN_POINT('Ctrl Pts',(25.0422355422083,3.1113032549384,15.8239473653686));
#44539=CARTESIAN_POINT('Ctrl Pts',(25.0885393723712,3.77073015079515,16.408173489534));
#44540=CARTESIAN_POINT('Ctrl Pts',(25.1348432025341,4.25026721316356,17.1145254722172));
#44541=CARTESIAN_POINT('Ctrl Pts',(25.181147032697,4.72980427553196,17.8208774549004));
#44542=CARTESIAN_POINT('Ctrl Pts',(25.2274508628598,5.02945150441205,18.6493552961014));
#44543=CARTESIAN_POINT('Ctrl Pts',(25.2737546930227,5.11270670165989,19.4990361125004));
#44544=CARTESIAN_POINT('Ctrl Pts',(25.3200585231856,5.19596189890774,20.3487169288995));
#44545=CARTESIAN_POINT('Ctrl Pts',(25.3663623533485,5.06282506452336,21.2196007204967));
#44546=CARTESIAN_POINT('Ctrl Pts',(25.4126661835114,4.72951456010185,22.0055988281711));
#44547=CARTESIAN_POINT('Ctrl Pts',(25.4589700136742,4.39620405568035,22.7915969358455));
#44548=CARTESIAN_POINT('Ctrl Pts',(25.5052738438371,3.86271988122177,23.4927093595969));
#44549=CARTESIAN_POINT('Ctrl Pts',(25.551577674,3.19404960599373,24.023528519624));
#44550=CARTESIAN_POINT('Ctrl Pts',(25.5978815041629,2.52537933076573,24.5543476796511));
#44551=CARTESIAN_POINT('Ctrl Pts',(25.6441853343257,1.72152295476826,24.9148735759537));
#44552=CARTESIAN_POINT('Ctrl Pts',(25.6904891644886,0.880404042405986,25.0611879391989));
#44553=CARTESIAN_POINT('Ctrl Pts',(25.7367929946515,0.0392851300436907,
25.207502302444));
#44554=CARTESIAN_POINT('Ctrl Pts',(25.7830968248144,-0.839096318683453,
25.1396051326317));
#44555=CARTESIAN_POINT('Ctrl Pts',(25.8294006549773,-1.64773830076283,24.8657674755352));
#44556=CARTESIAN_POINT('Ctrl Pts',(25.8757044851401,-2.4563802828422,24.5919298184387));
#44557=CARTESIAN_POINT('Ctrl Pts',(25.922008315303,-3.19528279827379,24.112151674058));
#44558=CARTESIAN_POINT('Ctrl Pts',(25.9683121454659,-3.77443478261991,23.4848782913505));
#44559=CARTESIAN_POINT('Ctrl Pts',(26.0146159756288,-4.35358676696605,22.8576049086429));
#44560=CARTESIAN_POINT('Ctrl Pts',(26.0609198057917,-4.7729882202267,22.0828362876086));
#44561=CARTESIAN_POINT('Ctrl Pts',(26.1072236359545,-4.98154881526628,21.2549526026491));
#44562=CARTESIAN_POINT('Ctrl Pts',(26.1301352555353,-5.08474677958754,20.8453070942711));
#44563=CARTESIAN_POINT('Ctrl Pts',(26.1530468751161,-5.13632301784513,20.422657032113));
#44564=CARTESIAN_POINT('Ctrl Pts',(26.1759584946969,-5.13631118199777,20.0000041318326));
#44565=CARTESIAN_POINT('Origin',(25.,0.,20.));
#44566=CARTESIAN_POINT('',(27.9259584946968,-5.13709288667488,20.0000779211054));
#44567=CARTESIAN_POINT('',(27.4490415053031,-5.13638193362529,19.999924256499));
#44568=CARTESIAN_POINT('',(25.,-5.13675,20.));
#44569=CARTESIAN_POINT('Ctrl Pts',(27.4490415053031,-5.13638193362529,19.999924256499));
#44570=CARTESIAN_POINT('Ctrl Pts',(27.4212155456225,-5.13611389747151,20.5132122334074));
#44571=CARTESIAN_POINT('Ctrl Pts',(27.3933895859419,-5.05965382718386,21.0265783069614));
#44572=CARTESIAN_POINT('Ctrl Pts',(27.3655636262614,-4.90817380383266,21.5167611448673));
#44573=CARTESIAN_POINT('Ctrl Pts',(27.3192597960985,-4.65610324257109,22.33245063539));
#44574=CARTESIAN_POINT('Ctrl Pts',(27.2729559659356,-4.19629737338143,23.0839441833737));
#44575=CARTESIAN_POINT('Ctrl Pts',(27.2266521357728,-3.58476847779756,23.679696919557));
#44576=CARTESIAN_POINT('Ctrl Pts',(27.1803483056099,-2.97323958221369,24.2754496557403));
#44577=CARTESIAN_POINT('Ctrl Pts',(27.134044475447,-2.20998766023563,24.7154615801233));
#44578=CARTESIAN_POINT('Ctrl Pts',(27.0877406452841,-1.38798995378171,24.9461316548803));
#44579=CARTESIAN_POINT('Ctrl Pts',(27.0414368151212,-0.5659922473278,25.1768017296374));
#44580=CARTESIAN_POINT('Ctrl Pts',(26.9951329849583,0.314751243601958,25.1981299547686));
#44581=CARTESIAN_POINT('Ctrl Pts',(26.9488291547955,1.14695077853503,25.0075181847724));
#44582=CARTESIAN_POINT('Ctrl Pts',(26.9025253246326,1.9791503134681,24.8169064147761));
#44583=CARTESIAN_POINT('Ctrl Pts',(26.8562214944697,2.76280589240449,24.4143546496523));
#44584=CARTESIAN_POINT('Ctrl Pts',(26.8099176643068,3.40245475626642,23.8489006340471));
#44585=CARTESIAN_POINT('Ctrl Pts',(26.763613834144,4.04210362012837,23.2834466184419));
#44586=CARTESIAN_POINT('Ctrl Pts',(26.7173100039811,4.53774576891585,22.5550903523552));
#44587=CARTESIAN_POINT('Ctrl Pts',(26.6710061738182,4.82900344445263,21.752558185246));
#44588=CARTESIAN_POINT('Ctrl Pts',(26.6247023436553,5.1202611199894,20.9500260181369));
#44589=CARTESIAN_POINT('Ctrl Pts',(26.5783985134924,5.20713432227547,20.0733179500054));
#44590=CARTESIAN_POINT('Ctrl Pts',(26.5320946833296,5.07904039765143,19.2292321372598));
#44591=CARTESIAN_POINT('Ctrl Pts',(26.4857908531667,4.95094647302739,18.3851463245142));
#44592=CARTESIAN_POINT('Ctrl Pts',(26.4394870230038,4.60788542149324,17.5736827671547));
#44593=CARTESIAN_POINT('Ctrl Pts',(26.3931831928409,4.09164799320993,16.8936917154169));
#44594=CARTESIAN_POINT('Ctrl Pts',(26.346879362678,3.57541056492662,16.2137006636792));
#44595=CARTESIAN_POINT('Ctrl Pts',(26.3005755325152,2.88599675989413,15.6651821175633));
#44596=CARTESIAN_POINT('Ctrl Pts',(26.2542717023523,2.10738906447981,15.3149550919848));
#44597=CARTESIAN_POINT('Ctrl Pts',(26.2079678721894,1.32878136906554,14.9647280664063));
#44598=CARTESIAN_POINT('Ctrl Pts',(26.1616640420265,0.460979783269443,14.8127925613651));
#44599=CARTESIAN_POINT('Ctrl Pts',(26.1153602118637,-0.390302499588795,
14.8776569406157));
#44600=CARTESIAN_POINT('Ctrl Pts',(26.0690563817008,-1.24158478244708,14.9425213198662));
#44601=CARTESIAN_POINT('Ctrl Pts',(26.0227525515379,-2.07634776236751,15.2241855834085));
#44602=CARTESIAN_POINT('Ctrl Pts',(25.976448721375,-2.79290291778382,15.6883381682879));
#44603=CARTESIAN_POINT('Ctrl Pts',(25.9301448912121,-3.50945807320011,16.1524907531674));
#44604=CARTESIAN_POINT('Ctrl Pts',(25.8838410610492,-4.10780540411229,16.799131659384));
#44605=CARTESIAN_POINT('Ctrl Pts',(25.8375372308864,-4.51505589061035,17.549488877015));
#44606=CARTESIAN_POINT('Ctrl Pts',(25.7913719890253,-4.92108746815155,18.2976002602917));
#44607=CARTESIAN_POINT('Ctrl Pts',(25.7452067471642,-5.13716440285434,19.1488080340486));
#44608=CARTESIAN_POINT('Ctrl Pts',(25.6990415053031,-5.1371911776762,20.0000027150593));
#44609=CARTESIAN_POINT('Ctrl Pts',(26.1759584946969,-5.13631118199777,20.0000041318326));
#44610=CARTESIAN_POINT('Ctrl Pts',(26.199350705279,-5.13629909788329,19.5684857220737));
#44611=CARTESIAN_POINT('Ctrl Pts',(26.2227429158611,-5.08251203280468,19.1369643538796));
#44612=CARTESIAN_POINT('Ctrl Pts',(26.2461351264432,-4.97498580108714,18.7192771912869));
#44613=CARTESIAN_POINT('Ctrl Pts',(26.292438956606,-4.76214245504992,17.892484213769));
#44614=CARTESIAN_POINT('Ctrl Pts',(26.3387427867689,-4.33873602615698,17.1198970076177));
#44615=CARTESIAN_POINT('Ctrl Pts',(26.3850466169318,-3.75634471661833,16.4956300132962));
#44616=CARTESIAN_POINT('Ctrl Pts',(26.4313504470947,-3.17395340707964,15.8713630189747));
#44617=CARTESIAN_POINT('Ctrl Pts',(26.4776542772576,-2.43257721689522,15.395416236483));
#44618=CARTESIAN_POINT('Ctrl Pts',(26.5239581074204,-1.62252854673174,15.125768188851));
#44619=CARTESIAN_POINT('Ctrl Pts',(26.5702619375833,-0.812479876568274,
14.8561201412189));
#44620=CARTESIAN_POINT('Ctrl Pts',(26.6165657677462,0.0662412735742456,
14.7927708284465));
#44621=CARTESIAN_POINT('Ctrl Pts',(26.6628695979091,0.906591519194633,14.9434372889184));
#44622=CARTESIAN_POINT('Ctrl Pts',(26.709173428072,1.74694176481502,15.0941037493902));
#44623=CARTESIAN_POINT('Ctrl Pts',(26.7554772582348,2.54892110591328,15.4587859831063));
#44624=CARTESIAN_POINT('Ctrl Pts',(26.8017810883977,3.21483463329406,15.9930594071849));
#44625=CARTESIAN_POINT('Ctrl Pts',(26.8480849185606,3.88074816067483,16.5273328312634));
#44626=CARTESIAN_POINT('Ctrl Pts',(26.8943887487234,4.41059587433813,17.2311974457045));
#44627=CARTESIAN_POINT('Ctrl Pts',(26.9406925788863,4.73983318863067,18.0189104064349));
#44628=CARTESIAN_POINT('Ctrl Pts',(26.9869964090492,5.06907050292324,18.8066233671654));
#44629=CARTESIAN_POINT('Ctrl Pts',(27.0333002392121,5.19769741784503,19.6781846741854));
#44630=CARTESIAN_POINT('Ctrl Pts',(27.079604069375,5.11004495773869,20.5274231353155));
#44631=CARTESIAN_POINT('Ctrl Pts',(27.1259078995379,5.02239249763235,21.3766615964457));
#44632=CARTESIAN_POINT('Ctrl Pts',(27.1722117297007,4.71846066249789,22.2035772116861));
#44633=CARTESIAN_POINT('Ctrl Pts',(27.2185155598636,4.23527358938399,22.9074374037704));
#44634=CARTESIAN_POINT('Ctrl Pts',(27.2648193900265,3.7520865162701,23.6112975958547));
#44635=CARTESIAN_POINT('Ctrl Pts',(27.3111232201894,3.08964420517678,24.192102364783));
#44636=CARTESIAN_POINT('Ctrl Pts',(27.3574270503523,2.32864354954369,24.579099677114));
#44637=CARTESIAN_POINT('Ctrl Pts',(27.4037308805151,1.5676428939106,24.9660969894449));
#44638=CARTESIAN_POINT('Ctrl Pts',(27.450034710678,0.708083893737729,25.1592868451784));
#44639=CARTESIAN_POINT('Ctrl Pts',(27.4963385408409,-0.145324346679379,
25.1351353894556));
#44640=CARTESIAN_POINT('Ctrl Pts',(27.5426423710038,-0.998732587096511,
25.1109839337327));
#44641=CARTESIAN_POINT('Ctrl Pts',(27.5889462011667,-1.84599006775788,24.8694911665534));
#44642=CARTESIAN_POINT('Ctrl Pts',(27.6352500313295,-2.58388622151231,24.4400750700923));
#44643=CARTESIAN_POINT('Ctrl Pts',(27.6815538614924,-3.32178237526671,24.0106589736313));
#44644=CARTESIAN_POINT('Ctrl Pts',(27.7278576916553,-3.95031720211417,23.3933195478886));
#44645=CARTESIAN_POINT('Ctrl Pts',(27.7741615218182,-4.3929243247327,22.6632593773323));
#44646=CARTESIAN_POINT('Ctrl Pts',(27.820465351981,-4.83553144735123,21.933199206776));
#44647=CARTESIAN_POINT('Ctrl Pts',(27.8667691821439,-5.09221086574084,21.0904182914061));
#44648=CARTESIAN_POINT('Ctrl Pts',(27.9130730123068,-5.13169460180429,20.2375818755491));
#44649=CARTESIAN_POINT('Ctrl Pts',(27.9173681731035,-5.13535712809314,20.1584724470961));
#44650=CARTESIAN_POINT('Ctrl Pts',(27.9216633339002,-5.13715079679223,20.0792764962122));
#44651=CARTESIAN_POINT('Ctrl Pts',(27.9259584946968,-5.13709288667488,20.0000779211054));
#44652=CARTESIAN_POINT('Origin',(25.,0.,20.));
#44653=CARTESIAN_POINT('',(29.6759584946968,-5.13655037571547,19.9998784050199));
#44654=CARTESIAN_POINT('',(29.1990415053031,-5.13683630912746,20.0001288548401));
#44655=CARTESIAN_POINT('',(25.,-5.13675,20.));
#44656=CARTESIAN_POINT('Ctrl Pts',(29.1990415053031,-5.13683630912746,20.0001288548401));
#44657=CARTESIAN_POINT('Ctrl Pts',(29.1898320044066,-5.13701109509047,20.1699675778401));
#44658=CARTESIAN_POINT('Ctrl Pts',(29.1806225035101,-5.1287533857283,20.3397893799859));
#44659=CARTESIAN_POINT('Ctrl Pts',(29.1714130026137,-5.11193684989818,20.5087593752073));
#44660=CARTESIAN_POINT('Ctrl Pts',(29.1251091724508,-5.0273861204115,21.3583122499286));
#44661=CARTESIAN_POINT('Ctrl Pts',(29.0788053422879,-4.7264759427746,22.1863322104349));
#44662=CARTESIAN_POINT('Ctrl Pts',(29.032501512125,-4.24586236406213,22.8919521511687));
#44663=CARTESIAN_POINT('Ctrl Pts',(28.9861976819621,-3.76524878534965,23.5975720919024));
#44664=CARTESIAN_POINT('Ctrl Pts',(28.9398938517992,-3.1049318055616,24.1807920128636));
#44665=CARTESIAN_POINT('Ctrl Pts',(28.8935900216364,-2.34534941614573,24.5705656734581));
#44666=CARTESIAN_POINT('Ctrl Pts',(28.8472861914735,-1.58576702672985,24.9603393340525));
#44667=CARTESIAN_POINT('Ctrl Pts',(28.8009823613106,-0.72691922768615,25.1566667342802));
#44668=CARTESIAN_POINT('Ctrl Pts',(28.7546785311478,0.126571513247889,25.1356318122742));
#44669=CARTESIAN_POINT('Ctrl Pts',(28.7083747009849,0.980062254181953,25.1145968902681));
#44670=CARTESIAN_POINT('Ctrl Pts',(28.662070870822,1.82819593700634,24.8761996460282));
#44671=CARTESIAN_POINT('Ctrl Pts',(28.6157670406591,2.56765525804144,24.449480973671));
#44672=CARTESIAN_POINT('Ctrl Pts',(28.5694632104962,3.30711457907652,24.0227623013138));
#44673=CARTESIAN_POINT('Ctrl Pts',(28.5231593803334,3.93789953832229,23.4077222008393));
#44674=CARTESIAN_POINT('Ctrl Pts',(28.4768555501705,4.38316965354029,22.6792831592595));
#44675=CARTESIAN_POINT('Ctrl Pts',(28.4305517200076,4.82843976875827,21.9508441176798));
#44676=CARTESIAN_POINT('Ctrl Pts',(28.3842478898447,5.08819503994849,21.1090061349946));
#44677=CARTESIAN_POINT('Ctrl Pts',(28.3379440596818,5.13079279711745,20.2563195900744));
#44678=CARTESIAN_POINT('Ctrl Pts',(28.2916402295189,5.17339055428642,19.403633045154));
#44679=CARTESIAN_POINT('Ctrl Pts',(28.2453363993561,4.99883079743415,18.5400979379986));
#44680=CARTESIAN_POINT('Ctrl Pts',(28.1990325691932,4.62837791420866,17.7709077312786));
#44681=CARTESIAN_POINT('Ctrl Pts',(28.1527287390303,4.25792503098319,17.0017175245586));
#44682=CARTESIAN_POINT('Ctrl Pts',(28.1064249088674,3.69157902138449,16.3268722182742));
#44683=CARTESIAN_POINT('Ctrl Pts',(28.0601210787046,2.99833059271081,15.8285796044965));
#44684=CARTESIAN_POINT('Ctrl Pts',(28.0138172485417,2.30508216403714,15.3302869907188));
#44685=CARTESIAN_POINT('Ctrl Pts',(27.9675134183788,1.48493131628847,15.0085470694478));
#44686=CARTESIAN_POINT('Ctrl Pts',(27.9212095882159,0.637786561431619,14.9025533096201));
#44687=CARTESIAN_POINT('Ctrl Pts',(27.8749057580531,-0.209358193425278,
14.7965595497923));
#44688=CARTESIAN_POINT('Ctrl Pts',(27.8286019278902,-1.08349685539034,14.9063119514078));
#44689=CARTESIAN_POINT('Ctrl Pts',(27.7822980977273,-1.87814426602063,15.2184407799106));
#44690=CARTESIAN_POINT('Ctrl Pts',(27.7359942675644,-2.6727916766509,15.5305696084134));
#44691=CARTESIAN_POINT('Ctrl Pts',(27.6896904374015,-3.38794783594639,16.0450748638036));
#44692=CARTESIAN_POINT('Ctrl Pts',(27.6433866072387,-3.93649439501402,16.6992809363365));
#44693=CARTESIAN_POINT('Ctrl Pts',(27.5970827770758,-4.48504095408165,17.3534870088695));
#44694=CARTESIAN_POINT('Ctrl Pts',(27.5507789469129,-4.8669779129214,18.1473938985452));
#44695=CARTESIAN_POINT('Ctrl Pts',(27.50447511675,-5.03577876567455,18.984290059914));
#44696=CARTESIAN_POINT('Ctrl Pts',(27.4859972462677,-5.10313993824936,19.3182593843202));
#44697=CARTESIAN_POINT('Ctrl Pts',(27.4675193757854,-5.13655992343736,19.6590746014891));
#44698=CARTESIAN_POINT('Ctrl Pts',(27.4490415053031,-5.13638193362529,19.999924256499));
#44699=CARTESIAN_POINT('Ctrl Pts',(27.9259584946968,-5.13709288667488,20.0000779211054));
#44700=CARTESIAN_POINT('Ctrl Pts',(27.967967164063,-5.13652649880541,19.2254790379847));
#44701=CARTESIAN_POINT('Ctrl Pts',(28.0099758334292,-4.95884272242568,18.4506291282816));
#44702=CARTESIAN_POINT('Ctrl Pts',(28.0519845027954,-4.62020714167552,17.7540212374586));
#44703=CARTESIAN_POINT('Ctrl Pts',(28.0982883329583,-4.24694789174599,16.9861889315691));
#44704=CARTESIAN_POINT('Ctrl Pts',(28.1445921631212,-3.67814133814964,16.3134162361345));
#44705=CARTESIAN_POINT('Ctrl Pts',(28.1908959932841,-2.98307792486126,15.8176584634942));
#44706=CARTESIAN_POINT('Ctrl Pts',(28.237199823447,-2.28801451157289,15.3219006908538));
#44707=CARTESIAN_POINT('Ctrl Pts',(28.2835036536098,-1.46669423859254,15.0031578410078));
#44708=CARTESIAN_POINT('Ctrl Pts',(28.3298074837727,-0.619168074040091,
14.9002582879261));
#44709=CARTESIAN_POINT('Ctrl Pts',(28.3761113139356,0.228358090512335,14.7973587348444));
#44710=CARTESIAN_POINT('Ctrl Pts',(28.4224151440985,1.10209014663687,14.9103024785271));
#44711=CARTESIAN_POINT('Ctrl Pts',(28.4687189742614,1.89559246749136,15.2253310239382));
#44712=CARTESIAN_POINT('Ctrl Pts',(28.5150228044242,2.68909478834583,15.5403595693494));
#44713=CARTESIAN_POINT('Ctrl Pts',(28.5613266345871,3.40236737393034,16.0574729164892));
#44714=CARTESIAN_POINT('Ctrl Pts',(28.60763046475,3.948521327101,16.7136777450765));
#44715=CARTESIAN_POINT('Ctrl Pts',(28.6539342949129,4.49467528027171,17.369882573664));
#44716=CARTESIAN_POINT('Ctrl Pts',(28.7002381250758,4.87371060102853,18.1651788836989));
#44717=CARTESIAN_POINT('Ctrl Pts',(28.7465419552386,5.03945425305308,19.0026858743796));
#44718=CARTESIAN_POINT('Ctrl Pts',(28.7928457854015,5.20519790507761,19.8401928650602));
#44719=CARTESIAN_POINT('Ctrl Pts',(28.8391496155644,5.15764988836987,20.7199105363865));
#44720=CARTESIAN_POINT('Ctrl Pts',(28.8854534457272,4.90260237105269,21.5346741103978));
#44721=CARTESIAN_POINT('Ctrl Pts',(28.9317572758901,4.6475548537355,22.3494376844091));
#44722=CARTESIAN_POINT('Ctrl Pts',(28.978061106053,4.18500783580885,23.0992471611055));
#44723=CARTESIAN_POINT('Ctrl Pts',(29.0243649362159,3.57130751797791,23.6927628201404));
#44724=CARTESIAN_POINT('Ctrl Pts',(29.0706687663788,2.95760720014698,24.2862784791752));
#44725=CARTESIAN_POINT('Ctrl Pts',(29.1169725965417,2.19275358241176,24.7235003205486));
#44726=CARTESIAN_POINT('Ctrl Pts',(29.1632764267045,1.36991902084573,24.9511671866442));
#44727=CARTESIAN_POINT('Ctrl Pts',(29.2095802568674,0.547084459279668,25.1788340527397));
#44728=CARTESIAN_POINT('Ctrl Pts',(29.2558840870303,-0.333731046117226,
25.1969459435576));
#44729=CARTESIAN_POINT('Ctrl Pts',(29.3021879171932,-1.16522898226883,25.0032965185623));
#44730=CARTESIAN_POINT('Ctrl Pts',(29.348491747356,-1.99672691842042,24.809647093567));
#44731=CARTESIAN_POINT('Ctrl Pts',(29.3947955775189,-2.77890728532674,24.4042363527586));
#44732=CARTESIAN_POINT('Ctrl Pts',(29.4410994076818,-3.41648703016668,23.8364503133078));
#44733=CARTESIAN_POINT('Ctrl Pts',(29.4874032378447,-4.05406677500665,23.268664273857));
#44734=CARTESIAN_POINT('Ctrl Pts',(29.5337070680076,-4.54704589778025,22.5385029357639));
#44735=CARTESIAN_POINT('Ctrl Pts',(29.5800108981704,-4.83537104278805,21.7349125373757));
#44736=CARTESIAN_POINT('Ctrl Pts',(29.6119934303459,-5.03452018865289,21.1798643765229));
#44737=CARTESIAN_POINT('Ctrl Pts',(29.6439759625214,-5.13603286926705,20.5897846273661));
#44738=CARTESIAN_POINT('Ctrl Pts',(29.6759584946968,-5.13655037571547,19.9998784050199));
#44739=CARTESIAN_POINT('Origin',(25.,0.,20.));
#44740=CARTESIAN_POINT('',(31.4259584946968,-5.13659957288456,20.0001275332863));
#44741=CARTESIAN_POINT('',(30.9490415053031,-5.1368247808178,19.9998702638696));
#44742=CARTESIAN_POINT('',(25.,-5.13675,20.));
#44743=CARTESIAN_POINT('Ctrl Pts',(30.9490415053031,-5.1368247808178,19.9998702638696));
#44744=CARTESIAN_POINT('Ctrl Pts',(30.9121446330278,-5.13612325801613,20.6803151941057));
#44745=CARTESIAN_POINT('Ctrl Pts',(30.8752477607525,-5.0001139989638,21.3610321796951));
#44746=CARTESIAN_POINT('Ctrl Pts',(30.8383508884773,-4.7368068132147,21.9883147822946));
#44747=CARTESIAN_POINT('Ctrl Pts',(30.7920470583144,-4.4063687446805,22.7755247896416));
#44748=CARTESIAN_POINT('Ctrl Pts',(30.7457432281516,-3.87544836617376,23.4785806492208));
#44749=CARTESIAN_POINT('Ctrl Pts',(30.6994393979887,-3.20872093241755,24.0118380372435));
#44750=CARTESIAN_POINT('Ctrl Pts',(30.6531355678258,-2.54199349866135,24.5450954252662));
#44751=CARTESIAN_POINT('Ctrl Pts',(30.6068317376629,-1.73945900965567,24.9085543417324));
#44752=CARTESIAN_POINT('Ctrl Pts',(30.5605279075,-0.898880001181268,25.0579392248904));
#44753=CARTESIAN_POINT('Ctrl Pts',(30.5142240773371,-0.0583009927068438,
25.2073241080484));
#44754=CARTESIAN_POINT('Ctrl Pts',(30.4679202471743,0.820322535236316,25.1426349578981));
#44755=CARTESIAN_POINT('Ctrl Pts',(30.4216164170114,1.6299590902138,24.8717520281145));
#44756=CARTESIAN_POINT('Ctrl Pts',(30.3753125868485,2.43959564519129,24.6008690983309));
#44757=CARTESIAN_POINT('Ctrl Pts',(30.3290087566856,3.18024522720312,24.1237923889139));
#44758=CARTESIAN_POINT('Ctrl Pts',(30.2827049265227,3.76168394898414,23.4986380674719));
#44759=CARTESIAN_POINT('Ctrl Pts',(30.2364010963599,4.34312267076514,22.8734837460299));
#44760=CARTESIAN_POINT('Ctrl Pts',(30.190097266197,4.76535053231536,22.1002518125629));
#44761=CARTESIAN_POINT('Ctrl Pts',(30.1437934360341,4.97693290124465,21.2731352464357));
#44762=CARTESIAN_POINT('Ctrl Pts',(30.0974896058712,5.18851527017395,20.4460186803083));
#44763=CARTESIAN_POINT('Ctrl Pts',(30.0511857757083,5.18945214648229,19.5650174815208));
#44764=CARTESIAN_POINT('Ctrl Pts',(30.0048819455455,4.97962940248438,18.7374527838052));
#44765=CARTESIAN_POINT('Ctrl Pts',(29.9585781153826,4.76980665848647,17.9098880860896));
#44766=CARTESIAN_POINT('Ctrl Pts',(29.9122742852197,4.3492242941823,17.135759889446));
#44767=CARTESIAN_POINT('Ctrl Pts',(29.8659704550569,3.76911649203047,16.5093703535448));
#44768=CARTESIAN_POINT('Ctrl Pts',(29.819666624894,3.18900868987863,15.8829808176436));
#44769=CARTESIAN_POINT('Ctrl Pts',(29.7733627947311,2.4493754498791,15.4043299424848));
#44770=CARTESIAN_POINT('Ctrl Pts',(29.7270589645682,1.64031685131906,15.1317256562015));
#44771=CARTESIAN_POINT('Ctrl Pts',(29.6807551344053,0.831258252759049,14.8591213699182));
#44772=CARTESIAN_POINT('Ctrl Pts',(29.6344513042424,-0.0472257043614852,
14.7925636725103));
#44773=CARTESIAN_POINT('Ctrl Pts',(29.5881474740796,-0.888120529740423,
14.9401604389208));
#44774=CARTESIAN_POINT('Ctrl Pts',(29.5418436439167,-1.72901535511936,15.0877572053314));
#44775=CARTESIAN_POINT('Ctrl Pts',(29.4955398137538,-2.53232104875672,15.4495084355604));
#44776=CARTESIAN_POINT('Ctrl Pts',(29.4492359835909,-3.20018112885267,15.9813465934789));
#44777=CARTESIAN_POINT('Ctrl Pts',(29.402932153428,-3.86804120894865,16.5131847513974));
#44778=CARTESIAN_POINT('Ctrl Pts',(29.3566283232652,-4.40045567550322,17.2151098370055));
#44779=CARTESIAN_POINT('Ctrl Pts',(29.3103244931023,-4.73256726811228,18.0016152742776));
#44780=CARTESIAN_POINT('Ctrl Pts',(29.2732301638359,-4.99862423847722,18.6316904010514));
#44781=CARTESIAN_POINT('Ctrl Pts',(29.2361358345695,-5.13613230050249,19.3160468851478));
#44782=CARTESIAN_POINT('Ctrl Pts',(29.1990415053031,-5.13683630912746,20.0001288548401));
#44783=CARTESIAN_POINT('Ctrl Pts',(29.6759584946968,-5.13655037571547,19.9998784050199));
#44784=CARTESIAN_POINT('Ctrl Pts',(29.6902797926843,-5.13678210733751,19.735727250618));
#44785=CARTESIAN_POINT('Ctrl Pts',(29.7046010906717,-5.11676315508257,19.4716108903201));
#44786=CARTESIAN_POINT('Ctrl Pts',(29.7189223886591,-5.0761919539234,19.210690250472));
#44787=CARTESIAN_POINT('Ctrl Pts',(29.765226218822,-4.94501655280897,18.3670778206395));
#44788=CARTESIAN_POINT('Ctrl Pts',(29.8115300489848,-4.59899458333809,17.5568724196578));
#44789=CARTESIAN_POINT('Ctrl Pts',(29.8578338791477,-4.08027748652016,16.8787710326262));
#44790=CARTESIAN_POINT('Ctrl Pts',(29.9041377093106,-3.56156038970222,16.2006696455946));
#44791=CARTESIAN_POINT('Ctrl Pts',(29.9504415394735,-2.87014816553721,15.6546722725132));
#44792=CARTESIAN_POINT('Ctrl Pts',(29.9967453696363,-2.09026674229388,15.307290805959));
#44793=CARTESIAN_POINT('Ctrl Pts',(30.0430491997992,-1.31038531905059,14.9599093394048));
#44794=CARTESIAN_POINT('Ctrl Pts',(30.0893530299621,-0.442034696728981,
14.8111437793778));
#44795=CARTESIAN_POINT('Ctrl Pts',(30.135656860125,0.409005049237525,14.8791163356824));
#44796=CARTESIAN_POINT('Ctrl Pts',(30.1819606902879,1.26004479520408,14.947088891987));
#44797=CARTESIAN_POINT('Ctrl Pts',(30.2282645204507,2.09377366481553,15.2317995646233));
#44798=CARTESIAN_POINT('Ctrl Pts',(30.2745683506136,2.80862910896845,15.6985656854914));
#44799=CARTESIAN_POINT('Ctrl Pts',(30.3208721807765,3.52348455312135,16.1653318063596));
#44800=CARTESIAN_POINT('Ctrl Pts',(30.3671760109394,4.11946657181572,16.8141533754597));
#44801=CARTESIAN_POINT('Ctrl Pts',(30.4134798411023,4.52397428094567,17.565992740537));
#44802=CARTESIAN_POINT('Ctrl Pts',(30.4597836712652,4.92848199007563,18.3178321056142));
#44803=CARTESIAN_POINT('Ctrl Pts',(30.506087501428,5.14151538964116,19.1726892666687));
#44804=CARTESIAN_POINT('Ctrl Pts',(30.5523913315909,5.13712333905848,20.0264278844652));
#44805=CARTESIAN_POINT('Ctrl Pts',(30.5986951617538,5.13273128847581,20.8801665022617));
#44806=CARTESIAN_POINT('Ctrl Pts',(30.6449989919167,4.91091378774491,21.7327865768002));
#44807=CARTESIAN_POINT('Ctrl Pts',(30.6913028220795,4.49869203240205,22.4804242845487));
#44808=CARTESIAN_POINT('Ctrl Pts',(30.7376066522424,4.08647027705919,23.2280619922972));
#44809=CARTESIAN_POINT('Ctrl Pts',(30.7839104824053,3.48384426710438,23.8707173332557));
#44810=CARTESIAN_POINT('Ctrl Pts',(30.8302143125682,2.76422423931584,24.3301038080577));
#44811=CARTESIAN_POINT('Ctrl Pts',(30.876518142731,2.04460421152731,24.7894902828596));
#44812=CARTESIAN_POINT('Ctrl Pts',(30.9228219728939,1.20799016590505,25.0656078915051));
#44813=CARTESIAN_POINT('Ctrl Pts',(30.9691258030568,0.356296115728621,25.1248207492256));
#44814=CARTESIAN_POINT('Ctrl Pts',(31.0154296332197,-0.495397934447808,
25.1840336069461));
#44815=CARTESIAN_POINT('Ctrl Pts',(31.0617334633826,-1.36217198917841,25.0263417137417));
#44816=CARTESIAN_POINT('Ctrl Pts',(31.1080372935454,-2.13843802614104,24.6709546606803));
#44817=CARTESIAN_POINT('Ctrl Pts',(31.1543411237083,-2.91470406310367,24.3155676076188));
#44818=CARTESIAN_POINT('Ctrl Pts',(31.2006449538712,-3.60046208229834,23.7624853947004));
#44819=CARTESIAN_POINT('Ctrl Pts',(31.2469487840341,-4.11217493509543,23.0790829701308));
#44820=CARTESIAN_POINT('Ctrl Pts',(31.293252614197,-4.62388778789254,22.3956805455612));
#44821=CARTESIAN_POINT('Ctrl Pts',(31.3395564443598,-4.96155547429207,21.5819579093403));
#44822=CARTESIAN_POINT('Ctrl Pts',(31.3858602745227,-5.08404424898353,20.7370405064541));
#44823=CARTESIAN_POINT('Ctrl Pts',(31.3992263479141,-5.11940188454817,20.4931464705417));
#44824=CARTESIAN_POINT('Ctrl Pts',(31.4125924213055,-5.13682979808384,20.2466531395095));
#44825=CARTESIAN_POINT('Ctrl Pts',(31.4259584946968,-5.13659957288456,20.0001275332863));
#44826=CARTESIAN_POINT('Origin',(25.,0.,20.));
#44827=CARTESIAN_POINT('',(33.1759584946969,-5.13705066379934,19.9999081473515));
#44828=CARTESIAN_POINT('',(32.6990415053031,-5.13638791342383,20.0000785319455));
#44829=CARTESIAN_POINT('',(25.,-5.13675,20.));
#44830=CARTESIAN_POINT('Ctrl Pts',(32.6990415053031,-5.13638791342383,20.0000785319455));
#44831=CARTESIAN_POINT('Ctrl Pts',(32.6807610918119,-5.13657075558928,20.3372846981639));
#44832=CARTESIAN_POINT('Ctrl Pts',(32.6624806783207,-5.10386611251029,20.6744558642531));
#44833=CARTESIAN_POINT('Ctrl Pts',(32.6442002648296,-5.03792763082465,21.0049973362063));
#44834=CARTESIAN_POINT('Ctrl Pts',(32.5978964346667,-4.87090710589811,21.842250617512));
#44835=CARTESIAN_POINT('Ctrl Pts',(32.5515926045038,-4.49065952554585,22.6369680312125));
#44836=CARTESIAN_POINT('Ctrl Pts',(32.5052887743409,-3.94350560020336,23.2923392960588));
#44837=CARTESIAN_POINT('Ctrl Pts',(32.458984944178,-3.39635167486089,23.9477105609051));
#44838=CARTESIAN_POINT('Ctrl Pts',(32.4126811140152,-2.68229140452821,24.4637356768973));
#44839=CARTESIAN_POINT('Ctrl Pts',(32.3663772838523,-1.88830963993053,24.7775538890685));
#44840=CARTESIAN_POINT('Ctrl Pts',(32.3200734536894,-1.09432787533286,25.0913721012397));
#44841=CARTESIAN_POINT('Ctrl Pts',(32.2737696235265,-0.220424616470207,
25.2029834095897));
#44842=CARTESIAN_POINT('Ctrl Pts',(32.2274657933636,0.626943654370524,25.0987916326766));
#44843=CARTESIAN_POINT('Ctrl Pts',(32.1811619632008,1.47431192521126,24.9945998557634));
#44844=CARTESIAN_POINT('Ctrl Pts',(32.1348581330379,2.29514520803006,24.674604993587));
#44845=CARTESIAN_POINT('Ctrl Pts',(32.088554302875,2.98945185850394,24.1777879368029));
#44846=CARTESIAN_POINT('Ctrl Pts',(32.0422504727122,3.68375850897784,23.6809708800187));
#44847=CARTESIAN_POINT('Ctrl Pts',(31.9959466425492,4.2515385271068,23.0073316286267));
#44848=CARTESIAN_POINT('Ctrl Pts',(31.9496428123864,4.62362651863257,22.2389310564209));
#44849=CARTESIAN_POINT('Ctrl Pts',(31.9033389822235,4.99571451015832,21.470530484215));
#44850=CARTESIAN_POINT('Ctrl Pts',(31.8570351520606,5.1721104750809,20.6073685911953));
#44851=CARTESIAN_POINT('Ctrl Pts',(31.8107313218978,5.1313263439546,19.7545933761168));
#44852=CARTESIAN_POINT('Ctrl Pts',(31.7644274917349,5.0905422128283,18.9018181610383));
#44853=CARTESIAN_POINT('Ctrl Pts',(31.718123661572,4.83257798565312,18.059429623901));
#44854=CARTESIAN_POINT('Ctrl Pts',(31.6718198314091,4.38885815238538,17.3300452105984));
#44855=CARTESIAN_POINT('Ctrl Pts',(31.6255160012462,3.94513831911763,16.6006607972957));
#44856=CARTESIAN_POINT('Ctrl Pts',(31.5792121710834,3.31566287975732,15.9842805078278));
#44857=CARTESIAN_POINT('Ctrl Pts',(31.5329083409205,2.57711279444588,15.5559900873297));
#44858=CARTESIAN_POINT('Ctrl Pts',(31.4866045107576,1.83856270913447,15.1276996668317));
#44859=CARTESIAN_POINT('Ctrl Pts',(31.4403006805947,0.990937977871945,14.8874991153034));
#44860=CARTESIAN_POINT('Ctrl Pts',(31.3939968504318,0.137493905263782,14.8646490007767));
#44861=CARTESIAN_POINT('Ctrl Pts',(31.3476930202689,-0.71595016734443,14.84179888625));
#44862=CARTESIAN_POINT('Ctrl Pts',(31.3013891901061,-1.57521358129828,15.0362992087248));
#44863=CARTESIAN_POINT('Ctrl Pts',(31.2550853599432,-2.33562323979935,15.4244564759018));
#44864=CARTESIAN_POINT('Ctrl Pts',(31.2087815297803,-3.09603289830041,15.8126137430787));
#44865=CARTESIAN_POINT('Ctrl Pts',(31.1624776996174,-3.7575888013487,16.3944279549576));
#44866=CARTESIAN_POINT('Ctrl Pts',(31.1161738694545,-4.23970203528538,17.099024110544));
#44867=CARTESIAN_POINT('Ctrl Pts',(31.0698700392917,-4.72181526922206,17.8036202661303));
#44868=CARTESIAN_POINT('Ctrl Pts',(31.0235662091288,-5.02448583404714,18.630998365424));
#44869=CARTESIAN_POINT('Ctrl Pts',(30.9772623789659,-5.11084323717886,19.4803694926283));
#44870=CARTESIAN_POINT('Ctrl Pts',(30.9678554210783,-5.12838736801396,19.6529253783177));
#44871=CARTESIAN_POINT('Ctrl Pts',(30.9584484631907,-5.13700363596311,19.8263889791738));
#44872=CARTESIAN_POINT('Ctrl Pts',(30.9490415053031,-5.1368247808178,19.9998702638696));
#44873=CARTESIAN_POINT('Ctrl Pts',(31.4259584946968,-5.13659957288456,20.0001275332863));
#44874=CARTESIAN_POINT('Ctrl Pts',(31.4588962514683,-5.13603223336795,19.3926192383697));
#44875=CARTESIAN_POINT('Ctrl Pts',(31.4918340082398,-5.02823267856117,18.7849149465654));
#44876=CARTESIAN_POINT('Ctrl Pts',(31.5247717650114,-4.81726509452241,18.215429563488));
#44877=CARTESIAN_POINT('Ctrl Pts',(31.5710755951742,-4.52068730238642,17.4148481929596));
#44878=CARTESIAN_POINT('Ctrl Pts',(31.6173794253371,-4.02022185513104,16.6897976214544));
#44879=CARTESIAN_POINT('Ctrl Pts',(31.6636832555,-3.3768340718355,16.128601507844));
#44880=CARTESIAN_POINT('Ctrl Pts',(31.7099870856629,-2.73344628853994,15.5674053942336));
#44881=CARTESIAN_POINT('Ctrl Pts',(31.7562909158257,-1.94713616920423,15.170063738518));
#44882=CARTESIAN_POINT('Ctrl Pts',(31.8025947459886,-1.11368984168881,14.9849796041994));
#44883=CARTESIAN_POINT('Ctrl Pts',(31.8488985761515,-0.28024351417343,14.7998954698808));
#44884=CARTESIAN_POINT('Ctrl Pts',(31.8952024063144,0.600339021521638,14.8270688569593));
#44885=CARTESIAN_POINT('Ctrl Pts',(31.9415062364773,1.4207876320462,15.0631895784423));
#44886=CARTESIAN_POINT('Ctrl Pts',(31.9878100666401,2.24123624257079,15.2993102999252));
#44887=CARTESIAN_POINT('Ctrl Pts',(32.034113896803,3.00155092792492,15.7443783558127));
#44888=CARTESIAN_POINT('Ctrl Pts',(32.0804177269659,3.60911225224641,16.3441767842986));
#44889=CARTESIAN_POINT('Ctrl Pts',(32.1267215571288,4.21667357656793,16.9439752127844));
#44890=CARTESIAN_POINT('Ctrl Pts',(32.1730253872917,4.67148153985684,17.6985040138686));
#44891=CARTESIAN_POINT('Ctrl Pts',(32.2193292174545,4.91813269167768,18.515848572137));
#44892=CARTESIAN_POINT('Ctrl Pts',(32.2656330476174,5.16478384349852,19.3331931304053));
#44893=CARTESIAN_POINT('Ctrl Pts',(32.3119368777803,5.20327818385128,20.2133534458577));
#44894=CARTESIAN_POINT('Ctrl Pts',(32.3582407079432,5.02892643847093,21.0491108188484));
#44895=CARTESIAN_POINT('Ctrl Pts',(32.4045445381061,4.85457469309059,21.884868191839));
#44896=CARTESIAN_POINT('Ctrl Pts',(32.4508483682689,4.46737686197716,22.6762226223678));
#44897=CARTESIAN_POINT('Ctrl Pts',(32.4971521984318,3.91450031592533,23.3267734985113));
#44898=CARTESIAN_POINT('Ctrl Pts',(32.5434560285947,3.36162376987346,23.9773243746549));
#44899=CARTESIAN_POINT('Ctrl Pts',(32.5897598587576,2.64306850888318,24.4870716964132));
#44900=CARTESIAN_POINT('Ctrl Pts',(32.6360636889204,1.84636695103165,24.7939194523808));
#44901=CARTESIAN_POINT('Ctrl Pts',(32.6823675190833,1.04966539318013,25.1007672083484));
#44902=CARTESIAN_POINT('Ctrl Pts',(32.7286713492462,0.174817538467357,25.2047153985253));
#44903=CARTESIAN_POINT('Ctrl Pts',(32.7749751794091,-0.671605062761131,
25.0931013413686));
#44904=CARTESIAN_POINT('Ctrl Pts',(32.821279009572,-1.51802766398958,24.9814872842118));
#44905=CARTESIAN_POINT('Ctrl Pts',(32.8675828397349,-2.33602501173377,24.6543109797215));
#44906=CARTESIAN_POINT('Ctrl Pts',(32.9138866698977,-3.02595092745193,24.1514281420289));
#44907=CARTESIAN_POINT('Ctrl Pts',(32.9601905000606,-3.71587684317011,23.6485453043363));
#44908=CARTESIAN_POINT('Ctrl Pts',(33.0064943302235,-4.27773132686224,22.9699559334413));
#44909=CARTESIAN_POINT('Ctrl Pts',(33.0527981603863,-4.64307081651572,22.1983239130293));
#44910=CARTESIAN_POINT('Ctrl Pts',(33.0938516051565,-4.96698450806331,21.5141871489335));
#44911=CARTESIAN_POINT('Ctrl Pts',(33.1349050499267,-5.1364221807677,20.7569116497994));
#44912=CARTESIAN_POINT('Ctrl Pts',(33.1759584946969,-5.13705066379934,19.9999081473515));
#44913=CARTESIAN_POINT('Origin',(25.,0.,20.));
#44914=CARTESIAN_POINT('',(34.9259584946969,-5.13631268534711,20.0000122781576));
#44915=CARTESIAN_POINT('',(34.4490415053031,-5.13719091754074,19.9999934144287));
#44916=CARTESIAN_POINT('',(25.,-5.13675,20.));
#44917=CARTESIAN_POINT('Ctrl Pts',(34.4490415053031,-5.13719058367308,19.9999934194154));
#44918=CARTESIAN_POINT('Ctrl Pts',(34.4030737204331,-5.1371267473639,20.847547674618));
#44919=CARTESIAN_POINT('Ctrl Pts',(34.3571059355632,-4.92296721330138,21.6951330054991));
#44920=CARTESIAN_POINT('Ctrl Pts',(34.3111381506932,-4.52025752915113,22.4409027693378));
#44921=CARTESIAN_POINT('Ctrl Pts',(34.2648343205303,-4.11460385511416,23.1921244473692));
#44922=CARTESIAN_POINT('Ctrl Pts',(34.2185304903674,-3.51763318064836,23.840036481391));
#44923=CARTESIAN_POINT('Ctrl Pts',(34.1722266602046,-2.80206682517619,24.3057120162007));
#44924=CARTESIAN_POINT('Ctrl Pts',(34.1259228300417,-2.08650046970406,24.7713875510104));
#44925=CARTESIAN_POINT('Ctrl Pts',(34.0796189998788,-1.25233843322558,25.0548265866079));
#44926=CARTESIAN_POINT('Ctrl Pts',(34.0333151697159,-0.401196032035998,
25.1215013622069));
#44927=CARTESIAN_POINT('Ctrl Pts',(33.9870113395531,0.449946369153583,25.1881761378058));
#44928=CARTESIAN_POINT('Ctrl Pts',(33.9407075093902,1.31806913505426,25.0380866534062));
#44929=CARTESIAN_POINT('Ctrl Pts',(33.8944036792273,2.09741994707273,24.6895163956244));
#44930=CARTESIAN_POINT('Ctrl Pts',(33.8480998490644,2.87677075909122,24.3409461378425));
#44931=CARTESIAN_POINT('Ctrl Pts',(33.8017960189015,3.56734961722749,23.7938951066785));
#44932=CARTESIAN_POINT('Ctrl Pts',(33.7554921887387,4.08503211156166,23.1150035484279));
#44933=CARTESIAN_POINT('Ctrl Pts',(33.7091883585758,4.60271460589581,22.4361119901773));
#44934=CARTESIAN_POINT('Ctrl Pts',(33.6628845284129,4.94750073642786,21.6253799048401));
#44935=CARTESIAN_POINT('Ctrl Pts',(33.61658069825,5.07738960863597,20.7815684367499));
#44936=CARTESIAN_POINT('Ctrl Pts',(33.5702768680871,5.20727848084407,19.9377569686598));
#44937=CARTESIAN_POINT('Ctrl Pts',(33.5239730379243,5.12227009472827,19.0608661178167));
#44938=CARTESIAN_POINT('Ctrl Pts',(33.4776692077614,4.83271993719056,18.2577163067143));
#44939=CARTESIAN_POINT('Ctrl Pts',(33.4313653775985,4.54316977965285,17.4545664956119));
#44940=CARTESIAN_POINT('Ctrl Pts',(33.3850615474356,4.04907785069323,16.7251577242503));
#44941=CARTESIAN_POINT('Ctrl Pts',(33.3387577172727,3.41063306498843,16.1583445553751));
#44942=CARTESIAN_POINT('Ctrl Pts',(33.2924538871099,2.77218827928362,15.5915313865));
#44943=CARTESIAN_POINT('Ctrl Pts',(33.246150056947,1.98939063683364,15.1873138201114));
#44944=CARTESIAN_POINT('Ctrl Pts',(33.1998462267841,1.15759838526208,14.9949325241664));
#44945=CARTESIAN_POINT('Ctrl Pts',(33.1535423966212,0.325806133690502,14.8025512282215));
#44946=CARTESIAN_POINT('Ctrl Pts',(33.1072385664583,-0.554980727002643,
14.8220062027202));
#44947=CARTESIAN_POINT('Ctrl Pts',(33.0609347362955,-1.37746717315998,15.0509274963813));
#44948=CARTESIAN_POINT('Ctrl Pts',(33.0146309061326,-2.19995361931729,15.2798487900423));
#44949=CARTESIAN_POINT('Ctrl Pts',(32.9683270759697,-2.9641396509388,15.7182364028657));
#44950=CARTESIAN_POINT('Ctrl Pts',(32.9220232458069,-3.57693423544831,16.3126871661756));
#44951=CARTESIAN_POINT('Ctrl Pts',(32.875719415644,-4.18972881995782,16.9071379294855));
#44952=CARTESIAN_POINT('Ctrl Pts',(32.8294155854811,-4.65113195735533,17.657651843282));
#44953=CARTESIAN_POINT('Ctrl Pts',(32.7831117553182,-4.90493679130367,18.4728033746358));
#44954=CARTESIAN_POINT('Ctrl Pts',(32.7550883386465,-5.05854133308798,18.9661390432695));
#44955=CARTESIAN_POINT('Ctrl Pts',(32.7270649219748,-5.13610762095725,19.4831499129748));
#44956=CARTESIAN_POINT('Ctrl Pts',(32.6990415053031,-5.13638791342383,20.0000785319455));
#44957=CARTESIAN_POINT('Ctrl Pts',(33.1759584946969,-5.13705066379934,19.9999081473515));
#44958=CARTESIAN_POINT('Ctrl Pts',(33.1812088800896,-5.13713104141801,19.9030938567668));
#44959=CARTESIAN_POINT('Ctrl Pts',(33.1864592654823,-5.13445033743313,19.8062840150219));
#44960=CARTESIAN_POINT('Ctrl Pts',(33.191709650875,-5.12897856940196,19.7096321843039));
#44961=CARTESIAN_POINT('Ctrl Pts',(33.2380134810379,-5.08072233701988,18.8572471459194));
#44962=CARTESIAN_POINT('Ctrl Pts',(33.2843173112007,-4.81538537664088,18.0171517390795));
#44963=CARTESIAN_POINT('Ctrl Pts',(33.3306211413636,-4.36529030422524,17.2916840668759));
#44964=CARTESIAN_POINT('Ctrl Pts',(33.3769249715265,-3.91519523180961,16.5662163946723));
#44965=CARTESIAN_POINT('Ctrl Pts',(33.4232288016894,-3.28034204735735,15.9553764571049));
#44966=CARTESIAN_POINT('Ctrl Pts',(33.4695326318523,-2.53806681306989,15.5335750889364));
#44967=CARTESIAN_POINT('Ctrl Pts',(33.5158364620152,-1.79579157878242,15.1117737207678));
#44968=CARTESIAN_POINT('Ctrl Pts',(33.562140292178,-0.946094294659754,14.8790109219982));
#44969=CARTESIAN_POINT('Ctrl Pts',(33.6084441223409,-0.0924827379748081,
14.8636412141524));
#44970=CARTESIAN_POINT('Ctrl Pts',(33.6547479525038,0.761128818710162,14.8482715063067));
#44971=CARTESIAN_POINT('Ctrl Pts',(33.7010517826667,1.61865464795741,15.050294889385));
#44972=CARTESIAN_POINT('Ctrl Pts',(33.7473556128296,2.37563332074029,15.4451014326151));
#44973=CARTESIAN_POINT('Ctrl Pts',(33.7936594429924,3.13261199352313,15.8399079758451));
#44974=CARTESIAN_POINT('Ctrl Pts',(33.8399632731553,3.78904350984162,16.4274976792269));
#44975=CARTESIAN_POINT('Ctrl Pts',(33.8862671033182,4.26496319468072,17.1362919873361));
#44976=CARTESIAN_POINT('Ctrl Pts',(33.9325709334811,4.74088287951985,17.8450862954453));
#44977=CARTESIAN_POINT('Ctrl Pts',(33.9788747636439,5.03629073287958,18.6750852082819));
#44978=CARTESIAN_POINT('Ctrl Pts',(34.0251785938068,5.11520098563766,19.525180549779));
#44979=CARTESIAN_POINT('Ctrl Pts',(34.0714824239697,5.19411123839575,20.3752758912761));
#44980=CARTESIAN_POINT('Ctrl Pts',(34.1177862541326,5.05652389055219,21.2454676614337));
#44981=CARTESIAN_POINT('Ctrl Pts',(34.1640900842955,4.71919945296453,22.029751501272));
#44982=CARTESIAN_POINT('Ctrl Pts',(34.2103939144583,4.38187501537688,22.8140353411103));
#44983=CARTESIAN_POINT('Ctrl Pts',(34.2566977446212,3.84481348804514,23.5124112506294));
#44984=CARTESIAN_POINT('Ctrl Pts',(34.3030015747841,3.17343822348752,24.0398050046363));
#44985=CARTESIAN_POINT('Ctrl Pts',(34.349305404947,2.50206295892989,24.5671987586433));
#44986=CARTESIAN_POINT('Ctrl Pts',(34.3956092351099,1.69637395714638,24.9236103571381));
#44987=CARTESIAN_POINT('Ctrl Pts',(34.4419130652727,0.854518027955203,25.0656227231878));
#44988=CARTESIAN_POINT('Ctrl Pts',(34.4882168954356,0.0126620987640046,
25.2076350892374));
#44989=CARTESIAN_POINT('Ctrl Pts',(34.5345207255985,-0.865360757834854,
25.135248222842));
#44990=CARTESIAN_POINT('Ctrl Pts',(34.5808245557613,-1.67259222153178,24.857280092217));
#44991=CARTESIAN_POINT('Ctrl Pts',(34.6271283859242,-2.47982368522869,24.5793119615921));
#44992=CARTESIAN_POINT('Ctrl Pts',(34.6734322160871,-3.21626375602367,24.0957625667378));
#44993=CARTESIAN_POINT('Ctrl Pts',(34.71973604625,-3.79220133768625,23.4655365599323));
#44994=CARTESIAN_POINT('Ctrl Pts',(34.7660398764129,-4.36813891934883,22.8353105531268));
#44995=CARTESIAN_POINT('Ctrl Pts',(34.8123437065758,-4.78357401187901,22.0584079343701));
#44996=CARTESIAN_POINT('Ctrl Pts',(34.8586475367386,-4.98789945925489,21.2294688357748));
#44997=CARTESIAN_POINT('Ctrl Pts',(34.8810845227247,-5.08690740704766,20.8277980695969));
#44998=CARTESIAN_POINT('Ctrl Pts',(34.9035215087108,-5.13634714026073,20.41390921932));
#44999=CARTESIAN_POINT('Ctrl Pts',(34.9259584946969,-5.13631268534711,20.0000122781576));
#45000=CARTESIAN_POINT('Origin',(25.,0.,20.));
#45001=CARTESIAN_POINT('',(36.6759584946969,-5.13711172348184,20.0000703967194));
#45002=CARTESIAN_POINT('',(36.1990415053031,-5.1363684901921,19.9999311527925));
#45003=CARTESIAN_POINT('',(25.,-5.13675,20.));
#45004=CARTESIAN_POINT('Ctrl Pts',(36.1990415053031,-5.1363684901921,19.9999311527925));
#45005=CARTESIAN_POINT('Ctrl Pts',(36.1716901792172,-5.13612980667983,20.5044676422258));
#45006=CARTESIAN_POINT('Ctrl Pts',(36.1443388531313,-5.06229487396435,21.0090724832292));
#45007=CARTESIAN_POINT('Ctrl Pts',(36.1169875270455,-4.91586386075298,21.4916490745987));
#45008=CARTESIAN_POINT('Ctrl Pts',(36.0706836968826,-4.66796667488968,22.3086165758158));
#45009=CARTESIAN_POINT('Ctrl Pts',(36.0243798667197,-4.21200870437187,23.0624509867601));
#45010=CARTESIAN_POINT('Ctrl Pts',(35.9780760365568,-3.60353349034068,23.661322280707));
#45011=CARTESIAN_POINT('Ctrl Pts',(35.931772206394,-2.99505827630949,24.2601935746539));
#45012=CARTESIAN_POINT('Ctrl Pts',(35.8854683762311,-2.23406581876493,24.7041017516034));
#45013=CARTESIAN_POINT('Ctrl Pts',(35.8391645460682,-1.41325811790606,24.9389711429994));
#45014=CARTESIAN_POINT('Ctrl Pts',(35.7928607159053,-0.592450417047175,
25.1738405343954));
#45015=CARTESIAN_POINT('Ctrl Pts',(35.7465568857425,0.288172527126009,25.1996711402378));
#45016=CARTESIAN_POINT('Ctrl Pts',(35.7002530555796,1.12133565881403,25.0133163474371));
#45017=CARTESIAN_POINT('Ctrl Pts',(35.6539492254167,1.95449879050203,24.8269615546364));
#45018=CARTESIAN_POINT('Ctrl Pts',(35.6076453952538,2.74020210970485,24.4284213631927));
#45019=CARTESIAN_POINT('Ctrl Pts',(35.5613415650909,3.38273340727898,23.8662448389215));
#45020=CARTESIAN_POINT('Ctrl Pts',(35.515037734928,4.02526470485311,23.3040683146503));
#45021=CARTESIAN_POINT('Ctrl Pts',(35.4687339047652,4.52462398079854,22.5782554575517));
#45022=CARTESIAN_POINT('Ctrl Pts',(35.4224300746023,4.81998066677103,21.7772227860237));
#45023=CARTESIAN_POINT('Ctrl Pts',(35.3761262444394,5.11533735274352,20.9761901144957));
#45024=CARTESIAN_POINT('Ctrl Pts',(35.3298224142765,5.20669144874308,20.0999376285383));
#45025=CARTESIAN_POINT('Ctrl Pts',(35.2835185841136,5.08291445100915,19.2552079867973));
#45026=CARTESIAN_POINT('Ctrl Pts',(35.2372147539508,4.95913745327523,18.4104783450563));
#45027=CARTESIAN_POINT('Ctrl Pts',(35.1909109237879,4.62022936180781,17.5972715475316));
#45028=CARTESIAN_POINT('Ctrl Pts',(35.144607093625,4.1074750246382,16.9146502011633));
#45029=CARTESIAN_POINT('Ctrl Pts',(35.0983032634622,3.59472068746857,16.232028854795));
#45030=CARTESIAN_POINT('Ctrl Pts',(35.0519994332993,2.90812010459674,15.679992959583));
#45031=CARTESIAN_POINT('Ctrl Pts',(35.0056956031364,2.13131306343327,15.3257900041989));
#45032=CARTESIAN_POINT('Ctrl Pts',(34.9593917729735,1.3545060222698,14.9715870488148));
#45033=CARTESIAN_POINT('Ctrl Pts',(34.9130879428106,0.487492522814696,14.8152170332586));
#45034=CARTESIAN_POINT('Ctrl Pts',(34.8667841126478,-0.364110244114622,
14.8757285211126));
#45035=CARTESIAN_POINT('Ctrl Pts',(34.8204802824849,-1.21571301104392,14.9362400089666));
#45036=CARTESIAN_POINT('Ctrl Pts',(34.774176452322,-2.05190504544742,15.2136330002308));
#45037=CARTESIAN_POINT('Ctrl Pts',(34.7278726221591,-2.77082374228716,15.6741162465473));
#45038=CARTESIAN_POINT('Ctrl Pts',(34.6815687919962,-3.48974243912691,16.1345994928638));
#45039=CARTESIAN_POINT('Ctrl Pts',(34.6352649618334,-4.09138779840288,16.7781729942326));
#45040=CARTESIAN_POINT('Ctrl Pts',(34.5889611316705,-4.50246904349511,17.5264384035209));
#45041=CARTESIAN_POINT('Ctrl Pts',(34.5426573015076,-4.91355028858735,18.2747038128091));
#45042=CARTESIAN_POINT('Ctrl Pts',(34.4963534713447,-5.13406741949585,19.1276611300169));
#45043=CARTESIAN_POINT('Ctrl Pts',(34.4500496411818,-5.13715764814602,19.9814054496412));
#45044=CARTESIAN_POINT('Ctrl Pts',(34.4497135958889,-5.13718007516315,19.9876014113782));
#45045=CARTESIAN_POINT('Ctrl Pts',(34.449377550596,-5.13719105034537,19.9937974145664));
#45046=CARTESIAN_POINT('Ctrl Pts',(34.4490415053031,-5.13719058367308,19.9999934194154));
#45047=CARTESIAN_POINT('Ctrl Pts',(34.9259584946969,-5.13631268534711,20.0000122781576));
#45048=CARTESIAN_POINT('Ctrl Pts',(34.9498253388737,-5.13627603470006,19.5597386243741));
#45049=CARTESIAN_POINT('Ctrl Pts',(34.9736921830504,-5.08025851475436,19.1194558156187));
#45050=CARTESIAN_POINT('Ctrl Pts',(34.9975590272272,-4.96837329816293,18.6938601132045));
#45051=CARTESIAN_POINT('Ctrl Pts',(35.0438628573901,-4.75130588747351,17.8681660676634));
#45052=CARTESIAN_POINT('Ctrl Pts',(35.090166687553,-4.32395526387306,17.0977535550153));
#45053=CARTESIAN_POINT('Ctrl Pts',(35.1364705177159,-3.73838010048158,16.4764721005646));
#45054=CARTESIAN_POINT('Ctrl Pts',(35.1827743478788,-3.15280493709009,15.8551906461138));
#45055=CARTESIAN_POINT('Ctrl Pts',(35.2290781780417,-2.40900523390756,15.3830402498605));
#45056=CARTESIAN_POINT('Ctrl Pts',(35.2753820082046,-1.59758861726315,15.1175369695442));
#45057=CARTESIAN_POINT('Ctrl Pts',(35.3216858383674,-0.786172000618762,
14.8520336892278));
#45058=CARTESIAN_POINT('Ctrl Pts',(35.3679896685303,0.0928615294875015,
14.7931775248485));
#45059=CARTESIAN_POINT('Ctrl Pts',(35.4142934986932,0.932430535289689,14.9481381718582));
#45060=CARTESIAN_POINT('Ctrl Pts',(35.460597328856,1.77199954109188,15.103098818868));
#45061=CARTESIAN_POINT('Ctrl Pts',(35.5069011590189,2.57210402259,15.4718762772669));
#45062=CARTESIAN_POINT('Ctrl Pts',(35.5532049891818,3.235277460809,16.0095470952086));
#45063=CARTESIAN_POINT('Ctrl Pts',(35.5995088193447,3.89845089902802,16.5472179131504));
#45064=CARTESIAN_POINT('Ctrl Pts',(35.6458126495076,4.4246932939679,17.2537820906349));
#45065=CARTESIAN_POINT('Ctrl Pts',(35.6921164796704,4.74989924994857,18.0431679302723));
#45066=CARTESIAN_POINT('Ctrl Pts',(35.7384203098333,5.07510520592925,18.8325537699098));
#45067=CARTESIAN_POINT('Ctrl Pts',(35.7847241399962,5.19927472295068,19.7047612717001));
#45068=CARTESIAN_POINT('Ctrl Pts',(35.8310279701591,5.10728181326158,20.5535405258011));
#45069=CARTESIAN_POINT('Ctrl Pts',(35.877331800322,5.01528890357248,21.4023197799021));
#45070=CARTESIAN_POINT('Ctrl Pts',(35.9236356304849,4.70713356717287,22.2276707863139));
#45071=CARTESIAN_POINT('Ctrl Pts',(35.9699394606477,4.22035443637511,22.9290515640981));
#45072=CARTESIAN_POINT('Ctrl Pts',(36.0162432908106,3.73357530557736,23.6304323418823));
#45073=CARTESIAN_POINT('Ctrl Pts',(36.0625471209735,3.06817238038148,24.2078428910389));
#45074=CARTESIAN_POINT('Ctrl Pts',(36.1088509511364,2.30520320806331,24.5909446526081));
#45075=CARTESIAN_POINT('Ctrl Pts',(36.1551547812992,1.54223403574514,24.9740464141774));
#45076=CARTESIAN_POINT('Ctrl Pts',(36.2014586114621,0.681698616304682,25.1628393881594));
#45077=CARTESIAN_POINT('Ctrl Pts',(36.247762441625,-0.171575001263084,25.134325335691));
#45078=CARTESIAN_POINT('Ctrl Pts',(36.2940662717879,-1.02484861883088,25.1058112832225));
#45079=CARTESIAN_POINT('Ctrl Pts',(36.3403701019507,-1.87086043452598,24.8599902043036));
#45080=CARTESIAN_POINT('Ctrl Pts',(36.3866739321136,-2.60655162466432,24.4268073440954));
#45081=CARTESIAN_POINT('Ctrl Pts',(36.4329777622765,-3.34224281480263,23.9936244838871));
#45082=CARTESIAN_POINT('Ctrl Pts',(36.4792815924394,-3.96761337938419,23.3730798423894));
#45083=CARTESIAN_POINT('Ctrl Pts',(36.5255854226023,-4.4064824027802,22.6407664546046));
#45084=CARTESIAN_POINT('Ctrl Pts',(36.5718892527651,-4.84535142617622,21.9084530668199));
#45085=CARTESIAN_POINT('Ctrl Pts',(36.618193082928,-5.09771890838669,21.064370932748));
#45086=CARTESIAN_POINT('Ctrl Pts',(36.6644969130909,-5.13284213947516,20.2113438075854));
#45087=CARTESIAN_POINT('Ctrl Pts',(36.6683174402929,-5.13574015588813,20.1409605731045));
#45088=CARTESIAN_POINT('Ctrl Pts',(36.6721379674949,-5.13715919655493,20.0705164420761));
#45089=CARTESIAN_POINT('Ctrl Pts',(36.6759584946969,-5.13711172348184,20.0000703967194));
#45090=CARTESIAN_POINT('Origin',(25.,0.,20.));
#45091=CARTESIAN_POINT('',(38.4259584946969,-5.13652713961075,19.9998820685162));
#45092=CARTESIAN_POINT('',(37.9490415053031,-5.13686389810347,20.0001263479959));
#45093=CARTESIAN_POINT('',(25.,-5.13675,20.));
#45094=CARTESIAN_POINT('Ctrl Pts',(37.9490415053031,-5.13686389810347,20.0001263479959));
#45095=CARTESIAN_POINT('Ctrl Pts',(37.9403066380013,-5.13702848944412,20.1612095334366));
#45096=CARTESIAN_POINT('Ctrl Pts',(37.9315717706995,-5.12960133194211,20.3222776015441));
#45097=CARTESIAN_POINT('Ctrl Pts',(37.9228369033977,-5.11447099711345,20.4826187717999));
#45098=CARTESIAN_POINT('Ctrl Pts',(37.8765330732349,-5.03426457496541,21.3325927964913));
#45099=CARTESIAN_POINT('Ctrl Pts',(37.830229243072,-4.73759144851179,22.1621402912393));
#45100=CARTESIAN_POINT('Ctrl Pts',(37.7839254129091,-4.26059151894989,22.8702080704821));
#45101=CARTESIAN_POINT('Ctrl Pts',(37.7376215827462,-3.78359158938799,23.5782758497249));
#45102=CARTESIAN_POINT('Ctrl Pts',(37.6913177525833,-3.12626485671779,24.1648639134627));
#45103=CARTESIAN_POINT('Ctrl Pts',(37.6450139224205,-2.36868504873878,24.5585157232469));
#45104=CARTESIAN_POINT('Ctrl Pts',(37.5987100922576,-1.61110524075978,24.9521675330312));
#45105=CARTESIAN_POINT('Ctrl Pts',(37.5524062620947,-0.753272357471954,
25.1528830888621));
#45106=CARTESIAN_POINT('Ctrl Pts',(37.5061024319319,0.100314767622557,25.1362117758719));
#45107=CARTESIAN_POINT('Ctrl Pts',(37.459798601769,0.953901892717081,25.1195404628817));
#45108=CARTESIAN_POINT('Ctrl Pts',(37.4134947716061,1.80324325961826,24.8854822810705));
#45109=CARTESIAN_POINT('Ctrl Pts',(37.3671909414432,2.54487444790653,24.4625495519491));
#45110=CARTESIAN_POINT('Ctrl Pts',(37.3208871112803,3.28650563619479,24.0396168228276));
#45111=CARTESIAN_POINT('Ctrl Pts',(37.2745832811174,3.92042664587011,23.427809546396));
#45112=CARTESIAN_POINT('Ctrl Pts',(37.2282794509546,4.36941496968878,22.7016563959667));
#45113=CARTESIAN_POINT('Ctrl Pts',(37.1819756207917,4.81840329350746,21.9755032455374));
#45114=CARTESIAN_POINT('Ctrl Pts',(37.1356717906288,5.08245893146949,21.1350042211103));
#45115=CARTESIAN_POINT('Ctrl Pts',(37.0893679604659,5.12941535477392,20.2825465933572));
#45116=CARTESIAN_POINT('Ctrl Pts',(37.0430641303031,5.17637177807835,19.4300889656041));
#45117=CARTESIAN_POINT('Ctrl Pts',(36.9967603001402,5.00622898672518,18.5656727345251));
#45118=CARTESIAN_POINT('Ctrl Pts',(36.9504564699773,4.6397133058199,17.7945986988745));
#45119=CARTESIAN_POINT('Ctrl Pts',(36.9041526398144,4.27319762491461,17.0235246632239));
#45120=CARTESIAN_POINT('Ctrl Pts',(36.8578488096515,3.71030905445721,16.3457928230018));
#45121=CARTESIAN_POINT('Ctrl Pts',(36.8115449794886,3.0196171260551,15.8439625998744));
#45122=CARTESIAN_POINT('Ctrl Pts',(36.7652411493258,2.328925197653,15.3421323767469));
#45123=CARTESIAN_POINT('Ctrl Pts',(36.7189373191629,1.51042991130619,15.0162037707142));
#45124=CARTESIAN_POINT('Ctrl Pts',(36.672633489,0.663838103062301,14.905880504726));
#45125=CARTESIAN_POINT('Ctrl Pts',(36.6263296588372,-0.182753705181584,
14.7955572387378));
#45126=CARTESIAN_POINT('Ctrl Pts',(36.5800258286743,-1.05744203532252,14.9008393127942));
#45127=CARTESIAN_POINT('Ctrl Pts',(36.5337219985114,-1.85367476985798,15.2089015553007));
#45128=CARTESIAN_POINT('Ctrl Pts',(36.4874181683485,-2.64990750439343,15.5169637978072));
#45129=CARTESIAN_POINT('Ctrl Pts',(36.4411143381856,-3.36768464332339,16.0278062087637));
#45130=CARTESIAN_POINT('Ctrl Pts',(36.3948105080228,-3.91956855725179,16.6791993760222));
#45131=CARTESIAN_POINT('Ctrl Pts',(36.3485066778599,-4.47145247118018,17.3305925432806));
#45132=CARTESIAN_POINT('Ctrl Pts',(36.302202847697,-4.85744316010701,18.122536466841));
#45133=CARTESIAN_POINT('Ctrl Pts',(36.2558990175341,-5.03052030396604,18.9585587243662));
#45134=CARTESIAN_POINT('Ctrl Pts',(36.2369465134571,-5.10136207370919,19.3007488885163));
#45135=CARTESIAN_POINT('Ctrl Pts',(36.2179940093801,-5.13653388071924,19.6503236111705));
#45136=CARTESIAN_POINT('Ctrl Pts',(36.1990415053031,-5.1363684901921,19.9999311527925));
#45137=CARTESIAN_POINT('Ctrl Pts',(36.6759584946969,-5.13711172348184,20.0000703967194));
#45138=CARTESIAN_POINT('Ctrl Pts',(36.7184417976577,-5.13658383483194,19.2167280648719));
#45139=CARTESIAN_POINT('Ctrl Pts',(36.7609251006186,-4.9547232608138,18.4331490285896));
#45140=CARTESIAN_POINT('Ctrl Pts',(36.8034084035795,-4.60866455922797,17.7304305222592));
#45141=CARTESIAN_POINT('Ctrl Pts',(36.8497122337424,-4.23148476792581,16.9645164783491));
#45142=CARTESIAN_POINT('Ctrl Pts',(36.8960160639053,-3.659246205355,16.2946605067825));
#45143=CARTESIAN_POINT('Ctrl Pts',(36.9423198940682,-2.96165739334837,15.8024626126499));
#45144=CARTESIAN_POINT('Ctrl Pts',(36.9886237242311,-2.26406858134175,15.3102647185174));
#45145=CARTESIAN_POINT('Ctrl Pts',(37.0349275543939,-1.44112951989932,14.9957249018188));
#45146=CARTESIAN_POINT('Ctrl Pts',(37.0812313845568,-0.593088373482288,
14.8971595346301));
#45147=CARTESIAN_POINT('Ctrl Pts',(37.1275352147197,0.254952772934734,14.7985941674414));
#45148=CARTESIAN_POINT('Ctrl Pts',(37.1738390448826,1.12809600432639,14.9160032497626));
#45149=CARTESIAN_POINT('Ctrl Pts',(37.2201428750454,1.91997742285391,15.235084331333));
#45150=CARTESIAN_POINT('Ctrl Pts',(37.2664467052083,2.71185884138146,15.5541654129035));
#45151=CARTESIAN_POINT('Ctrl Pts',(37.3127505353712,3.42247844704487,16.0749184937233));
#45152=CARTESIAN_POINT('Ctrl Pts',(37.3590543655341,3.96527052138986,16.7339068712033));
#45153=CARTESIAN_POINT('Ctrl Pts',(37.4053581956969,4.50806259573483,17.3928952486832));
#45154=CARTESIAN_POINT('Ctrl Pts',(37.4516620258598,4.88302713876135,18.1901189228233));
#45155=CARTESIAN_POINT('Ctrl Pts',(37.4979658560227,5.04448700505531,19.0284623066475));
#45156=CARTESIAN_POINT('Ctrl Pts',(37.5442696861856,5.20594687134927,19.8668056904716));
#45157=CARTESIAN_POINT('Ctrl Pts',(37.5905735163485,5.15390206091068,20.7462687839798));
#45158=CARTESIAN_POINT('Ctrl Pts',(37.6368773465114,4.89469252885972,21.5597178211784));
#45159=CARTESIAN_POINT('Ctrl Pts',(37.6831811766742,4.63548299680876,22.373166858377));
#45160=CARTESIAN_POINT('Ctrl Pts',(37.7294850068371,4.16910874314546,23.120601839266));
#45161=CARTESIAN_POINT('Ctrl Pts',(37.775788837,3.55238219186601,23.7109722980224));
#45162=CARTESIAN_POINT('Ctrl Pts',(37.8220926671629,2.93565564058657,24.3013427567789));
#45163=CARTESIAN_POINT('Ctrl Pts',(37.8683964973257,2.16857679169099,24.7346486934028));
#45164=CARTESIAN_POINT('Ctrl Pts',(37.9147003274886,1.34458907276917,24.9581059749834));
#45165=CARTESIAN_POINT('Ctrl Pts',(37.9610041576515,0.520601353847358,25.181563256564));
#45166=CARTESIAN_POINT('Ctrl Pts',(38.0073079878144,-0.360295235100682,
25.1951718831012));
#45167=CARTESIAN_POINT('Ctrl Pts',(38.0536118179773,-1.19079230362451,24.9972740892816));
#45168=CARTESIAN_POINT('Ctrl Pts',(38.0999156481402,-2.02128937214836,24.7993762954619));
#45169=CARTESIAN_POINT('Ctrl Pts',(38.146219478303,-2.80138692024799,24.3899720812854));
#45170=CARTESIAN_POINT('Ctrl Pts',(38.1925233084659,-3.43605561833901,23.8189339378232));
#45171=CARTESIAN_POINT('Ctrl Pts',(38.2388271386288,-4.07072431643002,23.2478957943609));
#45172=CARTESIAN_POINT('Ctrl Pts',(38.2851309687917,-4.55996416451244,22.5152237216129));
#45173=CARTESIAN_POINT('Ctrl Pts',(38.3314347989545,-4.84417731500616,21.7101698086905));
#45174=CARTESIAN_POINT('Ctrl Pts',(38.3629426975353,-5.03757296045447,21.1623629220638));
#45175=CARTESIAN_POINT('Ctrl Pts',(38.3944505961161,-5.136035987151,20.5810413872539));
#45176=CARTESIAN_POINT('Ctrl Pts',(38.4259584946969,-5.13652713961075,19.9998820685162));
#45177=CARTESIAN_POINT('Origin',(25.,0.,20.));
#45178=CARTESIAN_POINT('',(40.1759584946969,-5.13662507615807,20.0001297408024));
#45179=CARTESIAN_POINT('',(39.6990415053031,-5.13679701019626,19.9998685352764));
#45180=CARTESIAN_POINT('',(25.,-5.13675,20.));
#45181=CARTESIAN_POINT('Ctrl Pts',(39.6990415053031,-5.13679701019626,19.9998685352764));
#45182=CARTESIAN_POINT('Ctrl Pts',(39.6626192666225,-5.13610342108661,20.671570825383));
#45183=CARTESIAN_POINT('Ctrl Pts',(39.626197027942,-5.00366088383949,21.3435385570443));
#45184=CARTESIAN_POINT('Ctrl Pts',(39.5897747892614,-4.74690985169674,21.9640726358953));
#45185=CARTESIAN_POINT('Ctrl Pts',(39.5434709590985,-4.42050058589771,22.7529616673848));
#45186=CARTESIAN_POINT('Ctrl Pts',(39.4971671289356,-3.89318140550294,23.4587225844028));
#45187=CARTESIAN_POINT('Ctrl Pts',(39.4508632987728,-3.22918887722381,23.9953815405318));
#45188=CARTESIAN_POINT('Ctrl Pts',(39.4045594686099,-2.56519634894465,24.5320404966608));
#45189=CARTESIAN_POINT('Ctrl Pts',(39.358255638447,-1.76453047278113,24.8995974919006));
#45190=CARTESIAN_POINT('Ctrl Pts',(39.3119518082841,-0.924726155256508,
25.0532777478576));
#45191=CARTESIAN_POINT('Ctrl Pts',(39.2656479781212,-0.0849218377319214,
25.2069580038146));
#45192=CARTESIAN_POINT('Ctrl Pts',(39.2193441479584,0.794020921153764,25.1467615204886));
#45193=CARTESIAN_POINT('Ctrl Pts',(39.1730403177955,1.60503174113409,24.8800212672857));
#45194=CARTESIAN_POINT('Ctrl Pts',(39.1267364876326,2.41604256111441,24.6132810140827));
#45195=CARTESIAN_POINT('Ctrl Pts',(39.0804326574697,3.15912144218937,24.1399969910027));
#45196=CARTESIAN_POINT('Ctrl Pts',(39.0341288273068,3.74374856658888,23.5178233510755));
#45197=CARTESIAN_POINT('Ctrl Pts',(38.987824997144,4.32837569098839,22.8956497111483));
#45198=CARTESIAN_POINT('Ctrl Pts',(38.9415211669811,4.75455105871245,22.1245864543738));
#45199=CARTESIAN_POINT('Ctrl Pts',(38.8952173368182,4.97035916306724,21.2985623779094));
#45200=CARTESIAN_POINT('Ctrl Pts',(38.8489135066553,5.18616726742202,20.4725383014451));
#45201=CARTESIAN_POINT('Ctrl Pts',(38.8026096764924,5.19160810840753,19.5915534052909));
#45202=CARTESIAN_POINT('Ctrl Pts',(38.7563058463296,4.9860188977962,18.7629268372374));
#45203=CARTESIAN_POINT('Ctrl Pts',(38.7100020161667,4.78042968718488,17.9343002691839));
#45204=CARTESIAN_POINT('Ctrl Pts',(38.6636981860038,4.36381042497672,17.158032029231));
#45205=CARTESIAN_POINT('Ctrl Pts',(38.6173943558409,3.78691251947449,16.5286849712169));
#45206=CARTESIAN_POINT('Ctrl Pts',(38.5710905256781,3.21001461397227,15.8993379132027));
#45207=CARTESIAN_POINT('Ctrl Pts',(38.5247866955152,2.47283806517597,15.4169120371273));
#45208=CARTESIAN_POINT('Ctrl Pts',(38.4784828653523,1.6651836850329,15.140175131313));
#45209=CARTESIAN_POINT('Ctrl Pts',(38.4321790351894,0.857529304889817,14.8634382254988));
#45210=CARTESIAN_POINT('Ctrl Pts',(38.3858752050266,-0.0206029066000382,
14.7923902899457));
#45211=CARTESIAN_POINT('Ctrl Pts',(38.3395713748637,-0.862241307816169,
14.9356861880109));
#45212=CARTESIAN_POINT('Ctrl Pts',(38.2932675447008,-1.70387970903231,15.0789820860761));
#45213=CARTESIAN_POINT('Ctrl Pts',(38.2469637145379,-2.50902429997473,15.4366218177595));
#45214=CARTESIAN_POINT('Ctrl Pts',(38.200659884375,-3.17959458945082,15.9650386983339));
#45215=CARTESIAN_POINT('Ctrl Pts',(38.1543560542121,-3.85016487892688,16.4934555789082));
#45216=CARTESIAN_POINT('Ctrl Pts',(38.1080522240493,-4.38616086693662,17.1926496083734));
#45217=CARTESIAN_POINT('Ctrl Pts',(38.0617483938864,-4.72228900202028,17.9774469004235));
#45218=CARTESIAN_POINT('Ctrl Pts',(38.0241794310253,-4.99500910701175,18.6141981198108));
#45219=CARTESIAN_POINT('Ctrl Pts',(37.9866104681642,-5.1361559851209,19.3073020608843));
#45220=CARTESIAN_POINT('Ctrl Pts',(37.9490415053031,-5.13686389810347,20.0001263479959));
#45221=CARTESIAN_POINT('Ctrl Pts',(38.4259584946969,-5.13652713961075,19.9998820685162));
#45222=CARTESIAN_POINT('Ctrl Pts',(38.440754426279,-5.13675778203751,19.726972928089));
#45223=CARTESIAN_POINT('Ctrl Pts',(38.4555503578611,-5.11538377782675,19.4540995593661));
#45224=CARTESIAN_POINT('Ctrl Pts',(38.4703462894432,-5.07209039864956,19.1847493503814));
#45225=CARTESIAN_POINT('Ctrl Pts',(38.516650119606,-4.9366038788942,18.3418185580918));
#45226=CARTESIAN_POINT('Ctrl Pts',(38.5629539497689,-4.58644438647845,17.5333927266096));
#45227=CARTESIAN_POINT('Ctrl Pts',(38.6092577799318,-4.0642673840338,16.857952058791));
#45228=CARTESIAN_POINT('Ctrl Pts',(38.6555616100947,-3.54209038158914,16.1825113909724));
#45229=CARTESIAN_POINT('Ctrl Pts',(38.7018654402576,-2.84789586911556,15.6400558868173));
#45230=CARTESIAN_POINT('Ctrl Pts',(38.7481692704204,-2.06624870556211,15.2966659782087));
#45231=CARTESIAN_POINT('Ctrl Pts',(38.7944731005833,-1.28460154200866,14.9532760696001));
#45232=CARTESIAN_POINT('Ctrl Pts',(38.8407769307462,-0.415501727375322,
14.808951756538));
#45233=CARTESIAN_POINT('Ctrl Pts',(38.8870807609091,0.43517939836545,14.8812742283831));
#45234=CARTESIAN_POINT('Ctrl Pts',(38.933384591072,1.28586052410621,14.9535967002282));
#45235=CARTESIAN_POINT('Ctrl Pts',(38.9796884212348,2.11812296095441,15.2425659569806));
#45236=CARTESIAN_POINT('Ctrl Pts',(39.0259922513977,2.83058279659726,15.7129805615808));
#45237=CARTESIAN_POINT('Ctrl Pts',(39.0722960815606,3.54304263224011,16.1833951661809));
#45238=CARTESIAN_POINT('Ctrl Pts',(39.1185999117235,4.13569986667761,16.8352551186289));
#45239=CARTESIAN_POINT('Ctrl Pts',(39.1649037418864,4.53635863184284,17.5891526391989));
#45240=CARTESIAN_POINT('Ctrl Pts',(39.2112075720492,4.93701739700806,18.3430501597689));
#45241=CARTESIAN_POINT('Ctrl Pts',(39.2575114022121,5.145677692901,19.198985248461));
#45242=CARTESIAN_POINT('Ctrl Pts',(39.303815232375,5.13692109835384,20.0526902558713));
#45243=CARTESIAN_POINT('Ctrl Pts',(39.3501190625379,5.12816450380669,20.9063952632815));
#45244=CARTESIAN_POINT('Ctrl Pts',(39.3964228927008,4.90199101881941,21.7578701894099));
#45245=CARTESIAN_POINT('Ctrl Pts',(39.4427267228636,4.48595247290419,22.503390709542));
#45246=CARTESIAN_POINT('Ctrl Pts',(39.4890305530265,4.06991392698898,23.2489112296742));
#45247=CARTESIAN_POINT('Ctrl Pts',(39.5353343831894,3.46401032014584,23.8884773438102));
#45248=CARTESIAN_POINT('Ctrl Pts',(39.5816382133523,2.74205115695702,24.3441788736662));
#45249=CARTESIAN_POINT('Ctrl Pts',(39.6279420435151,2.02009199376821,24.7998804035221));
#45250=CARTESIAN_POINT('Ctrl Pts',(39.674245873678,1.18207727423371,25.071717349098));
#45251=CARTESIAN_POINT('Ctrl Pts',(39.7205497038409,0.330091637862047,25.1265752841824));
#45252=CARTESIAN_POINT('Ctrl Pts',(39.7668535340038,-0.52189399850962,25.1814332192668));
#45253=CARTESIAN_POINT('Ctrl Pts',(39.8131573641667,-1.38785055171847,25.0193121438596));
#45254=CARTESIAN_POINT('Ctrl Pts',(39.8594611943296,-2.16228958522074,24.6599611997765));
#45255=CARTESIAN_POINT('Ctrl Pts',(39.9057650244924,-2.93672861872303,24.3006102556934));
#45256=CARTESIAN_POINT('Ctrl Pts',(39.9520688546553,-3.61965013251875,23.7440294429343));
#45257=CARTESIAN_POINT('Ctrl Pts',(39.9983726848182,-4.12786251323483,23.0580198994786));
#45258=CARTESIAN_POINT('Ctrl Pts',(40.044676514981,-4.6360748939509,22.3720103560229));
#45259=CARTESIAN_POINT('Ctrl Pts',(40.0909803451439,-4.96957814158735,21.5565720818707));
#45260=CARTESIAN_POINT('Ctrl Pts',(40.1372841753068,-5.08774581126648,20.7110395162838));
#45261=CARTESIAN_POINT('Ctrl Pts',(40.1501756151035,-5.1206448477873,20.4756349692505));
#45262=CARTESIAN_POINT('Ctrl Pts',(40.1630670549002,-5.13685279015782,20.2378977531038));
#45263=CARTESIAN_POINT('Ctrl Pts',(40.1759584946969,-5.13662507615807,20.0001297408024));
#45264=CARTESIAN_POINT('Origin',(25.,0.,20.));
#45265=CARTESIAN_POINT('',(41.9259584946969,-5.13702782547439,19.9999018799691));
#45266=CARTESIAN_POINT('',(41.4490415053031,-5.13640319548555,20.0000850263462));
#45267=CARTESIAN_POINT('',(25.,-5.13675,20.));
#45268=CARTESIAN_POINT('Ctrl Pts',(41.4490415053031,-5.13640319548555,20.0000850263462));
#45269=CARTESIAN_POINT('Ctrl Pts',(41.4312357254066,-5.13659675996406,20.3285331564035));
#45270=CARTESIAN_POINT('Ctrl Pts',(41.4134299455101,-5.10557932918625,20.6569451919344));
#45271=CARTESIAN_POINT('Ctrl Pts',(41.3956241656136,-5.0429996819552,20.9792286081442));
#45272=CARTESIAN_POINT('Ctrl Pts',(41.3493203354508,-4.88026166239715,21.8173248137163));
#45273=CARTESIAN_POINT('Ctrl Pts',(41.3030165052879,-4.50408191610273,22.613975796569));
#45274=CARTESIAN_POINT('Ctrl Pts',(41.2567126751251,-3.96028562119314,23.2721357333979));
#45275=CARTESIAN_POINT('Ctrl Pts',(41.2104088449622,-3.41648932628355,23.9302956702267));
#45276=CARTESIAN_POINT('Ctrl Pts',(41.1641050147993,-2.70507648275881,24.4499645610316));
#45277=CARTESIAN_POINT('Ctrl Pts',(41.1178011846364,-1.91270943911951,24.7678377762578));
#45278=CARTESIAN_POINT('Ctrl Pts',(41.0714973544735,-1.12034239548021,25.0857109914841));
#45279=CARTESIAN_POINT('Ctrl Pts',(41.0251935243106,-0.247021151726365,
25.2017885311316));
#45280=CARTESIAN_POINT('Ctrl Pts',(40.9788896941478,0.600868709328828,25.1019301497921));
#45281=CARTESIAN_POINT('Ctrl Pts',(40.9325858639849,1.44875857038403,25.0020717684527));
#45282=CARTESIAN_POINT('Ctrl Pts',(40.886282033822,2.27121704874058,24.6862774661262));
#45283=CARTESIAN_POINT('Ctrl Pts',(40.8399782036591,2.96805452324197,24.1930164328644));
#45284=CARTESIAN_POINT('Ctrl Pts',(40.7936743734962,3.66489199774336,23.6997553996026));
#45285=CARTESIAN_POINT('Ctrl Pts',(40.7473705433334,4.23610846838958,23.0290276354055));
#45286=CARTESIAN_POINT('Ctrl Pts',(40.7010667131705,4.61211992176423,22.262539344735));
#45287=CARTESIAN_POINT('Ctrl Pts',(40.6547628830076,4.98813137513887,21.4960510540645));
#45288=CARTESIAN_POINT('Ctrl Pts',(40.6084590528447,5.16893781124195,20.6338022369205));
#45289=CARTESIAN_POINT('Ctrl Pts',(40.5621552226818,5.13251388920516,19.780829663676));
#45290=CARTESIAN_POINT('Ctrl Pts',(40.5158513925189,5.09608996716837,18.9278570904315));
#45291=CARTESIAN_POINT('Ctrl Pts',(40.4695475623561,4.84243568699171,18.0841607610863));
#45292=CARTESIAN_POINT('Ctrl Pts',(40.4232437321932,4.40245051278724,17.3525174331702));
#45293=CARTESIAN_POINT('Ctrl Pts',(40.3769399020303,3.96246533858275,16.6208741052541));
#45294=CARTESIAN_POINT('Ctrl Pts',(40.3306360718675,3.33614927035045,16.0012837787669));
#45295=CARTESIAN_POINT('Ctrl Pts',(40.2843322417046,2.59979840236344,15.5692232366912));
#45296=CARTESIAN_POINT('Ctrl Pts',(40.2380284115417,1.86344753437645,15.1371626946156));
#45297=CARTESIAN_POINT('Ctrl Pts',(40.1917245813788,1.01706186663476,14.8926319369513));
#45298=CARTESIAN_POINT('Ctrl Pts',(40.1454207512159,0.163745764446629,14.8654190254867));
#45299=CARTESIAN_POINT('Ctrl Pts',(40.099116921053,-0.689570337741517,14.8382061140221));
#45300=CARTESIAN_POINT('Ctrl Pts',(40.0528130908902,-1.54981687437611,15.028311048757));
#45301=CARTESIAN_POINT('Ctrl Pts',(40.0065092607273,-2.31220098736803,15.4125757713917));
#45302=CARTESIAN_POINT('Ctrl Pts',(39.9602054305644,-3.07458510035994,15.7968404940263));
#45303=CARTESIAN_POINT('Ctrl Pts',(39.9139016004016,-3.73910678970917,16.3752650045606));
#45304=CARTESIAN_POINT('Ctrl Pts',(39.8675977702387,-4.22481585785777,17.0773872260592));
#45305=CARTESIAN_POINT('Ctrl Pts',(39.8212939400758,-4.71052492600638,17.7795094475579));
#45306=CARTESIAN_POINT('Ctrl Pts',(39.7749901099129,-5.01742137295435,18.6053293800208));
#45307=CARTESIAN_POINT('Ctrl Pts',(39.72868627975,-5.10811992082669,19.4542479192328));
#45308=CARTESIAN_POINT('Ctrl Pts',(39.7188046882677,-5.12747568459311,19.635413627917));
#45309=CARTESIAN_POINT('Ctrl Pts',(39.7089230967854,-5.13698518545639,19.8176313123869));
#45310=CARTESIAN_POINT('Ctrl Pts',(39.6990415053031,-5.13679701019626,19.9998685352764));
#45311=CARTESIAN_POINT('Ctrl Pts',(40.1759584946969,-5.13662507615807,20.0001297408024));
#45312=CARTESIAN_POINT('Ctrl Pts',(40.2093708850631,-5.13603488071278,19.3838760275705));
#45313=CARTESIAN_POINT('Ctrl Pts',(40.2427832754292,-5.02503700210934,18.7674154389927));
#45314=CARTESIAN_POINT('Ctrl Pts',(40.2761956657955,-4.80807881275319,18.1908253914753));
#45315=CARTESIAN_POINT('Ctrl Pts',(40.3224994959583,-4.50741205283897,17.3917706892752));
#45316=CARTESIAN_POINT('Ctrl Pts',(40.3688033261212,-4.00324644128875,16.6692881418965));
#45317=CARTESIAN_POINT('Ctrl Pts',(40.4151071562841,-3.35699804098061,16.1113885786017));
#45318=CARTESIAN_POINT('Ctrl Pts',(40.461410986447,-2.71074964067246,15.5534890153069));
#45319=CARTESIAN_POINT('Ctrl Pts',(40.5077148166099,-1.92241845160638,15.160172436096));
#45320=CARTESIAN_POINT('Ctrl Pts',(40.5540186467727,-1.08803680277753,14.9793515807639));
#45321=CARTESIAN_POINT('Ctrl Pts',(40.6003224769356,-0.253655153948683,
14.7985307254318));
#45322=CARTESIAN_POINT('Ctrl Pts',(40.6466263070985,0.626776954642942,14.8302055939786));
#45323=CARTESIAN_POINT('Ctrl Pts',(40.6929301372614,1.44600771426156,15.0705176413671));
#45324=CARTESIAN_POINT('Ctrl Pts',(40.7392339674242,2.26523847388015,15.3108296887557));
#45325=CARTESIAN_POINT('Ctrl Pts',(40.7855377975871,3.02326788452574,15.759778914986));
#45326=CARTESIAN_POINT('Ctrl Pts',(40.83184162775,3.62775489619198,16.362675564796));
#45327=CARTESIAN_POINT('Ctrl Pts',(40.8781454579129,4.23224190785823,16.9655722146061));
#45328=CARTESIAN_POINT('Ctrl Pts',(40.9244492880757,4.68318652054512,17.7224162879959));
#45329=CARTESIAN_POINT('Ctrl Pts',(40.9707531182386,4.92565590652139,18.541011129471));
#45330=CARTESIAN_POINT('Ctrl Pts',(41.0170569484015,5.16812529249767,19.3596059709461));
#45331=CARTESIAN_POINT('Ctrl Pts',(41.0633607785644,5.20211945176333,20.2399515805066));
#45332=CARTESIAN_POINT('Ctrl Pts',(41.1096646087273,5.0234973096891,21.0748066864897));
#45333=CARTESIAN_POINT('Ctrl Pts',(41.1559684388902,4.84487516761487,21.9096617924729));
#45334=CARTESIAN_POINT('Ctrl Pts',(41.202272269053,4.45363672420075,22.6990263948788));
#45335=CARTESIAN_POINT('Ctrl Pts',(41.2485760992159,3.8974415664764,23.3467422771523));
#45336=CARTESIAN_POINT('Ctrl Pts',(41.2948799293788,3.34124640875205,23.9944581594258));
#45337=CARTESIAN_POINT('Ctrl Pts',(41.3411837595417,2.62009453671747,24.500525321567));
#45338=CARTESIAN_POINT('Ctrl Pts',(41.3874875897045,1.82183468043843,24.8032960590545));
#45339=CARTESIAN_POINT('Ctrl Pts',(41.4337914198674,1.0235748241594,25.106066796542));
#45340=CARTESIAN_POINT('Ctrl Pts',(41.4800952500303,0.148206983635904,25.205541109376));
#45341=CARTESIAN_POINT('Ctrl Pts',(41.5263990801932,-0.697633947550682,
25.0896013113997));
#45342=CARTESIAN_POINT('Ctrl Pts',(41.5727029103561,-1.54347487873726,24.9736615134234));
#45343=CARTESIAN_POINT('Ctrl Pts',(41.6190067405189,-2.35978890058693,24.6423076046368));
#45344=CARTESIAN_POINT('Ctrl Pts',(41.6653105706818,-3.04713489267099,24.135904203393));
#45345=CARTESIAN_POINT('Ctrl Pts',(41.7116144008447,-3.73448088475504,23.6295008021491));
#45346=CARTESIAN_POINT('Ctrl Pts',(41.7579182310076,-4.29285884707349,22.948047908448));
#45347=CARTESIAN_POINT('Ctrl Pts',(41.8042220611704,-4.65424871784935,22.1745582324174));
#45348=CARTESIAN_POINT('Ctrl Pts',(41.8448008723459,-4.97095624021537,21.4967030442091));
#45349=CARTESIAN_POINT('Ctrl Pts',(41.8853796835214,-5.13637565909862,20.7481630235307));
#45350=CARTESIAN_POINT('Ctrl Pts',(41.9259584946969,-5.13702782547439,19.9999018799691));
#45351=CARTESIAN_POINT('Origin',(25.,0.,20.));
#45352=CARTESIAN_POINT('',(43.6759584946968,-5.13631567875976,20.0000203800902));
#45353=CARTESIAN_POINT('',(43.1990415053031,-5.13718721057151,19.9999841637545));
#45354=CARTESIAN_POINT('',(25.,-5.13675,20.));
#45355=CARTESIAN_POINT('Ctrl Pts',(43.1990415053031,-5.13718721057151,19.9999841637545));
#45356=CARTESIAN_POINT('Ctrl Pts',(43.1535483540278,-5.13703940376405,20.8387887285521));
#45357=CARTESIAN_POINT('Ctrl Pts',(43.1080552027526,-4.92745027586239,21.6776644683076));
#45358=CARTESIAN_POINT('Ctrl Pts',(43.0625620514773,-4.53267718080418,22.4177617818605));
#45359=CARTESIAN_POINT('Ctrl Pts',(43.0162582213144,-4.13086930788185,23.1710474820179));
#45360=CARTESIAN_POINT('Ctrl Pts',(42.9699543911515,-3.537218780741,23.822002965617));
#45361=CARTESIAN_POINT('Ctrl Pts',(42.9236505609887,-2.82404246762336,24.2913306328303));
#45362=CARTESIAN_POINT('Ctrl Pts',(42.8773467308258,-2.11086615450573,24.7606583000437));
#45363=CARTESIAN_POINT('Ctrl Pts',(42.8310429006629,-1.27816405541132,25.0483581508711));
#45364=CARTESIAN_POINT('Ctrl Pts',(42.7847390705,-0.427373641093902,25.1193833837784));
#45365=CARTESIAN_POINT('Ctrl Pts',(42.7384352403371,0.423416773223512,25.1904086166857));
#45366=CARTESIAN_POINT('Ctrl Pts',(42.6921314101743,1.29229550276393,25.0447592316728));
#45367=CARTESIAN_POINT('Ctrl Pts',(42.6458275800114,2.07341813953054,24.7001778347073));
#45368=CARTESIAN_POINT('Ctrl Pts',(42.5995237498485,2.85454077629716,24.3555964377418));
#45369=CARTESIAN_POINT('Ctrl Pts',(42.5532199196856,3.54790732028998,23.8120830288236));
#45370=CARTESIAN_POINT('Ctrl Pts',(42.5069160895227,4.0690537733944,23.1358469108732));
#45371=CARTESIAN_POINT('Ctrl Pts',(42.4606122593599,4.59020022649883,22.4596107929228));
#45372=CARTESIAN_POINT('Ctrl Pts',(42.414308429197,4.93912658871485,21.6506519659402));
#45373=CARTESIAN_POINT('Ctrl Pts',(42.3680045990342,5.07332761392745,20.8075155608218));
#45374=CARTESIAN_POINT('Ctrl Pts',(42.3217007688713,5.20752863914005,19.9643791557036));
#45375=CARTESIAN_POINT('Ctrl Pts',(42.2753969387083,5.12700432734922,19.0870651724496));
#45376=CARTESIAN_POINT('Ctrl Pts',(42.2290931085455,4.84156392790253,18.2824455783757));
#45377=CARTESIAN_POINT('Ctrl Pts',(42.1827892783826,4.55612352845583,17.4778259843018));
#45378=CARTESIAN_POINT('Ctrl Pts',(42.1364854482197,4.06576704135327,16.745900779408));
#45379=CARTESIAN_POINT('Ctrl Pts',(42.0901816180569,3.43022834005749,16.1758310714255));
#45380=CARTESIAN_POINT('Ctrl Pts',(42.043877787894,2.79468963876171,15.605761363443));
#45381=CARTESIAN_POINT('Ctrl Pts',(41.9975739577311,2.01396872327272,15.1975471523719));
#45382=CARTESIAN_POINT('Ctrl Pts',(41.9512701275682,1.18317086006926,15.0009159663903));
#45383=CARTESIAN_POINT('Ctrl Pts',(41.9049662974053,0.352372996865793,14.8042847804088));
#45384=CARTESIAN_POINT('Ctrl Pts',(41.8586624672425,-0.528501814052137,
14.8192366195168));
#45385=CARTESIAN_POINT('Ctrl Pts',(41.8123586370796,-1.35214783517359,15.0439500919539));
#45386=CARTESIAN_POINT('Ctrl Pts',(41.7660548069167,-2.17579385629504,15.268663564391));
#45387=CARTESIAN_POINT('Ctrl Pts',(41.7197509767538,-2.94221108762,15.7031386701572));
#45388=CARTESIAN_POINT('Ctrl Pts',(41.6734471465909,-3.55803669798442,16.2944488513847));
#45389=CARTESIAN_POINT('Ctrl Pts',(41.627143316428,-4.17386230834885,16.8857590326121));
#45390=CARTESIAN_POINT('Ctrl Pts',(41.5808394862652,-4.63909629775273,17.6339042893008));
#45391=CARTESIAN_POINT('Ctrl Pts',(41.5345356561023,-4.89706514604382,18.4477476317908));
#45392=CARTESIAN_POINT('Ctrl Pts',(41.5060376058359,-5.05583406818061,18.9486338090611));
#45393=CARTESIAN_POINT('Ctrl Pts',(41.4775395555695,-5.13609339662976,19.4744056472516));
#45394=CARTESIAN_POINT('Ctrl Pts',(41.4490415053031,-5.13640319548555,20.0000850263462));
#45395=CARTESIAN_POINT('Ctrl Pts',(41.9259584946969,-5.13702782547439,19.9999018799691));
#45396=CARTESIAN_POINT('Ctrl Pts',(41.9316835136843,-5.13711983568307,19.8943342418265));
#45397=CARTESIAN_POINT('Ctrl Pts',(41.9374085326717,-5.13393220627652,19.788772154644));
#45398=CARTESIAN_POINT('Ctrl Pts',(41.9431335516591,-5.12742708469005,19.6834149009136));
#45399=CARTESIAN_POINT('Ctrl Pts',(41.989437381822,-5.07481380152163,18.8312877038006));
#45400=CARTESIAN_POINT('Ctrl Pts',(42.0357412119849,-4.80518545595153,17.9925597679348));
#45401=CARTESIAN_POINT('Ctrl Pts',(42.0820450421477,-4.35138742863618,17.2694026148691));
#45402=CARTESIAN_POINT('Ctrl Pts',(42.1283488723106,-3.89758940132085,16.5462454618034));
#45403=CARTESIAN_POINT('Ctrl Pts',(42.1746527024735,-3.25962169226028,15.9386590915378));
#45404=CARTESIAN_POINT('Ctrl Pts',(42.2209565326364,-2.51519976644497,15.5206579982489));
#45405=CARTESIAN_POINT('Ctrl Pts',(42.2672603627992,-1.77077784062965,15.1026569049599));
#45406=CARTESIAN_POINT('Ctrl Pts',(42.3135641929621,-0.919901698059582,
14.8742410886476));
#45407=CARTESIAN_POINT('Ctrl Pts',(42.359868023125,-0.0662227212891285,
14.8632355334353));
#45408=CARTESIAN_POINT('Ctrl Pts',(42.4061718532879,0.787456255481325,14.8522299782231));
#45409=CARTESIAN_POINT('Ctrl Pts',(42.4524756834507,1.64393806645217,15.0586346841109));
#45410=CARTESIAN_POINT('Ctrl Pts',(42.4987795136136,2.39888846202082,15.4573059996782));
#45411=CARTESIAN_POINT('Ctrl Pts',(42.5450833437765,3.15383885758947,15.8559773152454));
#45412=CARTESIAN_POINT('Ctrl Pts',(42.5913871739394,3.80725783775592,16.446915240492));
#45413=CARTESIAN_POINT('Ctrl Pts',(42.6376910041023,4.27954770634207,17.1581333488499));
#45414=CARTESIAN_POINT('Ctrl Pts',(42.6839948342652,4.75183757492822,17.8693514572079));
#45415=CARTESIAN_POINT('Ctrl Pts',(42.730298664428,5.04299833193406,18.7008497486771));
#45416=CARTESIAN_POINT('Ctrl Pts',(42.7766024945909,5.11756157778963,19.5513373970253));
#45417=CARTESIAN_POINT('Ctrl Pts',(42.8229063247538,5.19212482364519,20.4018250453735));
#45418=CARTESIAN_POINT('Ctrl Pts',(42.8692101549167,5.05009055835048,21.2713020506007));
#45419=CARTESIAN_POINT('Ctrl Pts',(42.9155139850795,4.70876100396969,22.0538511244175));
#45420=CARTESIAN_POINT('Ctrl Pts',(42.9618178152424,4.36743144958891,22.8364001982343));
#45421=CARTESIAN_POINT('Ctrl Pts',(43.0081216454053,3.82680660612205,23.5320213406409));
#45422=CARTESIAN_POINT('Ctrl Pts',(43.0544254755682,3.15274389942116,24.0559759045684));
#45423=CARTESIAN_POINT('Ctrl Pts',(43.1007293057311,2.47868119272028,24.5799304684959));
#45424=CARTESIAN_POINT('Ctrl Pts',(43.1470331358939,1.67118062278537,24.9322184539443));
#45425=CARTESIAN_POINT('Ctrl Pts',(43.1933369660568,0.828609679665406,25.0699251111374));
#45426=CARTESIAN_POINT('Ctrl Pts',(43.2396407962197,-0.0139612634545576,
25.2076317683305));
#45427=CARTESIAN_POINT('Ctrl Pts',(43.2859446263826,-0.89160257975957,25.1307570972682));
#45428=CARTESIAN_POINT('Ctrl Pts',(43.3322484565454,-1.69740242712528,24.8486657581407));
#45429=CARTESIAN_POINT('Ctrl Pts',(43.3785522867083,-2.50320227449099,24.5665744190131));
#45430=CARTESIAN_POINT('Ctrl Pts',(43.4248561168712,-3.2371606529174,24.0792664118203));
#45431=CARTESIAN_POINT('Ctrl Pts',(43.4711599470341,-3.80986877908679,23.4461042526186));
#45432=CARTESIAN_POINT('Ctrl Pts',(43.517463777197,-4.38257690525619,22.812942093417));
#45433=CARTESIAN_POINT('Ctrl Pts',(43.5637676073598,-4.79403477916857,22.0339257822065));
#45434=CARTESIAN_POINT('Ctrl Pts',(43.6100714375227,-4.99411973859361,21.2039529352788));
#45435=CARTESIAN_POINT('Ctrl Pts',(43.6320337899141,-5.08902196097241,20.810288824224));
#45436=CARTESIAN_POINT('Ctrl Pts',(43.6539961423055,-5.13637169871656,20.4051610405998));
#45437=CARTESIAN_POINT('Ctrl Pts',(43.6759584946968,-5.13631567875976,20.0000203800902));
#45438=CARTESIAN_POINT('Origin',(25.,0.,20.));
#45439=CARTESIAN_POINT('',(45.4259584946969,-5.13712894348962,20.0000625125626));
#45440=CARTESIAN_POINT('',(44.9490415053031,-5.13635638952797,19.9999383013781));
#45441=CARTESIAN_POINT('',(25.,-5.13675,20.));
#45442=CARTESIAN_POINT('Ctrl Pts',(44.9490415053031,-5.13635638952797,19.9999383013781));
#45443=CARTESIAN_POINT('Ctrl Pts',(44.9221648128119,-5.13614682048153,20.4957228006643));
#45444=CARTESIAN_POINT('Ctrl Pts',(44.8952881203207,-5.06488923577723,20.9915662676101));
#45445=CARTESIAN_POINT('Ctrl Pts',(44.8684114278296,-4.92342543575894,21.4664980183179));
#45446=CARTESIAN_POINT('Ctrl Pts',(44.8221075976667,-4.67970810437996,22.2847221778178));
#45447=CARTESIAN_POINT('Ctrl Pts',(44.7758037675038,-4.22760994953467,23.040877749369));
#45448=CARTESIAN_POINT('Ctrl Pts',(44.7294999373409,-3.62220432027531,23.6428519488702));
#45449=CARTESIAN_POINT('Ctrl Pts',(44.6831961071781,-3.01679869101595,24.2448261483713));
#45450=CARTESIAN_POINT('Ctrl Pts',(44.6368922770152,-2.25808558734251,24.6926189758224));
#45451=CARTESIAN_POINT('Ctrl Pts',(44.5905884468523,-1.43848934485844,24.931681545268));
#45452=CARTESIAN_POINT('Ctrl Pts',(44.5442846166895,-0.618893102374381,
25.1707441147136));
#45453=CARTESIAN_POINT('Ctrl Pts',(44.4979807865265,0.261586278920312,25.2010764261538));
#45454=CARTESIAN_POINT('Ctrl Pts',(44.4516769563636,1.09569123165968,25.0189834811516));
#45455=CARTESIAN_POINT('Ctrl Pts',(44.4053731262007,1.92979618439905,24.8368905361493));
#45456=CARTESIAN_POINT('Ctrl Pts',(44.3590692960379,2.7175267085831,24.4423723347047));
#45457=CARTESIAN_POINT('Ctrl Pts',(44.312765465875,3.36292364655426,23.8834879949157));
#45458=CARTESIAN_POINT('Ctrl Pts',(44.2664616357121,4.00832058452544,23.3246036551267));
#45459=CARTESIAN_POINT('Ctrl Pts',(44.2201578055493,4.51138393628372,22.6013531769933));
#45460=CARTESIAN_POINT('Ctrl Pts',(44.1738539753864,4.81083191319573,21.8018409369824));
#45461=CARTESIAN_POINT('Ctrl Pts',(44.1275501452235,5.11027989010774,21.0023286969715));
#45462=CARTESIAN_POINT('Ctrl Pts',(44.0812463150606,5.20611249217347,20.1265546950831));
#45463=CARTESIAN_POINT('Ctrl Pts',(44.0349424848978,5.08665565638783,19.2812033023546));
#45464=CARTESIAN_POINT('Ctrl Pts',(43.9886386547349,4.96719882060219,18.4358519096261));
#45465=CARTESIAN_POINT('Ctrl Pts',(43.942334824572,4.63245254696518,17.6209231260575));
#45466=CARTESIAN_POINT('Ctrl Pts',(43.8960309944091,4.12319470235011,16.9356893261746));
#45467=CARTESIAN_POINT('Ctrl Pts',(43.8497271642462,3.61393685773505,16.2504555262917));
#45468=CARTESIAN_POINT('Ctrl Pts',(43.8034233340834,2.93016744214192,15.6949167100945));
#45469=CARTESIAN_POINT('Ctrl Pts',(43.7571195039205,2.15518135799981,15.3367470824179));
#45470=CARTESIAN_POINT('Ctrl Pts',(43.7108156737576,1.3801952738577,14.9785774547412));
#45471=CARTESIAN_POINT('Ctrl Pts',(43.6645118435947,0.513992521166593,14.8177770155852));
#45472=CARTESIAN_POINT('Ctrl Pts',(43.6182080134318,-0.337908472188524,
14.8739340305034));
#45473=CARTESIAN_POINT('Ctrl Pts',(43.571904183269,-1.18980946554365,14.9300910454215));
#45474=CARTESIAN_POINT('Ctrl Pts',(43.5256003531061,-2.02740869956279,15.2032055144139));
#45475=CARTESIAN_POINT('Ctrl Pts',(43.4792965229432,-2.74867214803584,15.6600073868934));
#45476=CARTESIAN_POINT('Ctrl Pts',(43.4329926927803,-3.46993559650886,16.1168092593728));
#45477=CARTESIAN_POINT('Ctrl Pts',(43.3866888626174,-4.07486325943579,16.7572985353393));
#45478=CARTESIAN_POINT('Ctrl Pts',(43.3403850324546,-4.48976451902782,17.5034525794836));
#45479=CARTESIAN_POINT('Ctrl Pts',(43.2940812022917,-4.90466577861986,18.2496066236279));
#45480=CARTESIAN_POINT('Ctrl Pts',(43.2477773721288,-5.129540634877,19.1014254359499));
#45481=CARTESIAN_POINT('Ctrl Pts',(43.2014735419659,-5.13699545365367,19.9551428004687));
#45482=CARTESIAN_POINT('Ctrl Pts',(43.2006628630783,-5.13712597124092,19.9700895260629));
#45483=CARTESIAN_POINT('Ctrl Pts',(43.1998521841907,-5.13718984445936,19.985036833608));
#45484=CARTESIAN_POINT('Ctrl Pts',(43.1990415053031,-5.13718721057151,19.9999841637545));
#45485=CARTESIAN_POINT('Ctrl Pts',(43.6759584946968,-5.13631567875976,20.0000203800902));
#45486=CARTESIAN_POINT('Ctrl Pts',(43.7002999724684,-5.13625359030453,19.5509918695563));
#45487=CARTESIAN_POINT('Ctrl Pts',(43.7246414502399,-5.07795875684034,19.1019475411889));
#45488=CARTESIAN_POINT('Ctrl Pts',(43.7489829280114,-4.96163094092812,18.6684771726323));
#45489=CARTESIAN_POINT('Ctrl Pts',(43.7952867581742,-4.74034513889991,17.8439036395583));
#45490=CARTESIAN_POINT('Ctrl Pts',(43.8415905883371,-4.30906148990579,17.0756859560552));
#45491=CARTESIAN_POINT('Ctrl Pts',(43.8878944185,-3.72031777736076,16.4574062794006));
#45492=CARTESIAN_POINT('Ctrl Pts',(43.9341982486629,-3.13157406481572,15.8391266027461));
#45493=CARTESIAN_POINT('Ctrl Pts',(43.9805020788258,-2.38537028871977,15.37078493294));
#45494=CARTESIAN_POINT('Ctrl Pts',(44.0268059089886,-1.57260693292711,15.1094333591816));
#45495=CARTESIAN_POINT('Ctrl Pts',(44.0731097391515,-0.759843577134466,
14.8480817854231));
#45496=CARTESIAN_POINT('Ctrl Pts',(44.1194135693144,0.119479358354885,14.7937203077121));
#45497=CARTESIAN_POINT('Ctrl Pts',(44.1657173994773,0.95824518121023,14.9529710911801));
#45498=CARTESIAN_POINT('Ctrl Pts',(44.2120212296401,1.79701100406557,15.112221874648));
#45499=CARTESIAN_POINT('Ctrl Pts',(44.258325059803,2.59521971428691,15.4850849192949));
#45500=CARTESIAN_POINT('Ctrl Pts',(44.3046288899659,3.25563573052222,16.0261390784372));
#45501=CARTESIAN_POINT('Ctrl Pts',(44.3509327201288,3.91605174675754,16.5671932375796));
#45502=CARTESIAN_POINT('Ctrl Pts',(44.3972365502917,4.43867506900683,17.2764385112175));
#45503=CARTESIAN_POINT('Ctrl Pts',(44.4435403804546,4.75984116703344,18.0674765982296));
#45504=CARTESIAN_POINT('Ctrl Pts',(44.4898442106174,5.08100726506006,18.8585146852417));
#45505=CARTESIAN_POINT('Ctrl Pts',(44.5361480407803,5.200716138864,19.7313455856279));
#45506=CARTESIAN_POINT('Ctrl Pts',(44.5824518709432,5.10438518393562,20.5796434488505));
#45507=CARTESIAN_POINT('Ctrl Pts',(44.6287557011061,5.00805422900723,21.427941312073));
#45508=CARTESIAN_POINT('Ctrl Pts',(44.6750595312689,4.69568344534651,22.2517061381319));
#45509=CARTESIAN_POINT('Ctrl Pts',(44.7213633614318,4.20532497941302,22.9505891702));
#45510=CARTESIAN_POINT('Ctrl Pts',(44.7676671915947,3.71496651347954,23.6494722022681));
#45511=CARTESIAN_POINT('Ctrl Pts',(44.8139710217576,3.04662036527329,24.2234734403455));
#45512=CARTESIAN_POINT('Ctrl Pts',(44.8602748519205,2.28170261737147,24.6026696383357));
#45513=CARTESIAN_POINT('Ctrl Pts',(44.9065786820833,1.51678486946965,24.9818658363258));
#45514=CARTESIAN_POINT('Ctrl Pts',(44.9528825122462,0.655295521872253,25.1662569942286));
#45515=CARTESIAN_POINT('Ctrl Pts',(44.9991863424091,-0.197821171531303,
25.1333810902631));
#45516=CARTESIAN_POINT('Ctrl Pts',(45.0454901725719,-1.05093786493486,25.1005051862975));
#45517=CARTESIAN_POINT('Ctrl Pts',(45.0917940027349,-1.89568190414457,24.8503622204636));
#45518=CARTESIAN_POINT('Ctrl Pts',(45.1380978328977,-2.6291489025077,24.4134239182543));
#45519=CARTESIAN_POINT('Ctrl Pts',(45.1844016630606,-3.36261590087082,23.976485616045));
#45520=CARTESIAN_POINT('Ctrl Pts',(45.2307054932235,-3.98480585838736,23.3527519774603));
#45521=CARTESIAN_POINT('Ctrl Pts',(45.2770093233863,-4.41992531220002,22.6182045123233));
#45522=CARTESIAN_POINT('Ctrl Pts',(45.3233131535492,-4.85504476601268,21.8836570471864));
#45523=CARTESIAN_POINT('Ctrl Pts',(45.3696169837121,-5.10309371612148,21.0382957554972));
#45524=CARTESIAN_POINT('Ctrl Pts',(45.415920813875,-5.13385552424782,20.1851002159014));
#45525=CARTESIAN_POINT('Ctrl Pts',(45.4192667074823,-5.13607835844526,20.1234486961101));
#45526=CARTESIAN_POINT('Ctrl Pts',(45.4226126010896,-5.1371666405299,20.0617562702512));
#45527=CARTESIAN_POINT('Ctrl Pts',(45.4259584946969,-5.13712894348962,20.0000625125626));
#45528=CARTESIAN_POINT('Origin',(25.,0.,20.));
#45529=CARTESIAN_POINT('',(47.1759584946969,-5.13650480025366,19.9998861825852));
#45530=CARTESIAN_POINT('',(46.6990415053031,-5.13689122437247,20.0001232958892));
#45531=CARTESIAN_POINT('',(25.,-5.13675,20.));
#45532=CARTESIAN_POINT('Ctrl Pts',(46.6990415053031,-5.13689122437247,20.0001232958892));
#45533=CARTESIAN_POINT('Ctrl Pts',(46.690781271596,-5.13704510784903,20.152451236073));
#45534=CARTESIAN_POINT('Ctrl Pts',(46.6825210378889,-5.13040429337675,20.3047658062091));
#45535=CARTESIAN_POINT('Ctrl Pts',(46.6742608041819,-5.11687147158231,20.4564655545811));
#45536=CARTESIAN_POINT('Ctrl Pts',(46.627956974019,-5.04101145306286,21.3068385141673));
#45537=CARTESIAN_POINT('Ctrl Pts',(46.5816531438561,-4.74858313169487,22.1378918619507));
#45538=CARTESIAN_POINT('Ctrl Pts',(46.5353493136932,-4.27520931824056,22.8483889735136));
#45539=CARTESIAN_POINT('Ctrl Pts',(46.4890454835303,-3.80183550478624,23.5588860850765));
#45540=CARTESIAN_POINT('Ctrl Pts',(46.4427416533675,-3.14751619924559,24.1488269604189));
#45541=CARTESIAN_POINT('Ctrl Pts',(46.3964378232046,-2.39195877294756,24.5463466308377));
#45542=CARTESIAN_POINT('Ctrl Pts',(46.3501339930417,-1.63640134664952,24.9438663012566));
#45543=CARTESIAN_POINT('Ctrl Pts',(46.3038301628788,-0.779605799594105,
25.1489647667518));
#45544=CARTESIAN_POINT('Ctrl Pts',(46.2575263327159,0.0740554001521648,
25.1366574985019));
#45545=CARTESIAN_POINT('Ctrl Pts',(46.211222502553,0.927716599898423,25.1243502302519));
#45546=CARTESIAN_POINT('Ctrl Pts',(46.1649186723902,1.77824345233553,24.8946372282569));
#45547=CARTESIAN_POINT('Ctrl Pts',(46.1186148422273,2.52202712446896,24.4755014962182));
#45548=CARTESIAN_POINT('Ctrl Pts',(46.0723110120645,3.2658107966024,24.0563657641796));
#45549=CARTESIAN_POINT('Ctrl Pts',(46.0260071819015,3.90285128843215,23.4478073020973));
#45550=CARTESIAN_POINT('Ctrl Pts',(45.9797033517386,4.35554608601079,22.7239590216896));
#45551=CARTESIAN_POINT('Ctrl Pts',(45.9333995215757,4.80824088358944,22.0001107412819));
#45552=CARTESIAN_POINT('Ctrl Pts',(45.8870956914129,5.07658998691698,21.1609726425487));
#45553=CARTESIAN_POINT('Ctrl Pts',(45.8407918612501,5.12790384909524,20.3087662119509));
#45554=CARTESIAN_POINT('Ctrl Pts',(45.7944880310872,5.17921771127349,19.4565597813531));
#45555=CARTESIAN_POINT('Ctrl Pts',(45.7481842009243,5.01349633230246,18.5912850188906));
#45556=CARTESIAN_POINT('Ctrl Pts',(45.7018803707614,4.65092743303804,17.818347307241));
#45557=CARTESIAN_POINT('Ctrl Pts',(45.6555765405985,4.28835853377361,17.0454095955914));
#45558=CARTESIAN_POINT('Ctrl Pts',(45.6092727104357,3.7289421142158,16.3648089347546));
#45559=CARTESIAN_POINT('Ctrl Pts',(45.5629688802728,3.04082473813548,15.8594542182037));
#45560=CARTESIAN_POINT('Ctrl Pts',(45.5166650501099,2.35270736205516,15.3540995016527));
#45561=CARTESIAN_POINT('Ctrl Pts',(45.470361219947,1.53588902945233,15.0239907293876));
#45562=CARTESIAN_POINT('Ctrl Pts',(45.4240573897841,0.689872294499334,14.909340840668));
#45563=CARTESIAN_POINT('Ctrl Pts',(45.3777535596212,-0.156144440453653,
14.7946909519484));
#45564=CARTESIAN_POINT('Ctrl Pts',(45.3314497294584,-1.03135957775681,14.8954999467743));
#45565=CARTESIAN_POINT('Ctrl Pts',(45.2851458992955,-1.8291568257135,15.1994875517135));
#45566=CARTESIAN_POINT('Ctrl Pts',(45.2388420691326,-2.62695407367019,15.5034751566527));
#45567=CARTESIAN_POINT('Ctrl Pts',(45.1925382389697,-3.3473334322804,16.0106413717052));
#45568=CARTESIAN_POINT('Ctrl Pts',(45.1462344088068,-3.90254027693094,16.6592046087586));
#45569=CARTESIAN_POINT('Ctrl Pts',(45.099930578644,-4.45774712158149,17.3077678458119));
#45570=CARTESIAN_POINT('Ctrl Pts',(45.0536267484811,-4.84778145227236,18.0977281048661));
#45571=CARTESIAN_POINT('Ctrl Pts',(45.0073229183182,-5.02513036366146,18.9328546081176));
#45572=CARTESIAN_POINT('Ctrl Pts',(44.9878957806465,-5.09953850021006,19.2832385287324));
#45573=CARTESIAN_POINT('Ctrl Pts',(44.9684686429748,-5.13650787121488,19.6415730104744));
#45574=CARTESIAN_POINT('Ctrl Pts',(44.9490415053031,-5.13635638952797,19.9999383013781));
#45575=CARTESIAN_POINT('Ctrl Pts',(45.4259584946969,-5.13712894348962,20.0000625125626));
#45576=CARTESIAN_POINT('Ctrl Pts',(45.4689164312525,-5.13664495109337,19.207976200288));
#45577=CARTESIAN_POINT('Ctrl Pts',(45.511874367808,-4.95055457497461,18.415670349234));
#45578=CARTESIAN_POINT('Ctrl Pts',(45.5548323043636,-4.59700152388307,17.7068991249416));
#45579=CARTESIAN_POINT('Ctrl Pts',(45.6011361345265,-4.21591104924808,16.9429233610801));
#45580=CARTESIAN_POINT('Ctrl Pts',(45.6474399646894,-3.64025543383418,16.2760016208595));
#45581=CARTESIAN_POINT('Ctrl Pts',(45.6937437948523,-2.94015945541774,15.7873764694085));
#45582=CARTESIAN_POINT('Ctrl Pts',(45.7400476250152,-2.2400634770013,15.2987513179574));
#45583=CARTESIAN_POINT('Ctrl Pts',(45.786351455178,-1.4155271355823,14.9884227552759));
#45584=CARTESIAN_POINT('Ctrl Pts',(45.8326552853409,-0.566993171858652,
14.8941941501028));
#45585=CARTESIAN_POINT('Ctrl Pts',(45.8789591155038,0.281540791864998,14.7999655449297));
#45586=CARTESIAN_POINT('Ctrl Pts',(45.9252629456667,1.1540723778933,14.9218368972651));
#45587=CARTESIAN_POINT('Ctrl Pts',(45.9715667758296,1.9443121973366,15.2449621754332));
#45588=CARTESIAN_POINT('Ctrl Pts',(46.0178706059924,2.73455201677989,15.5680874536012));
#45589=CARTESIAN_POINT('Ctrl Pts',(46.0641744361553,3.44250006963818,16.0924666576019));
#45590=CARTESIAN_POINT('Ctrl Pts',(46.1104782663182,3.981916078645,16.7542213605348));
#45591=CARTESIAN_POINT('Ctrl Pts',(46.1567820964811,4.52133208765183,17.4159760634677));
#45592=CARTESIAN_POINT('Ctrl Pts',(46.2030859266439,4.89221605280719,18.2151062653327));
#45593=CARTESIAN_POINT('Ctrl Pts',(46.2493897568068,5.04938791342566,19.0542641312032));
#45594=CARTESIAN_POINT('Ctrl Pts',(46.2956935869697,5.20655977404413,19.8934219970738));
#45595=CARTESIAN_POINT('Ctrl Pts',(46.3419974171325,5.15001953012569,20.7726075269498));
#45596=CARTESIAN_POINT('Ctrl Pts',(46.3883012472954,4.8866547580894,21.5847207668863));
#45597=CARTESIAN_POINT('Ctrl Pts',(46.4346050774583,4.62328998605311,22.3968340068228));
#45598=CARTESIAN_POINT('Ctrl Pts',(46.4809089076212,4.15310068589896,23.1418749568197));
#45599=CARTESIAN_POINT('Ctrl Pts',(46.5272127377841,3.53336402004704,23.7290847852619));
#45600=CARTESIAN_POINT('Ctrl Pts',(46.573516567947,2.91362735419512,24.316294613704));
#45601=CARTESIAN_POINT('Ctrl Pts',(46.6198203981098,2.14434332264542,24.7456733205914));
#45602=CARTESIAN_POINT('Ctrl Pts',(46.6661242282727,1.31922398226423,24.9649151773485));
#45603=CARTESIAN_POINT('Ctrl Pts',(46.7124280584356,0.494104641883048,25.1841570341056));
#45604=CARTESIAN_POINT('Ctrl Pts',(46.7587318885985,-0.386850007329603,
25.1932620407324));
#45605=CARTESIAN_POINT('Ctrl Pts',(46.8050357187614,-1.21632450220898,24.9911210503581));
#45606=CARTESIAN_POINT('Ctrl Pts',(46.8513395489243,-2.04579899708836,24.7889800599838));
#45607=CARTESIAN_POINT('Ctrl Pts',(46.8976433790871,-2.82379333763447,24.3755930726083));
#45608=CARTESIAN_POINT('Ctrl Pts',(46.94394720925,-3.45553440114763,23.8013177499372));
#45609=CARTESIAN_POINT('Ctrl Pts',(46.9902510394129,-4.0872754646608,23.2270424272662));
#45610=CARTESIAN_POINT('Ctrl Pts',(47.0365548695757,-4.57276325114104,22.4918787692994));
#45611=CARTESIAN_POINT('Ctrl Pts',(47.0828586997386,-4.85285697889777,21.6853823827887));
#45612=CARTESIAN_POINT('Ctrl Pts',(47.1138919647247,-5.04057844478594,21.1448608754995));
#45613=CARTESIAN_POINT('Ctrl Pts',(47.1449252297108,-5.13604085957544,20.572298081872));
#45614=CARTESIAN_POINT('Ctrl Pts',(47.1759584946969,-5.13650480025366,19.9998861825852));
#45615=CARTESIAN_POINT('Origin',(25.,0.,20.));
#45616=CARTESIAN_POINT('',(48.9259584946969,-5.13665113575917,20.0001315872378));
#45617=CARTESIAN_POINT('',(48.4490415053031,-5.1367692385953,19.9998673509107));
#45618=CARTESIAN_POINT('',(25.,-5.13675,20.));
#45619=CARTESIAN_POINT('',(50.,3.87994761181438,23.3663343702128));
#45620=CARTESIAN_POINT('Ctrl Pts',(48.9259584946969,-5.13665113575917,20.0001315872378));
#45621=CARTESIAN_POINT('Ctrl Pts',(48.9598455186578,-5.13603933143329,19.3751337947736));
#45622=CARTESIAN_POINT('Ctrl Pts',(48.9937325426186,-5.02179317828337,18.7499187416812));
#45623=CARTESIAN_POINT('Ctrl Pts',(49.0276195665795,-4.79876653798914,18.1662697419488));
#45624=CARTESIAN_POINT('Ctrl Pts',(49.0739233967424,-4.49401898370703,17.3687614039629));
#45625=CARTESIAN_POINT('Ctrl Pts',(49.1202272269053,-3.98616766501212,16.6488609360172));
#45626=CARTESIAN_POINT('Ctrl Pts',(49.1665310570682,-3.33707491734228,16.0942748452934));
#45627=CARTESIAN_POINT('Ctrl Pts',(49.212834887231,-2.68798216967244,15.5396887545696));
#45628=CARTESIAN_POINT('Ctrl Pts',(49.2591387173939,-1.89764799302765,15.1504170410676));
#45629=CARTESIAN_POINT('Ctrl Pts',(49.3054425475568,-1.0623540544481,14.9738595777119));
#45630=CARTESIAN_POINT('Ctrl Pts',(49.3517463777197,-0.22706011586855,14.7973021143561));
#45631=CARTESIAN_POINT('Ctrl Pts',(49.3980502078826,0.653193584645775,14.8334589011466));
#45632=CARTESIAN_POINT('Ctrl Pts',(49.4443540380455,1.47118750635313,15.0779651040003));
#45633=CARTESIAN_POINT('Ctrl Pts',(49.4906578682084,2.28918142806049,15.3224713068541));
#45634=CARTESIAN_POINT('Ctrl Pts',(49.5369616983712,3.04491557096088,15.7753269257712));
#45635=CARTESIAN_POINT('Ctrl Pts',(49.5832655285341,3.64630753914303,16.3812878173559));
#45636=CARTESIAN_POINT('Ctrl Pts',(49.6295693586969,4.24769950732517,16.9872487089406));
#45637=CARTESIAN_POINT('Ctrl Pts',(49.6758731888598,4.69474930078906,17.7463148731928));
#45638=CARTESIAN_POINT('Ctrl Pts',(49.7221770190227,4.93304205845025,18.5661776434962));
#45639=CARTESIAN_POINT('Ctrl Pts',(49.7684808491856,5.17133481611145,19.3860404137995));
#45640=CARTESIAN_POINT('Ctrl Pts',(49.8147846793485,5.20087053796993,20.2666997901539));
#45641=CARTESIAN_POINT('Ctrl Pts',(49.8610885095113,5.0179360691547,21.1005140400636));
#45642=CARTESIAN_POINT('Ctrl Pts',(49.9073923396742,4.83500160033947,21.9343282899734));
#45643=CARTESIAN_POINT('Ctrl Pts',(49.9536961698371,4.43959694085051,22.7212974134384));
#45644=CARTESIAN_POINT('Ctrl Pts',(50.,3.87994761181434,23.3663343702128));
#45645=CARTESIAN_POINT('',(50.,-3.88028650238532,23.366567607224));
#45646=CARTESIAN_POINT('Origin',(50.,0.,20.));
#45647=CARTESIAN_POINT('Ctrl Pts',(50.,-3.88028650238532,23.366567607224));
#45648=CARTESIAN_POINT('Ctrl Pts',(49.9564083618068,-3.35323397491262,23.9734064748655));
#45649=CARTESIAN_POINT('Ctrl Pts',(49.9128167236137,-2.68147453498408,24.4549327642161));
#45650=CARTESIAN_POINT('Ctrl Pts',(49.8692250854205,-1.93705761091916,24.7579923400498));
#45651=CARTESIAN_POINT('Ctrl Pts',(49.8229212552576,-1.14632442788237,25.0799077281905));
#45652=CARTESIAN_POINT('Ctrl Pts',(49.7766174250947,-0.273611264823877,
25.2004577954347));
#45653=CARTESIAN_POINT('Ctrl Pts',(49.7303135949318,0.574777228598876,25.1049377152569));
#45654=CARTESIAN_POINT('Ctrl Pts',(49.6840097647689,1.42316572202163,25.0094176350791));
#45655=CARTESIAN_POINT('Ctrl Pts',(49.6377059346061,2.24722954580865,24.6978274074791));
#45656=CARTESIAN_POINT('Ctrl Pts',(49.5914021044432,2.94658003659829,24.2081341237764));
#45657=CARTESIAN_POINT('Ctrl Pts',(49.5450982742803,3.64593052738793,23.7184408400736));
#45658=CARTESIAN_POINT('Ctrl Pts',(49.4987944441175,4.22056768518019,23.0506445002681));
#45659=CARTESIAN_POINT('Ctrl Pts',(49.4524906139546,4.60049256722468,22.2860891164051));
#45660=CARTESIAN_POINT('Ctrl Pts',(49.4061867837917,4.98041744926916,21.5215337325421));
#45661=CARTESIAN_POINT('Ctrl Pts',(49.3598829536288,5.16563005556587,20.6602193046217));
#45662=CARTESIAN_POINT('Ctrl Pts',(49.3135791234659,5.13356739906873,19.8070713658671));
#45663=CARTESIAN_POINT('Ctrl Pts',(49.2672752933031,5.10150474257159,18.9539234271126));
#45664=CARTESIAN_POINT('Ctrl Pts',(49.2209714631402,4.85216682328062,18.108941977524));
#45665=CARTESIAN_POINT('Ctrl Pts',(49.1746676329773,4.41592775461009,17.3750590101374));
#45666=CARTESIAN_POINT('Ctrl Pts',(49.1283638028144,3.97968868593957,16.6411760427509));
#45667=CARTESIAN_POINT('Ctrl Pts',(49.0820599726515,3.3565484678895,16.0183915575663));
#45668=CARTESIAN_POINT('Ctrl Pts',(49.0357561424887,2.62241608957914,15.5825721087253));
#45669=CARTESIAN_POINT('Ctrl Pts',(48.9894523123258,1.88828371126878,15.1467526598842));
#45670=CARTESIAN_POINT('Ctrl Pts',(48.9431484821629,1.04315917269814,14.8978982473866));
#45671=CARTESIAN_POINT('Ctrl Pts',(48.8968446520001,0.189993329665845,14.8663232896413));
#45672=CARTESIAN_POINT('Ctrl Pts',(48.8505408218372,-0.663172513366446,
14.834748331896));
#45673=CARTESIAN_POINT('Ctrl Pts',(48.8042369916742,-1.52437966086038,15.0204528289029));
#45674=CARTESIAN_POINT('Ctrl Pts',(48.7579331615114,-2.28871829557969,15.4008149437621));
#45675=CARTESIAN_POINT('Ctrl Pts',(48.7116293313485,-3.053056930299,15.7811770586214));
#45676=CARTESIAN_POINT('Ctrl Pts',(48.6653255011856,-3.72052705224367,16.3561967913331));
#45677=CARTESIAN_POINT('Ctrl Pts',(48.6190216710228,-4.20981926355514,17.0558267381184));
#45678=CARTESIAN_POINT('Ctrl Pts',(48.5727178408599,-4.69911147486661,17.7554566849037));
#45679=CARTESIAN_POINT('Ctrl Pts',(48.526414010697,-5.01022577554488,18.5796968457626));
#45680=CARTESIAN_POINT('Ctrl Pts',(48.4801101805341,-5.1052630958502,19.4281406043275));
#45681=CARTESIAN_POINT('Ctrl Pts',(48.4697539554571,-5.12651895905494,19.6179018940085));
#45682=CARTESIAN_POINT('Ctrl Pts',(48.4593977303801,-5.13696601854414,19.8088739185692));
#45683=CARTESIAN_POINT('Ctrl Pts',(48.4490415053031,-5.1367692385953,19.9998673509107));
#45684=CARTESIAN_POINT('Origin',(53.8647410325606,0.,20.));
#45685=CARTESIAN_POINT('',(0.635258967439483,-6.11286903553622,19.9998876627387));
#45686=CARTESIAN_POINT('',(0.489741032560566,-6.11272135172475,19.9999876119473));
#45687=CARTESIAN_POINT('',(53.8647410325606,-6.11325,19.9999999999994));
#45688=CARTESIAN_POINT('',(0.,1.1399249411295,26.0060300274883));
#45689=CARTESIAN_POINT('Ctrl Pts',(0.489741032560565,-6.11272135172475,
19.9999876119473));
#45690=CARTESIAN_POINT('Ctrl Pts',(0.465405512195678,-6.1126401423534,20.5342537111184));
#45691=CARTESIAN_POINT('Ctrl Pts',(0.394766161667913,-5.91134392484222,
22.0851281076538));
#45692=CARTESIAN_POINT('Ctrl Pts',(0.277822980977271,-4.61535544548857,
24.3940602366606));
#45693=CARTESIAN_POINT('Ctrl Pts',(0.138911490488638,-1.95089886648438,
26.0667560931559));
#45694=CARTESIAN_POINT('Ctrl Pts',(0.0463038301628798,0.141429157467205,
26.1955412757171));
#45695=CARTESIAN_POINT('Ctrl Pts',(0.,1.1399249411295,26.0060300274883));
#45696=CARTESIAN_POINT('',(3.4031358915606E-15,3.9853303828714,24.6362610213064));
#45697=CARTESIAN_POINT('Origin',(0.,0.,20.));
#45698=CARTESIAN_POINT('Ctrl Pts',(0.635258967439483,-6.11286903553622,
19.9998876627387));
#45699=CARTESIAN_POINT('Ctrl Pts',(0.606009106974798,-6.11244475391168,
20.6419943076294));
#45700=CARTESIAN_POINT('Ctrl Pts',(0.530455416347233,-5.85230460599341,
22.3009199263206));
#45701=CARTESIAN_POINT('Ctrl Pts',(0.408597895556788,-4.37627520273034,
24.6322128254603));
#45702=CARTESIAN_POINT('Ctrl Pts',(0.269686405068149,-1.62745906490466,
26.1612286823026));
#45703=CARTESIAN_POINT('Ctrl Pts',(0.133487106549218,1.45644183765853,26.1885630898315));
#45704=CARTESIAN_POINT('Ctrl Pts',(0.0435916381931709,3.25961188313384,
25.2594316761304));
#45705=CARTESIAN_POINT('Ctrl Pts',(2.63081657153608E-15,3.9853303828714,
24.6362610213064));
#45706=CARTESIAN_POINT('Origin',(53.8647410325606,0.,20.));
#45707=CARTESIAN_POINT('',(2.38525896743947,-6.11325364908754,20.0001583732729));
#45708=CARTESIAN_POINT('',(2.23974103256055,-6.11358099250321,20.0001166795099));
#45709=CARTESIAN_POINT('',(53.8647410325606,-6.11325,19.9999999999994));
#45710=CARTESIAN_POINT('Ctrl Pts',(2.23974103256055,-6.11358099250321,20.0001166795099));
#45711=CARTESIAN_POINT('Ctrl Pts',(2.23402197097976,-6.11369031868212,20.1256220477198));
#45712=CARTESIAN_POINT('Ctrl Pts',(2.18199907923609,-6.07925402918527,21.2672095839662));
#45713=CARTESIAN_POINT('Ctrl Pts',(2.08367235732954,-5.39798721704175,23.3868805022452));
#45714=CARTESIAN_POINT('Ctrl Pts',(1.94476086684091,-3.12038893862028,25.556293575601));
#45715=CARTESIAN_POINT('Ctrl Pts',(1.80584937635227,-0.0825561728535726,
26.3720021186908));
#45716=CARTESIAN_POINT('Ctrl Pts',(1.66693788586364,2.97538981548086,25.6352709416678));
#45717=CARTESIAN_POINT('Ctrl Pts',(1.528026395375,5.30842886408474,23.5255940754177));
#45718=CARTESIAN_POINT('Ctrl Pts',(1.38911490488636,6.34815042253135,20.5569597405651));
#45719=CARTESIAN_POINT('Ctrl Pts',(1.25020341439772,5.84124601468089,17.4526331642158));
#45720=CARTESIAN_POINT('Ctrl Pts',(1.11129192390908,3.91120805214414,14.9689283406313));
#45721=CARTESIAN_POINT('Ctrl Pts',(0.972380433420452,1.02827407433471,13.7109751703986));
#45722=CARTESIAN_POINT('Ctrl Pts',(0.833468942931815,-2.10520088120389,
13.985227291767));
#45723=CARTESIAN_POINT('Ctrl Pts',(0.694557452443171,-4.72574094137507,
15.7249208643558));
#45724=CARTESIAN_POINT('Ctrl Pts',(0.579981482319428,-5.93760230752943,
18.0188739705022));
#45725=CARTESIAN_POINT('Ctrl Pts',(0.511709342358557,-6.11279466154519,
19.5176916509335));
#45726=CARTESIAN_POINT('Ctrl Pts',(0.489741032560565,-6.11272135172475,
19.9999876119473));
#45727=CARTESIAN_POINT('Ctrl Pts',(2.38525896743947,-6.11325364908754,20.0001583732729));
#45728=CARTESIAN_POINT('Ctrl Pts',(2.37462556575888,-6.11349338758375,20.2335454665235));
#45729=CARTESIAN_POINT('Ctrl Pts',(2.31768833391541,-6.04330000224885,21.4830882729956));
#45730=CARTESIAN_POINT('Ctrl Pts',(2.21444727190907,-5.2112318370928,23.6677360978016));
#45731=CARTESIAN_POINT('Ctrl Pts',(2.07553578142043,-2.82204320093811,25.7136063473297));
#45732=CARTESIAN_POINT('Ctrl Pts',(1.93662429093179,0.254692459677778,26.3674451025059));
#45733=CARTESIAN_POINT('Ctrl Pts',(1.79771280044316,3.26937625297555,25.4699546773483));
#45734=CARTESIAN_POINT('Ctrl Pts',(1.65880130995452,5.48752727391192,23.2397947266211));
#45735=CARTESIAN_POINT('Ctrl Pts',(1.51988981946589,6.36872743946243,20.220309021366));
#45736=CARTESIAN_POINT('Ctrl Pts',(1.38097832897725,5.69828603890732,17.1471485537567));
#45737=CARTESIAN_POINT('Ctrl Pts',(1.24206683848861,3.63954565029315,14.7690408411714));
#45738=CARTESIAN_POINT('Ctrl Pts',(1.10315534799997,0.694086537873731,13.6653755651264));
#45739=CARTESIAN_POINT('Ctrl Pts',(0.964243857511333,-2.4204761475888,14.1050423605135));
#45740=CARTESIAN_POINT('Ctrl Pts',(0.8253323670227,-4.94532707163062,15.9809257548385));
#45741=CARTESIAN_POINT('Ctrl Pts',(0.715670736998751,-5.98738112992614,
18.2348148939576));
#45742=CARTESIAN_POINT('Ctrl Pts',(0.652312937137678,-6.11311641059558,
19.6255109275677));
#45743=CARTESIAN_POINT('Ctrl Pts',(0.635258967439483,-6.11286903553622,
19.9998876627387));
#45744=CARTESIAN_POINT('Origin',(53.8647410325606,0.,20.));
#45745=CARTESIAN_POINT('',(4.13525896743946,-6.11343686380434,19.9998556839975));
#45746=CARTESIAN_POINT('',(3.98974103256054,-6.1131009424828,19.999845624611));
#45747=CARTESIAN_POINT('',(53.8647410325606,-6.11325,19.9999999999994));
#45748=CARTESIAN_POINT('Ctrl Pts',(3.98974103256054,-6.11310094248279,19.999845624611));
#45749=CARTESIAN_POINT('Ctrl Pts',(3.95633459960097,-6.11239888135295,20.7331189949968));
#45750=CARTESIAN_POINT('Ctrl Pts',(3.87662433647851,-5.79731641090071,22.4833515156035));
#45751=CARTESIAN_POINT('Ctrl Pts',(3.75061024319318,-4.16456822152471,24.8234424569172));
#45752=CARTESIAN_POINT('Ctrl Pts',(3.61169875270454,-1.35007773082975,26.2278821221607));
#45753=CARTESIAN_POINT('Ctrl Pts',(3.47278726221591,1.79333824355105,26.1149949755885));
#45754=CARTESIAN_POINT('Ctrl Pts',(3.33387577172728,4.49983519042547,24.5122842181282));
#45755=CARTESIAN_POINT('Ctrl Pts',(3.19496428123863,6.11001713833909,21.8102254493376));
#45756=CARTESIAN_POINT('Ctrl Pts',(3.05605279075,6.23158824788668,18.6671333472082));
#45757=CARTESIAN_POINT('Ctrl Pts',(2.91714130026136,4.83492960625386,15.8487735173902));
#45758=CARTESIAN_POINT('Ctrl Pts',(2.77822980977273,2.26031541093747,14.041795584685));
#45759=CARTESIAN_POINT('Ctrl Pts',(2.63931831928409,-0.864989547684349,
13.6864416790982));
#45760=CARTESIAN_POINT('Ctrl Pts',(2.50040682879546,-3.77955323437126,14.8692882560822));
#45761=CARTESIAN_POINT('Ctrl Pts',(2.36721439988761,-5.69120430944527,17.2019907534407));
#45762=CARTESIAN_POINT('Ctrl Pts',(2.28032580114264,-6.11280516982525,19.109479946078));
#45763=CARTESIAN_POINT('Ctrl Pts',(2.23974103256055,-6.11358099250321,20.0001166795099));
#45764=CARTESIAN_POINT('Ctrl Pts',(4.13525896743946,-6.11343686380434,19.9998556839975));
#45765=CARTESIAN_POINT('Ctrl Pts',(4.09693819438009,-6.11259463033327,20.8408660932363));
#45766=CARTESIAN_POINT('Ctrl Pts',(4.01231359115783,-5.72621975022473,22.6988376413813));
#45767=CARTESIAN_POINT('Ctrl Pts',(3.8813851577727,-3.90353405789533,25.0370276152856));
#45768=CARTESIAN_POINT('Ctrl Pts',(3.74247366728407,-1.01867885543911,26.2905896963458));
#45769=CARTESIAN_POINT('Ctrl Pts',(3.60356217679543,2.11436163853657,26.0115472384233));
#45770=CARTESIAN_POINT('Ctrl Pts',(3.46465068630679,4.73227073773,24.2678846051763));
#45771=CARTESIAN_POINT('Ctrl Pts',(3.32573919581815,6.19723552447633,21.4844181326321));
#45772=CARTESIAN_POINT('Ctrl Pts',(3.18682770532951,6.15234006719685,18.3392962227209));
#45773=CARTESIAN_POINT('Ctrl Pts',(3.04791621484088,4.60852244721424,15.5987790112615));
#45774=CARTESIAN_POINT('Ctrl Pts',(2.90900472435224,1.94190986497335,13.9305509792932));
#45775=CARTESIAN_POINT('Ctrl Pts',(2.77009323386361,-1.19781891413772,13.7410499932924));
#45776=CARTESIAN_POINT('Ctrl Pts',(2.63118174337496,-4.04571770703044,15.0764450267472));
#45777=CARTESIAN_POINT('Ctrl Pts',(2.50290365456693,-5.76539070545534,17.4173429185103));
#45778=CARTESIAN_POINT('Ctrl Pts',(2.42092939592176,-6.11244943091349,19.2172463881382));
#45779=CARTESIAN_POINT('Ctrl Pts',(2.38525896743947,-6.11325364908754,20.0001583732729));
#45780=CARTESIAN_POINT('Origin',(53.8647410325606,0.,20.));
#45781=CARTESIAN_POINT('',(5.88525896743946,-6.11277390858896,20.0000683331812));
#45782=CARTESIAN_POINT('',(5.73974103256054,-6.1129851143326,20.0001404084395));
#45783=CARTESIAN_POINT('',(53.8647410325606,-6.11325,19.9999999999994));
#45784=CARTESIAN_POINT('Ctrl Pts',(5.73974103256054,-6.1129851143326,20.0001404084395));
#45785=CARTESIAN_POINT('Ctrl Pts',(5.72495105838506,-6.11325962756252,20.3247989551979));
#45786=CARTESIAN_POINT('Ctrl Pts',(5.6638572540467,-6.00826961576545,21.6657090484576));
#45787=CARTESIAN_POINT('Ctrl Pts',(5.55645961954546,-5.04185590001004,23.897295817673));
#45788=CARTESIAN_POINT('Ctrl Pts',(5.41754812905682,-2.56349596308158,25.8341849520033));
#45789=CARTESIAN_POINT('Ctrl Pts',(5.27863663856818,0.539419975483812,26.3496654791388));
#45790=CARTESIAN_POINT('Ctrl Pts',(5.13972514807955,3.51091460972764,25.3181485697674));
#45791=CARTESIAN_POINT('Ctrl Pts',(5.00081365759091,5.62702939460967,22.9909473079805));
#45792=CARTESIAN_POINT('Ctrl Pts',(4.86190216710228,6.37220580845331,19.9350481591359));
#45793=CARTESIAN_POINT('Ctrl Pts',(4.72299067661364,5.56489318441634,16.8949735181558));
#45794=CARTESIAN_POINT('Ctrl Pts',(4.584079186125,3.40178071249615,14.6113903842451));
#45795=CARTESIAN_POINT('Ctrl Pts',(4.44516769563636,0.409877171332637,13.6406583429304));
#45796=CARTESIAN_POINT('Ctrl Pts',(4.30625620514773,-2.68188658064232,14.2192811886858));
#45797=CARTESIAN_POINT('Ctrl Pts',(4.16734471465908,-5.12025029463462,16.2062864463399));
#45798=CARTESIAN_POINT('Ctrl Pts',(4.06183965713003,-6.02474970735384,18.4174444764408));
#45799=CARTESIAN_POINT('Ctrl Pts',(4.00263842976385,-6.1133719909142,19.7167469194031));
#45800=CARTESIAN_POINT('Ctrl Pts',(3.98974103256054,-6.11310094248279,19.999845624611));
#45801=CARTESIAN_POINT('Ctrl Pts',(5.88525896743946,-6.11277390858896,20.0000683331812));
#45802=CARTESIAN_POINT('Ctrl Pts',(5.86555465316417,-6.11294380838857,20.4326456386692));
#45803=CARTESIAN_POINT('Ctrl Pts',(5.79954650872601,-5.96128629022551,21.8816334848052));
#45804=CARTESIAN_POINT('Ctrl Pts',(5.68723453412497,-4.82859400298248,24.1585941485866));
#45805=CARTESIAN_POINT('Ctrl Pts',(5.54832304363634,-2.25122745380935,25.9616440928248));
#45806=CARTESIAN_POINT('Ctrl Pts',(5.4094115531477,0.874615721648888,26.3122319885871));
#45807=CARTESIAN_POINT('Ctrl Pts',(5.27050006265906,3.78737235203403,25.1249425367847));
#45808=CARTESIAN_POINT('Ctrl Pts',(5.13158857217043,5.77739449523354,22.6890403836206));
#45809=CARTESIAN_POINT('Ctrl Pts',(4.99267708168179,6.35984414454672,19.5979952794158));
#45810=CARTESIAN_POINT('Ctrl Pts',(4.85376559119316,5.39281648351639,16.604892385592));
#45811=CARTESIAN_POINT('Ctrl Pts',(4.71485410070452,3.11191279185723,14.4389547642397));
#45812=CARTESIAN_POINT('Ctrl Pts',(4.57594261021589,0.0728398505813112,
13.6278794978073));
#45813=CARTESIAN_POINT('Ctrl Pts',(4.43703111972725,-2.98397938969178,14.3692724857092));
#45814=CARTESIAN_POINT('Ctrl Pts',(4.29811962923861,-5.31379836804421,16.4825048341088));
#45815=CARTESIAN_POINT('Ctrl Pts',(4.19752891180935,-6.06341926380413,18.6333427654839));
#45816=CARTESIAN_POINT('Ctrl Pts',(4.14324202454297,-6.11361231949996,19.8246547789638));
#45817=CARTESIAN_POINT('Ctrl Pts',(4.13525896743946,-6.11343686380434,19.9998556839975));
#45818=CARTESIAN_POINT('Origin',(53.8647410325606,0.,20.));
#45819=CARTESIAN_POINT('',(7.63525896743946,-6.11376652953962,20.0000252316214));
#45820=CARTESIAN_POINT('',(7.48974103256053,-6.11368021756426,19.9999161056822));
#45821=CARTESIAN_POINT('',(53.8647410325606,-6.11325,19.9999999999994));
#45822=CARTESIAN_POINT('Ctrl Pts',(7.48974103256053,-6.11368021756426,19.9999161056822));
#45823=CARTESIAN_POINT('Ctrl Pts',(7.44726368700626,-6.11305136260232,20.9320417877776));
#45824=CARTESIAN_POINT('Ctrl Pts',(7.35848251128911,-5.66082090355657,22.8808510542445));
#45825=CARTESIAN_POINT('Ctrl Pts',(7.2233975054091,-3.67418420606118,25.206687625242));
#45826=CARTESIAN_POINT('Ctrl Pts',(7.08448601492046,-0.73611510378342,26.3298783685707));
#45827=CARTESIAN_POINT('Ctrl Pts',(6.94557452443182,2.38129701778703,25.9108924977533));
#45828=CARTESIAN_POINT('Ctrl Pts',(6.80666303394318,4.91854308270761,24.0518094168491));
#45829=CARTESIAN_POINT('Ctrl Pts',(6.66775154345454,6.2574624695857,21.2055658624248));
#45830=CARTESIAN_POINT('Ctrl Pts',(6.5288400529659,6.07184825208871,18.0656048980302));
#45831=CARTESIAN_POINT('Ctrl Pts',(6.38992856247727,4.40692245326515,15.3969292751659));
#45832=CARTESIAN_POINT('Ctrl Pts',(6.25101707198863,1.66831840155036,13.8497203870096));
#45833=CARTESIAN_POINT('Ctrl Pts',(6.11210558150001,-1.47674553359532,13.8009316638769));
#45834=CARTESIAN_POINT('Ctrl Pts',(5.97319409101137,-4.26202334105436,15.2624497208763));
#45835=CARTESIAN_POINT('Ctrl Pts',(5.84907257469821,-5.82293180962636,17.5996983337315));
#45836=CARTESIAN_POINT('Ctrl Pts',(5.77125488854794,-6.11240019306826,19.3083716084245));
#45837=CARTESIAN_POINT('Ctrl Pts',(5.73974103256054,-6.1129851143326,20.0001404084395));
#45838=CARTESIAN_POINT('Ctrl Pts',(7.63525896743946,-6.11376652953962,20.0000252316214));
#45839=CARTESIAN_POINT('Ctrl Pts',(7.63417111194827,-6.1137720723984,20.0238962246036));
#45840=CARTESIAN_POINT('Ctrl Pts',(7.5867794262942,-6.10780882306453,21.0638170421152));
#45841=CARTESIAN_POINT('Ctrl Pts',(7.49308391047725,-5.56015202049796,23.1135084466321));
#45842=CARTESIAN_POINT('Ctrl Pts',(7.35417241998862,-3.39355996620412,25.3937905126241));
#45843=CARTESIAN_POINT('Ctrl Pts',(7.21526092949997,-0.400179699901651,
26.3599592409137));
#45844=CARTESIAN_POINT('Ctrl Pts',(7.07634943901134,2.69069813882,25.7766226174165));
#45845=CARTESIAN_POINT('Ctrl Pts',(6.93743794852271,5.12602914017768,23.7859015560823));
#45846=CARTESIAN_POINT('Ctrl Pts',(6.79852645803408,6.31248270612288,20.8728043441669));
#45847=CARTESIAN_POINT('Ctrl Pts',(6.65961496754543,5.96099784106742,17.7470619011862));
#45848=CARTESIAN_POINT('Ctrl Pts',(6.5207034770568,4.15720837674583,15.1702128565938));
#45849=CARTESIAN_POINT('Ctrl Pts',(6.38179198656816,1.34057961829449,13.7700664830746));
#45850=CARTESIAN_POINT('Ctrl Pts',(6.24288049607952,-1.80266055610438,13.8877467119104));
#45851=CARTESIAN_POINT('Ctrl Pts',(6.10396900559088,-4.50671046633138,15.4945825819403));
#45852=CARTESIAN_POINT('Ctrl Pts',(5.98476182937753,-5.88495397728115,17.8154640682276));
#45853=CARTESIAN_POINT('Ctrl Pts',(5.91185848332706,-6.11254455514097,19.416117694291));
#45854=CARTESIAN_POINT('Ctrl Pts',(5.88525896743946,-6.11277390858896,20.0000683331812));
#45855=CARTESIAN_POINT('Origin',(53.8647410325606,0.,20.));
#45856=CARTESIAN_POINT('',(9.38525896743945,-6.11284857941777,19.9998944676288));
#45857=CARTESIAN_POINT('',(9.23974103256053,-6.11272951804558,19.9999855091883));
#45858=CARTESIAN_POINT('',(53.8647410325606,-6.11325,19.9999999999994));
#45859=CARTESIAN_POINT('Ctrl Pts',(9.23974103256053,-6.11272951804558,19.9999855091883));
#45860=CARTESIAN_POINT('Ctrl Pts',(9.21588014579035,-6.11268627364501,20.523824732368));
#45861=CARTESIAN_POINT('Ctrl Pts',(9.14571542885729,-5.91674747053061,22.0642447887842));
#45862=CARTESIAN_POINT('Ctrl Pts',(9.02924688176137,-4.63763254324486,24.3705365804159));
#45863=CARTESIAN_POINT('Ctrl Pts',(8.89033539127272,-1.98215097657166,26.0564265960212));
#45864=CARTESIAN_POINT('Ctrl Pts',(8.7514239007841,1.15625090922707,26.2667622774308));
#45865=CARTESIAN_POINT('Ctrl Pts',(8.61251241029546,4.01295020795098,24.9502986006324));
#45866=CARTESIAN_POINT('Ctrl Pts',(8.47360091980683,5.8919564762427,22.4277715067483));
#45867=CARTESIAN_POINT('Ctrl Pts',(8.33468942931819,6.33547900216983,19.3137555683411));
#45868=CARTESIAN_POINT('Ctrl Pts',(8.19577793882954,5.23546040650557,16.3669324340401));
#45869=CARTESIAN_POINT('Ctrl Pts',(8.05686644834092,2.85990314594527,14.3052498208675));
#45870=CARTESIAN_POINT('Ctrl Pts',(7.91795495785227,-0.212425125618811,
13.6310046967419));
#45871=CARTESIAN_POINT('Ctrl Pts',(7.77904346736364,-3.23299931252101,14.5084664207386));
#45872=CARTESIAN_POINT('Ctrl Pts',(7.64013197687499,-5.46590339851313,16.7238550634869));
#45873=CARTESIAN_POINT('Ctrl Pts',(7.54369783194064,-6.09154300913412,18.8159145025665));
#45874=CARTESIAN_POINT('Ctrl Pts',(7.49356751716914,-6.11373686667455,19.9159474741849));
#45875=CARTESIAN_POINT('Ctrl Pts',(7.48974103256053,-6.11368021756426,19.9999161056822));
#45876=CARTESIAN_POINT('Ctrl Pts',(9.38525896743944,-6.11284857941777,19.9998944676288));
#45877=CARTESIAN_POINT('Ctrl Pts',(9.35648374056947,-6.11245938709689,20.6315873376648));
#45878=CARTESIAN_POINT('Ctrl Pts',(9.28140468353662,-5.85828893938936,22.2800786383337));
#45879=CARTESIAN_POINT('Ctrl Pts',(9.16002179634088,-4.39989835807759,24.6097852202552));
#45880=CARTESIAN_POINT('Ctrl Pts',(9.02111030585225,-1.65893824958895,26.152816365076));
#45881=CARTESIAN_POINT('Ctrl Pts',(8.88219881536361,1.48619641390095,26.1968093046023));
#45882=CARTESIAN_POINT('Ctrl Pts',(8.74328732487498,4.26924238941132,24.7310458419625));
#45883=CARTESIAN_POINT('Ctrl Pts',(8.60437583438633,6.01215372256228,22.1126364937154));
#45884=CARTESIAN_POINT('Ctrl Pts',(8.4654643438977,6.29029711994617,18.9795160554453));
#45885=CARTESIAN_POINT('Ctrl Pts',(8.32655285340906,5.03590726004376,16.0950206906393));
#45886=CARTESIAN_POINT('Ctrl Pts',(8.18764136292043,2.55459676198038,14.1619129227137));
#45887=CARTESIAN_POINT('Ctrl Pts',(8.04872987243179,-0.549101585502231,
13.6511644542408));
#45888=CARTESIAN_POINT('Ctrl Pts',(7.90981838194317,-3.51901985465715,14.6872112218886));
#45889=CARTESIAN_POINT('Ctrl Pts',(7.7719947469457,-5.61503946859896,16.9993862869652));
#45890=CARTESIAN_POINT('Ctrl Pts',(7.68047494211115,-6.11353614437879,19.0078436203562));
#45891=CARTESIAN_POINT('Ctrl Pts',(7.63525896743946,-6.11376652953962,20.0000252316214));
#45892=CARTESIAN_POINT('Origin',(53.8647410325606,0.,20.));
#45893=CARTESIAN_POINT('',(11.1352589674394,-6.11328663918834,20.0001573543196));
#45894=CARTESIAN_POINT('',(10.9897410325605,-6.11360815273101,20.0001092168757));
#45895=CARTESIAN_POINT('',(53.8647410325606,-6.11325,19.9999999999994));
#45896=CARTESIAN_POINT('Ctrl Pts',(10.9897410325605,-6.11360815273101,20.0001092168757));
#45897=CARTESIAN_POINT('Ctrl Pts',(10.9844966045744,-6.11370363815739,20.1151972238524));
#45898=CARTESIAN_POINT('Ctrl Pts',(10.9329483464255,-6.08241679304912,21.2463623732547));
#45899=CARTESIAN_POINT('Ctrl Pts',(10.8350962581136,-5.41523157606947,23.3592398819462));
#45900=CARTESIAN_POINT('Ctrl Pts',(10.696184767625,-3.14875378158332,25.5402685160452));
#45901=CARTESIAN_POINT('Ctrl Pts',(10.5572732771364,-0.115131002167762,
26.3714967204933));
#45902=CARTESIAN_POINT('Ctrl Pts',(10.4183617866477,2.94654165889923,25.6504086453361));
#45903=CARTESIAN_POINT('Ctrl Pts',(10.2794502961591,5.29033518005657,23.5526862075862));
#45904=CARTESIAN_POINT('Ctrl Pts',(10.1405388056704,6.34522064949098,20.5894069190218));
#45905=CARTESIAN_POINT('Ctrl Pts',(10.0016273151818,5.854191596171,17.4825277832241));
#45906=CARTESIAN_POINT('Ctrl Pts',(9.86271582469318,3.9368796273414,14.9889916776419));
#45907=CARTESIAN_POINT('Ctrl Pts',(9.72380433420454,1.06040804430175,13.716309970527));
#45908=CARTESIAN_POINT('Ctrl Pts',(9.58489284371591,-2.07441549941601,13.974551805658));
#45909=CARTESIAN_POINT('Ctrl Pts',(9.44598135322726,-4.70383990511773,15.7008005682523));
#45910=CARTESIAN_POINT('Ctrl Pts',(9.33093074950883,-5.93244129797807,17.998045990015));
#45911=CARTESIAN_POINT('Ctrl Pts',(9.26218397595324,-6.1127701926292,19.5072756553621));
#45912=CARTESIAN_POINT('Ctrl Pts',(9.23974103256053,-6.11272951804558,19.9999855091883));
#45913=CARTESIAN_POINT('Ctrl Pts',(11.1352589674394,-6.11328663918834,20.0001573543196));
#45914=CARTESIAN_POINT('Ctrl Pts',(11.1251001993536,-6.11351667627268,20.2231234942924));
#45915=CARTESIAN_POINT('Ctrl Pts',(11.0686376011048,-6.04702917925912,21.4622364723876));
#45916=CARTESIAN_POINT('Ctrl Pts',(10.9658711726931,-5.22991444725156,23.6410465820594));
#45917=CARTESIAN_POINT('Ctrl Pts',(10.8269596822045,-2.85121621531744,25.699104441209));
#45918=CARTESIAN_POINT('Ctrl Pts',(10.6880481917159,0.222136591808738,26.3686639629421));
#45919=CARTESIAN_POINT('Ctrl Pts',(10.5491367012273,3.24136926627416,25.486597362478));
#45920=CARTESIAN_POINT('Ctrl Pts',(10.4102252107386,5.47089263051329,23.267806475863));
#45921=CARTESIAN_POINT('Ctrl Pts',(10.27131372025,6.36751792278091,20.2528652632554));
#45922=CARTESIAN_POINT('Ctrl Pts',(10.1324022297613,5.71279630774815,17.1763173541497));
#45923=CARTESIAN_POINT('Ctrl Pts',(9.99349073927272,3.66624054453745,14.7877158934027));
#45924=CARTESIAN_POINT('Ctrl Pts',(9.85457924878407,0.726462178868265,13.6690065518142));
#45925=CARTESIAN_POINT('Ctrl Pts',(9.71566775829543,-2.39030742076759,14.0927454962123));
#45926=CARTESIAN_POINT('Ctrl Pts',(9.5767562678068,-4.92471571892393,15.9556953099351));
#45927=CARTESIAN_POINT('Ctrl Pts',(9.46662000418813,-5.98283846110334,18.2139615092778));
#45928=CARTESIAN_POINT('Ctrl Pts',(9.40278757073235,-6.11308565827133,19.6150949394844));
#45929=CARTESIAN_POINT('Ctrl Pts',(9.38525896743944,-6.11284857941777,19.9998944676288));
#45930=CARTESIAN_POINT('Origin',(53.8647410325606,0.,20.));
#45931=CARTESIAN_POINT('',(12.8852589674394,-6.11340458852378,19.9998516759371));
#45932=CARTESIAN_POINT('',(12.7397410325605,-6.11307060053939,19.9998482593178));
#45933=CARTESIAN_POINT('',(53.8647410325606,-6.11325,19.9999999999994));
#45934=CARTESIAN_POINT('Ctrl Pts',(12.7397410325605,-6.11307060053939,19.9998482593178));
#45935=CARTESIAN_POINT('Ctrl Pts',(12.7068092331956,-6.11239576113666,20.7227136938253));
#45936=CARTESIAN_POINT('Ctrl Pts',(12.6275736036679,-5.80383176099062,22.462526520406));
#45937=CARTESIAN_POINT('Ctrl Pts',(12.5020341439773,-4.1891728722864,24.8020887385612));
#45938=CARTESIAN_POINT('Ctrl Pts',(12.3631226534886,-1.38189913347912,26.2208986804004));
#45939=CARTESIAN_POINT('Ctrl Pts',(12.224211163,1.76205287980219,26.124083217568));
#45940=CARTESIAN_POINT('Ctrl Pts',(12.0852996725114,4.4767080589433,24.5352299348445));
#45941=CARTESIAN_POINT('Ctrl Pts',(11.9463881820227,6.1006828055596,21.8414382728907));
#45942=CARTESIAN_POINT('Ctrl Pts',(11.8074766915341,6.23832087945686,18.6990087579656));
#45943=CARTESIAN_POINT('Ctrl Pts',(11.6685652010455,4.85608890030431,15.8735455655904));
#45944=CARTESIAN_POINT('Ctrl Pts',(11.5296537105568,2.29074623525794,14.0534289466476));
#45945=CARTESIAN_POINT('Ctrl Pts',(11.3907422200682,-0.832701193775514,
13.6821020640721));
#45946=CARTESIAN_POINT('Ctrl Pts',(11.2518307295795,-3.75327390186831,14.8500329491858));
#45947=CARTESIAN_POINT('Ctrl Pts',(11.118163667077,-5.68368017920984,17.1812096389043));
#45948=CARTESIAN_POINT('Ctrl Pts',(11.0308004347373,-6.11286058320882,19.0990681926252));
#45949=CARTESIAN_POINT('Ctrl Pts',(10.9897410325605,-6.11360815273101,20.0001092168757));
#45950=CARTESIAN_POINT('Ctrl Pts',(12.8852589674394,-6.11340458852378,19.9998516759371));
#45951=CARTESIAN_POINT('Ctrl Pts',(12.8474128279748,-6.11256107075738,20.8304581458768));
#45952=CARTESIAN_POINT('Ctrl Pts',(12.7632628583472,-5.73337822611735,22.6780379247862));
#45953=CARTESIAN_POINT('Ctrl Pts',(12.6328090585568,-3.92923403963699,25.0170056009591));
#45954=CARTESIAN_POINT('Ctrl Pts',(12.4938975680681,-1.05082517123617,26.285299658552));
#45955=CARTESIAN_POINT('Ctrl Pts',(12.3549860775795,2.0836009395627,26.0222780127582));
#45956=CARTESIAN_POINT('Ctrl Pts',(12.2160745870909,4.71039002242726,24.2920218050372));
#45957=CARTESIAN_POINT('Ctrl Pts',(12.0771630966022,6.1895656895012,21.5160811039145));
#45958=CARTESIAN_POINT('Ctrl Pts',(11.9382516061136,6.1607497487956,18.370770773951));
#45959=CARTESIAN_POINT('Ctrl Pts',(11.799340115625,4.63096275699136,15.6223968565371));
#45960=CARTESIAN_POINT('Ctrl Pts',(11.6604286251363,1.97291356977519,13.9405579972662));
#45961=CARTESIAN_POINT('Ctrl Pts',(11.5215171346477,-1.1658053857806,13.7350081292326));
#45962=CARTESIAN_POINT('Ctrl Pts',(11.3826056441591,-4.02049395435078,15.0558262873028));
#45963=CARTESIAN_POINT('Ctrl Pts',(11.2538529217563,-5.75851899348006,17.3965308011831));
#45964=CARTESIAN_POINT('Ctrl Pts',(11.1714040295164,-6.11246816350081,19.2068402018603));
#45965=CARTESIAN_POINT('Ctrl Pts',(11.1352589674394,-6.11328663918834,20.0001573543196));
#45966=CARTESIAN_POINT('Origin',(53.8647410325606,0.,20.));
#45967=CARTESIAN_POINT('',(14.6352589674394,-6.11278735830072,20.0000770013196));
#45968=CARTESIAN_POINT('',(14.4897410325605,-6.11301278051747,20.0001447615033));
#45969=CARTESIAN_POINT('',(53.8647410325606,-6.11325,19.9999999999994));
#45970=CARTESIAN_POINT('Ctrl Pts',(14.4897410325605,-6.11301278051747,20.0001447615033));
#45971=CARTESIAN_POINT('Ctrl Pts',(14.4754256919797,-6.11328857136773,20.3143804240189));
#45972=CARTESIAN_POINT('Ctrl Pts',(14.4148065212361,-6.01248627071629,21.6448549593419));
#45973=CARTESIAN_POINT('Ctrl Pts',(14.3078835203295,-5.06171431056786,23.8714692101462));
#45974=CARTESIAN_POINT('Ctrl Pts',(14.1689720298409,-2.59328879522498,25.8210032495677));
#45975=CARTESIAN_POINT('Ctrl Pts',(14.0300605393523,0.506951282871708,26.3523401989906));
#45976=CARTESIAN_POINT('Ctrl Pts',(13.8911490488636,3.48368054963307,25.3360280579309));
#45977=CARTESIAN_POINT('Ctrl Pts',(13.752237558375,5.6116651230563,23.0196755046844));
#45978=CARTESIAN_POINT('Ctrl Pts',(13.6133260678864,6.37245459172572,19.967625885163));
#45979=CARTESIAN_POINT('Ctrl Pts',(13.4744145773977,5.58069441033177,16.9234637162209));
#45980=CARTESIAN_POINT('Ctrl Pts',(13.3355030869091,3.42928465762181,14.6288518598053));
#45981=CARTESIAN_POINT('Ctrl Pts',(13.1965915964205,0.442382926346631,13.6428368784973));
#45982=CARTESIAN_POINT('Ctrl Pts',(13.0576801059318,-2.65229853840607,14.205646017882));
#45983=CARTESIAN_POINT('Ctrl Pts',(12.9187686154432,-5.10078863240939,16.1801595668928));
#45984=CARTESIAN_POINT('Ctrl Pts',(12.8127889243194,-6.02070026988043,18.3965909557952));
#45985=CARTESIAN_POINT('Ctrl Pts',(12.7531130633585,-6.11334462058844,19.7063271326415));
#45986=CARTESIAN_POINT('Ctrl Pts',(12.7397410325605,-6.11307060053939,19.9998482593178));
#45987=CARTESIAN_POINT('Ctrl Pts',(14.6352589674394,-6.11278735830072,20.0000770013196));
#45988=CARTESIAN_POINT('Ctrl Pts',(14.6160292867589,-6.11297471112037,20.4222318127276));
#45989=CARTESIAN_POINT('Ctrl Pts',(14.5504957759154,-5.96609040238597,21.8607796245411));
#45990=CARTESIAN_POINT('Ctrl Pts',(14.4386584349091,-4.84979104615329,24.133854393535));
#45991=CARTESIAN_POINT('Ctrl Pts',(14.2997469444204,-2.28167598106183,25.950057147267));
#45992=CARTESIAN_POINT('Ctrl Pts',(14.1608354539318,0.842334021367499,26.3166208319594));
#45993=CARTESIAN_POINT('Ctrl Pts',(14.0219239634432,3.7611224139311,25.1442378955218));
#45994=CARTESIAN_POINT('Ctrl Pts',(13.8830124729545,5.76357170928461,22.7185412430624));
#45995=CARTESIAN_POINT('Ctrl Pts',(13.7441009824659,6.36181621799531,19.6305142130623));
#45996=CARTESIAN_POINT('Ctrl Pts',(13.6051894919773,5.41010295127669,16.6325066600089));
#45997=CARTESIAN_POINT('Ctrl Pts',(13.4662780014886,3.14030207437455,14.4549365900852));
#45998=CARTESIAN_POINT('Ctrl Pts',(13.327366511,0.105415339819669,13.6283351512789));
#45999=CARTESIAN_POINT('Ctrl Pts',(13.1884550205113,-2.95515420605895,14.354090953911));
#46000=CARTESIAN_POINT('Ctrl Pts',(13.0495435300227,-5.29574629859371,16.4553848616206));
#46001=CARTESIAN_POINT('Ctrl Pts',(12.9484781789987,-6.05994210690123,18.6124928036776));
#46002=CARTESIAN_POINT('Ctrl Pts',(12.8937166581377,-6.11359309420672,19.8142313533877));
#46003=CARTESIAN_POINT('Ctrl Pts',(12.8852589674394,-6.11340458852378,19.9998516759371));
#46004=CARTESIAN_POINT('Origin',(53.8647410325606,0.,20.));
#46005=CARTESIAN_POINT('',(16.3852589674394,-6.1137723837536,20.0000142741886));
#46006=CARTESIAN_POINT('',(16.2397410325605,-6.11365777682639,19.9999071565179));
#46007=CARTESIAN_POINT('',(53.8647410325606,-6.11325,19.9999999999994));
#46008=CARTESIAN_POINT('Ctrl Pts',(16.2397410325605,-6.11365777682639,19.9999071565179));
#46009=CARTESIAN_POINT('Ctrl Pts',(16.197738320601,-6.11298318269978,20.9216272610411));
#46010=CARTESIAN_POINT('Ctrl Pts',(16.1094317784785,-5.66853645373843,22.8600809899514));
#46011=CARTESIAN_POINT('Ctrl Pts',(15.9748214061932,-3.70075454447885,25.1878359080099));
#46012=CARTESIAN_POINT('Ctrl Pts',(15.8359099157046,-0.768465969166765,
26.3260323790785));
#46013=CARTESIAN_POINT('Ctrl Pts',(15.6969984252159,2.35104741164878,25.9229892516446));
#46014=CARTESIAN_POINT('Ctrl Pts',(15.5580869347273,4.89776458282526,24.0769017278002));
#46015=CARTESIAN_POINT('Ctrl Pts',(15.4191754442386,6.25121743493832,21.2375403783475));
#46016=CARTESIAN_POINT('Ctrl Pts',(15.28026395375,6.08165818843483,18.096671524418));
#46017=CARTESIAN_POINT('Ctrl Pts',(15.1413524632613,4.43039732188061,15.4195191107057));
#46018=CARTESIAN_POINT('Ctrl Pts',(15.0024409727728,1.69973891506645,13.8583297689044));
#46019=CARTESIAN_POINT('Ctrl Pts',(14.8635294822841,-1.44503449559759,13.7934630498602));
#46020=CARTESIAN_POINT('Ctrl Pts',(14.7246179917955,-4.23774768077446,15.2407227228278));
#46021=CARTESIAN_POINT('Ctrl Pts',(14.6000218418876,-5.81659899729983,17.5788677726848));
#46022=CARTESIAN_POINT('Ctrl Pts',(14.5217295221426,-6.11239650927398,19.2979662726303));
#46023=CARTESIAN_POINT('Ctrl Pts',(14.4897410325605,-6.11301278051747,20.0001447615033));
#46024=CARTESIAN_POINT('Ctrl Pts',(16.3852589674394,-6.1137723837536,20.0000142741886));
#46025=CARTESIAN_POINT('Ctrl Pts',(16.384645745543,-6.11377420047576,20.0134702661335));
#46026=CARTESIAN_POINT('Ctrl Pts',(16.3377286934836,-6.11044645114222,21.0429751237547));
#46027=CARTESIAN_POINT('Ctrl Pts',(16.2445078112613,-5.57599667105201,23.0850423761618));
#46028=CARTESIAN_POINT('Ctrl Pts',(16.1055963207727,-3.42109050526117,25.3763709966026));
#46029=CARTESIAN_POINT('Ctrl Pts',(15.9666848302841,-0.432688738940727,
26.3578302740393));
#46030=CARTESIAN_POINT('Ctrl Pts',(15.8277733397954,2.66113092256575,25.7903028894231));
#46031=CARTESIAN_POINT('Ctrl Pts',(15.6888618493068,5.10660734001576,23.8120580810363));
#46032=CARTESIAN_POINT('Ctrl Pts',(15.5499503588182,6.30793814220377,20.9050644907565));
#46033=CARTESIAN_POINT('Ctrl Pts',(15.4110388683295,5.97243772585063,17.7775659854265));
#46034=CARTESIAN_POINT('Ctrl Pts',(15.2721273778409,4.1818455598703,15.1915290318346));
#46035=CARTESIAN_POINT('Ctrl Pts',(15.1332158873523,1.37241163250246,13.777001394081));
#46036=CARTESIAN_POINT('Ctrl Pts',(14.9943043968636,-1.77138908698832,13.8786107752573));
#46037=CARTESIAN_POINT('Ctrl Pts',(14.855392906375,-4.48361835037166,15.4716016267882));
#46038=CARTESIAN_POINT('Ctrl Pts',(14.7357110965669,-5.87924374865939,17.7946193487845));
#46039=CARTESIAN_POINT('Ctrl Pts',(14.6623331169217,-6.11252357762077,19.4057102690483));
#46040=CARTESIAN_POINT('Ctrl Pts',(14.6352589674394,-6.11278735830072,20.0000770013196));
#46041=CARTESIAN_POINT('Origin',(53.8647410325606,0.,20.));
#46042=CARTESIAN_POINT('',(18.1352589674394,-6.11282951797325,19.9999019817517));
#46043=CARTESIAN_POINT('',(17.9897410325605,-6.11272775120567,19.9999952045773));
#46044=CARTESIAN_POINT('',(53.8647410325606,-6.11325,19.9999999999994));
#46045=CARTESIAN_POINT('Ctrl Pts',(17.9897410325605,-6.11272775120567,19.9999952045773));
#46046=CARTESIAN_POINT('Ctrl Pts',(17.966354779385,-6.11271372992993,20.5134147996941));
#46047=CARTESIAN_POINT('Ctrl Pts',(17.8966646960467,-5.92205872661351,22.0433945389182));
#46048=CARTESIAN_POINT('Ctrl Pts',(17.7806707825455,-4.65991560350942,24.3467703154281));
#46049=CARTESIAN_POINT('Ctrl Pts',(17.6417592920568,-2.01308758044197,26.0462140220462));
#46050=CARTESIAN_POINT('Ctrl Pts',(17.5028478015682,1.12419798509589,26.2725915296011));
#46051=CARTESIAN_POINT('Ctrl Pts',(17.3639363110796,3.98759016100821,24.9707494721368));
#46052=CARTESIAN_POINT('Ctrl Pts',(17.2250248205909,5.87946788829534,22.4578614601765));
#46053=CARTESIAN_POINT('Ctrl Pts',(17.0861133301023,6.33890452382744,19.3461536535871));
#46054=CARTESIAN_POINT('Ctrl Pts',(16.9472018396136,5.25396546258616,16.3937453605064));
#46055=CARTESIAN_POINT('Ctrl Pts',(16.808290349125,2.88897926676432,14.3199450352023));
#46056=CARTESIAN_POINT('Ctrl Pts',(16.6693788586364,-0.179861885588608,
13.630001938067));
#46057=CARTESIAN_POINT('Ctrl Pts',(16.5304673681478,-3.2048824812767,14.4920099956406));
#46058=CARTESIAN_POINT('Ctrl Pts',(16.3915558776591,-5.44908320556687,16.6959543245097));
#46059=CARTESIAN_POINT('Ctrl Pts',(16.29464709913,-6.08854185718405,18.7950688508708));
#46060=CARTESIAN_POINT('Ctrl Pts',(16.2440421507638,-6.11372685591539,19.9055221291));
#46061=CARTESIAN_POINT('Ctrl Pts',(16.2397410325605,-6.11365777682639,19.9999071565179));
#46062=CARTESIAN_POINT('Ctrl Pts',(18.1352589674394,-6.11282951797326,19.9999019817517));
#46063=CARTESIAN_POINT('Ctrl Pts',(18.1069583741642,-6.11247543877291,20.6211809276915));
#46064=CARTESIAN_POINT('Ctrl Pts',(18.032353950726,-5.86421293859169,22.2592379783294));
#46065=CARTESIAN_POINT('Ctrl Pts',(17.911445697125,-4.42340764526233,24.5872312065266));
#46066=CARTESIAN_POINT('Ctrl Pts',(17.7725342066364,-1.6903718544226,26.1442549045489));
#46067=CARTESIAN_POINT('Ctrl Pts',(17.6336227161477,1.45449680133364,26.2043262642456));
#46068=CARTESIAN_POINT('Ctrl Pts',(17.4947112256591,4.24499988768104,24.7528098312351));
#46069=CARTESIAN_POINT('Ctrl Pts',(17.3557997351704,6.00127464093126,22.1433450544447));
#46070=CARTESIAN_POINT('Ctrl Pts',(17.2168882446818,6.29543197779222,19.0116875234582));
#46071=CARTESIAN_POINT('Ctrl Pts',(17.0779767541932,5.05580502895429,16.1208169871096));
#46072=CARTESIAN_POINT('Ctrl Pts',(16.9390652637045,2.5844096594071,14.1750491804084));
#46073=CARTESIAN_POINT('Ctrl Pts',(16.8001537732159,-0.516637009270994,
13.6484402278693));
#46074=CARTESIAN_POINT('Ctrl Pts',(16.6612422827273,-3.49181308971526,14.6692902269219));
#46075=CARTESIAN_POINT('Ctrl Pts',(16.5229440141351,-5.6068847690672,16.9786451178929));
#46076=CARTESIAN_POINT('Ctrl Pts',(16.4309495757058,-6.11363702143042,18.9974204980683));
#46077=CARTESIAN_POINT('Ctrl Pts',(16.3852589674394,-6.1137723837536,20.0000142741886));
#46078=CARTESIAN_POINT('Origin',(53.8647410325606,0.,20.));
#46079=CARTESIAN_POINT('',(19.8852589674394,-6.11331970325597,20.000155680082));
#46080=CARTESIAN_POINT('',(19.7397410325605,-6.11363390149491,20.0001012241782));
#46081=CARTESIAN_POINT('',(53.8647410325606,-6.11325,19.9999999999994));
#46082=CARTESIAN_POINT('Ctrl Pts',(19.7397410325605,-6.11363390149491,20.0001012241782));
#46083=CARTESIAN_POINT('Ctrl Pts',(19.7349712381691,-6.11371586791688,20.104772207252));
#46084=CARTESIAN_POINT('Ctrl Pts',(19.6838976136149,-6.08552537520897,21.2255156751894));
#46085=CARTESIAN_POINT('Ctrl Pts',(19.5865201588977,-5.43233438289444,23.3315114826968));
#46086=CARTESIAN_POINT('Ctrl Pts',(19.4476086684091,-3.17703636502164,25.5240986180776));
#46087=CARTESIAN_POINT('Ctrl Pts',(19.3086971779205,-0.14770274975791,26.3708248684634));
#46088=CARTESIAN_POINT('Ctrl Pts',(19.1697856874318,2.91761634788927,25.6653985255625));
#46089=CARTESIAN_POINT('Ctrl Pts',(19.0308741969432,5.27210350868496,23.5796857684201));
#46090=CARTESIAN_POINT('Ctrl Pts',(18.8919627064546,6.34212448150116,20.6218381365444));
#46091=CARTESIAN_POINT('Ctrl Pts',(18.7530512159659,5.86698526483596,17.5124892946733));
#46092=CARTESIAN_POINT('Ctrl Pts',(18.6141397254773,3.96244615387019,15.0091838258059));
#46093=CARTESIAN_POINT('Ctrl Pts',(18.4752282349886,1.09251854134113,13.7218132519219));
#46094=CARTESIAN_POINT('Ctrl Pts',(18.3363167445,-2.0435842560608,13.9640254311919));
#46095=CARTESIAN_POINT('Ctrl Pts',(18.1974052540114,-4.68179946933745,15.6768091256771));
#46096=CARTESIAN_POINT('Ctrl Pts',(18.0818800166982,-5.92724600164252,17.9771945968397));
#46097=CARTESIAN_POINT('Ctrl Pts',(18.0126586095479,-6.11274149148563,19.4968648822612));
#46098=CARTESIAN_POINT('Ctrl Pts',(17.9897410325605,-6.11272775120567,19.9999952045773));
#46099=CARTESIAN_POINT('Ctrl Pts',(19.8852589674394,-6.11331970325597,20.000155680082));
#46100=CARTESIAN_POINT('Ctrl Pts',(19.8755748329482,-6.11353913440155,20.2127011814972));
#46101=CARTESIAN_POINT('Ctrl Pts',(19.8195868682942,-6.05070320076175,21.4413850412945));
#46102=CARTESIAN_POINT('Ctrl Pts',(19.7172950734772,-5.24846036724355,23.6142619041474));
#46103=CARTESIAN_POINT('Ctrl Pts',(19.5783835829886,-2.8803147101225,25.6844535805079));
#46104=CARTESIAN_POINT('Ctrl Pts',(19.4394720925,0.189574918792307,26.3697163742558));
#46105=CARTESIAN_POINT('Ctrl Pts',(19.3005606020113,3.21327756126488,25.5030966421251));
#46106=CARTESIAN_POINT('Ctrl Pts',(19.1616491115227,5.45411500140619,23.2957328304541));
#46107=CARTESIAN_POINT('Ctrl Pts',(19.0227376210341,6.36614197849088,20.2854148699583));
#46108=CARTESIAN_POINT('Ctrl Pts',(18.8838261305454,5.72715727574455,17.2055600065159));
#46109=CARTESIAN_POINT('Ctrl Pts',(18.7449146400568,3.69283959787427,14.8065270730783));
#46110=CARTESIAN_POINT('Ctrl Pts',(18.6060031495682,0.758818871062057,13.6728032068524));
#46111=CARTESIAN_POINT('Ctrl Pts',(18.4670916590795,-2.36007629553962,14.0806026305434));
#46112=CARTESIAN_POINT('Ctrl Pts',(18.3281801685909,-4.90397550508568,15.9305713443019));
#46113=CARTESIAN_POINT('Ctrl Pts',(18.2175692713775,-5.9782391292396,18.1931071368928));
#46114=CARTESIAN_POINT('Ctrl Pts',(18.153262204327,-6.11305476313539,19.6046794530843));
#46115=CARTESIAN_POINT('Ctrl Pts',(18.1352589674394,-6.11282951797326,19.9999019817517));
#46116=CARTESIAN_POINT('Origin',(53.8647410325606,0.,20.));
#46117=CARTESIAN_POINT('',(21.6352589674394,-6.11337192102228,19.9998483128521));
#46118=CARTESIAN_POINT('',(21.4897410325605,-6.11304106492475,19.9998514866922));
#46119=CARTESIAN_POINT('',(53.8647410325606,-6.11325,19.9999999999994));
#46120=CARTESIAN_POINT('Ctrl Pts',(21.4897410325605,-6.11304106492475,19.9998514866922));
#46121=CARTESIAN_POINT('Ctrl Pts',(21.4572838667903,-6.11239501336448,20.7123084151566));
#46122=CARTESIAN_POINT('Ctrl Pts',(21.3785228708573,-5.81028586147664,22.441699581993));
#46123=CARTESIAN_POINT('Ctrl Pts',(21.2534580447614,-4.21366803405649,24.7806095119438));
#46124=CARTESIAN_POINT('Ctrl Pts',(21.1145465542727,-1.41368441857138,26.2137526480868));
#46125=CARTESIAN_POINT('Ctrl Pts',(20.9756350637841,1.73072146273936,26.1330113994131));
#46126=CARTESIAN_POINT('Ctrl Pts',(20.8367235732955,4.453463923361,24.5580571179221));
#46127=CARTESIAN_POINT('Ctrl Pts',(20.6978120828068,6.09118902430437,21.8726029683601));
#46128=CARTESIAN_POINT('Ctrl Pts',(20.5589005923182,6.2448904649721,18.7309181715043));
#46129=CARTESIAN_POINT('Ctrl Pts',(20.4199891018296,4.87712127505025,15.8984254638773));
#46130=CARTESIAN_POINT('Ctrl Pts',(20.2810776113409,2.32111718758555,14.0652177286431));
#46131=CARTESIAN_POINT('Ctrl Pts',(20.1421661208523,-0.800391074992589,
13.6779275760247));
#46132=CARTESIAN_POINT('Ctrl Pts',(20.0032546303637,-3.72689647556414,14.8309122403131));
#46133=CARTESIAN_POINT('Ctrl Pts',(19.8691129342664,-5.67609213148412,17.1604321151321));
#46134=CARTESIAN_POINT('Ctrl Pts',(19.781275068332,-6.11292016081293,19.0886555729594));
#46135=CARTESIAN_POINT('Ctrl Pts',(19.7397410325605,-6.11363390149491,20.0001012241782));
#46136=CARTESIAN_POINT('Ctrl Pts',(21.6352589674394,-6.11337192102228,19.9998483128521));
#46137=CARTESIAN_POINT('Ctrl Pts',(21.5978874615695,-6.11253093386954,20.8200506714862));
#46138=CARTESIAN_POINT('Ctrl Pts',(21.5142121255366,-5.74047386468237,22.6572353299736));
#46139=CARTESIAN_POINT('Ctrl Pts',(21.3842329593409,-3.95483132620118,24.9968524612595));
#46140=CARTESIAN_POINT('Ctrl Pts',(21.2453214688522,-1.08294402247514,26.2798453470195));
#46141=CARTESIAN_POINT('Ctrl Pts',(21.1064099783636,2.05278578321474,26.0328513877377));
#46142=CARTESIAN_POINT('Ctrl Pts',(20.967498487875,4.68838619551153,24.3160468278314));
#46143=CARTESIAN_POINT('Ctrl Pts',(20.8285869973864,6.18173408290928,21.5477044506284));
#46144=CARTESIAN_POINT('Ctrl Pts',(20.6896755068977,6.16899841191383,18.4022879070052));
#46145=CARTESIAN_POINT('Ctrl Pts',(20.5507640164091,4.65328203108421,15.646129115662));
#46146=CARTESIAN_POINT('Ctrl Pts',(20.4118525259204,2.00386571014259,13.9507233858905));
#46147=CARTESIAN_POINT('Ctrl Pts',(20.2729410354318,-1.13376138770991,13.7291300082018));
#46148=CARTESIAN_POINT('Ctrl Pts',(20.1340295449432,-3.99516512133005,15.0353367695678));
#46149=CARTESIAN_POINT('Ctrl Pts',(20.0048021889457,-5.75158500211091,17.3757212187838));
#46150=CARTESIAN_POINT('Ctrl Pts',(19.9218786631111,-6.1124899438408,19.1964337175973));
#46151=CARTESIAN_POINT('Ctrl Pts',(19.8852589674394,-6.11331970325597,20.000155680082));
#46152=CARTESIAN_POINT('Origin',(53.8647410325606,0.,20.));
#46153=CARTESIAN_POINT('',(23.3852589674394,-6.11280242905631,20.0000853877862));
#46154=CARTESIAN_POINT('',(23.2397410325605,-6.11304143026726,20.0001485574224));
#46155=CARTESIAN_POINT('',(53.8647410325606,-6.11325,19.9999999999994));
#46156=CARTESIAN_POINT('Ctrl Pts',(23.2397410325605,-6.11304143026726,20.0001485574224));
#46157=CARTESIAN_POINT('Ctrl Pts',(23.2259003255744,-6.11331703329572,20.3039614647346));
#46158=CARTESIAN_POINT('Ctrl Pts',(23.1657557884255,-6.01664684285281,21.6240010332314));
#46159=CARTESIAN_POINT('Ctrl Pts',(23.0593074211136,-5.08144042723737,23.8455414171941));
#46160=CARTESIAN_POINT('Ctrl Pts',(22.920395930625,-2.62301384869953,25.8076694083296));
#46161=CARTESIAN_POINT('Ctrl Pts',(22.7814844401364,0.474469340488402,26.3548488929206));
#46162=CARTESIAN_POINT('Ctrl Pts',(22.6425729496477,3.45635543942831,25.353768082692));
#46163=CARTESIAN_POINT('Ctrl Pts',(22.5036614591591,5.59615418399987,23.0483247785986));
#46164=CARTESIAN_POINT('Ctrl Pts',(22.3647499686705,6.37253682336279,20.0002044573261));
#46165=CARTESIAN_POINT('Ctrl Pts',(22.2258384781818,5.59634977820039,16.9520343231995));
#46166=CARTESIAN_POINT('Ctrl Pts',(22.0869269876932,3.45669897433838,14.6464537166729));
#46167=CARTESIAN_POINT('Ctrl Pts',(21.9480154972045,0.474877119159393,13.6451815660385));
#46168=CARTESIAN_POINT('Ctrl Pts',(21.8091040067159,-2.62264117521137,14.1921622893711));
#46169=CARTESIAN_POINT('Ctrl Pts',(21.6701925162273,-5.08119365504295,16.1541325234911));
#46170=CARTESIAN_POINT('Ctrl Pts',(21.5637381915088,-6.01659496814579,18.3757372179489));
#46171=CARTESIAN_POINT('Ctrl Pts',(21.5035876969532,-6.1133166792282,19.6959077581311));
#46172=CARTESIAN_POINT('Ctrl Pts',(21.4897410325605,-6.11304106492475,19.9998514866922));
#46173=CARTESIAN_POINT('Ctrl Pts',(23.3852589674394,-6.11280242905631,20.0000853877862));
#46174=CARTESIAN_POINT('Ctrl Pts',(23.3665039203536,-6.11300568882329,20.4118175234676));
#46175=CARTESIAN_POINT('Ctrl Pts',(23.3014450431048,-5.97083721962065,21.8399255703595));
#46176=CARTESIAN_POINT('Ctrl Pts',(23.1900823356932,-4.87086133430093,24.109006595311));
#46177=CARTESIAN_POINT('Ctrl Pts',(23.0511708452045,-2.31206487401468,25.9383146899305));
#46178=CARTESIAN_POINT('Ctrl Pts',(22.9122593547159,0.810030305690605,26.3208445829778));
#46179=CARTESIAN_POINT('Ctrl Pts',(22.7733478642273,3.73477417444681,25.1633988035191));
#46180=CARTESIAN_POINT('Ctrl Pts',(22.6344363737386,5.74959828557432,22.7479710502147));
#46181=CARTESIAN_POINT('Ctrl Pts',(22.49552488325,6.36362201785506,19.6630428036569));
#46182=CARTESIAN_POINT('Ctrl Pts',(22.3566133927613,5.42724801959969,16.6602089478459));
#46183=CARTESIAN_POINT('Ctrl Pts',(22.2177019022727,3.16860928138414,14.4710633427192));
#46184=CARTESIAN_POINT('Ctrl Pts',(22.0787904117841,0.137988073903447,13.628957335745));
#46185=CARTESIAN_POINT('Ctrl Pts',(21.9398789212955,-2.9262517859769,14.3390569846214));
#46186=CARTESIAN_POINT('Ctrl Pts',(21.8009674308068,-5.27755581855221,16.4283575318402));
#46187=CARTESIAN_POINT('Ctrl Pts',(21.6994274461882,-6.05641014667787,18.5916424107086));
#46188=CARTESIAN_POINT('Ctrl Pts',(21.6441912917324,-6.11357292897739,19.8038082207395));
#46189=CARTESIAN_POINT('Ctrl Pts',(21.6352589674394,-6.11337192102228,19.9998483128521));
#46190=CARTESIAN_POINT('Origin',(53.8647410325606,0.,20.));
#46191=CARTESIAN_POINT('',(25.1352589674394,-6.11377511406864,20.0000032316134));
#46192=CARTESIAN_POINT('',(24.9897410325605,-6.11363358775036,19.9998986723535));
#46193=CARTESIAN_POINT('',(53.8647410325606,-6.11325,19.9999999999994));
#46194=CARTESIAN_POINT('Ctrl Pts',(24.9897410325605,-6.11363358775036,19.9998986723535));
#46195=CARTESIAN_POINT('Ctrl Pts',(24.9482129541956,-6.11291938677644,20.9112137264931));
#46196=CARTESIAN_POINT('Ctrl Pts',(24.8603810456679,-5.6761877702843,22.8393071165725));
#46197=CARTESIAN_POINT('Ctrl Pts',(24.7262453069773,-3.72722815930074,25.1688486005525));
#46198=CARTESIAN_POINT('Ctrl Pts',(24.5873338164887,-0.800796749783299,
26.3220210512505));
#46199=CARTESIAN_POINT('Ctrl Pts',(24.448422326,2.32073635810671,25.9349312012086));
#46200=CARTESIAN_POINT('Ctrl Pts',(24.3095108355114,4.87685807407465,24.1018874841042));
#46201=CARTESIAN_POINT('Ctrl Pts',(24.1705993450227,6.24480901733213,21.2694825496889));
#46202=CARTESIAN_POINT('Ctrl Pts',(24.0316878545341,6.09130917345336,18.1277878965458));
#46203=CARTESIAN_POINT('Ctrl Pts',(23.8927763640454,4.45375639682368,15.4422286625293));
#46204=CARTESIAN_POINT('Ctrl Pts',(23.7538648735569,1.73111500389623,13.8670996706124));
#46205=CARTESIAN_POINT('Ctrl Pts',(23.6149533830682,-1.41328568991475,13.7861566510251));
#46206=CARTESIAN_POINT('Ctrl Pts',(23.4760418925796,-4.21336126194841,15.2191201141181));
#46207=CARTESIAN_POINT('Ctrl Pts',(23.3509711090769,-5.81020523120089,17.558038995093));
#46208=CARTESIAN_POINT('Ctrl Pts',(23.2722041557373,-6.11239500844286,19.2875609820401));
#46209=CARTESIAN_POINT('Ctrl Pts',(23.2397410325605,-6.11304143026726,20.0001485574224));
#46210=CARTESIAN_POINT('Ctrl Pts',(25.1352589674394,-6.11377504588096,20.0000032311938));
#46211=CARTESIAN_POINT('Ctrl Pts',(25.1351203791376,-6.11377514153906,20.0030442848715));
#46212=CARTESIAN_POINT('Ctrl Pts',(25.088677960673,-6.11303068323524,21.0221337688692));
#46213=CARTESIAN_POINT('Ctrl Pts',(24.9959317120454,-5.59169558634022,23.0564956744613));
#46214=CARTESIAN_POINT('Ctrl Pts',(24.8570202215568,-3.44853163007304,25.358810962768));
#46215=CARTESIAN_POINT('Ctrl Pts',(24.7181087310682,-0.465186469148229,
26.3555351377534));
#46216=CARTESIAN_POINT('Ctrl Pts',(24.5791972405795,2.63149415450833,25.8038318250175));
#46217=CARTESIAN_POINT('Ctrl Pts',(24.4402857500909,5.08705207263311,23.8381149733452));
#46218=CARTESIAN_POINT('Ctrl Pts',(24.3013742596023,6.30322871286294,20.9373009824156));
#46219=CARTESIAN_POINT('Ctrl Pts',(24.1624627691136,5.98372151391236,17.8081281556077));
#46220=CARTESIAN_POINT('Ctrl Pts',(24.023551278625,4.20637344551665,15.2129708821494));
#46221=CARTESIAN_POINT('Ctrl Pts',(23.8846397881363,1.40420777710976,13.784098950514));
#46222=CARTESIAN_POINT('Ctrl Pts',(23.7457282976477,-1.74007132052403,13.8696348283494));
#46223=CARTESIAN_POINT('Ctrl Pts',(23.6068168071591,-4.46040904974499,15.4487390266817));
#46224=CARTESIAN_POINT('Ctrl Pts',(23.4866603637563,-5.87347405505967,17.7737756783798));
#46225=CARTESIAN_POINT('Ctrl Pts',(23.4128077505164,-6.11250386626396,19.3953031529145));
#46226=CARTESIAN_POINT('Ctrl Pts',(23.3852589674394,-6.11280242905631,20.0000853877862));
#46227=CARTESIAN_POINT('Origin',(53.8647410325606,0.,20.));
#46228=CARTESIAN_POINT('',(26.8852589674394,-6.11281196393338,19.9999098576029));
#46229=CARTESIAN_POINT('',(26.7397410325605,-6.11272776236879,20.0000049172972));
#46230=CARTESIAN_POINT('',(53.8647410325606,-6.11325,19.9999999999994));
#46231=CARTESIAN_POINT('Ctrl Pts',(26.7397410325605,-6.11272776236879,20.0000049172972));
#46232=CARTESIAN_POINT('Ctrl Pts',(26.7168294129797,-6.11274184821953,20.5030044486427));
#46233=CARTESIAN_POINT('Ctrl Pts',(26.6476139632361,-5.92731157177153,22.0225436883079));
#46234=CARTESIAN_POINT('Ctrl Pts',(26.5320946833296,-4.68207687136995,24.3228904424587));
#46235=CARTESIAN_POINT('Ctrl Pts',(26.3931831928409,-2.04397156988813,26.0358434231188));
#46236=CARTESIAN_POINT('Ctrl Pts',(26.2542717023523,1.09211567872115,26.2782568401754));
#46237=CARTESIAN_POINT('Ctrl Pts',(26.1153602118636,3.96212589368178,24.9910704272264));
#46238=CARTESIAN_POINT('Ctrl Pts',(25.976448721375,5.86682563350311,22.4878871744893));
#46239=CARTESIAN_POINT('Ctrl Pts',(25.8375372308864,6.34216437072042,19.3785688278802));
#46240=CARTESIAN_POINT('Ctrl Pts',(25.6986257403977,5.27233320006711,16.4206525407014));
#46241=CARTESIAN_POINT('Ctrl Pts',(25.5597142499091,2.91797988069426,14.3347887044894));
#46242=CARTESIAN_POINT('Ctrl Pts',(25.4208027594205,-0.147293944655354,
13.6291656668231));
#46243=CARTESIAN_POINT('Ctrl Pts',(25.2818912689318,-3.17668188663938,14.4756975283739));
#46244=CARTESIAN_POINT('Ctrl Pts',(25.1429797784432,-5.43212059438828,16.6681399406727));
#46245=CARTESIAN_POINT('Ctrl Pts',(25.0455963663194,-6.08548669297453,18.7742226688102));
#46246=CARTESIAN_POINT('Ctrl Pts',(24.9945167843585,-6.11371572125424,19.8950969410976));
#46247=CARTESIAN_POINT('Ctrl Pts',(24.9897410325605,-6.11363358775036,19.9998986723535));
#46248=CARTESIAN_POINT('Ctrl Pts',(26.8852589674394,-6.11281196393338,19.9999098576029));
#46249=CARTESIAN_POINT('Ctrl Pts',(26.8574330077589,-6.11249297390719,20.6107742611335));
#46250=CARTESIAN_POINT('Ctrl Pts',(26.7833032179154,-5.87007710988381,22.2383961010393));
#46251=CARTESIAN_POINT('Ctrl Pts',(26.6628695979091,-4.44680132145817,24.5645573000867));
#46252=CARTESIAN_POINT('Ctrl Pts',(26.5239581074204,-1.7217612793893,26.135532856655));
#46253=CARTESIAN_POINT('Ctrl Pts',(26.3850466169318,1.42275917377253,26.2116810664862));
#46254=CARTESIAN_POINT('Ctrl Pts',(26.2461351264432,4.22064643785949,24.7744496002033));
#46255=CARTESIAN_POINT('Ctrl Pts',(26.1072236359545,5.99023870889178,22.1739975963169));
#46256=CARTESIAN_POINT('Ctrl Pts',(25.968312145466,6.30040229708003,19.0438848221863));
#46257=CARTESIAN_POINT('Ctrl Pts',(25.8294006549772,5.07557065842261,16.1467146706146));
#46258=CARTESIAN_POINT('Ctrl Pts',(25.6904891644886,2.61415501023178,14.18833768008));
#46259=CARTESIAN_POINT('Ctrl Pts',(25.551577674,-0.484158930120513,13.6458820070224));
#46260=CARTESIAN_POINT('Ctrl Pts',(25.4126661835113,-3.46451506210964,14.6515085563579));
#46261=CARTESIAN_POINT('Ctrl Pts',(25.2738932813245,-5.5986645637313,16.9579086962675));
#46262=CARTESIAN_POINT('Ctrl Pts',(25.1814242093005,-6.11374318114547,18.9869958074943));
#46263=CARTESIAN_POINT('Ctrl Pts',(25.1352589674394,-6.11377504588096,20.0000032311938));
#46264=CARTESIAN_POINT('Origin',(53.8647410325606,0.,20.));
#46265=CARTESIAN_POINT('',(28.6352589674394,-6.11335271655686,20.0001533502409));
#46266=CARTESIAN_POINT('',(28.4897410325605,-6.1136580696871,20.0000927339656));
#46267=CARTESIAN_POINT('',(53.8647410325606,-6.11325,19.9999999999994));
#46268=CARTESIAN_POINT('Ctrl Pts',(28.4897410325605,-6.1136580696871,20.0000927339656));
#46269=CARTESIAN_POINT('Ctrl Pts',(28.4854458717638,-6.11372698856088,20.0943470171741));
#46270=CARTESIAN_POINT('Ctrl Pts',(28.4348468808043,-6.0885798609534,21.2046694997386));
#46271=CARTESIAN_POINT('Ctrl Pts',(28.3379440596818,-5.4492952092373,23.3036960104557));
#46272=CARTESIAN_POINT('Ctrl Pts',(28.1990325691932,-3.2052359128581,25.5077843412612));
#46273=CARTESIAN_POINT('Ctrl Pts',(28.0601210787046,-0.180270636962042,
26.3699865073929));
#46274=CARTESIAN_POINT('Ctrl Pts',(27.9212095882159,2.88861478152641,25.6802403339));
#46275=CARTESIAN_POINT('Ctrl Pts',(27.7822980977273,5.2537340446546,23.6065917699339));
#46276=CARTESIAN_POINT('Ctrl Pts',(27.6433866072386,6.33886255458932,20.6542531015921));
#46277=CARTESIAN_POINT('Ctrl Pts',(27.50447511675,5.87962559290408,17.5425158201557));
#46278=CARTESIAN_POINT('Ctrl Pts',(27.3655636262614,3.98790911718367,15.0295064148517));
#46279=CARTESIAN_POINT('Ctrl Pts',(27.2266521357728,1.12460048411671,13.7274806211505));
#46280=CARTESIAN_POINT('Ctrl Pts',(27.0877406452841,-2.01269960121476,13.953656814058));
#46281=CARTESIAN_POINT('Ctrl Pts',(26.9488291547955,-4.65963666919246,15.6529306748069));
#46282=CARTESIAN_POINT('Ctrl Pts',(26.8328292838876,-5.92199242415093,17.9563437534471));
#46283=CARTESIAN_POINT('Ctrl Pts',(26.7631332431426,-6.11271338105516,19.4864545365197));
#46284=CARTESIAN_POINT('Ctrl Pts',(26.7397410325605,-6.11272776236879,20.0000049172972));
#46285=CARTESIAN_POINT('Ctrl Pts',(28.6352589674394,-6.11335271655686,20.0001533502409));
#46286=CARTESIAN_POINT('Ctrl Pts',(28.6260494665429,-6.1135607294616,20.202278540951));
#46287=CARTESIAN_POINT('Ctrl Pts',(28.5705361354836,-6.05432216663628,21.4205339982837));
#46288=CARTESIAN_POINT('Ctrl Pts',(28.4687189742614,-5.26686911251823,23.587382763227));
#46289=CARTESIAN_POINT('Ctrl Pts',(28.3298074837727,-2.90933792449704,25.6696541498914));
#46290=CARTESIAN_POINT('Ctrl Pts',(28.1908959932841,0.157008291011193,26.3706023055007));
#46291=CARTESIAN_POINT('Ctrl Pts',(28.0519845027954,3.18510187344724,25.5194520918348));
#46292=CARTESIAN_POINT('Ctrl Pts',(27.9130730123068,5.43719482255474,23.3235730471709));
#46293=CARTESIAN_POINT('Ctrl Pts',(27.7741615218181,6.36459964755315,20.3179570170062));
#46294=CARTESIAN_POINT('Ctrl Pts',(27.6352500313296,5.74136855771394,17.2348756948754));
#46295=CARTESIAN_POINT('Ctrl Pts',(27.4963385408409,3.71934213448194,14.8254739903094));
#46296=CARTESIAN_POINT('Ctrl Pts',(27.3574270503523,0.791155730627478,13.6767652306598));
#46297=CARTESIAN_POINT('Ctrl Pts',(27.2185155598636,-2.3297834869271,14.0686144753238));
#46298=CARTESIAN_POINT('Ctrl Pts',(27.079604069375,-4.88310712004916,15.905553737998));
#46299=CARTESIAN_POINT('Ctrl Pts',(26.9685185385669,-5.97358281620434,18.172252857223));
#46300=CARTESIAN_POINT('Ctrl Pts',(26.9037368379217,-6.11302378974126,19.5942644293674));
#46301=CARTESIAN_POINT('Ctrl Pts',(26.8852589674394,-6.11281196393338,19.9999098576029));
#46302=CARTESIAN_POINT('Origin',(53.8647410325606,0.,20.));
#46303=CARTESIAN_POINT('',(30.3852589674394,-6.11333899670695,19.9998456009343));
#46304=CARTESIAN_POINT('',(30.2397410325605,-6.11301242699033,19.9998552897238));
#46305=CARTESIAN_POINT('',(53.8647410325606,-6.11325,19.9999999999994));
#46306=CARTESIAN_POINT('Ctrl Pts',(30.2397410325605,-6.11301242699033,19.9998552897238));
#46307=CARTESIAN_POINT('Ctrl Pts',(30.207758500385,-6.1123965421807,20.7019031242023));
#46308=CARTESIAN_POINT('Ctrl Pts',(30.1294721380467,-5.81667886159044,22.4208707815258));
#46309=CARTESIAN_POINT('Ctrl Pts',(30.0048819455455,-4.23805306663042,24.7590053384444));
#46310=CARTESIAN_POINT('Ctrl Pts',(29.8659704550568,-1.4454327553499,26.2064442120009));
#46311=CARTESIAN_POINT('Ctrl Pts',(29.7270589645682,1.69934481122473,26.1417792877538));
#46312=CARTESIAN_POINT('Ctrl Pts',(29.5881474740796,4.43010339123342,24.5807651707875));
#46313=CARTESIAN_POINT('Ctrl Pts',(29.4492359835909,6.08153604262198,21.9037187211369));
#46314=CARTESIAN_POINT('Ctrl Pts',(29.3103244931023,6.2512968328913,18.762860753997));
#46315=CARTESIAN_POINT('Ctrl Pts',(29.1714130026136,4.89802618046513,15.9234125616644));
#46316=CARTESIAN_POINT('Ctrl Pts',(29.032501512125,2.35142747477107,14.0771616231904));
#46317=CARTESIAN_POINT('Ctrl Pts',(28.8935900216364,-0.76806003704259,13.673918322815));
#46318=CARTESIAN_POINT('Ctrl Pts',(28.7546785311478,-3.70042164241411,14.8119266316608));
#46319=CARTESIAN_POINT('Ctrl Pts',(28.6200622014558,-5.66844000970638,17.1396582888592));
#46320=CARTESIAN_POINT('Ctrl Pts',(28.5317497019267,-6.11298401106189,19.0782420263708));
#46321=CARTESIAN_POINT('Ctrl Pts',(28.4897410325605,-6.1136580696871,20.0000927339656));
#46322=CARTESIAN_POINT('Ctrl Pts',(30.3852589674394,-6.11333899670695,19.9998456009343));
#46323=CARTESIAN_POINT('Ctrl Pts',(30.3483620951642,-6.11250411389834,20.8096436190909));
#46324=CARTESIAN_POINT('Ctrl Pts',(30.265161392726,-5.74750682244695,22.6364299549355));
#46325=CARTESIAN_POINT('Ctrl Pts',(30.135656860125,-3.98032524857262,24.9765687229126));
#46326=CARTESIAN_POINT('Ctrl Pts',(29.9967453696363,-1.11503456969162,26.2742269043038));
#46327=CARTESIAN_POINT('Ctrl Pts',(29.8578338791477,2.02191697488329,26.0432670870131));
#46328=CARTESIAN_POINT('Ctrl Pts',(29.7189223886591,4.6662598320792,24.3399590456387));
#46329=CARTESIAN_POINT('Ctrl Pts',(29.5800108981704,6.17374090938801,21.5792873462565));
#46330=CARTESIAN_POINT('Ctrl Pts',(29.4410994076818,6.17708584096459,18.4338467981542));
#46331=CARTESIAN_POINT('Ctrl Pts',(29.3021879171932,4.6754796861493,15.6699751683504));
#46332=CARTESIAN_POINT('Ctrl Pts',(29.1632764267045,2.03476547711032,13.9610468795116));
#46333=CARTESIAN_POINT('Ctrl Pts',(29.0243649362159,-1.10168775744487,13.7234157837727));
#46334=CARTESIAN_POINT('Ctrl Pts',(28.8854534457272,-3.96973186994514,15.0149770091765));
#46335=CARTESIAN_POINT('Ctrl Pts',(28.7557514561351,-5.74458857655193,17.3549142648056));
#46336=CARTESIAN_POINT('Ctrl Pts',(28.6723532967058,-6.11251487536801,19.1860268887194));
#46337=CARTESIAN_POINT('Ctrl Pts',(28.6352589674394,-6.11335271655686,20.0001533502409));
#46338=CARTESIAN_POINT('Origin',(53.8647410325606,0.,20.));
#46339=CARTESIAN_POINT('',(32.1352589674394,-6.11281908049607,20.0000934609265));
#46340=CARTESIAN_POINT('',(31.9897410325605,-6.1130709765779,20.0001517774591));
#46341=CARTESIAN_POINT('',(53.8647410325606,-6.11325,19.9999999999994));
#46342=CARTESIAN_POINT('Ctrl Pts',(31.9897410325605,-6.1130709765779,20.0001517774591));
#46343=CARTESIAN_POINT('Ctrl Pts',(31.9763749591691,-6.113344967759,20.2935420849967));
#46344=CARTESIAN_POINT('Ctrl Pts',(31.9167050556149,-6.02075144272683,21.6031472979479));
#46345=CARTESIAN_POINT('Ctrl Pts',(31.8107313218978,-5.10103373445315,23.8195131164703));
#46346=CARTESIAN_POINT('Ctrl Pts',(31.6718198314091,-2.65267034660569,25.7941837767848));
#46347=CARTESIAN_POINT('Ctrl Pts',(31.5329083409205,0.441974997287937,26.357191495361));
#46348=CARTESIAN_POINT('Ctrl Pts',(31.3939968504318,3.4289399932875,25.3713681803941));
#46349=CARTESIAN_POINT('Ctrl Pts',(31.2550853599432,5.58049698283711,23.0768943809405));
#46350=CARTESIAN_POINT('Ctrl Pts',(31.1161738694545,6.37245250121533,20.0327830241454));
#46351=CARTESIAN_POINT('Ctrl Pts',(30.977262378966,5.6118588788506,16.9806845923648));
#46352=CARTESIAN_POINT('Ctrl Pts',(30.8383508884773,3.48402294614019,14.6641954948025));
#46353=CARTESIAN_POINT('Ctrl Pts',(30.6994393979887,0.507358900497252,13.6476923442733));
#46354=CARTESIAN_POINT('Ctrl Pts',(30.5605279075,-2.59291526618855,14.1788303555657));
#46355=CARTESIAN_POINT('Ctrl Pts',(30.4216164170114,-5.06146587467247,16.1282059963831));
#46356=CARTESIAN_POINT('Ctrl Pts',(30.3146874586982,-6.01243369276824,18.3548832896175));
#46357=CARTESIAN_POINT('Ctrl Pts',(30.2540623305479,-6.11328821096629,19.685488804174));
#46358=CARTESIAN_POINT('Ctrl Pts',(30.2397410325605,-6.11301242699033,19.9998552897238));
#46359=CARTESIAN_POINT('Ctrl Pts',(32.1352589674394,-6.11281908049607,20.0000934609265));
#46360=CARTESIAN_POINT('Ctrl Pts',(32.1169785539483,-6.11303668109335,20.4014027704384));
#46361=CARTESIAN_POINT('Ctrl Pts',(32.0523943102942,-5.97552686421729,21.819071362413));
#46362=CARTESIAN_POINT('Ctrl Pts',(31.9415062364773,-4.8918043167284,24.0840514033414));
#46363=CARTESIAN_POINT('Ctrl Pts',(31.8025947459886,-2.34239333841841,25.9264170277183));
#46364=CARTESIAN_POINT('Ctrl Pts',(31.6636832554999,0.777705418913837,26.3249031312495));
#46365=CARTESIAN_POINT('Ctrl Pts',(31.5247717650114,3.70832832222358,25.1824247599837));
#46366=CARTESIAN_POINT('Ctrl Pts',(31.3858602745226,5.73547458931472,22.7773290358944));
#46367=CARTESIAN_POINT('Ctrl Pts',(31.2469487840341,6.36526149692924,19.6955802010263));
#46368=CARTESIAN_POINT('Ctrl Pts',(31.1080372935454,5.44425124037868,16.6879985250709));
#46369=CARTESIAN_POINT('Ctrl Pts',(30.9691258030568,3.19683367304369,14.48733460065));
#46370=CARTESIAN_POINT('Ctrl Pts',(30.8302143125682,0.170557201505726,13.629746034944));
#46371=CARTESIAN_POINT('Ctrl Pts',(30.6913028220795,-2.8972728848445,14.3241709707707));
#46372=CARTESIAN_POINT('Ctrl Pts',(30.5523913315909,-5.25922740334937,16.4014235511586));
#46373=CARTESIAN_POINT('Ctrl Pts',(30.4503767133775,-6.0528232864935,18.5707916024673));
#46374=CARTESIAN_POINT('Ctrl Pts',(30.3946659253271,-6.11355185234856,19.7933853948378));
#46375=CARTESIAN_POINT('Ctrl Pts',(30.3852589674394,-6.11333899670695,19.9998456009343));
#46376=CARTESIAN_POINT('Origin',(53.8647410325606,0.,20.));
#46377=CARTESIAN_POINT('',(33.8852589674394,-6.11377473629356,19.9999921625065));
#46378=CARTESIAN_POINT('',(33.7397410325605,-6.11360782021149,19.9998906860949));
#46379=CARTESIAN_POINT('',(53.8647410325606,-6.11325,19.9999999999994));
#46380=CARTESIAN_POINT('Ctrl Pts',(33.7397410325605,-6.11360782021148,19.9998906860949));
#46381=CARTESIAN_POINT('Ctrl Pts',(33.6986875877904,-6.11285986208749,20.9008011180488));
#46382=CARTESIAN_POINT('Ctrl Pts',(33.6113303128573,-5.68377501480363,22.8185295471014));
#46383=CARTESIAN_POINT('Ctrl Pts',(33.4776692077614,-3.75360435860782,25.1497261991253));
#46384=CARTESIAN_POINT('Ctrl Pts',(33.3387577172728,-0.833106600630097,
26.3178444899273));
#46385=CARTESIAN_POINT('Ctrl Pts',(33.1998462267841,2.29036464937583,25.9467180343284));
#46386=CARTESIAN_POINT('Ctrl Pts',(33.0609347362955,4.855824102872,24.1267660327289));
#46387=CARTESIAN_POINT('Ctrl Pts',(32.9220232458069,6.2382373842586,21.301391541603));
#46388=CARTESIAN_POINT('Ctrl Pts',(32.7831117553182,6.10080095490451,18.1589532011506));
#46389=CARTESIAN_POINT('Ctrl Pts',(32.6442002648296,4.47699906757734,15.4650573370957));
#46390=CARTESIAN_POINT('Ctrl Pts',(32.5052887743409,1.76244584798862,13.8760298629218));
#46391=CARTESIAN_POINT('Ctrl Pts',(32.3663772838523,-1.38149994633938,13.779012658333));
#46392=CARTESIAN_POINT('Ctrl Pts',(32.2274657933637,-4.18886472194398,15.197642459357));
#46393=CARTESIAN_POINT('Ctrl Pts',(32.1019203762664,-5.8037503628612,17.5372120805641));
#46394=CARTESIAN_POINT('Ctrl Pts',(32.022678789332,-6.11239578539673,19.2771557033073));
#46395=CARTESIAN_POINT('Ctrl Pts',(31.9897410325605,-6.1130709765779,20.0001517774591));
#46396=CARTESIAN_POINT('Ctrl Pts',(33.8852589674394,-6.11377433895741,19.9999921684411));
#46397=CARTESIAN_POINT('Ctrl Pts',(33.8392911825694,-6.11369836731836,21.0086671186757));
#46398=CARTESIAN_POINT('Ctrl Pts',(33.7470195675366,-5.6020923000678,23.0334651258696));
#46399=CARTESIAN_POINT('Ctrl Pts',(33.6084441223409,-3.47588262343321,25.341110870073));
#46400=CARTESIAN_POINT('Ctrl Pts',(33.4695326318522,-0.497672041157185,
26.3530738920422));
#46401=CARTESIAN_POINT('Ctrl Pts',(33.3306211413636,2.60178860923987,25.8172090706048));
#46402=CARTESIAN_POINT('Ctrl Pts',(33.191709650875,5.0673638491298,23.8640715519811));
#46403=CARTESIAN_POINT('Ctrl Pts',(33.0527981603864,6.29835454118703,20.9695129766052));
#46404=CARTESIAN_POINT('Ctrl Pts',(32.9138866698977,5.99484891033732,17.8387476129511));
#46405=CARTESIAN_POINT('Ctrl Pts',(32.774975179409,4.23079139261945,15.2345378471302));
#46406=CARTESIAN_POINT('Ctrl Pts',(32.6360636889205,1.43596722108643,13.7913589668703));
#46407=CARTESIAN_POINT('Ctrl Pts',(32.4971521984318,-1.70870807523846,13.8608191057836));
#46408=CARTESIAN_POINT('Ctrl Pts',(32.3582407079432,-4.43708317105403,15.4259953791621));
#46409=CARTESIAN_POINT('Ctrl Pts',(32.2376096309457,-5.86764475673546,17.7529331209653));
#46410=CARTESIAN_POINT('Ctrl Pts',(32.1632823841111,-6.11248550422285,19.3848963265668));
#46411=CARTESIAN_POINT('Ctrl Pts',(32.1352589674394,-6.11281908049607,20.0000934609265));
#46412=CARTESIAN_POINT('Origin',(53.8647410325606,0.,20.));
#46413=CARTESIAN_POINT('',(35.6352589674395,-6.11279596489353,19.9999180648868));
#46414=CARTESIAN_POINT('',(35.4897410325605,-6.11272955150596,20.0000146122445));
#46415=CARTESIAN_POINT('',(53.8647410325606,-6.11325,19.9999999999994));
#46416=CARTESIAN_POINT('Ctrl Pts',(35.4897410325605,-6.11272955150596,20.0000146122445));
#46417=CARTESIAN_POINT('Ctrl Pts',(35.4673040465744,-6.11277055632431,20.4925936701237));
#46418=CARTESIAN_POINT('Ctrl Pts',(35.3985632304255,-5.93250613741697,22.0016922885538));
#46419=CARTESIAN_POINT('Ctrl Pts',(35.2835185841137,-4.70411576761554,24.2988975856361));
#46420=CARTESIAN_POINT('Ctrl Pts',(35.144607093625,-2.07480213772069,26.025315070287));
#46421=CARTESIAN_POINT('Ctrl Pts',(35.0056956031364,1.06000482861184,26.2837580610839));
#46422=CARTESIAN_POINT('Ctrl Pts',(34.8667841126477,3.93655807151044,25.0112609347891));
#46423=CARTESIAN_POINT('Ctrl Pts',(34.7278726221591,5.85403004228618,22.5178478649292));
#46424=CARTESIAN_POINT('Ctrl Pts',(34.5889611316705,6.34525845764879,19.4110002440119));
#46425=CARTESIAN_POINT('Ctrl Pts',(34.4500496411818,5.29056313888617,16.4476532713745));
#46426=CARTESIAN_POINT('Ctrl Pts',(34.3111381506932,2.94690422977004,14.3497804407721));
#46427=CARTESIAN_POINT('Ctrl Pts',(34.1722266602045,-0.114722154020674,
13.6284959048672));
#46428=CARTESIAN_POINT('Ctrl Pts',(34.033315169716,-3.14839826566498,14.459529445284));
#46429=CARTESIAN_POINT('Ctrl Pts',(33.8944036792273,-5.41501600831516,16.6404126389379));
#46430=CARTESIAN_POINT('Ctrl Pts',(33.7965456335088,-6.08237743127135,18.7533759642386));
#46431=CARTESIAN_POINT('Ctrl Pts',(33.7449914179532,-6.11370347767532,19.8846719267787));
#46432=CARTESIAN_POINT('Ctrl Pts',(33.7397410325605,-6.11360782021148,19.9998906860949));
#46433=CARTESIAN_POINT('Ctrl Pts',(35.6352589674395,-6.11279596489353,19.9999180648868));
#46434=CARTESIAN_POINT('Ctrl Pts',(35.6079076413536,-6.11251190746788,20.6003673166567));
#46435=CARTESIAN_POINT('Ctrl Pts',(35.5342524851048,-5.87588159442696,22.2175530727367));
#46436=CARTESIAN_POINT('Ctrl Pts',(35.4142934986932,-4.47007877524375,24.5417640935448));
#46437=CARTESIAN_POINT('Ctrl Pts',(35.2753820082045,-1.7531057040892,26.1266504493554));
#46438=CARTESIAN_POINT('Ctrl Pts',(35.1364705177159,1.39098436071829,26.2188735190977));
#46439=CARTESIAN_POINT('Ctrl Pts',(34.9975590272273,4.19618267645299,24.7959645832859));
#46440=CARTESIAN_POINT('Ctrl Pts',(34.8586475367386,5.97904621488101,22.2045933181914));
#46441=CARTESIAN_POINT('Ctrl Pts',(34.7197360462499,6.3052079479044,19.0761071101149));
#46442=CARTESIAN_POINT('Ctrl Pts',(34.5808245557615,5.09520363185058,16.1727130642877));
#46443=CARTESIAN_POINT('Ctrl Pts',(34.4419130652726,2.64383203702432,14.2017780744179));
#46444=CARTESIAN_POINT('Ctrl Pts',(34.3030015747841,-0.451668196904035,
13.6434898585621));
#46445=CARTESIAN_POINT('Ctrl Pts',(34.1640900842954,-3.43712648530661,14.6338666749417));
#46446=CARTESIAN_POINT('Ctrl Pts',(34.0251785938068,-5.58518225554684,16.9316185845593));
#46447=CARTESIAN_POINT('Ctrl Pts',(33.9322348881881,-6.1119620728916,18.9691958825699));
#46448=CARTESIAN_POINT('Ctrl Pts',(33.8855950127323,-6.11377489434444,19.9926182984567));
#46449=CARTESIAN_POINT('Ctrl Pts',(33.8852589674394,-6.11377433895741,19.9999921684411));
#46450=CARTESIAN_POINT('Origin',(53.8647410325606,0.,20.));
#46451=CARTESIAN_POINT('',(37.3852589674394,-6.11338555021776,20.0001503668437));
#46452=CARTESIAN_POINT('',(37.2397410325605,-6.11368048738509,20.0000837791882));
#46453=CARTESIAN_POINT('',(53.8647410325606,-6.11325,19.9999999999994));
#46454=CARTESIAN_POINT('Ctrl Pts',(37.2397410325605,-6.11368048738509,20.0000837791882));
#46455=CARTESIAN_POINT('Ctrl Pts',(37.2359205053585,-6.11373698512472,20.0839216702238));
#46456=CARTESIAN_POINT('Ctrl Pts',(37.1857961479937,-6.09158033549965,21.183823854746));
#46457=CARTESIAN_POINT('Ctrl Pts',(37.0893679604659,-5.46611361180679,23.2757941922132));
#46458=CARTESIAN_POINT('Ctrl Pts',(36.9504564699773,-3.23335168806423,25.4913261119888));
#46459=CARTESIAN_POINT('Ctrl Pts',(36.8115449794887,-0.212833812579934,
26.3689816591933));
#46460=CARTESIAN_POINT('Ctrl Pts',(36.672633489,2.85953771780081,25.6949336824402));
#46461=CARTESIAN_POINT('Ctrl Pts',(36.5337219985114,5.23522726807311,23.6334035089075));
#46462=CARTESIAN_POINT('Ctrl Pts',(36.3948105080228,6.33543495400973,20.6866509669615));
#46463=CARTESIAN_POINT('Ctrl Pts',(36.2558990175341,5.8921122500055,17.572606574893));
#46464=CARTESIAN_POINT('Ctrl Pts',(36.1169875270455,4.01326785177723,15.0499589136242));
#46465=CARTESIAN_POINT('Ctrl Pts',(35.9780760365568,1.15665303412888,13.7333119300896));
#46466=CARTESIAN_POINT('Ctrl Pts',(35.8391645460682,-1.98176234208496,13.9434462252522));
#46467=CARTESIAN_POINT('Ctrl Pts',(35.7002530555796,-4.63735208393372,15.6291658397334));
#46468=CARTESIAN_POINT('Ctrl Pts',(35.583778551077,-5.91668043407849,17.9354935114547));
#46469=CARTESIAN_POINT('Ctrl Pts',(35.5136078767373,-6.11268593354361,19.4760446090339));
#46470=CARTESIAN_POINT('Ctrl Pts',(35.4897410325605,-6.11272955150596,20.0000146122445));
#46471=CARTESIAN_POINT('Ctrl Pts',(37.3852589674394,-6.11338555021775,20.0001503668437));
#46472=CARTESIAN_POINT('Ctrl Pts',(37.3765241001376,-6.11358143049483,20.1918555857849));
#46473=CARTESIAN_POINT('Ctrl Pts',(37.321485402673,-6.05788617552704,21.3996833608107));
#46474=CARTESIAN_POINT('Ctrl Pts',(37.2201428750454,-5.2851402019413,23.5604098618166));
#46475=CARTESIAN_POINT('Ctrl Pts',(37.0812313845568,-2.93828509988496,25.6547065361601));
#46476=CARTESIAN_POINT('Ctrl Pts',(36.9423198940682,0.124437559632812,26.371321733522));
#46477=CARTESIAN_POINT('Ctrl Pts',(36.8034084035795,3.15684293922622,25.5356632841381));
#46478=CARTESIAN_POINT('Ctrl Pts',(36.6644969130909,5.42013253618787,23.3513263983764));
#46479=CARTESIAN_POINT('Ctrl Pts',(36.5255854226022,6.36289097027834,20.3504908538714));
#46480=CARTESIAN_POINT('Ctrl Pts',(36.3866739321137,5.75542978222766,17.2642636530279));
#46481=CARTESIAN_POINT('Ctrl Pts',(36.247762441625,3.74574746168526,14.844556149896));
#46482=CARTESIAN_POINT('Ctrl Pts',(36.1088509511364,0.823471912402398,13.6808925196843));
#46483=CARTESIAN_POINT('Ctrl Pts',(35.9699394606477,-2.29942978666854,14.0567813438779));
#46484=CARTESIAN_POINT('Ctrl Pts',(35.8310279701591,-4.86211110923449,15.8806431448883));
#46485=CARTESIAN_POINT('Ctrl Pts',(35.7194678057564,-5.96886940144111,18.1513987084486));
#46486=CARTESIAN_POINT('Ctrl Pts',(35.6542114715165,-6.11299279628302,19.5838498692729));
#46487=CARTESIAN_POINT('Ctrl Pts',(35.6352589674395,-6.11279596489353,19.9999180648868));
#46488=CARTESIAN_POINT('Origin',(53.8647410325606,0.,20.));
#46489=CARTESIAN_POINT('',(39.1352589674394,-6.11330594686957,19.9998435437343));
#46490=CARTESIAN_POINT('',(38.9897410325605,-6.11298477368481,19.9998596496536));
#46491=CARTESIAN_POINT('',(53.8647410325606,-6.11325,19.9999999999994));
#46492=CARTESIAN_POINT('Ctrl Pts',(38.9897410325605,-6.11298477368481,19.9998596496536));
#46493=CARTESIAN_POINT('Ctrl Pts',(38.9582331339797,-6.1124002527767,20.6914977876344));
#46494=CARTESIAN_POINT('Ctrl Pts',(38.8804214052361,-5.82301090979044,22.4000401985929));
#46495=CARTESIAN_POINT('Ctrl Pts',(38.7563058463296,-4.26232733267651,24.7372767827135));
#46496=CARTESIAN_POINT('Ctrl Pts',(38.6173943558409,-1.47714331403435,26.1989735631571));
#46497=CARTESIAN_POINT('Ctrl Pts',(38.4784828653523,1.66792374532418,26.1503866534309));
#46498=CARTESIAN_POINT('Ctrl Pts',(38.3395713748636,4.40662707311566,24.6033534999391));
#46499=CARTESIAN_POINT('Ctrl Pts',(38.200659884375,6.0717241128045,21.9347847179741));
#46500=CARTESIAN_POINT('Ctrl Pts',(38.0617483938864,6.25753981577645,18.7948356705868));
#46501=CARTESIAN_POINT('Ctrl Pts',(37.9228369033978,4.91880307017454,15.9485062058842));
#46502=CARTESIAN_POINT('Ctrl Pts',(37.7839254129091,2.3816763046193,14.0892603181216));
#46503=CARTESIAN_POINT('Ctrl Pts',(37.6450139224205,-0.735708924935337,
13.6700744092298));
#46504=CARTESIAN_POINT('Ctrl Pts',(37.5061024319318,-3.67385009436911,14.7930766194401));
#46505=CARTESIAN_POINT('Ctrl Pts',(37.3710114686452,-5.660723652261,17.1188882731015));
#46506=CARTESIAN_POINT('Ctrl Pts',(37.2822243355214,-6.11305224670977,19.067827486753));
#46507=CARTESIAN_POINT('Ctrl Pts',(37.2397410325605,-6.11368048738509,20.0000837791882));
#46508=CARTESIAN_POINT('Ctrl Pts',(39.1352589674394,-6.11330594686957,19.9998435437343));
#46509=CARTESIAN_POINT('Ctrl Pts',(39.0988367287589,-6.11248050595374,20.7992369393628));
#46510=CARTESIAN_POINT('Ctrl Pts',(39.0161106599154,-5.75447725529317,22.6156218959943));
#46511=CARTESIAN_POINT('Ctrl Pts',(38.8870807609091,-4.00571514043749,24.9561549160581));
#46512=CARTESIAN_POINT('Ctrl Pts',(38.7481692704204,-1.14709597416125,26.2684444772495));
#46513=CARTESIAN_POINT('Ctrl Pts',(38.6092577799318,1.990995321361,26.0535248383579));
#46514=CARTESIAN_POINT('Ctrl Pts',(38.4703462894431,4.64401151042891,24.3637578334849));
#46515=CARTESIAN_POINT('Ctrl Pts',(38.3314347989546,6.16558637784845,21.6108289653426));
#46516=CARTESIAN_POINT('Ctrl Pts',(38.1925233084659,6.18501182457331,18.4654466225688));
#46517=CARTESIAN_POINT('Ctrl Pts',(38.0536118179773,4.69755514202461,15.6939343913573));
#46518=CARTESIAN_POINT('Ctrl Pts',(37.9147003274886,2.06561206307644,13.9715282083127));
#46519=CARTESIAN_POINT('Ctrl Pts',(37.775788837,-1.06958533326773,13.7178656052934));
#46520=CARTESIAN_POINT('Ctrl Pts',(37.6368773465114,-3.94419486492413,14.9947475382551));
#46521=CARTESIAN_POINT('Ctrl Pts',(37.5067007233245,-5.73752956130376,17.3341100346003));
#46522=CARTESIAN_POINT('Ctrl Pts',(37.4228279303005,-6.11254306245003,19.1756196668516));
#46523=CARTESIAN_POINT('Ctrl Pts',(37.3852589674394,-6.11338555021775,20.0001503668437));
#46524=CARTESIAN_POINT('Origin',(53.8647410325606,0.,20.));
#46525=CARTESIAN_POINT('',(40.8852589674394,-6.11283726768911,20.0001011899177));
#46526=CARTESIAN_POINT('',(40.7397410325605,-6.11310132804271,20.0001544046255));
#46527=CARTESIAN_POINT('',(53.8647410325606,-6.11325,19.9999999999994));
#46528=CARTESIAN_POINT('Ctrl Pts',(40.7397410325605,-6.1131013280427,20.0001544046255));
#46529=CARTESIAN_POINT('Ctrl Pts',(40.7268495927638,-6.11337233064336,20.2831222931156));
#46530=CARTESIAN_POINT('Ctrl Pts',(40.6676543228043,-6.02480017970596,21.5822937801942));
#46531=CARTESIAN_POINT('Ctrl Pts',(40.5621552226819,-5.12049372012104,23.793384988255));
#46532=CARTESIAN_POINT('Ctrl Pts',(40.4232437321932,-2.68225751383601,25.7805467073961));
#46533=CARTESIAN_POINT('Ctrl Pts',(40.2843322417046,0.409469102548303,26.3593679450851));
#46534=CARTESIAN_POINT('Ctrl Pts',(40.145420751216,3.4014349277457,25.388827891038));
#46535=CARTESIAN_POINT('Ctrl Pts',(40.0065092607273,5.56469392878752,23.1053835650098));
#46536=CARTESIAN_POINT('Ctrl Pts',(39.8675977702387,6.37220162748716,20.0653607341416));
#46537=CARTESIAN_POINT('Ctrl Pts',(39.72868627975,5.62722130693377,17.0094137749083));
#46538=CARTESIAN_POINT('Ctrl Pts',(39.5897747892614,3.51125585888291,14.6820767304917));
#46539=CARTESIAN_POINT('Ctrl Pts',(39.4508632987728,0.539827421410421,13.6503691475795));
#46540=CARTESIAN_POINT('Ctrl Pts',(39.3119518082841,-2.56312158825944,14.1656505649116));
#46541=CARTESIAN_POINT('Ctrl Pts',(39.1730403177955,-5.04160580690685,16.1023806631893));
#46542=CARTESIAN_POINT('Ctrl Pts',(39.0656367258876,-6.00821633318123,18.3340291986372));
#46543=CARTESIAN_POINT('Ctrl Pts',(39.0045369641426,-6.11325926140866,19.6750702784136));
#46544=CARTESIAN_POINT('Ctrl Pts',(38.9897410325605,-6.11298477368481,19.9998596496536));
#46545=CARTESIAN_POINT('Ctrl Pts',(40.8852589674394,-6.11283726768911,20.0001011899177));
#46546=CARTESIAN_POINT('Ctrl Pts',(40.8674531875429,-6.11306762891914,20.3909875540726));
#46547=CARTESIAN_POINT('Ctrl Pts',(40.8033435774836,-5.98015945737357,21.7982170396047));
#46548=CARTESIAN_POINT('Ctrl Pts',(40.6929301372614,-4.91261944606622,24.0589894698594));
#46549=CARTESIAN_POINT('Ctrl Pts',(40.5540186467727,-2.37266058160269,25.91436447159));
#46550=CARTESIAN_POINT('Ctrl Pts',(40.4151071562841,0.745360205886424,26.3287963706994));
#46551=CARTESIAN_POINT('Ctrl Pts',(40.2761956657955,3.68178554845507,25.2013152676496));
#46552=CARTESIAN_POINT('Ctrl Pts',(40.1372841753068,5.72120098964531,22.806614432796));
#46553=CARTESIAN_POINT('Ctrl Pts',(39.9983726848182,6.36673461236813,19.728125554767));
#46554=CARTESIAN_POINT('Ctrl Pts',(39.8594611943296,5.46111216921441,16.7158746653705));
#46555=CARTESIAN_POINT('Ctrl Pts',(39.7205497038409,3.22497451167542,14.5037499386089));
#46556=CARTESIAN_POINT('Ctrl Pts',(39.5816382133523,0.203121871393965,13.6307012282624));
#46557=CARTESIAN_POINT('Ctrl Pts',(39.4427267228636,-2.86821826005961,14.3094333014226));
#46558=CARTESIAN_POINT('Ctrl Pts',(39.303815232375,-5.24076153202002,16.3745836235273));
#46559=CARTESIAN_POINT('Ctrl Pts',(39.2013259805669,-6.04918142844035,18.5499403958289));
#46560=CARTESIAN_POINT('Ctrl Pts',(39.1451405589217,-6.11352989438677,19.7829628890735));
#46561=CARTESIAN_POINT('Ctrl Pts',(39.1352589674394,-6.11330594686957,19.9998435437343));
#46562=CARTESIAN_POINT('Origin',(53.8647410325606,0.,20.));
#46563=CARTESIAN_POINT('',(42.6352589674395,-6.11377032462672,19.9999811532723));
#46564=CARTESIAN_POINT('',(42.4897410325605,-6.11358064030395,19.9998832272783));
#46565=CARTESIAN_POINT('',(53.8647410325606,-6.11325,19.9999999999994));
#46566=CARTESIAN_POINT('Ctrl Pts',(42.4897410325605,-6.11358064030395,19.9998832272783));
#46567=CARTESIAN_POINT('Ctrl Pts',(42.4491622213851,-6.1128044966145,20.8903893714117));
#46568=CARTESIAN_POINT('Ctrl Pts',(42.3622795800467,-5.69129834837748,22.7977483927856));
#46569=CARTESIAN_POINT('Ctrl Pts',(42.2290931085455,-3.77988245302682,25.1304692035152));
#46570=CARTESIAN_POINT('Ctrl Pts',(42.0901816180568,-0.865394677250782,
26.3135028042683));
#46571=CARTESIAN_POINT('Ctrl Pts',(41.9512701275682,2.25993307925686,25.9583494429412));
#46572=CARTESIAN_POINT('Ctrl Pts',(41.8123586370795,4.83466321896507,24.151536723444));
#46573=CARTESIAN_POINT('Ctrl Pts',(41.673447146591,6.23150270747516,21.3332665201104));
#46574=CARTESIAN_POINT('Ctrl Pts',(41.5345356561023,6.11013328470932,18.1901666236902));
#46575=CARTESIAN_POINT('Ctrl Pts',(41.3956241656137,4.5001247266669,15.4880045377507));
#46576=CARTESIAN_POINT('Ctrl Pts',(41.256712675125,1.79373062847491,13.8851201124316));
#46577=CARTESIAN_POINT('Ctrl Pts',(41.1178011846364,-1.34967809562946,13.7720312585004));
#46578=CARTESIAN_POINT('Ctrl Pts',(40.9788896941477,-4.16425870100727,15.1762903198884));
#46579=CARTESIAN_POINT('Ctrl Pts',(40.8528696434558,-5.79723424303751,17.5163871102771));
#46580=CARTESIAN_POINT('Ctrl Pts',(40.7731534229267,-6.11239893600378,19.2667504016246));
#46581=CARTESIAN_POINT('Ctrl Pts',(40.7397410325605,-6.1131013280427,20.0001544046255));
#46582=CARTESIAN_POINT('Ctrl Pts',(42.6352589674394,-6.11377032462672,19.9999811532723));
#46583=CARTESIAN_POINT('Ctrl Pts',(42.5897658161642,-6.11359441963512,20.9982430904406));
#46584=CARTESIAN_POINT('Ctrl Pts',(42.497968834726,-5.61028523359083,23.0127267136883));
#46585=CARTESIAN_POINT('Ctrl Pts',(42.3598680231251,-3.5031427704913,25.3232711811303));
#46586=CARTESIAN_POINT('Ctrl Pts',(42.2209565326363,-0.530144605918972,
26.350446601233));
#46587=CARTESIAN_POINT('Ctrl Pts',(42.0820450421478,2.57201506314977,25.8304342765551));
#46588=CARTESIAN_POINT('Ctrl Pts',(41.943133551659,5.04754318408075,23.8899271385383));
#46589=CARTESIAN_POINT('Ctrl Pts',(41.8042220611705,6.2933157545682,21.001699631427));
#46590=CARTESIAN_POINT('Ctrl Pts',(41.6653105706818,6.00581962429792,17.869423557181));
#46591=CARTESIAN_POINT('Ctrl Pts',(41.5263990801932,4.25509876298692,15.256229363099));
#46592=CARTESIAN_POINT('Ctrl Pts',(41.3874875897045,1.46768913436197,13.7987812534008));
#46593=CARTESIAN_POINT('Ctrl Pts',(41.248576099216,-1.67730017084697,13.8521638379692));
#46594=CARTESIAN_POINT('Ctrl Pts',(41.1096646087272,-4.41364132394809,15.4033712786614));
#46595=CARTESIAN_POINT('Ctrl Pts',(40.9885588981351,-5.86175571304379,17.7320917419551));
#46596=CARTESIAN_POINT('Ctrl Pts',(40.9137570177058,-6.11246857584011,19.3744897694183));
#46597=CARTESIAN_POINT('Ctrl Pts',(40.8852589674394,-6.11283726768911,20.0001011899177));
#46598=CARTESIAN_POINT('Origin',(53.8647410325606,0.,20.));
#46599=CARTESIAN_POINT('',(44.3852589674394,-6.11278156388414,19.9999265724237));
#46600=CARTESIAN_POINT('',(44.2397410325605,-6.11273311396858,20.0000242543606));
#46601=CARTESIAN_POINT('',(53.8647410325606,-6.11325,19.9999999999994));
#46602=CARTESIAN_POINT('Ctrl Pts',(44.2397410325605,-6.11273311396858,20.0000242543606));
#46603=CARTESIAN_POINT('Ctrl Pts',(44.2177786801691,-6.11279978336087,20.4821824561146));
#46604=CARTESIAN_POINT('Ctrl Pts',(44.1495124976149,-5.9376425539596,21.9808403899033));
#46605=CARTESIAN_POINT('Ctrl Pts',(44.0349424848978,-4.72603171623352,24.2747923720425));
#46606=CARTESIAN_POINT('Ctrl Pts',(43.8960309944091,-2.10557847814608,26.0146292387217));
#46607=CARTESIAN_POINT('Ctrl Pts',(43.7571195039205,1.02786627402308,26.2890950485458));
#46608=CARTESIAN_POINT('Ctrl Pts',(43.6182080134318,3.91088736273947,25.0313204671222));
#46609=CARTESIAN_POINT('Ctrl Pts',(43.4792965229432,5.84108144907249,22.5477427484381));
#46610=CARTESIAN_POINT('Ctrl Pts',(43.3403850324546,6.34818670374496,19.4434470543486));
#46611=CARTESIAN_POINT('Ctrl Pts',(43.2014735419659,5.30865480258217,16.4747468468295));
#46612=CARTESIAN_POINT('Ctrl Pts',(43.0625620514773,2.9757515580194,14.3649198522237));
#46613=CARTESIAN_POINT('Ctrl Pts',(42.9236505609886,-0.0821473649868688,
13.6279926697042));
#46614=CARTESIAN_POINT('Ctrl Pts',(42.7847390705,-3.12003235757933,14.4435061689429));
#46615=CARTESIAN_POINT('Ctrl Pts',(42.6458275800114,-5.39776989439614,16.6127731439911));
#46616=CARTESIAN_POINT('Ctrl Pts',(42.5474949006982,-6.07921398551127,18.7325287458751));
#46617=CARTESIAN_POINT('Ctrl Pts',(42.4954660515479,-6.11369014172182,19.8742471025154));
#46618=CARTESIAN_POINT('Ctrl Pts',(42.4897410325605,-6.11358064030395,19.9998832272783));
#46619=CARTESIAN_POINT('Ctrl Pts',(44.3852589674395,-6.11278156388414,19.9999265724237));
#46620=CARTESIAN_POINT('Ctrl Pts',(44.3583822749483,-6.11253215560594,20.5899600742025));
#46621=CARTESIAN_POINT('Ctrl Pts',(44.2852017522942,-5.88162653249256,22.1967089582262));
#46622=CARTESIAN_POINT('Ctrl Pts',(44.1657173994773,-4.49323939823524,24.5188521826282));
#46623=CARTESIAN_POINT('Ctrl Pts',(44.0268059089887,-1.78440430929869,26.1176079148025));
#46624=CARTESIAN_POINT('Ctrl Pts',(43.8878944185,1.35917319264309,26.2259034340967));
#46625=CARTESIAN_POINT('Ctrl Pts',(43.7489829280113,4.1716092428508,24.8173542181636));
#46626=CARTESIAN_POINT('Ctrl Pts',(43.6100714375227,5.967697451428,22.2351314204129));
#46627=CARTESIAN_POINT('Ctrl Pts',(43.4711599470341,6.309848804664,19.1083535450766));
#46628=CARTESIAN_POINT('Ctrl Pts',(43.3322484565454,5.11470343610716,16.1988114886301));
#46629=CARTESIAN_POINT('Ctrl Pts',(43.1933369660568,2.67343996414062,14.2153700121414));
#46630=CARTESIAN_POINT('Ctrl Pts',(43.0544254755682,-0.419165658805117,
13.6412638450101));
#46631=CARTESIAN_POINT('Ctrl Pts',(42.9155139850796,-3.40964807513886,14.6163650437647));
#46632=CARTESIAN_POINT('Ctrl Pts',(42.7766024945909,-5.56942266143649,16.9031053365388));
#46633=CARTESIAN_POINT('Ctrl Pts',(42.6831841553776,-6.10935563599417,18.9483542931198));
#46634=CARTESIAN_POINT('Ctrl Pts',(42.6360696463271,-6.11377345921861,19.9821923245347));
#46635=CARTESIAN_POINT('Ctrl Pts',(42.6352589674394,-6.11377032462672,19.9999811532723));
#46636=CARTESIAN_POINT('Origin',(53.8647410325606,0.,20.));
#46637=CARTESIAN_POINT('',(46.1352589674395,-6.11341807123084,20.0001467345291));
#46638=CARTESIAN_POINT('',(45.9897410325605,-6.11370098092917,20.0000743962474));
#46639=CARTESIAN_POINT('',(53.8647410325606,-6.11325,19.9999999999994));
#46640=CARTESIAN_POINT('Ctrl Pts',(45.9897410325605,-6.11370098092917,20.0000743962474));
#46641=CARTESIAN_POINT('Ctrl Pts',(45.9863951389532,-6.11374584420487,20.0734961832118));
#46642=CARTESIAN_POINT('Ctrl Pts',(45.9367454151831,-6.09452688272932,21.1629787472043));
#46643=CARTESIAN_POINT('Ctrl Pts',(45.84079186125,-5.48278915103411,23.2478067572163));
#46644=CARTESIAN_POINT('Ctrl Pts',(45.7018803707614,-3.26138295580096,25.4747243604157));
#46645=CARTESIAN_POINT('Ctrl Pts',(45.5629688802727,-0.245391425534477,
26.3678103501275));
#46646=CARTESIAN_POINT('Ctrl Pts',(45.4240573897841,2.83038591667594,25.7094781871552));
#46647=CARTESIAN_POINT('Ctrl Pts',(45.2851458992955,5.21658366263703,23.6601202845843));
#46648=CARTESIAN_POINT('Ctrl Pts',(45.1462344088069,6.33184176934682,20.719030885896));
#46649=CARTESIAN_POINT('Ctrl Pts',(45.0073229183182,5.90444490978662,17.6027607724275));
#46650=CARTESIAN_POINT('Ctrl Pts',(44.8684114278296,4.03852169487032,15.0705407875732));
#46651=CARTESIAN_POINT('Ctrl Pts',(44.7294999373409,1.18867535364643,13.7393070263308));
#46652=CARTESIAN_POINT('Ctrl Pts',(44.5905884468523,-1.95077328725316,13.9333939316404));
#46653=CARTESIAN_POINT('Ctrl Pts',(44.4516769563636,-4.61494629599519,15.6055152415786));
#46654=CARTESIAN_POINT('Ctrl Pts',(44.3347278182664,-5.91130989900841,17.9146439238443));
#46655=CARTESIAN_POINT('Ctrl Pts',(44.264082510332,-6.11265922245179,19.4656350896121));
#46656=CARTESIAN_POINT('Ctrl Pts',(44.2397410325605,-6.11273311396858,20.0000242543606));
#46657=CARTESIAN_POINT('Ctrl Pts',(46.1352589674395,-6.11341807123084,20.0001467345292));
#46658=CARTESIAN_POINT('Ctrl Pts',(46.1269987337324,-6.11360120807088,20.1814323295707));
#46659=CARTESIAN_POINT('Ctrl Pts',(46.0724346698624,-6.06139532481641,21.3788331453416));
#46660=CARTESIAN_POINT('Ctrl Pts',(45.9715667758295,-5.30327315797554,23.5333439048828));
#46661=CARTESIAN_POINT('Ctrl Pts',(45.832655285341,-2.96715547971806,25.6396111299885));
#46662=CARTESIAN_POINT('Ctrl Pts',(45.6937437948522,0.0918635759318163,
26.371874639516));
#46663=CARTESIAN_POINT('Ctrl Pts',(45.5548323043637,3.12850149718234,25.5517297953366));
#46664=CARTESIAN_POINT('Ctrl Pts',(45.4159208138749,5.40292858824861,23.3789921587039));
#46665=CARTESIAN_POINT('Ctrl Pts',(45.2770093233864,6.36101599132474,20.3830155302438));
#46666=CARTESIAN_POINT('Ctrl Pts',(45.1380978328977,5.76934058177901,17.2937231128846));
#46667=CARTESIAN_POINT('Ctrl Pts',(44.9991863424091,3.77205488934985,14.8637730531032));
#46668=CARTESIAN_POINT('Ctrl Pts',(44.8602748519205,0.855766571765285,13.6851849660543));
#46669=CARTESIAN_POINT('Ctrl Pts',(44.7213633614318,-2.26901598809372,14.0451035454785));
#46670=CARTESIAN_POINT('Ctrl Pts',(44.5824518709432,-4.84098802139722,15.8558402160407));
#46671=CARTESIAN_POINT('Ctrl Pts',(44.4704170729457,-5.96409876329752,18.130544729991));
#46672=CARTESIAN_POINT('Ctrl Pts',(44.4046861051111,-6.1129618423525,19.5734357728683));
#46673=CARTESIAN_POINT('Ctrl Pts',(44.3852589674395,-6.11278156388414,19.9999265724237));
#46674=CARTESIAN_POINT('Origin',(53.8647410325606,0.,20.));
#46675=CARTESIAN_POINT('',(47.8852589674394,-6.1132728958666,19.9998421342197));
#46676=CARTESIAN_POINT('',(47.7397410325605,-6.1129581875993,19.99986454581));
#46677=CARTESIAN_POINT('',(53.8647410325606,-6.11325,19.9999999999994));
#46678=CARTESIAN_POINT('Ctrl Pts',(47.7397410325605,-6.1129581875993,19.99986454581));
#46679=CARTESIAN_POINT('Ctrl Pts',(47.7087077675744,-6.11240605145268,20.6810923733887));
#46680=CARTESIAN_POINT('Ctrl Pts',(47.6313706724255,-5.82928215365088,22.3792079115881));
#46681=CARTESIAN_POINT('Ctrl Pts',(47.5077297471136,-4.28649019781716,24.71542441243));
#46682=CARTESIAN_POINT('Ctrl Pts',(47.3688182566251,-1.50881526580176,26.1913408969229));
#46683=CARTESIAN_POINT('Ctrl Pts',(47.2299067661364,1.63645908624929,26.1588332714235));
#46684=CARTESIAN_POINT('Ctrl Pts',(47.0909952756477,4.38303558259688,24.6258215150332));
#46685=CARTESIAN_POINT('Ctrl Pts',(46.9520837851591,6.06175349129441,21.9658001469101));
#46686=CARTESIAN_POINT('Ctrl Pts',(46.8131722946704,6.26361925046179,18.8268420855787));
#46687=CARTESIAN_POINT('Ctrl Pts',(46.6742608041818,4.93945140114888,15.9737057406808));
#46688=CARTESIAN_POINT('Ctrl Pts',(46.5353493136932,2.41186288654182,14.1015134972249));
#46689=CARTESIAN_POINT('Ctrl Pts',(46.3964378232046,-0.703338584205735,
13.6663959357331));
#46690=CARTESIAN_POINT('Ctrl Pts',(46.257526332716,-3.64718252590797,14.7743626963189));
#46691=CARTESIAN_POINT('Ctrl Pts',(46.1219607358346,-5.65294289701776,17.0981221826294));
#46692=CARTESIAN_POINT('Ctrl Pts',(46.0326989691161,-6.11312498121801,19.0574118861948));
#46693=CARTESIAN_POINT('Ctrl Pts',(45.9897410325605,-6.11370098092917,20.0000743962474));
#46694=CARTESIAN_POINT('Ctrl Pts',(47.8852589674394,-6.1132728958666,19.9998421342197));
#46695=CARTESIAN_POINT('Ctrl Pts',(47.8493113623536,-6.11246000348838,20.7888305772424));
#46696=CARTESIAN_POINT('Ctrl Pts',(47.7670599271048,-5.76138532239845,22.5948112591935));
#46697=CARTESIAN_POINT('Ctrl Pts',(47.6385046616932,-4.03100033593876,24.9356115677216));
#46698=CARTESIAN_POINT('Ctrl Pts',(47.4995931712046,-1.17912739907028,26.2624982202955));
#46699=CARTESIAN_POINT('Ctrl Pts',(47.3606816807159,1.96002163140553,26.0636243719931));
#46700=CARTESIAN_POINT('Ctrl Pts',(47.2217701902273,4.62164181175045,24.387442570214));
#46701=CARTESIAN_POINT('Ctrl Pts',(47.0828586997386,6.15727070156947,21.6423284830756));
#46702=CARTESIAN_POINT('Ctrl Pts',(46.94394720925,6.19277615550858,18.4970865545706));
#46703=CARTESIAN_POINT('Ctrl Pts',(46.8050357187613,4.71950782178093,15.7180061583685));
#46704=CARTESIAN_POINT('Ctrl Pts',(46.6661242282728,2.09640466180927,13.9821670984087));
#46705=CARTESIAN_POINT('Ctrl Pts',(46.527212737784,-1.03745495420322,13.7124796177954));
#46706=CARTESIAN_POINT('Ctrl Pts',(46.3883012472955,-3.91855477371191,14.9746488855395));
#46707=CARTESIAN_POINT('Ctrl Pts',(46.2576499905139,-5.73040780021207,17.3133086251774));
#46708=CARTESIAN_POINT('Ctrl Pts',(46.1733025638953,-6.11257461034511,19.1652120019819));
#46709=CARTESIAN_POINT('Ctrl Pts',(46.1352589674395,-6.11341807123084,20.0001467345292));
#46710=CARTESIAN_POINT('Origin',(53.8647410325606,0.,20.));
#46711=CARTESIAN_POINT('',(49.6352589674395,-6.11286344962028,20.0001278181581));
#46712=CARTESIAN_POINT('',(49.4897410325605,-6.11313234159337,20.00015660207));
#46713=CARTESIAN_POINT('',(53.8647410325606,-6.11325,19.9999999999994));
#46714=CARTESIAN_POINT('',(50.,-1.57888188187521,14.0941590297752));
#46715=CARTESIAN_POINT('Ctrl Pts',(50.,-1.57888188187519,14.0941590297752));
#46716=CARTESIAN_POINT('Ctrl Pts',(49.9536961698371,-2.56072134667313,14.356646379112));
#46717=CARTESIAN_POINT('Ctrl Pts',(49.8610885095113,-4.38996617743935,15.3805039208954));
#46718=CARTESIAN_POINT('Ctrl Pts',(49.7395081653245,-5.85584351099758,17.7113562466293));
#46719=CARTESIAN_POINT('Ctrl Pts',(49.6642316513006,-6.11246881893309,19.3641290267299));
#46720=CARTESIAN_POINT('Ctrl Pts',(49.6352589674395,-6.11286344962028,20.0001278181581));
#46721=CARTESIAN_POINT('',(50.,1.57906037163134,14.0937031294847));
#46722=CARTESIAN_POINT('Origin',(50.,0.,20.));
#46723=CARTESIAN_POINT('Ctrl Pts',(50.,1.57906037163134,14.0937031294847));
#46724=CARTESIAN_POINT('Ctrl Pts',(49.9564083618068,0.654826993355806,13.8471232379456));
#46725=CARTESIAN_POINT('Ctrl Pts',(49.8665128934508,-1.37290819747911,13.7923707941805));
#46726=CARTESIAN_POINT('Ctrl Pts',(49.7303135949318,-4.13954687382562,15.1550528216166));
#46727=CARTESIAN_POINT('Ctrl Pts',(49.6038189106453,-5.79065559120778,17.495568430254));
#46728=CARTESIAN_POINT('Ctrl Pts',(49.5236280565214,-6.1124042328096,19.2563462638635));
#46729=CARTESIAN_POINT('Ctrl Pts',(49.4897410325605,-6.11313234159337,20.00015660207));
#46730=CARTESIAN_POINT('Origin',(53.8647410325606,0.,20.));
#46731=CARTESIAN_POINT('Ctrl Pts',(49.4897410325605,-6.11313234159337,20.00015660207));
#46732=CARTESIAN_POINT('Ctrl Pts',(49.4773242263585,-6.11339913355694,20.2727018934829));
#46733=CARTESIAN_POINT('Ctrl Pts',(49.4186035899936,-6.02879365594887,21.5614386427174));
#46734=CARTESIAN_POINT('Ctrl Pts',(49.313579123466,-5.13981947893865,23.7671592113954));
#46735=CARTESIAN_POINT('Ctrl Pts',(49.1746676329772,-2.71177477849166,25.7667577971016));
#46736=CARTESIAN_POINT('Ctrl Pts',(49.0357561424887,0.376952608096762,26.3613785707909));
#46737=CARTESIAN_POINT('Ctrl Pts',(48.896844652,3.37384090977041,25.4061465625371));
#46738=CARTESIAN_POINT('Ctrl Pts',(48.7579331615114,5.54874546123675,23.1337916855913));
#46739=CARTESIAN_POINT('Ctrl Pts',(48.6190216710227,6.37178419535544,20.0979366854017));
#46740=CARTESIAN_POINT('Ctrl Pts',(48.4801101805342,5.64243666772738,17.0382211455748));
#46741=CARTESIAN_POINT('Ctrl Pts',(48.3411986900455,3.53839699735355,14.7000969433883));
#46742=CARTESIAN_POINT('Ctrl Pts',(48.2022871995569,0.572281835046422,13.653211912598));
#46743=CARTESIAN_POINT('Ctrl Pts',(48.0633757090682,-2.53326092100598,14.1526232585264));
#46744=CARTESIAN_POINT('Ctrl Pts',(47.9244642185796,-5.02161397036119,16.0766572005871));
#46745=CARTESIAN_POINT('Ctrl Pts',(47.816585993077,-6.00394277771977,18.3131749736855));
#46746=CARTESIAN_POINT('Ctrl Pts',(47.7550115977373,-6.11322987770401,19.664652187524));
#46747=CARTESIAN_POINT('Ctrl Pts',(47.7397410325605,-6.1129581875993,19.99986454581));
#46748=CARTESIAN_POINT('Ctrl Pts',(49.6352589674395,-6.11286344962028,20.0001278181581));
#46749=CARTESIAN_POINT('Ctrl Pts',(49.6179278211377,-6.11309951343155,20.3805754202803));
#46750=CARTESIAN_POINT('Ctrl Pts',(49.554292844673,-5.9847147188434,21.7773037579676));
#46751=CARTESIAN_POINT('Ctrl Pts',(49.4443540380453,-4.93332128443375,24.0338649607667));
#46752=CARTESIAN_POINT('Ctrl Pts',(49.3054425475569,-2.40285814042326,25.9021352451997));
#46753=CARTESIAN_POINT('Ctrl Pts',(49.1665310570681,0.712991615200806,26.332535419579));
#46754=CARTESIAN_POINT('Ctrl Pts',(49.0276195665795,3.65514852614605,25.2200641339167));
#46755=CARTESIAN_POINT('Ctrl Pts',(48.8887080760909,5.70677685429529,22.8358293701168));
#46756=CARTESIAN_POINT('Ctrl Pts',(48.7497965856023,6.36804183630338,19.7606765440198));
#46757=CARTESIAN_POINT('Ctrl Pts',(48.6108850951136,5.47783010606213,16.7438373869472));
#46758=CARTESIAN_POINT('Ctrl Pts',(48.471973604625,3.25303119352331,14.5203085482529));
#46759=CARTESIAN_POINT('Ctrl Pts',(48.3330621141364,0.235681165538501,13.6318230833962));
#46760=CARTESIAN_POINT('Ctrl Pts',(48.1941506236477,-2.83908863701214,14.2948442639057));
#46761=CARTESIAN_POINT('Ctrl Pts',(48.0552391331592,-5.22215870445453,16.3478385001443));
#46762=CARTESIAN_POINT('Ctrl Pts',(47.9522752477563,-6.04548447131879,18.5290888028145));
#46763=CARTESIAN_POINT('Ctrl Pts',(47.8956151925164,-6.11350708383023,19.7725407081699));
#46764=CARTESIAN_POINT('Ctrl Pts',(47.8852589674394,-6.1132728958666,19.9998421342197));
#46765=CARTESIAN_POINT('Ctrl Pts',(50.,3.87994761181434,23.3663343702128));
#46766=CARTESIAN_POINT('Ctrl Pts',(49.9536961698371,4.43959694085051,22.7212974134384));
#46767=CARTESIAN_POINT('Ctrl Pts',(49.8610885095113,5.23040625982842,21.1473591665083));
#46768=CARTESIAN_POINT('Ctrl Pts',(49.7221770190228,5.14179909425296,18.5053810374451));
#46769=CARTESIAN_POINT('Ctrl Pts',(49.583265528534,3.80064971386127,16.2281825446883));
#46770=CARTESIAN_POINT('Ctrl Pts',(49.4443540380455,1.5334472851601,14.869615687937));
#46771=CARTESIAN_POINT('Ctrl Pts',(49.3054425475568,-1.10731381638287,14.7611453275656));
#46772=CARTESIAN_POINT('Ctrl Pts',(49.1665310570682,-3.47831634631721,15.9289604680716));
#46773=CARTESIAN_POINT('Ctrl Pts',(49.0276195665795,-5.00187030240194,18.0886618719085));
#46774=CARTESIAN_POINT('Ctrl Pts',(48.8887080760909,-5.30680167200989,20.7140104959872));
#46775=CARTESIAN_POINT('Ctrl Pts',(48.7497965856023,-4.31881040501176,23.1654120278307));
#46776=CARTESIAN_POINT('Ctrl Pts',(48.6108850951136,-2.27860942925891,24.8456047297691));
#46777=CARTESIAN_POINT('Ctrl Pts',(48.471973604625,0.316740082548733,25.345243753079));
#46778=CARTESIAN_POINT('Ctrl Pts',(48.3330621141364,2.83492042583946,24.5425957314215));
#46779=CARTESIAN_POINT('Ctrl Pts',(48.1941506236477,4.66241659477494,22.6332154649264));
#46780=CARTESIAN_POINT('Ctrl Pts',(48.0552391331591,5.35398723518456,20.0822927687788));
#46781=CARTESIAN_POINT('Ctrl Pts',(47.9163276426705,4.74114203622437,17.5113208963368));
#46782=CARTESIAN_POINT('Ctrl Pts',(47.7774161521818,2.97319114646969,15.5466769678894));
#46783=CARTESIAN_POINT('Ctrl Pts',(47.6385046616932,0.480868395072131,14.6670161194189));
#46784=CARTESIAN_POINT('Ctrl Pts',(47.4995931712046,-2.12861048312721,15.0866539930864));
#46785=CARTESIAN_POINT('Ctrl Pts',(47.3606816807159,-4.21948645356445,16.7033523698713));
#46786=CARTESIAN_POINT('Ctrl Pts',(47.2217701902273,-5.28235004472098,19.1232277661683));
#46787=CARTESIAN_POINT('Ctrl Pts',(47.0828586997386,-5.05825103762128,21.7567151113327));
#46788=CARTESIAN_POINT('Ctrl Pts',(46.94394720925,-3.60178767818055,23.9622060852329));
#46789=CARTESIAN_POINT('Ctrl Pts',(46.8050357187614,-1.2678046565423,25.2023670473592));
#46790=CARTESIAN_POINT('Ctrl Pts',(46.6661242282727,1.37505929109574,25.1750520274788));
#46791=CARTESIAN_POINT('Ctrl Pts',(46.5272127377841,3.68291138574482,23.8869159068166));
#46792=CARTESIAN_POINT('Ctrl Pts',(46.3883012472954,5.09347928620727,21.6517930568259));
#46793=CARTESIAN_POINT('Ctrl Pts',(46.2493897568068,5.26310001796256,19.0142364671977));
#46794=CARTESIAN_POINT('Ctrl Pts',(46.1104782663182,4.15044812249646,16.6168458616026));
#46795=CARTESIAN_POINT('Ctrl Pts',(45.9715667758295,2.0266039639216,15.0437082496005));
#46796=CARTESIAN_POINT('Ctrl Pts',(45.8326552853409,-0.590990794163301,
14.6780941925943));
#46797=CARTESIAN_POINT('Ctrl Pts',(45.6937437948523,-3.06459981842027,15.609079880639));
#46798=CARTESIAN_POINT('Ctrl Pts',(45.5548323043636,-4.79156666466196,17.6098451013006));
#46799=CARTESIAN_POINT('Ctrl Pts',(45.415920813875,-5.35114266623027,20.1929344638081));
#46800=CARTESIAN_POINT('Ctrl Pts',(45.2770093233863,-4.60699581590389,22.7290183388755));
#46801=CARTESIAN_POINT('Ctrl Pts',(45.1380978328978,-2.74042594335429,24.6002192546297));
#46802=CARTESIAN_POINT('Ctrl Pts',(44.999186342409,-0.206193825725144,25.3506481521314));
#46803=CARTESIAN_POINT('Ctrl Pts',(44.8602748519205,2.37827421706705,24.797474678423));
#46804=CARTESIAN_POINT('Ctrl Pts',(44.7213633614318,4.3833126616858,23.0754709641907));
#46805=CARTESIAN_POINT('Ctrl Pts',(44.5824518709432,5.32042501266795,20.6041764860142));
#46806=CARTESIAN_POINT('Ctrl Pts',(44.4435403804546,4.9612983912561,17.9856837848553));
#46807=CARTESIAN_POINT('Ctrl Pts',(44.3046288899659,3.39342842450826,15.8579479639417));
#46808=CARTESIAN_POINT('Ctrl Pts',(44.1657173994772,0.998802293844237,14.7393588300012));
#46809=CARTESIAN_POINT('Ctrl Pts',(44.0268059089887,-1.63916651262383,14.902443263134));
#46810=CARTESIAN_POINT('Ctrl Pts',(43.8878944185,-3.87777784091168,16.3074682725521));
#46811=CARTESIAN_POINT('Ctrl Pts',(43.7489829280114,-5.17162878789402,18.6121213230614));
#46812=CARTESIAN_POINT('Ctrl Pts',(43.6100714375227,-5.20549265308095,21.254909470996));
#46813=CARTESIAN_POINT('Ctrl Pts',(43.4711599470341,-3.9711190313438,23.5919584046275));
#46814=CARTESIAN_POINT('Ctrl Pts',(43.3322484565454,-1.7692438960646,25.053882426206));
#46815=CARTESIAN_POINT('Ctrl Pts',(43.1933369660568,0.863680052850456,25.2845064393927));
#46816=CARTESIAN_POINT('Ctrl Pts',(43.0544254755682,3.28618176265521,24.2276424830475));
#46817=CARTESIAN_POINT('Ctrl Pts',(42.9155139850795,4.90805629305576,22.1407790558278));
#46818=CARTESIAN_POINT('Ctrl Pts',(42.7766024945909,5.3341590889399,19.5323480401464));
#46819=CARTESIAN_POINT('Ctrl Pts',(42.6376910041023,4.46067681792238,17.0378531657386));
#46820=CARTESIAN_POINT('Ctrl Pts',(42.4987795136136,2.500419877423,15.2650393899988));
#46821=CARTESIAN_POINT('Ctrl Pts',(42.359868023125,-0.0690255554895172,
14.6458252723352));
#46822=CARTESIAN_POINT('Ctrl Pts',(42.2209565326364,-2.6216539831997,15.3310727212722));
#46823=CARTESIAN_POINT('Ctrl Pts',(42.0820450421477,-4.53555711038145,17.1538318320691));
#46824=CARTESIAN_POINT('Ctrl Pts',(41.9431335516591,-5.34444214709172,19.6700156396664));
#46825=CARTESIAN_POINT('Ctrl Pts',(41.8042220611705,-4.85123680939198,22.2665950147469));
#46826=CARTESIAN_POINT('Ctrl Pts',(41.6653105706818,-3.17610292243659,24.3109536958502));
#46827=CARTESIAN_POINT('Ctrl Pts',(41.5263990801932,-0.727160856887576,
25.30501542221));
#46828=CARTESIAN_POINT('Ctrl Pts',(41.3874875897045,1.89894266468289,25.0065924837081));
#46829=CARTESIAN_POINT('Ctrl Pts',(41.2485760992159,4.06239828078662,23.4883909972847));
#46830=CARTESIAN_POINT('Ctrl Pts',(41.1096646087273,5.236113611029,21.120297190067));
#46831=CARTESIAN_POINT('Ctrl Pts',(40.9707531182386,5.13413113323201,18.4792603613856));
#46832=CARTESIAN_POINT('Ctrl Pts',(40.83184162775,3.78129729517135,16.2087281412163));
#46833=CARTESIAN_POINT('Ctrl Pts',(40.6929301372613,1.50720906323453,14.8618804625253));
#46834=CARTESIAN_POINT('Ctrl Pts',(40.5540186467727,-1.13408726254032,14.766855856885));
#46835=CARTESIAN_POINT('Ctrl Pts',(40.4151071562841,-3.49908082973853,15.9468055945179));
#46836=CARTESIAN_POINT('Ctrl Pts',(40.2761956657955,-5.01157766438919,18.1142532366539));
#46837=CARTESIAN_POINT('Ctrl Pts',(40.1372841753068,-5.30308138922381,20.7411338077184));
#46838=CARTESIAN_POINT('Ctrl Pts',(39.9983726848182,-4.30257164631444,23.1874486301752));
#46839=CARTESIAN_POINT('Ctrl Pts',(39.8594611943296,-2.25380710492735,24.8571910684525));
#46840=CARTESIAN_POINT('Ctrl Pts',(39.7205497038409,0.344062554699214,25.343554294674));
#46841=CARTESIAN_POINT('Ctrl Pts',(39.5816382133522,2.8581067133027,24.5280434579462));
#46842=CARTESIAN_POINT('Ctrl Pts',(39.4427267228637,4.67581753383213,22.6093451155382));
#46843=CARTESIAN_POINT('Ctrl Pts',(39.303815232375,5.35433798879396,20.0549203371532));
#46844=CARTESIAN_POINT('Ctrl Pts',(39.1649037418864,4.72835710111512,17.4871150710768));
#46845=CARTESIAN_POINT('Ctrl Pts',(39.0259922513977,2.95038539780261,15.531535213733));
#46846=CARTESIAN_POINT('Ctrl Pts',(38.8870807609091,0.453598087257998,14.6646274434759));
#46847=CARTESIAN_POINT('Ctrl Pts',(38.7481692704204,-2.15370135664199,15.0976003826622));
#46848=CARTESIAN_POINT('Ctrl Pts',(38.6092577799318,-4.2362848940627,16.7249668951274));
#46849=CARTESIAN_POINT('Ctrl Pts',(38.4703462894432,-5.28676337130995,19.150244389574));
#46850=CARTESIAN_POINT('Ctrl Pts',(38.3314347989546,-5.04920401259486,21.7825516488649));
#46851=CARTESIAN_POINT('Ctrl Pts',(38.1925233084659,-3.58148446834762,23.9805678671089));
#46852=CARTESIAN_POINT('Ctrl Pts',(38.0536118179773,-1.24119182404874,25.2087805096385));
#46853=CARTESIAN_POINT('Ctrl Pts',(37.9147003274886,1.4014979427954,25.1679546300268));
#46854=CARTESIAN_POINT('Ctrl Pts',(37.775788837,3.70273448948216,23.8680368201549));
#46855=CARTESIAN_POINT('Ctrl Pts',(37.6368773465113,5.10185725047209,21.625731877488));
#46856=CARTESIAN_POINT('Ctrl Pts',(37.4979658560227,5.25799168178786,18.9873425969634));
#46857=CARTESIAN_POINT('Ctrl Pts',(37.3590543655341,4.13309805270831,16.5956715745431));
#46858=CARTESIAN_POINT('Ctrl Pts',(37.2201428750455,2.00123923571802,15.0334123320837));
#46859=CARTESIAN_POINT('Ctrl Pts',(37.0812313845568,-0.618190458456889,
14.6811850851202));
#46860=CARTESIAN_POINT('Ctrl Pts',(36.9423198940682,-3.0870076427842,15.624804535216));
#46861=CARTESIAN_POINT('Ctrl Pts',(36.8034084035795,-4.80372333049662,17.6343724499157));
#46862=CARTESIAN_POINT('Ctrl Pts',(36.6644969130909,-5.35008639059716,20.2202887986762));
#46863=CARTESIAN_POINT('Ctrl Pts',(36.5255854226023,-4.59298394396574,22.7525352008917));
#46864=CARTESIAN_POINT('Ctrl Pts',(36.3866739321136,-2.71687225022107,24.6141691253848));
#46865=CARTESIAN_POINT('Ctrl Pts',(36.247762441625,-0.178836803135813,25.3516323621414));
#46866=CARTESIAN_POINT('Ctrl Pts',(36.1088509511364,2.40276945518559,24.7852534401954));
#46867=CARTESIAN_POINT('Ctrl Pts',(35.9699394606477,4.39897823077324,23.0530217927257));
#46868=CARTESIAN_POINT('Ctrl Pts',(35.8310279701591,5.32344423997211,20.5769687734903));
#46869=CARTESIAN_POINT('Ctrl Pts',(35.6921164796704,4.95093568890783,17.9603462681195));
#46870=CARTESIAN_POINT('Ctrl Pts',(35.5532049891818,3.37220850408812,15.8406537356658));
#46871=CARTESIAN_POINT('Ctrl Pts',(35.4142934986931,0.971895059593761,14.7343213604691));
#46872=CARTESIAN_POINT('Ctrl Pts',(35.2753820082046,-1.66520553072505,14.9108898536072));
#46873=CARTESIAN_POINT('Ctrl Pts',(35.1364705177159,-3.8966046402726,16.3273410423671));
#46874=CARTESIAN_POINT('Ctrl Pts',(34.9975590272272,-5.17865651107395,18.6385785803116));
#46875=CARTESIAN_POINT('Ctrl Pts',(34.8586475367386,-5.19900910440918,21.2815053156134));
#46876=CARTESIAN_POINT('Ctrl Pts',(34.71973604625,-3.95270382681866,23.6122131718835));
#46877=CARTESIAN_POINT('Ctrl Pts',(34.5808245557613,-1.74338361443369,25.0628613564465));
#46878=CARTESIAN_POINT('Ctrl Pts',(34.4419130652727,0.890684955362837,25.2800219556329));
#46879=CARTESIAN_POINT('Ctrl Pts',(34.3030015747841,3.30775196071341,24.2107871601485));
#46880=CARTESIAN_POINT('Ctrl Pts',(34.1640900842955,4.91893654270863,22.1156594315912));
#46881=CARTESIAN_POINT('Ctrl Pts',(34.0251785938068,5.33169858623931,19.5050841211186));
#46882=CARTESIAN_POINT('Ctrl Pts',(33.8862671033182,4.44547502616015,17.0150873826088));
#46883=CARTESIAN_POINT('Ctrl Pts',(33.7473556128296,2.47618047720463,15.2523182724633));
#46884=CARTESIAN_POINT('Ctrl Pts',(33.6084441223409,-0.0963970105370617,
14.6462481232285));
#46885=CARTESIAN_POINT('Ctrl Pts',(33.4695326318523,-2.64548886290509,15.3445365195375));
#46886=CARTESIAN_POINT('Ctrl Pts',(33.3306211413636,-4.55004841626188,17.1770563322397));
#46887=CARTESIAN_POINT('Ctrl Pts',(33.191709650875,-5.34605929739887,19.6973425527592));
#46888=CARTESIAN_POINT('Ctrl Pts',(33.0527981603863,-4.83958581055438,22.2913665625464));
#46889=CARTESIAN_POINT('Ctrl Pts',(32.9138866698977,-3.15402235947797,24.3271346752312));
#46890=CARTESIAN_POINT('Ctrl Pts',(32.7749751794091,-0.700030316245315,
25.3086635887022));
#46891=CARTESIAN_POINT('Ctrl Pts',(32.6360636889204,1.9245132478929,24.9968190181714));
#46892=CARTESIAN_POINT('Ctrl Pts',(32.4971521984318,4.08017903086373,23.4675770528966));
#46893=CARTESIAN_POINT('Ctrl Pts',(32.3582407079432,5.24177252420404,21.0935137613101));
#46894=CARTESIAN_POINT('Ctrl Pts',(32.2193292174545,5.12628950314575,18.4530328149528));
#46895=CARTESIAN_POINT('Ctrl Pts',(32.0804177269659,3.76186561327901,16.1894464117002));
#46896=CARTESIAN_POINT('Ctrl Pts',(31.9415062364773,1.48092155721679,14.8542422440378));
#46897=CARTESIAN_POINT('Ctrl Pts',(31.8025947459886,-1.16082604986853,14.7727220828024));
#46898=CARTESIAN_POINT('Ctrl Pts',(31.6636832555,-3.51975640787564,15.9647470499492));
#46899=CARTESIAN_POINT('Ctrl Pts',(31.5247717650114,-5.0211527496418,18.1398987644648));
#46900=CARTESIAN_POINT('Ctrl Pts',(31.3858602745227,-5.29922316069158,20.7682352731195));
#46901=CARTESIAN_POINT('Ctrl Pts',(31.2469487840341,-4.28622010149303,23.209403181782));
#46902=CARTESIAN_POINT('Ctrl Pts',(31.1080372935454,-2.22894604390901,24.8686498205372));
#46903=CARTESIAN_POINT('Ctrl Pts',(30.9691258030568,0.371376120282793,25.3417255001506));
#46904=CARTESIAN_POINT('Ctrl Pts',(30.8302143125681,2.88121825714956,24.5133726742142));
#46905=CARTESIAN_POINT('Ctrl Pts',(30.6913028220796,4.68909628701403,22.5854066513387));
#46906=CARTESIAN_POINT('Ctrl Pts',(30.5523913315909,5.35454878920669,20.0275464277232));
#46907=CARTESIAN_POINT('Ctrl Pts',(30.4134798411023,4.7154485905101,17.4629749445598));
#46908=CARTESIAN_POINT('Ctrl Pts',(30.2745683506136,2.92750253442696,15.5165102372595));
#46909=CARTESIAN_POINT('Ctrl Pts',(30.135656860125,0.426315925592653,14.6623782193507));
#46910=CARTESIAN_POINT('Ctrl Pts',(29.9967453696363,-2.17873594137227,15.1086748994319));
#46911=CARTESIAN_POINT('Ctrl Pts',(29.8578338791477,-4.25297261386722,16.746667018676));
#46912=CARTESIAN_POINT('Ctrl Pts',(29.7189223886591,-5.29103852227984,19.1772832216213));
#46913=CARTESIAN_POINT('Ctrl Pts',(29.5800108981704,-5.04002502055383,21.8083415976708));
#46914=CARTESIAN_POINT('Ctrl Pts',(29.4410994076818,-3.56108765223307,23.9988256119501));
#46915=CARTESIAN_POINT('Ctrl Pts',(29.3021879171931,-1.21454655151411,25.2150578343754));
#46916=CARTESIAN_POINT('Ctrl Pts',(29.1632764267045,1.4278999646765,25.1607221619219));
#46917=CARTESIAN_POINT('Ctrl Pts',(29.0243649362159,3.72246081788218,23.8490566378019));
#46918=CARTESIAN_POINT('Ctrl Pts',(28.8854534457272,5.11010187166212,21.5996282077128));
#46919=CARTESIAN_POINT('Ctrl Pts',(28.7465419552387,5.25274592178536,18.960475193734));
#46920=CARTESIAN_POINT('Ctrl Pts',(28.6076304647499,4.11563995951487,16.5745862636289));
#46921=CARTESIAN_POINT('Ctrl Pts',(28.4687189742614,1.97582220276126,15.0232462222096));
#46922=CARTESIAN_POINT('Ctrl Pts',(28.3298074837727,-0.645373965612155,
14.6844149911618));
#46923=CARTESIAN_POINT('Ctrl Pts',(28.1908959932841,-3.10933478455334,15.6406435406999));
#46924=CARTESIAN_POINT('Ctrl Pts',(28.0519845027954,-4.81575444534233,17.6589616270038));
#46925=CARTESIAN_POINT('Ctrl Pts',(27.9130730123068,-5.34889028413044,20.2476373760362));
#46926=CARTESIAN_POINT('Ctrl Pts',(27.7741615218182,-4.57885202896163,22.7759801221459));
#46927=CARTESIAN_POINT('Ctrl Pts',(27.6352500313295,-2.69324754841923,24.6279983993741));
#46928=CARTESIAN_POINT('Ctrl Pts',(27.4963385408409,-0.151475106435163,
25.352476700912));
#46929=CARTESIAN_POINT('Ctrl Pts',(27.3574270503523,2.42720189408347,24.7729071337113));
#46930=CARTESIAN_POINT('Ctrl Pts',(27.2185155598636,4.41452882736344,23.0304928269264));
#46931=CARTESIAN_POINT('Ctrl Pts',(27.079604069375,5.32632433276681,20.5497459812053));
#46932=CARTESIAN_POINT('Ctrl Pts',(26.9406925788863,4.94044358800147,17.9350620601456));
#46933=CARTESIAN_POINT('Ctrl Pts',(26.8017810883977,3.35090044701153,15.8234682168224));
#46934=CARTESIAN_POINT('Ctrl Pts',(26.6628695979091,0.944962423716766,14.7294215156742));
#46935=CARTESIAN_POINT('Ctrl Pts',(26.5239581074204,-1.69120102671082,14.9194694539913));
#46936=CARTESIAN_POINT('Ctrl Pts',(26.3850466169318,-3.91532959726404,16.3473098014664));
#46937=CARTESIAN_POINT('Ctrl Pts',(26.2461351264432,-5.1855488839429,18.6650714199203));
#46938=CARTESIAN_POINT('Ctrl Pts',(26.1072236359545,-5.19238967348734,21.3080676665743));
#46939=CARTESIAN_POINT('Ctrl Pts',(25.9683121454659,-3.93418531370541,23.6323735296772));
#46940=CARTESIAN_POINT('Ctrl Pts',(25.8294006549773,-1.7174777674106,25.0717079628193));
#46941=CARTESIAN_POINT('Ctrl Pts',(25.6904891644886,0.917666578770842,25.2753994722563));
#46942=CARTESIAN_POINT('Ctrl Pts',(25.551577674,3.32923570676315,24.1938217833485));
#46943=CARTESIAN_POINT('Ctrl Pts',(25.4126661835114,4.92968823013898,22.0904845120939));
#46944=CARTESIAN_POINT('Ctrl Pts',(25.2737546930227,5.32909873329212,19.4778331373023));
#46945=CARTESIAN_POINT('Ctrl Pts',(25.1348432025341,4.43015704665191,16.9923996136994));
#46946=CARTESIAN_POINT('Ctrl Pts',(24.9959317120454,2.45187635908171,15.2397212412033));
#46947=CARTESIAN_POINT('Ctrl Pts',(24.8570202215568,-0.123765946134771,
14.6468109007572));
#46948=CARTESIAN_POINT('Ctrl Pts',(24.7181087310681,-2.6692545996311,15.3581219938452));
#46949=CARTESIAN_POINT('Ctrl Pts',(24.5791972405796,-4.56442080124713,17.2003546133809));
#46950=CARTESIAN_POINT('Ctrl Pts',(24.4402857500909,-5.34753672212527,19.7246773761623));
#46951=CARTESIAN_POINT('Ctrl Pts',(24.3013742596023,-4.82780832341947,22.3160782227716));
#46952=CARTESIAN_POINT('Ctrl Pts',(24.1624627691136,-3.13185936241575,24.3432025598312));
#46953=CARTESIAN_POINT('Ctrl Pts',(24.023551278625,-0.672881479482988,25.3121730069948));
#46954=CARTESIAN_POINT('Ctrl Pts',(23.8846397881364,1.95003353167377,24.9869149548617));
#46955=CARTESIAN_POINT('Ctrl Pts',(23.7457282976477,4.09785314063762,23.4466724792822));
#46956=CARTESIAN_POINT('Ctrl Pts',(23.6068168071591,5.24729443745648,21.0667017522782));
#46957=CARTESIAN_POINT('Ctrl Pts',(23.4679053166704,5.11831389142216,18.4268457003364));
#46958=CARTESIAN_POINT('Ctrl Pts',(23.3289938261818,3.74233561058096,16.1702642755077));
#46959=CARTESIAN_POINT('Ctrl Pts',(23.1900823356931,1.45459534556316,14.8467385160133));
#46960=CARTESIAN_POINT('Ctrl Pts',(23.0511708452045,-1.1875344976354,14.7787249298087));
#46961=CARTESIAN_POINT('Ctrl Pts',(22.9122593547159,-3.54033999301738,15.9827939714875));
#46962=CARTESIAN_POINT('Ctrl Pts',(22.7733478642272,-5.03059660113046,18.1655929082208));
#46963=CARTESIAN_POINT('Ctrl Pts',(22.6344363737386,-5.29522643069642,20.7953166597835));
#46964=CARTESIAN_POINT('Ctrl Pts',(22.49552488325,-4.26975653124141,23.2312738518418));
#46965=CARTESIAN_POINT('Ctrl Pts',(22.3566133927614,-2.20402672675047,24.8799813247024));
#46966=CARTESIAN_POINT('Ctrl Pts',(22.2177019022727,0.398679979512333,25.3397570933153));
#46967=CARTESIAN_POINT('Ctrl Pts',(22.0787904117841,2.90425449695062,24.4985839281508));
#46968=CARTESIAN_POINT('Ctrl Pts',(21.9398789212954,4.70225248512023,22.5614006144795));
#46969=CARTESIAN_POINT('Ctrl Pts',(21.8009674308068,5.35461964215578,20.0001717983347));
#46970=CARTESIAN_POINT('Ctrl Pts',(21.6620559403182,4.70241683608078,17.4389011261923));
#46971=CARTESIAN_POINT('Ctrl Pts',(21.5231444498295,2.9045431573112,15.5016024420921));
#46972=CARTESIAN_POINT('Ctrl Pts',(21.3842329593409,0.399022621656567,14.6602685002819));
#46973=CARTESIAN_POINT('Ctrl Pts',(21.2453214688522,-2.20371358226263,15.1198772567664));
#46974=CARTESIAN_POINT('Ctrl Pts',(21.1064099783636,-4.26954917720392,16.7684521719287));
#46975=CARTESIAN_POINT('Ctrl Pts',(20.967498487875,-5.29517538570201,19.2043435563444));
#46976=CARTESIAN_POINT('Ctrl Pts',(20.8285869973863,-5.03071430149971,21.8340842833308));
#46977=CARTESIAN_POINT('Ctrl Pts',(20.6896755068977,-3.54059776288221,24.0169788427559));
#46978=CARTESIAN_POINT('Ctrl Pts',(20.550764016409,-1.18786953536933,25.2211988574097));
#46979=CARTESIAN_POINT('Ctrl Pts',(20.4118525259204,1.4542646667037,25.1533548122415));
#46980=CARTESIAN_POINT('Ctrl Pts',(20.2729410354318,3.74208985536738,23.8299758558027));
#46981=CARTESIAN_POINT('Ctrl Pts',(20.1340295449431,5.11821293429771,21.5734827297631));
#46982=CARTESIAN_POINT('Ctrl Pts',(19.9951180544545,5.24736287505752,18.9336349597145));
#46983=CARTESIAN_POINT('Ctrl Pts',(19.8562065639659,4.0980742992049,16.5535904799529));
#46984=CARTESIAN_POINT('Ctrl Pts',(19.7172950734773,1.9503535293551,15.0132101856798));
#46985=CARTESIAN_POINT('Ctrl Pts',(19.5783835829886,-0.672540605155714,
14.6877838263027));
#46986=CARTESIAN_POINT('Ctrl Pts',(19.4394720925,-3.13158066018142,15.6565964831191));
#46987=CARTESIAN_POINT('Ctrl Pts',(19.3005606020113,-4.8276596947516,17.6836119898977));
#46988=CARTESIAN_POINT('Ctrl Pts',(19.1616491115227,-5.3475543780918,20.2749794811006));
#46989=CARTESIAN_POINT('Ctrl Pts',(19.0227376210341,-4.56460044024587,22.7993524898773));
#46990=CARTESIAN_POINT('Ctrl Pts',(18.8838261305454,-2.66955245540832,24.6417067151532));
#46991=CARTESIAN_POINT('Ctrl Pts',(18.7449146400568,-0.124109450753522,
25.3531811463754));
#46992=CARTESIAN_POINT('Ctrl Pts',(18.6060031495681,2.45157089518999,24.760436081656));
#46993=CARTESIAN_POINT('Ctrl Pts',(18.4670916590795,4.4299640450231,23.0078846556139));
#46994=CARTESIAN_POINT('Ctrl Pts',(18.3281801685909,5.32906521577738,20.5225088206591));
#46995=CARTESIAN_POINT('Ctrl Pts',(18.1892686781023,4.92982236276058,17.9098318217663));
#46996=CARTESIAN_POINT('Ctrl Pts',(18.0503571876136,3.32950481018978,15.8063918565752));
#46997=CARTESIAN_POINT('Ctrl Pts',(17.911445697125,0.918005090129485,14.7246594236797));
#46998=CARTESIAN_POINT('Ctrl Pts',(17.7725342066363,-1.71715232115819,14.9281818400483));
#46999=CARTESIAN_POINT('Ctrl Pts',(17.6336227161477,-3.93395222248708,16.3673740279429));
#47000=CARTESIAN_POINT('Ctrl Pts',(17.4947112256591,-5.19230572636053,18.6915991494658));
#47001=CARTESIAN_POINT('Ctrl Pts',(17.3557997351705,-5.18563453332208,21.3345958296401));
#47002=CARTESIAN_POINT('Ctrl Pts',(17.2168882446818,-3.91556397600737,23.652438951094));
#47003=CARTESIAN_POINT('Ctrl Pts',(17.0779767541931,-1.69152703207546,25.0804220141079));
#47004=CARTESIAN_POINT('Ctrl Pts',(16.9390652637045,0.94462421787777,25.2706391100771));
#47005=CARTESIAN_POINT('Ctrl Pts',(16.8001537732159,3.35063243930134,24.1767467960574));
#47006=CARTESIAN_POINT('Ctrl Pts',(16.6612422827273,4.9403110743387,22.0652549553122));
#47007=CARTESIAN_POINT('Ctrl Pts',(16.5223307922386,5.3263595980486,19.4505958009346));
#47008=CARTESIAN_POINT('Ctrl Pts',(16.38341930175,4.41472327975128,16.9697904519824));
#47009=CARTESIAN_POINT('Ctrl Pts',(16.2445078112613,2.42750815827123,15.227248625457));
#47010=CARTESIAN_POINT('Ctrl Pts',(16.1055963207727,-0.151131646963111,
14.6475135902124));
#47011=CARTESIAN_POINT('Ctrl Pts',(15.9666848302841,-2.69295057223214,15.3718287891231));
#47012=CARTESIAN_POINT('Ctrl Pts',(15.8277733397954,-4.57867388969788,17.2237260665644));
#47013=CARTESIAN_POINT('Ctrl Pts',(15.6888618493068,-5.34887438265668,19.7520193954475));
#47014=CARTESIAN_POINT('Ctrl Pts',(15.5499503588182,-4.81590465580583,22.3407293495539));
#47015=CARTESIAN_POINT('Ctrl Pts',(15.4110388683295,-3.10961451050615,24.3591569296969));
#47016=CARTESIAN_POINT('Ctrl Pts',(15.2721273778409,-0.645715056167731,
25.3155435853648));
#47017=CARTESIAN_POINT('Ctrl Pts',(15.1332158873523,1.97550284902251,24.9768805526333));
#47018=CARTESIAN_POINT('Ctrl Pts',(14.9943043968636,4.11542014817447,23.4256778228074));
#47019=CARTESIAN_POINT('Ctrl Pts',(14.855392906375,5.25267920646456,21.0398618637348));
#47020=CARTESIAN_POINT('Ctrl Pts',(14.7164814158863,5.11020450651333,18.4006997019677));
#47021=CARTESIAN_POINT('Ctrl Pts',(14.5775699253977,3.72270779751692,16.1511822339864));
#47022=CARTESIAN_POINT('Ctrl Pts',(14.4386584349091,1.42823111634034,14.8393694745707));
#47023=CARTESIAN_POINT('Ctrl Pts',(14.2997469444204,-1.21421190778405,14.7848642410124));
#47024=CARTESIAN_POINT('Ctrl Pts',(14.1608354539318,-3.56083104718738,16.0009458874552));
#47025=CARTESIAN_POINT('Ctrl Pts',(14.0219239634432,-5.03990897202894,18.1913349963752));
#47026=CARTESIAN_POINT('Ctrl Pts',(13.8830124729545,-5.29109130369761,20.8223772599062));
#47027=CARTESIAN_POINT('Ctrl Pts',(13.7441009824659,-4.2531813658544,23.2530600687389));
#47028=CARTESIAN_POINT('Ctrl Pts',(13.6051894919772,-2.17904980474738,24.8911852847859));
#47029=CARTESIAN_POINT('Ctrl Pts',(13.4662780014886,0.425973418769273,25.3376491256149));
#47030=CARTESIAN_POINT('Ctrl Pts',(13.327366511,2.92721483062653,24.4836776062776));
#47031=CARTESIAN_POINT('Ctrl Pts',(13.1884550205113,4.71528578429796,22.5373276323866));
#47032=CARTESIAN_POINT('Ctrl Pts',(13.0495435300227,5.3545505457894,19.9727971644561));
#47033=CARTESIAN_POINT('Ctrl Pts',(12.9106320395341,4.68926217842746,17.414894245172));
#47034=CARTESIAN_POINT('Ctrl Pts',(12.7717205490454,2.8815078665258,15.4868122178637));
#47035=CARTESIAN_POINT('Ctrl Pts',(12.6328090585568,0.371718888792551,14.6582983414094));
#47036=CARTESIAN_POINT('Ctrl Pts',(12.4938975680682,-2.22863362649285,15.1312071618788));
#47037=CARTESIAN_POINT('Ctrl Pts',(12.3549860775795,-4.28601415082467,16.7903217855047));
#47038=CARTESIAN_POINT('Ctrl Pts',(12.2160745870909,-5.29917385345463,19.2314246864894));
#47039=CARTESIAN_POINT('Ctrl Pts',(12.0771630966022,-5.02127209877919,21.8597790330297));
#47040=CARTESIAN_POINT('Ctrl Pts',(11.9382516061136,-3.52001533582255,24.03502708507));
#47041=CARTESIAN_POINT('Ctrl Pts',(11.799340115625,-1.16116147284977,25.2272034182385));
#47042=CARTESIAN_POINT('Ctrl Pts',(11.6604286251363,1.48059135980434,25.1458527735399));
#47043=CARTESIAN_POINT('Ctrl Pts',(11.5215171346477,3.76162108890966,23.8107949728561));
#47044=CARTESIAN_POINT('Ctrl Pts',(11.3826056441591,5.12619022638666,21.5472961269818));
#47045=CARTESIAN_POINT('Ctrl Pts',(11.2436941536704,5.24184268229665,18.9068225964061));
#47046=CARTESIAN_POINT('Ctrl Pts',(11.1047826631818,4.0804015308777,16.5326847722646));
#47047=CARTESIAN_POINT('Ctrl Pts',(10.9658711726932,1.92483388115344,15.0033044847981));
#47048=CARTESIAN_POINT('Ctrl Pts',(10.8269596822045,-0.69968966705539,14.6912915024941));
#47049=CARTESIAN_POINT('Ctrl Pts',(10.6880481917159,-3.15374468824635,15.6726629455249));
#47050=CARTESIAN_POINT('Ctrl Pts',(10.5491367012272,-4.83943876756671,17.708322894331));
#47051=CARTESIAN_POINT('Ctrl Pts',(10.4102252107386,-5.34607870739673,20.3023143992512));
#47052=CARTESIAN_POINT('Ctrl Pts',(10.27131372025,-4.55022955030055,22.8226516932216));
#47053=CARTESIAN_POINT('Ctrl Pts',(10.1324022297614,-2.64578759048757,24.6552937144392));
#47054=CARTESIAN_POINT('Ctrl Pts',(9.99349073927269,-0.096740551324623,
25.3537456801201));
#47055=CARTESIAN_POINT('Ctrl Pts',(9.85457924878407,2.47587582159254,24.7478406099751));
#47056=CARTESIAN_POINT('Ctrl Pts',(9.71566775829542,4.44528348033462,22.9851978696795));
#47057=CARTESIAN_POINT('Ctrl Pts',(9.5767562678068,5.33166681736764,20.4952580037272));
#47058=CARTESIAN_POINT('Ctrl Pts',(9.43784477731815,4.91907229078337,17.8846562124036));
#47059=CARTESIAN_POINT('Ctrl Pts',(9.29893328682952,3.30802215282312,15.7894251012354));
#47060=CARTESIAN_POINT('Ctrl Pts',(9.16002179634088,0.891023763393785,14.7200352089486));
#47061=CARTESIAN_POINT('Ctrl Pts',(9.02111030585224,-1.74305873579932,14.9370267840696));
#47062=CARTESIAN_POINT('Ctrl Pts',(8.8821988153636,-3.95247202921743,16.3875331973942));
#47063=CARTESIAN_POINT('Ctrl Pts',(8.74328732487497,-5.19892686172881,18.7181610756146));
#47064=CARTESIAN_POINT('Ctrl Pts',(8.60437583438634,-5.17874386046697,21.3610891114658));
#47065=CARTESIAN_POINT('Ctrl Pts',(8.46546434389769,-3.89684030041517,23.6724089117002));
#47066=CARTESIAN_POINT('Ctrl Pts',(8.32655285340906,-1.66553208668131,25.0890032825603));
#47067=CARTESIAN_POINT('Ctrl Pts',(8.18764136292043,0.971557168113871,25.2657409935129));
#47068=CARTESIAN_POINT('Ctrl Pts',(8.0487298724318,3.37194159909904,24.1595626445505));
#47069=CARTESIAN_POINT('Ctrl Pts',(7.90981838194316,4.95080479766731,22.0399714206502));
#47070=CARTESIAN_POINT('Ctrl Pts',(7.77090689145451,5.32348125209927,19.423372823895));
#47071=CARTESIAN_POINT('Ctrl Pts',(7.63199540096589,4.39917412883777,16.9472604883745));
#47072=CARTESIAN_POINT('Ctrl Pts',(7.49308391047725,2.40307651166472,15.2149007512111));
#47073=CARTESIAN_POINT('Ctrl Pts',(7.35417241998861,-0.17849339778717,14.6483561732285));
#47074=CARTESIAN_POINT('Ctrl Pts',(7.21526092949998,-2.71657616138589,15.3856565471278));
#47075=CARTESIAN_POINT('Ctrl Pts',(7.07634943901133,-4.59280730909292,17.2471700809498));
#47076=CARTESIAN_POINT('Ctrl Pts',(6.93743794852271,-5.3500722440318,19.7793678959993));
#47077=CARTESIAN_POINT('Ctrl Pts',(6.79852645803405,-4.80387511882975,22.3653192986072));
#47078=CARTESIAN_POINT('Ctrl Pts',(6.65961496754543,-3.08728838514452,24.3749973678423));
#47079=CARTESIAN_POINT('Ctrl Pts',(6.52070347705679,-0.61853175632593,25.3187752357184));
#47080=CARTESIAN_POINT('Ctrl Pts',(6.38179198656815,2.0009205342686,24.9667160737471));
#47081=CARTESIAN_POINT('Ctrl Pts',(6.24288049607952,4.13287959433989,23.4045936321923));
#47082=CARTESIAN_POINT('Ctrl Pts',(6.10396900559087,5.25792669049103,21.0129947971718));
#47083=CARTESIAN_POINT('Ctrl Pts',(5.96505751510225,5.10196156036751,18.3745955032032));
#47084=CARTESIAN_POINT('Ctrl Pts',(5.82614602461359,3.70298268708293,16.1322007858681));
#47085=CARTESIAN_POINT('Ctrl Pts',(5.68723453412498,1.40182955860857,14.8321353123087));
#47086=CARTESIAN_POINT('Ctrl Pts',(5.54832304363632,-1.24085758306887,14.7911398559554));
#47087=CARTESIAN_POINT('Ctrl Pts',(5.40941155314771,-3.58122903482779,16.0192023234305));
#47088=CARTESIAN_POINT('Ctrl Pts',(5.27050006265906,-5.04908961894742,18.2171243561278));
#47089=CARTESIAN_POINT('Ctrl Pts',(5.13158857217043,-5.28681788777155,20.8494163662269));
#47090=CARTESIAN_POINT('Ctrl Pts',(4.9926770816818,-4.23649503854359,23.2747612630649));
#47091=CARTESIAN_POINT('Ctrl Pts',(4.85376559119315,-2.15401593070123,24.9022614079586));
#47092=CARTESIAN_POINT('Ctrl Pts',(4.71485410070452,0.453255724707226,25.3354016521434));
#47093=CARTESIAN_POINT('Ctrl Pts',(4.57594261021588,2.95009865808178,24.4686540981888));
#47094=CARTESIAN_POINT('Ctrl Pts',(4.43703111972724,4.72819584390646,22.5131883342361));
#47095=CARTESIAN_POINT('Ctrl Pts',(4.29811962923862,5.35434150191347,19.9454232415558));
#47096=CARTESIAN_POINT('Ctrl Pts',(4.15920813874997,4.67598496136272,17.3909549289472));
#47097=CARTESIAN_POINT('Ctrl Pts',(4.02029664826134,2.85839726412539,15.4721399511341));
#47098=CARTESIAN_POINT('Ctrl Pts',(3.88138515777269,0.344405440615539,14.6564677942253));
#47099=CARTESIAN_POINT('Ctrl Pts',(3.74247366728406,-2.25349542274803,15.1426643186491));
#47100=CARTESIAN_POINT('Ctrl Pts',(3.60356217679542,-4.30236710439854,16.8122752878152));
#47101=CARTESIAN_POINT('Ctrl Pts',(3.46465068630679,-5.30303382103181,19.25852590426));
#47102=CARTESIAN_POINT('Ctrl Pts',(3.32573919581815,-5.01169865917778,21.885425175202));
#47103=CARTESIAN_POINT('Ctrl Pts',(3.18682770532951,-3.49934090899555,24.0529698671851));
#47104=CARTESIAN_POINT('Ctrl Pts',(3.04791621484087,-1.13442306201116,25.2330713599164));
#47105=CARTESIAN_POINT('Ctrl Pts',(2.90900472435224,1.5068793559172,25.1382162419096));
#47106=CARTESIAN_POINT('Ctrl Pts',(2.77009323386361,3.78105400800197,23.7915144902417));
#47107=CARTESIAN_POINT('Ctrl Pts',(2.63118174337497,5.13403353950245,21.5210690838564));
#47108=CARTESIAN_POINT('Ctrl Pts',(2.49227025288633,5.23618548764273,18.8800388044447));
#47109=CARTESIAN_POINT('Ctrl Pts',(2.3533587623977,4.06262211670135,16.5118696872292));
#47110=CARTESIAN_POINT('Ctrl Pts',(2.21444727190906,1.8992639246118,14.99352937793));
#47111=CARTESIAN_POINT('Ctrl Pts',(2.07553578142043,-0.726820440693177,
14.694937929106));
#47112=CARTESIAN_POINT('Ctrl Pts',(1.93662429093179,-3.17582629152359,15.6888425059388));
#47113=CARTESIAN_POINT('Ctrl Pts',(1.79771280044315,-4.8510913518727,17.7330936985172));
#47114=CARTESIAN_POINT('Ctrl Pts',(1.65880130995451,-5.34446331860061,20.3296414080563));
#47115=CARTESIAN_POINT('Ctrl Pts',(1.51988981946587,-4.53573971899385,22.8458771389863));
#47116=CARTESIAN_POINT('Ctrl Pts',(1.38097832897724,-2.62195360576743,24.6687590110773));
#47117=CARTESIAN_POINT('Ctrl Pts',(1.24206683848861,-0.0693690624308824,
25.3541703485356));
#47118=CARTESIAN_POINT('Ctrl Pts',(1.10315534799997,2.50011591782952,24.7351209274301));
#47119=CARTESIAN_POINT('Ctrl Pts',(0.964243857511331,4.46048696971124,22.9624332992928));
#47120=CARTESIAN_POINT('Ctrl Pts',(0.82533236702269,5.33412860310603,20.467993775381));
#47121=CARTESIAN_POINT('Ctrl Pts',(0.686420876534053,4.90819457177639,17.8595368104176));
#47122=CARTESIAN_POINT('Ctrl Pts',(0.54750938604542,3.28645122673724,15.7725665813991));
#47123=CARTESIAN_POINT('Ctrl Pts',(0.408597895556785,0.864022713178557,
14.7155525631285));
#47124=CARTESIAN_POINT('Ctrl Pts',(0.269686405068149,-1.76892661457066,
14.9459970213854));
#47125=CARTESIAN_POINT('Ctrl Pts',(0.130774914579505,-3.97087470340791,
16.4078006379552));
#47126=CARTESIAN_POINT('Ctrl Pts',(-0.00813657590912362,-5.20543936546245,
18.7447292011997));
#47127=CARTESIAN_POINT('Ctrl Pts',(-0.147048066397761,-5.17166407855605,
21.3876007430961));
#47128=CARTESIAN_POINT('Ctrl Pts',(-0.285959556886395,-3.87812163490998,
23.6921750166713));
#47129=CARTESIAN_POINT('Ctrl Pts',(-0.424871047375028,-1.63927203245633,
25.0976827974512));
#47130=CARTESIAN_POINT('Ctrl Pts',(-0.517478707700787,0.118837970738912,
25.205896478639));
#47131=CARTESIAN_POINT('Ctrl Pts',(-0.563782537863666,0.957839028560417,
25.0466568099948));
#47132=CARTESIAN_POINT('Ctrl Pts',(50.1879275126212,4.1258079218636,23.5796485937013));
#47133=CARTESIAN_POINT('Ctrl Pts',(50.1416236824583,4.72092050229439,22.8937376349937));
#47134=CARTESIAN_POINT('Ctrl Pts',(50.0490160221326,5.56184096807278,21.220063777147));
#47135=CARTESIAN_POINT('Ctrl Pts',(49.9101045316439,5.46761903977869,18.4106716448697));
#47136=CARTESIAN_POINT('Ctrl Pts',(49.7711930411553,4.04148516076094,15.9891741090619));
#47137=CARTESIAN_POINT('Ctrl Pts',(49.6322815506667,1.63061710874887,14.5445190619427));
#47138=CARTESIAN_POINT('Ctrl Pts',(49.4933700601781,-1.17748087672893,14.4291752694788));
#47139=CARTESIAN_POINT('Ctrl Pts',(49.3544585696893,-3.69872652215335,15.6709912525866));
#47140=CARTESIAN_POINT('Ctrl Pts',(49.2155470792008,-5.31882339208546,17.9675462714425));
#47141=CARTESIAN_POINT('Ctrl Pts',(49.076635588712,-5.64307732183502,20.7592551383084));
#47142=CARTESIAN_POINT('Ctrl Pts',(48.9377240982236,-4.59248009632072,23.3659944223523));
#47143=CARTESIAN_POINT('Ctrl Pts',(48.7988126077348,-2.42299787900316,25.1526557522133));
#47144=CARTESIAN_POINT('Ctrl Pts',(48.6599011172463,0.336810924398074,25.6839553589829));
#47145=CARTESIAN_POINT('Ctrl Pts',(48.5209896267575,3.01456058714978,24.8304460084601));
#47146=CARTESIAN_POINT('Ctrl Pts',(48.382078136269,4.95785955026221,22.8000742051481));
#47147=CARTESIAN_POINT('Ctrl Pts',(48.2431666457803,5.69325288857485,20.0875074076531));
#47148=CARTESIAN_POINT('Ctrl Pts',(48.1042551552917,5.04157358005871,17.3536209794161));
#47149=CARTESIAN_POINT('Ctrl Pts',(47.965343664803,3.16159309676431,15.264483626389));
#47150=CARTESIAN_POINT('Ctrl Pts',(47.8264321743145,0.51133954173023,14.329081383812));
#47151=CARTESIAN_POINT('Ctrl Pts',(47.6875206838257,-2.26349396242014,14.7753104148998));
#47152=CARTESIAN_POINT('Ctrl Pts',(47.5486091933372,-4.48686229249669,16.4944539801099));
#47153=CARTESIAN_POINT('Ctrl Pts',(47.4096977028484,-5.61707627036106,19.0676694146596));
#47154=CARTESIAN_POINT('Ctrl Pts',(47.2707862123599,-5.3787768005542,21.8680327282576));
#47155=CARTESIAN_POINT('Ctrl Pts',(47.1318747218712,-3.83002185139275,24.2132788609653));
#47156=CARTESIAN_POINT('Ctrl Pts',(46.9929632313826,-1.34814152629545,25.5320249972138));
#47157=CARTESIAN_POINT('Ctrl Pts',(46.854051740894,1.46219255614692,25.5029791087937));
#47158=CARTESIAN_POINT('Ctrl Pts',(46.7151402504053,3.91628611802883,24.1332177762222));
#47159=CARTESIAN_POINT('Ctrl Pts',(46.5762287599167,5.41623735456965,21.7564620868539));
#47160=CARTESIAN_POINT('Ctrl Pts',(46.437317269428,5.59660642879563,18.9517716733247));
#47161=CARTESIAN_POINT('Ctrl Pts',(46.2984057789394,4.4134492153806,16.4024658212954));
#47162=CARTESIAN_POINT('Ctrl Pts',(46.1594942884507,2.15502360479501,14.729643332142));
#47163=CARTESIAN_POINT('Ctrl Pts',(46.0205827979622,-0.62844005751078,14.3408614403073));
#47164=CARTESIAN_POINT('Ctrl Pts',(45.8816713074735,-3.2587940542495,15.330840819199));
#47165=CARTESIAN_POINT('Ctrl Pts',(45.7427598169849,-5.09519346163427,17.4583883592892));
#47166=CARTESIAN_POINT('Ctrl Pts',(45.6038483264962,-5.69022806806176,20.2051601255532));
#47167=CARTESIAN_POINT('Ctrl Pts',(45.4649368360076,-4.89892692761397,22.9019478116558));
#47168=CARTESIAN_POINT('Ctrl Pts',(45.326025345519,-2.91407828083651,24.8917209565584));
#47169=CARTESIAN_POINT('Ctrl Pts',(45.1871138550302,-0.219259692328256,
25.6897022181302));
#47170=CARTESIAN_POINT('Ctrl Pts',(45.0482023645418,2.52897811693668,25.1014758480003));
#47171=CARTESIAN_POINT('Ctrl Pts',(44.9092908740529,4.66106966200288,23.2703540709886));
#47172=CARTESIAN_POINT('Ctrl Pts',(44.7703793835645,5.6575639315609,20.6424612859748));
#47173=CARTESIAN_POINT('Ctrl Pts',(44.6314678930757,5.27568056409961,17.8580427807128));
#47174=CARTESIAN_POINT('Ctrl Pts',(44.4925564025872,3.60845951462895,15.5954789051522));
#47175=CARTESIAN_POINT('Ctrl Pts',(44.3536449120985,1.0620933137783,14.4060082287777));
#47176=CARTESIAN_POINT('Ctrl Pts',(44.2147334216099,-1.74303543750027,14.5794268193028));
#47177=CARTESIAN_POINT('Ctrl Pts',(44.0758219311212,-4.12350065927285,16.0734839288943));
#47178=CARTESIAN_POINT('Ctrl Pts',(43.9369104406326,-5.49933894907755,18.5241757330787));
#47179=CARTESIAN_POINT('Ctrl Pts',(43.797998950144,-5.53534866292723,21.3344292126242));
#47180=CARTESIAN_POINT('Ctrl Pts',(43.6590874596553,-4.22275659297371,23.8195697270992));
#47181=CARTESIAN_POINT('Ctrl Pts',(43.5201759691667,-1.88135542342509,25.3741313637112));
#47182=CARTESIAN_POINT('Ctrl Pts',(43.381264478678,0.918408793241331,25.6193693091104));
#47183=CARTESIAN_POINT('Ctrl Pts',(43.2423529881894,3.49441696268329,24.4955351444057));
#47184=CARTESIAN_POINT('Ctrl Pts',(43.1034414977008,5.21906467839467,22.2764336200312));
#47185=CARTESIAN_POINT('Ctrl Pts',(42.9645300072122,5.67216829387492,19.5027143782138));
#47186=CARTESIAN_POINT('Ctrl Pts',(42.8256185167235,4.74333614614231,16.8501510594355));
#47187=CARTESIAN_POINT('Ctrl Pts',(42.6867070262348,2.65886377095513,14.9649995440738));
#47188=CARTESIAN_POINT('Ctrl Pts',(42.5477955357463,-0.0733994919886356,
14.3065477381249));
#47189=CARTESIAN_POINT('Ctrl Pts',(42.4088840452575,-2.78778010799291,15.0352172038291));
#47190=CARTESIAN_POINT('Ctrl Pts',(42.269972554769,-4.82296137171968,16.9734789360431));
#47191=CARTESIAN_POINT('Ctrl Pts',(42.1310610642803,-5.68310295769733,19.649105548794));
#47192=CARTESIAN_POINT('Ctrl Pts',(41.9921495737917,-5.15864471934614,22.4102221481095));
#47193=CARTESIAN_POINT('Ctrl Pts',(41.8532380833031,-3.37736276596667,24.5841255317385));
#47194=CARTESIAN_POINT('Ctrl Pts',(41.7143265928144,-0.773238797008643,
25.6411778828961));
#47195=CARTESIAN_POINT('Ctrl Pts',(41.5754151023258,2.01927280287421,25.3238448034525));
#47196=CARTESIAN_POINT('Ctrl Pts',(41.4365036118371,4.3198199268461,23.7094395726711));
#47197=CARTESIAN_POINT('Ctrl Pts',(41.2975921213485,5.56790997651105,21.1912869667481));
#47198=CARTESIAN_POINT('Ctrl Pts',(41.1586806308598,5.45946518372445,18.3828957821538));
#47199=CARTESIAN_POINT('Ctrl Pts',(41.0197691403712,4.0209064390032,15.9684869400611));
#47200=CARTESIAN_POINT('Ctrl Pts',(40.8808576498826,1.60271625164799,14.5362936791607));
#47201=CARTESIAN_POINT('Ctrl Pts',(40.7419461593939,-1.20595087357003,14.4352476574235));
#47202=CARTESIAN_POINT('Ctrl Pts',(40.6030346689053,-3.72080678682811,15.6899671696414));
#47203=CARTESIAN_POINT('Ctrl Pts',(40.4641231784166,-5.32914587965345,17.9947592820193));
#47204=CARTESIAN_POINT('Ctrl Pts',(40.325211687928,-5.63912129620631,20.7880971706253));
#47205=CARTESIAN_POINT('Ctrl Pts',(40.1863001974394,-4.57521233758331,23.3894274162019));
#47206=CARTESIAN_POINT('Ctrl Pts',(40.0473887069508,-2.3966239078969,25.1649762814336));
#47207=CARTESIAN_POINT('Ctrl Pts',(39.9084772164621,0.365864737315575,25.6821588448111));
#47208=CARTESIAN_POINT('Ctrl Pts',(39.7695657259735,3.03921611811703,24.8149716023101));
#47209=CARTESIAN_POINT('Ctrl Pts',(39.6306542354848,4.97210966548392,22.7746912653621));
#47210=CARTESIAN_POINT('Ctrl Pts',(39.4917427449962,5.69362586835836,20.0584004694827));
#47211=CARTESIAN_POINT('Ctrl Pts',(39.3528312545076,5.02797850305467,17.3278813056873));
#47212=CARTESIAN_POINT('Ctrl Pts',(39.2139197640189,3.13734221816271,15.2483823859859));
#47213=CARTESIAN_POINT('Ctrl Pts',(39.0750082735303,0.482341198642141,14.3265413448437));
#47214=CARTESIAN_POINT('Ctrl Pts',(38.9360967830416,-2.29017476718114,14.786950443412));
#47215=CARTESIAN_POINT('Ctrl Pts',(38.7971852925531,-4.50472519834409,16.5174381511481));
#47216=CARTESIAN_POINT('Ctrl Pts',(38.6582738020644,-5.62176925584033,19.096397998141));
#47217=CARTESIAN_POINT('Ctrl Pts',(38.5193623115758,-5.36915649346304,21.8955064474643));
#47218=CARTESIAN_POINT('Ctrl Pts',(38.3804508210871,-3.80843208979058,24.2328041723104));
#47219=CARTESIAN_POINT('Ctrl Pts',(38.2415393305985,-1.31984232071061,25.5388448608114));
#47220=CARTESIAN_POINT('Ctrl Pts',(38.1026278401098,1.49030654363833,25.4954319711615));
#47221=CARTESIAN_POINT('Ctrl Pts',(37.9637163496212,3.93736535069332,24.113142380083));
#47222=CARTESIAN_POINT('Ctrl Pts',(37.8248048591326,5.42514620458289,21.7287494909833));
#47223=CARTESIAN_POINT('Ctrl Pts',(37.6858933686439,5.59117439311739,18.9231736215046));
#47224=CARTESIAN_POINT('Ctrl Pts',(37.5469818781553,4.39499972519705,16.3799497849901));
#47225=CARTESIAN_POINT('Ctrl Pts',(37.4080703876667,2.12805159201845,14.7186949940963));
#47226=CARTESIAN_POINT('Ctrl Pts',(37.269158897178,-0.657363280616373,14.3441481931567));
#47227=CARTESIAN_POINT('Ctrl Pts',(37.1302474066894,-3.2826217933125,15.347561896624));
#47228=CARTESIAN_POINT('Ctrl Pts',(36.9913359162008,-5.10812045787807,17.4844699303163));
#47229=CARTESIAN_POINT('Ctrl Pts',(36.8524244257121,-5.68910485950053,20.2342478202305));
#47230=CARTESIAN_POINT('Ctrl Pts',(36.7135129352235,-4.88402716657942,22.9269548646656));
#47231=CARTESIAN_POINT('Ctrl Pts',(36.5746014447348,-2.88903206283546,24.9065547875861));
#47232=CARTESIAN_POINT('Ctrl Pts',(36.4356899542462,-0.190169139617183,
25.690748794492));
#47233=CARTESIAN_POINT('Ctrl Pts',(36.2967784637576,2.55502554272399,25.0884801876104));
#47234=CARTESIAN_POINT('Ctrl Pts',(36.1578669732689,4.6777279098732,23.2464823647863));
#47235=CARTESIAN_POINT('Ctrl Pts',(36.0189554827803,5.66077447798464,20.6135295046474));
#47236=CARTESIAN_POINT('Ctrl Pts',(35.8800439922917,5.26466120927372,17.8310997037107));
#47237=CARTESIAN_POINT('Ctrl Pts',(35.741132501803,3.58589495331782,15.5770887949852));
#47238=CARTESIAN_POINT('Ctrl Pts',(35.6022210113144,1.03348105110547,14.4006515503426));
#47239=CARTESIAN_POINT('Ctrl Pts',(35.4633095208258,-1.77072446784502,14.5884086441555));
#47240=CARTESIAN_POINT('Ctrl Pts',(35.3243980303371,-4.14352045482631,16.0946159748226));
#47241=CARTESIAN_POINT('Ctrl Pts',(35.1854865398485,-5.50681199739401,18.552309505097));
#47242=CARTESIAN_POINT('Ctrl Pts',(35.0465750493599,-5.52845427177867,21.3627103538637));
#47243=CARTESIAN_POINT('Ctrl Pts',(34.9076635588712,-4.20317447375095,23.8411079764677));
#47244=CARTESIAN_POINT('Ctrl Pts',(34.7687520683826,-1.85385645552935,25.38367926106));
#47245=CARTESIAN_POINT('Ctrl Pts',(34.6298405778939,0.947124913112505,25.6146006574499));
#47246=CARTESIAN_POINT('Ctrl Pts',(34.4909290874053,3.51735399764575,24.4776117516954));
#47247=CARTESIAN_POINT('Ctrl Pts',(34.3520175969167,5.23063437590115,22.2497222427039));
#47248=CARTESIAN_POINT('Ctrl Pts',(34.213106106428,5.66955187670913,19.4737228287497));
#47249=CARTESIAN_POINT('Ctrl Pts',(34.0741946159394,4.72717106373549,16.825942678864));
#47250=CARTESIAN_POINT('Ctrl Pts',(33.9352831254507,2.63308839472643,14.9514723285663));
#47251=CARTESIAN_POINT('Ctrl Pts',(33.7963716349621,-0.102505391698266,
14.3069973837747));
#47252=CARTESIAN_POINT('Ctrl Pts',(33.6574601444735,-2.81312533049172,15.049534161453));
#47253=CARTESIAN_POINT('Ctrl Pts',(33.5185486539848,-4.83837094694631,16.9981751011391));
#47254=CARTESIAN_POINT('Ctrl Pts',(33.3796371634962,-5.68482258183033,19.6781640840627));
#47255=CARTESIAN_POINT('Ctrl Pts',(33.2407256730075,-5.14625543265696,22.4365633924698));
#47256=CARTESIAN_POINT('Ctrl Pts',(33.101814182519,-3.35388302585458,24.6013318498626));
#47257=CARTESIAN_POINT('Ctrl Pts',(32.9629026920303,-0.744389077706911,
25.6450572224439));
#47258=CARTESIAN_POINT('Ctrl Pts',(32.8239912015417,2.04646371505388,25.3134520235571));
#47259=CARTESIAN_POINT('Ctrl Pts',(32.685079711053,4.33872738819982,23.6873067128407));
#47260=CARTESIAN_POINT('Ctrl Pts',(32.5461682205644,5.57392747755557,21.1628063547411));
#47261=CARTESIAN_POINT('Ctrl Pts',(32.4072567300757,5.451126653732,18.3550062770187));
#47262=CARTESIAN_POINT('Ctrl Pts',(32.2683452395871,4.00024343137845,15.9479833868321));
#47263=CARTESIAN_POINT('Ctrl Pts',(32.1294337490985,1.57476298747406,14.5281714503324));
#47264=CARTESIAN_POINT('Ctrl Pts',(31.9905222586099,-1.23438401535882,14.4414856079792));
#47265=CARTESIAN_POINT('Ctrl Pts',(31.8516107681212,-3.74279251256509,15.7090455197518));
#47266=CARTESIAN_POINT('Ctrl Pts',(31.7126992776326,-5.33932770851822,18.022029887808));
#47267=CARTESIAN_POINT('Ctrl Pts',(31.5737877871439,-5.6350185836351,20.8169159722777));
#47268=CARTESIAN_POINT('Ctrl Pts',(31.4348762966553,-4.55782464581307,23.4127731600114));
#47269=CARTESIAN_POINT('Ctrl Pts',(31.2959648061666,-2.37018747814123,25.1771611392864));
#47270=CARTESIAN_POINT('Ctrl Pts',(31.157053315678,0.394909079284509,25.6802141652207));
#47271=CARTESIAN_POINT('Ctrl Pts',(31.0181418251894,3.06379216919554,24.7993711762741));
#47272=CARTESIAN_POINT('Ctrl Pts',(30.8792303347008,4.98622985228839,22.7492358945393));
#47273=CARTESIAN_POINT('Ctrl Pts',(30.7403188442121,5.6938500265429,20.0292919598639));
#47274=CARTESIAN_POINT('Ctrl Pts',(30.6014073537235,5.01425201995693,17.3022114938281));
#47275=CARTESIAN_POINT('Ctrl Pts',(30.4624958632348,3.11300933833137,15.2324053231072));
#47276=CARTESIAN_POINT('Ctrl Pts',(30.3235843727462,0.453330250560852,14.3241495943249));
#47277=CARTESIAN_POINT('Ctrl Pts',(30.1846728822575,-2.31679571631103,14.7987267181431));
#47278=CARTESIAN_POINT('Ctrl Pts',(30.045761391769,-4.52247036746897,16.5405133445784));
#47279=CARTESIAN_POINT('Ctrl Pts',(29.9068499012803,-5.62631530993781,19.125150197557));
#47280=CARTESIAN_POINT('Ctrl Pts',(29.7679384107917,-5.35939585701468,21.9229306257609));
#47281=CARTESIAN_POINT('Ctrl Pts',(29.629026920303,-3.78674279036552,24.2522188541149));
#47282=CARTESIAN_POINT('Ctrl Pts',(29.4901154298144,-1.29150861945937,25.5455199602506));
#47283=CARTESIAN_POINT('Ctrl Pts',(29.3512039393258,1.51838158019258,25.4877412038659));
#47284=CARTESIAN_POINT('Ctrl Pts',(29.2122924488371,3.95834167566592,24.0929594821304));
#47285=CARTESIAN_POINT('Ctrl Pts',(29.0733809583485,5.43391326198207,21.7009917121875));
#47286=CARTESIAN_POINT('Ctrl Pts',(28.9344694678598,5.58559622548734,18.8946037138217));
#47287=CARTESIAN_POINT('Ctrl Pts',(28.7955579773712,4.37643536649829,16.3575283629741));
#47288=CARTESIAN_POINT('Ctrl Pts',(28.6566464868826,2.10102396009786,14.7078846892032));
#47289=CARTESIAN_POINT('Ctrl Pts',(28.5177349963939,-0.686269322755631,
14.3475827683796));
#47290=CARTESIAN_POINT('Ctrl Pts',(28.3788235059053,-3.3063637371736,15.3644045710202));
#47291=CARTESIAN_POINT('Ctrl Pts',(28.2399120154166,-5.12091394735409,17.5106172476958));
#47292=CARTESIAN_POINT('Ctrl Pts',(28.101000524928,-5.68783295945715,20.2633293925641));
#47293=CARTESIAN_POINT('Ctrl Pts',(27.9620890344394,-4.86899975572019,22.9518854182492));
#47294=CARTESIAN_POINT('Ctrl Pts',(27.8231775439507,-2.86391033656552,24.9212603800031));
#47295=CARTESIAN_POINT('Ctrl Pts',(27.6842660534621,-0.161073616610791,
25.6916466364056));
#47296=CARTESIAN_POINT('Ctrl Pts',(27.5453545629735,2.58100618989778,25.0753515337742));
#47297=CARTESIAN_POINT('Ctrl Pts',(27.4064430724848,4.69426389979383,23.2225258079289));
#47298=CARTESIAN_POINT('Ctrl Pts',(27.2675315819962,5.66383707337432,20.5845816880009));
#47299=CARTESIAN_POINT('Ctrl Pts',(27.1286200915076,5.25350425630234,17.8042133134823));
#47300=CARTESIAN_POINT('Ctrl Pts',(26.9897086010189,3.56323667040224,15.5588142828321));
#47301=CARTESIAN_POINT('Ctrl Pts',(26.8507971105303,1.00484177718341,14.3954412174996));
#47302=CARTESIAN_POINT('Ctrl Pts',(26.7118856200417,-1.79836721821213,14.5975319073469));
#47303=CARTESIAN_POINT('Ctrl Pts',(26.572974129553,-4.16343195457351,16.1158500925799));
#47304=CARTESIAN_POINT('Ctrl Pts',(26.4340626390644,-5.51414111866785,18.580481114218));
#47305=CARTESIAN_POINT('Ctrl Pts',(26.2951511485758,-5.52141538794106,21.3909558790569));
#47306=CARTESIAN_POINT('Ctrl Pts',(26.1562396580872,-4.18348249959358,23.8625458339377));
#47307=CARTESIAN_POINT('Ctrl Pts',(26.0173281675984,-1.82630903490311,25.3930864495858));
#47308=CARTESIAN_POINT('Ctrl Pts',(25.8784166771098,0.975816278754277,25.6096852615627));
#47309=CARTESIAN_POINT('Ctrl Pts',(25.7395051866212,3.54019910240269,24.4595713313078));
#47310=CARTESIAN_POINT('Ctrl Pts',(25.6005936961325,5.24206736459369,22.2229520662257));
#47311=CARTESIAN_POINT('Ctrl Pts',(25.4616822056439,5.66678727910155,19.4447450341616));
#47312=CARTESIAN_POINT('Ctrl Pts',(25.3227707151553,4.71088243112365,16.8018172560334));
#47313=CARTESIAN_POINT('Ctrl Pts',(25.1838592246667,2.60724419961922,14.9380770622986));
#47314=CARTESIAN_POINT('Ctrl Pts',(25.044947734178,-0.131608612308295,14.3075958227792));
#47315=CARTESIAN_POINT('Ctrl Pts',(24.9060362436894,-2.83839702863386,15.0639805053548));
#47316=CARTESIAN_POINT('Ctrl Pts',(24.7671247532008,-4.85365406562751,17.0229497224782));
#47317=CARTESIAN_POINT('Ctrl Pts',(24.6282132627121,-5.68639362640362,19.7072310308935));
#47318=CARTESIAN_POINT('Ctrl Pts',(24.4893017722235,-5.13373164249729,22.4628409543649));
#47319=CARTESIAN_POINT('Ctrl Pts',(24.3503902817348,-3.33031562804408,24.6184179067382));
#47320=CARTESIAN_POINT('Ctrl Pts',(24.2114787912462,-0.715519902916424,
25.6487890217467));
#47321=CARTESIAN_POINT('Ctrl Pts',(24.0725673007576,2.07360114048475,25.3029203703106));
#47322=CARTESIAN_POINT('Ctrl Pts',(23.9336558102689,4.3575214517833,23.6650774808896));
#47323=CARTESIAN_POINT('Ctrl Pts',(23.7947443197803,5.57979929741503,21.1342953514151));
#47324=CARTESIAN_POINT('Ctrl Pts',(23.6558328292917,5.44264565209923,18.3271597657396));
#47325=CARTESIAN_POINT('Ctrl Pts',(23.516921338803,3.97947587266186,15.9275857378482));
#47326=CARTESIAN_POINT('Ctrl Pts',(23.3780098483144,1.54676856500752,14.520192234213));
#47327=CARTESIAN_POINT('Ctrl Pts',(23.2390983578257,-1.26278489506185,14.4478688368808));
#47328=CARTESIAN_POINT('Ctrl Pts',(23.1001868673371,-3.76468041599438,15.7282360190311));
#47329=CARTESIAN_POINT('Ctrl Pts',(22.9612753768485,-5.34936998774029,18.0493521901843));
#47330=CARTESIAN_POINT('Ctrl Pts',(22.8223638863598,-5.63076859319054,20.8457134228651));
#47331=CARTESIAN_POINT('Ctrl Pts',(22.6834523958712,-4.54031782990674,23.4360297069592));
#47332=CARTESIAN_POINT('Ctrl Pts',(22.5445409053826,-2.34368910073348,25.1892106859115));
#47333=CARTESIAN_POINT('Ctrl Pts',(22.4056294148939,0.423943099837686,25.6781210265171));
#47334=CARTESIAN_POINT('Ctrl Pts',(22.2667179244053,3.08828814444319,24.7836453129979));
#47335=CARTESIAN_POINT('Ctrl Pts',(22.1278064339167,5.0002197180801,22.7237086691859));
#47336=CARTESIAN_POINT('Ctrl Pts',(21.988894943428,5.69392536922479,20.0001826846651));
#47337=CARTESIAN_POINT('Ctrl Pts',(21.8499834529394,5.00039448345398,17.2766121918614));
#47338=CARTESIAN_POINT('Ctrl Pts',(21.7110719624507,3.08859509632026,15.2165528669524));
#47339=CARTESIAN_POINT('Ctrl Pts',(21.5721604719621,0.424307454157508,14.3219061888675));
#47340=CARTESIAN_POINT('Ctrl Pts',(21.4332489814735,-2.34335611324554,14.8106389343013));
#47341=CARTESIAN_POINT('Ctrl Pts',(21.2943374909848,-4.54009733648359,16.5636789557828));
#47342=CARTESIAN_POINT('Ctrl Pts',(21.1554260004962,-5.63071431363232,19.1539252622071));
#47343=CARTESIAN_POINT('Ctrl Pts',(21.0165145100076,-5.3494951464188,21.9503045459919));
#47344=CARTESIAN_POINT('Ctrl Pts',(20.8776030195189,-3.76495451994031,24.2715223991519));
#47345=CARTESIAN_POINT('Ctrl Pts',(20.7386915290303,-1.26314116310334,25.5520501209687));
#47346=CARTESIAN_POINT('Ctrl Pts',(20.5997800385416,1.54641693204892,25.4799070079654));
#47347=CARTESIAN_POINT('Ctrl Pts',(20.460868548053,3.97921454469859,24.0726696098425));
#47348=CARTESIAN_POINT('Ctrl Pts',(20.3219570575644,5.44253829763327,21.6731894759621));
#47349=CARTESIAN_POINT('Ctrl Pts',(20.1830455670758,5.57987207169572,18.8660626969777));
#47350=CARTESIAN_POINT('Ctrl Pts',(20.0441340765871,4.35775662448668,16.335202141261));
#47351=CARTESIAN_POINT('Ctrl Pts',(19.9052225860985,2.07394141543192,14.6972127000009));
#47352=CARTESIAN_POINT('Ctrl Pts',(19.7663110956099,-0.715157428434673,
14.35116507621));
#47353=CARTESIAN_POINT('Ctrl Pts',(19.6273996051212,-3.33001926530899,15.3813684021838));
#47354=CARTESIAN_POINT('Ctrl Pts',(19.4884881146326,-5.13357359568929,17.5368296280369));
#47355=CARTESIAN_POINT('Ctrl Pts',(19.3495766241439,-5.68641240117427,20.2924040824727));
#47356=CARTESIAN_POINT('Ctrl Pts',(19.2106651336553,-4.85384508779539,22.9767388208171));
#47357=CARTESIAN_POINT('Ctrl Pts',(19.0717536431667,-2.83871375861276,24.9358373494614));
#47358=CARTESIAN_POINT('Ctrl Pts',(18.932842152678,-0.131973883754986,25.6923957204047));
#47359=CARTESIAN_POINT('Ctrl Pts',(18.7939306621894,2.60691937942308,25.0620902296248));
#47360=CARTESIAN_POINT('Ctrl Pts',(18.6550191717008,4.71067719957706,23.1984850265493));
#47361=CARTESIAN_POINT('Ctrl Pts',(18.5161076812121,5.66675163768531,20.5556185926209));
#47362=CARTESIAN_POINT('Ctrl Pts',(18.3771961907235,5.24220999678571,17.7773843127353));
#47363=CARTESIAN_POINT('Ctrl Pts',(18.2382847002348,3.54048525808325,15.5406558463188));
#47364=CARTESIAN_POINT('Ctrl Pts',(18.0993732097462,0.97617624053337,14.3903773664271));
#47365=CARTESIAN_POINT('Ctrl Pts',(17.9604617192575,-1.82596296612573,14.6067963704295));
#47366=CARTESIAN_POINT('Ctrl Pts',(17.821550228769,-4.18323463810387,16.1371857271876));
#47367=CARTESIAN_POINT('Ctrl Pts',(17.6826387382803,-5.52132612134381,18.6086898241436));
#47368=CARTESIAN_POINT('Ctrl Pts',(17.5437272477917,-5.51423219538396,21.4191650499735));
#47369=CARTESIAN_POINT('Ctrl Pts',(17.404815757303,-4.16368118517472,23.8838827392053));
#47370=CARTESIAN_POINT('Ctrl Pts',(17.2659042668144,-1.79871388153097,25.4023526834207));
#47371=CARTESIAN_POINT('Ctrl Pts',(17.1269927763257,1.00448214028381,25.6046232499185));
#47372=CARTESIAN_POINT('Ctrl Pts',(16.9880812858371,3.5629516798703,24.4414143547506));
#47373=CARTESIAN_POINT('Ctrl Pts',(16.8491697953485,5.25336334565759,22.1961237902669));
#47374=CARTESIAN_POINT('Ctrl Pts',(16.7102583048598,5.66387457330821,19.4157817518188));
#47375=CARTESIAN_POINT('Ctrl Pts',(16.5713468143712,4.69447067402958,16.7777754214904));
#47376=CARTESIAN_POINT('Ctrl Pts',(16.4324353238826,2.58133186110226,14.9248140953721));
#47377=CARTESIAN_POINT('Ctrl Pts',(16.2935238333939,-0.160708393171607,
14.3083430394972));
#47378=CARTESIAN_POINT('Ctrl Pts',(16.1546123429053,-2.86359454191366,15.0785558579623));
#47379=CARTESIAN_POINT('Ctrl Pts',(16.0157008524166,-4.86881032832087,17.0478021525462));
#47380=CARTESIAN_POINT('Ctrl Pts',(15.876789361928,-5.68781605035605,19.7363056295874));
#47381=CARTESIAN_POINT('Ctrl Pts',(15.7378778714394,-5.12107367619125,22.4890541469997));
#47382=CARTESIAN_POINT('Ctrl Pts',(15.5989663809508,-3.30666118849705,24.6353832558012));
#47383=CARTESIAN_POINT('Ctrl Pts',(15.4600548904621,-0.686632027167408,
25.6523731832694));
#47384=CARTESIAN_POINT('Ctrl Pts',(15.3211433999735,2.10068436989794,25.2922501189704));
#47385=CARTESIAN_POINT('Ctrl Pts',(15.1822319094848,4.3762016263914,23.642752457805));
#47386=CARTESIAN_POINT('Ctrl Pts',(15.0433204189962,5.58552528262248,21.105754701939));
#47387=CARTESIAN_POINT('Ctrl Pts',(14.9044089285076,5.43402240048716,18.2993569761178));
#47388=CARTESIAN_POINT('Ctrl Pts',(14.7654974380189,3.95860430563815,15.9072945262262));
#47389=CARTESIAN_POINT('Ctrl Pts',(14.6265859475303,1.51873371591571,14.5123562393486));
#47390=CARTESIAN_POINT('Ctrl Pts',(14.4876744570417,-1.29115277038856,14.454397177295));
#47391=CARTESIAN_POINT('Ctrl Pts',(14.348762966553,-3.78646992504974,15.7475381659127));
#47392=CARTESIAN_POINT('Ctrl Pts',(14.2098514760644,-5.3592724548528,18.0767254750475));
#47393=CARTESIAN_POINT('Ctrl Pts',(14.0709399855757,-5.62637143595118,20.8744887697324));
#47394=CARTESIAN_POINT('Ctrl Pts',(13.9320284950871,-4.52269234742555,23.459196449208));
#47395=CARTESIAN_POINT('Ctrl Pts',(13.7931170045985,-2.31712946823991,25.2011246063798));
#47396=CARTESIAN_POINT('Ctrl Pts',(13.6542055141098,0.452966040136749,25.6758794834068));
#47397=CARTESIAN_POINT('Ctrl Pts',(13.5152940236212,3.11270340362871,24.7677944234954));
#47398=CARTESIAN_POINT('Ctrl Pts',(13.3763825331326,5.01407889721741,22.6981102564859));
#47399=CARTESIAN_POINT('Ctrl Pts',(13.2374710426439,5.69385189443484,19.9710734046917));
#47400=CARTESIAN_POINT('Ctrl Pts',(13.0985595521553,4.9864062557289,17.251084068855));
#47401=CARTESIAN_POINT('Ctrl Pts',(12.9596480616667,3.06410013022447,15.2008254318442));
#47402=CARTESIAN_POINT('Ctrl Pts',(12.820736571178,0.395273567977247,14.3198111871053));
#47403=CARTESIAN_POINT('Ctrl Pts',(12.6818250806894,-2.36985526379726,14.8226867805465));
#47404=CARTESIAN_POINT('Ctrl Pts',(12.5429135902007,-4.55760564468624,16.5869343793007));
#47405=CARTESIAN_POINT('Ctrl Pts',(12.4040020997121,-5.63496615195067,19.1827224400208));
#47406=CARTESIAN_POINT('Ctrl Pts',(12.2650906092235,-5.33945462044222,21.9776274927077));
#47407=CARTESIAN_POINT('Ctrl Pts',(12.1261791187348,-3.74306784797717,24.2907143029005));
#47408=CARTESIAN_POINT('Ctrl Pts',(11.9872676282462,-1.23474069305955,25.5584351722925));
#47409=CARTESIAN_POINT('Ctrl Pts',(11.8483561377576,1.57441186647029,25.4719295882159));
#47410=CARTESIAN_POINT('Ctrl Pts',(11.7094446472689,3.9999834122542,24.0522732935189));
#47411=CARTESIAN_POINT('Ctrl Pts',(11.5705331567803,5.45102108611097,21.6453435089515));
#47412=CARTESIAN_POINT('Ctrl Pts',(11.4316216662917,5.57400208135005,18.8375513169259));
#47413=CARTESIAN_POINT('Ctrl Pts',(11.292710175803,4.33896398735324,16.3129717033732));
#47414=CARTESIAN_POINT('Ctrl Pts',(11.1537986853144,2.04680466585494,14.6866793054146));
#47415=CARTESIAN_POINT('Ctrl Pts',(11.0148871948257,-0.744026842628766,
14.3548950230201));
#47416=CARTESIAN_POINT('Ctrl Pts',(10.8759757043371,-3.35358775945367,15.3984529467452));
#47417=CARTESIAN_POINT('Ctrl Pts',(10.7370642138485,-5.14609907200881,17.563106386248));
#47418=CARTESIAN_POINT('Ctrl Pts',(10.5981527233598,-5.68484322177988,20.3214711300549));
#47419=CARTESIAN_POINT('Ctrl Pts',(10.4592412328712,-4.83856355889019,23.0015144227965));
#47420=CARTESIAN_POINT('Ctrl Pts',(10.3203297423826,-2.81344298751949,24.9502853149745));
#47421=CARTESIAN_POINT('Ctrl Pts',(10.1814182518939,-0.10287070160567,25.6929960269112));
#47422=CARTESIAN_POINT('Ctrl Pts',(10.0425067614053,2.6327644340281,25.0486966217621));
#47423=CARTESIAN_POINT('Ctrl Pts',(9.90359527091664,4.72696738024193,23.1743606489817));
#47424=CARTESIAN_POINT('Ctrl Pts',(9.76468378042803,5.66951809474209,20.526640975492));
#47425=CARTESIAN_POINT('Ctrl Pts',(9.62577228993937,5.23077872591258,17.7506134026771));
#47426=CARTESIAN_POINT('Ctrl Pts',(9.48686079945075,3.51764131099587,15.5226139600376));
#47427=CARTESIAN_POINT('Ctrl Pts',(9.3479493089621,0.947485190363111,14.3854601294747));
#47428=CARTESIAN_POINT('Ctrl Pts',(9.20903781847346,-1.85351099033822,14.6162017912657));
#47429=CARTESIAN_POINT('Ctrl Pts',(9.07012632798483,-4.20292798785086,16.1586223210136));
#47430=CARTESIAN_POINT('Ctrl Pts',(8.93121483749619,-5.52836681763337,18.6369348976056));
#47431=CARTESIAN_POINT('Ctrl Pts',(8.79230334700757,-5.50690488184858,21.4473371293336));
#47432=CARTESIAN_POINT('Ctrl Pts',(8.6533918565189,-4.14377104802507,23.9051181346055));
#47433=CARTESIAN_POINT('Ctrl Pts',(8.51448036603029,-1.77107171664475,25.4114777203806));
#47434=CARTESIAN_POINT('Ctrl Pts',(8.37556887554165,1.03312174848493,25.5994147548189));
#47435=CARTESIAN_POINT('Ctrl Pts',(8.23665738505302,3.58561113538302,24.4231412965778));
#47436=CARTESIAN_POINT('Ctrl Pts',(8.09774589456438,5.2645220238591,22.1692381160162));
#47437=CARTESIAN_POINT('Ctrl Pts',(7.95883440407574,5.66081383545613,19.3868337387104));
#47438=CARTESIAN_POINT('Ctrl Pts',(7.8199229135871,4.6779362213937,16.7538178035964));
#47439=CARTESIAN_POINT('Ctrl Pts',(7.68101142309847,2.55535205642491,14.9116837744299));
#47440=CARTESIAN_POINT('Ctrl Pts',(7.54209993260983,-0.189803973731052,
14.3092390143996));
#47441=CARTESIAN_POINT('Ctrl Pts',(7.40318844212119,-2.88871721176426,15.0932598383313));
#47442=CARTESIAN_POINT('Ctrl Pts',(7.26427695163256,-4.88383933889966,17.0727317417955));
#47443=CARTESIAN_POINT('Ctrl Pts',(7.12536546114392,-5.68908981651096,19.7653871202457));
#47444=CARTESIAN_POINT('Ctrl Pts',(6.98645397065528,-5.10828186456958,22.5152022852615));
#47445=CARTESIAN_POINT('Ctrl Pts',(6.84754248016665,-3.28292032545007,24.6522274536422));
#47446=CARTESIAN_POINT('Ctrl Pts',(6.70863098967801,-0.657726205478431,
25.6558096133358));
#47447=CARTESIAN_POINT('Ctrl Pts',(6.56971949918938,2.12771269544141,25.2814415484158));
#47448=CARTESIAN_POINT('Ctrl Pts',(6.43080800870074,4.39476742379579,23.6203322270779));
#47449=CARTESIAN_POINT('Ctrl Pts',(6.29189651821209,5.5911052835226,21.0771851522562));
#47450=CARTESIAN_POINT('Ctrl Pts',(6.15298502772346,5.42525712427457,18.2715986348122));
#47451=CARTESIAN_POINT('Ctrl Pts',(6.01407353723483,3.93762927581034,15.8871102823007));
#47452=CARTESIAN_POINT('Ctrl Pts',(5.87516204674619,1.4906591729225,14.5046636705423));
#47453=CARTESIAN_POINT('Ctrl Pts',(5.73625055625756,-1.31948689991102,14.4610704585959));
#47454=CARTESIAN_POINT('Ctrl Pts',(5.59733906576892,-3.80816047023665,15.7669514559124));
#47455=CARTESIAN_POINT('Ctrl Pts',(5.45842757528029,-5.36903485104308,18.1041490269644));
#47456=CARTESIAN_POINT('Ctrl Pts',(5.31951608479166,-5.6218272268419,20.9032412608016));
#47457=CARTESIAN_POINT('Ctrl Pts',(5.18060459430301,-4.50494865903241,23.4822727812676));
#47458=CARTESIAN_POINT('Ctrl Pts',(5.04169310381438,-2.29050927482802,25.2129025893069));
#47459=CARTESIAN_POINT('Ctrl Pts',(4.90278161332574,0.481977141632756,25.6734895944752));
#47460=CARTESIAN_POINT('Ctrl Pts',(4.7638701228371,3.1370373086304,24.7518189220483));
#47461=CARTESIAN_POINT('Ctrl Pts',(4.62495863234846,5.0278070274742,22.6724413254842));
#47462=CARTESIAN_POINT('Ctrl Pts',(4.48604714185984,5.69362960409341,19.9419648807492));
#47463=CARTESIAN_POINT('Ctrl Pts',(4.34713565137119,4.97228770238059,17.2256277920167));
#47464=CARTESIAN_POINT('Ctrl Pts',(4.20822416088256,3.03952508024898,15.1852234288378));
#47465=CARTESIAN_POINT('Ctrl Pts',(4.06931267039391,0.366229350854573,14.3178646437937));
#47466=CARTESIAN_POINT('Ctrl Pts',(3.93040117990528,-2.39629247537946,14.8348699419947));
#47467=CARTESIAN_POINT('Ctrl Pts',(3.79148968941664,-4.57499483447723,16.6102790073235));
#47468=CARTESIAN_POINT('Ctrl Pts',(3.65257819892802,-5.63907071376474,19.2115409783509));
#47469=CARTESIAN_POINT('Ctrl Pts',(3.51366670843937,-5.3292745415085,22.004898751788));
#47470=CARTESIAN_POINT('Ctrl Pts',(3.37475521795074,-3.72108334650527,24.3097940637625));
#47471=CARTESIAN_POINT('Ctrl Pts',(3.23584372746209,-1.20630795161736,25.5646749473313));
#47472=CARTESIAN_POINT('Ctrl Pts',(3.09693223697347,1.60236565179515,25.4638091531359));
#47473=CARTESIAN_POINT('Ctrl Pts',(2.95802074648483,4.02064773547646,24.0317710662039));
#47474=CARTESIAN_POINT('Ctrl Pts',(2.8191092559962,5.45936140578133,21.6174545390167));
#47475=CARTESIAN_POINT('Ctrl Pts',(2.68019776550755,5.56798640772404,18.8090703186992));
#47476=CARTESIAN_POINT('Ctrl Pts',(2.54128627501892,4.32005794655219,16.2908376306162));
#47477=CARTESIAN_POINT('Ctrl Pts',(2.40237478453028,2.01961442005369,14.6762847801816));
#47478=CARTESIAN_POINT('Ctrl Pts',(2.26346329404165,-0.772876809690231,
14.3587725124367));
#47479=CARTESIAN_POINT('Ctrl Pts',(2.12455180355301,-3.37706860580615,15.4156577559866));
#47480=CARTESIAN_POINT('Ctrl Pts',(1.98564031306437,-5.15849004463263,17.5894468398745));
#47481=CARTESIAN_POINT('Ctrl Pts',(1.84672882257574,-5.68312547077942,20.3505297671009));
#47482=CARTESIAN_POINT('Ctrl Pts',(1.7078173320871,-4.82315555167649,23.0262115934059));
#47483=CARTESIAN_POINT('Ctrl Pts',(1.56890584159846,-2.78809871671838,24.9646038659185));
#47484=CARTESIAN_POINT('Ctrl Pts',(1.42999435110983,-0.0737647659051136,
25.693447605254));
#47485=CARTESIAN_POINT('Ctrl Pts',(1.29108286062119,2.65854055037997,25.035170932176));
#47486=CARTESIAN_POINT('Ctrl Pts',(1.15217137013255,4.74313426783574,23.1501535580012));
#47487=CARTESIAN_POINT('Ctrl Pts',(1.01325987964391,5.6721358762478,20.497649097109));
#47488=CARTESIAN_POINT('Ctrl Pts',(0.874348389155275,5.21921171941123,17.7239022616837));
#47489=CARTESIAN_POINT('Ctrl Pts',(0.735436898666642,3.49470350187287,15.5046871678098));
#47490=CARTESIAN_POINT('Ctrl Pts',(0.596525408178007,0.918773166897274,
14.3806934322185));
#47491=CARTESIAN_POINT('Ctrl Pts',(0.457613917689371,-1.88101803678174,
14.625740444846));
#47492=CARTESIAN_POINT('Ctrl Pts',(0.318702427200727,-4.2224967827303,16.1801740467554));
#47493=CARTESIAN_POINT('Ctrl Pts',(0.179790936712099,-5.53529199863674,
18.6651865633432));
#47494=CARTESIAN_POINT('Ctrl Pts',(0.0408794462234612,-5.49937647599996,
21.4755287212687));
#47495=CARTESIAN_POINT('Ctrl Pts',(-0.098032044265173,-4.12386623843618,
23.9261367566677));
#47496=CARTESIAN_POINT('Ctrl Pts',(-0.236943534753806,-1.74314764379901,
25.4207072293527));
#47497=CARTESIAN_POINT('Ctrl Pts',(-0.329551195079564,0.12636836631501,
25.5357780776651));
#47498=CARTESIAN_POINT('Ctrl Pts',(-0.375855025242444,1.01853433275011,
25.3664478824926));
#47499=CARTESIAN_POINT('Ctrl Pts',(50.3758550252424,4.37166823191287,23.7929628171897));
#47500=CARTESIAN_POINT('Ctrl Pts',(50.3295511950796,5.00224406373827,23.066177856549));
#47501=CARTESIAN_POINT('Ctrl Pts',(50.2369435347538,5.89327567631712,21.2927683877858));
#47502=CARTESIAN_POINT('Ctrl Pts',(50.0980320442652,5.79343898530443,18.3159622522944));
#47503=CARTESIAN_POINT('Ctrl Pts',(49.9591205537765,4.2823206076606,15.7501656734355));
#47504=CARTESIAN_POINT('Ctrl Pts',(49.8202090632879,1.72778693233764,14.2194224359483));
#47505=CARTESIAN_POINT('Ctrl Pts',(49.6812975727993,-1.247647937075,14.097205211392));
#47506=CARTESIAN_POINT('Ctrl Pts',(49.5423860823106,-3.91913669798948,15.4130220371016));
#47507=CARTESIAN_POINT('Ctrl Pts',(49.403474591822,-5.63577648176899,17.8464306709765));
#47508=CARTESIAN_POINT('Ctrl Pts',(49.2645631013334,-5.97935297166014,20.8044997806298));
#47509=CARTESIAN_POINT('Ctrl Pts',(49.1256516108447,-4.86614978762969,23.5665768168738));
#47510=CARTESIAN_POINT('Ctrl Pts',(48.9867401203561,-2.56738632874741,25.4597067746574));
#47511=CARTESIAN_POINT('Ctrl Pts',(48.8478286298675,0.356881766247415,26.0226669648869));
#47512=CARTESIAN_POINT('Ctrl Pts',(48.7089171393788,3.19420074846009,25.1182962854986));
#47513=CARTESIAN_POINT('Ctrl Pts',(48.5700056488902,5.25330250574948,22.9669329453697));
#47514=CARTESIAN_POINT('Ctrl Pts',(48.4310941584015,6.03251854196515,20.0927220465274));
#47515=CARTESIAN_POINT('Ctrl Pts',(48.2921826679129,5.34200512389304,17.1959210624955));
#47516=CARTESIAN_POINT('Ctrl Pts',(48.1532711774242,3.34999504705893,14.9822902848886));
#47517=CARTESIAN_POINT('Ctrl Pts',(48.0143596869356,0.541810688388326,13.991146648205));
#47518=CARTESIAN_POINT('Ctrl Pts',(47.8754481964469,-2.39837744171306,14.4639668367131));
#47519=CARTESIAN_POINT('Ctrl Pts',(47.7365367059584,-4.75423813142894,16.2855555903485));
#47520=CARTESIAN_POINT('Ctrl Pts',(47.5976252154697,-5.95180249600114,19.012111063151));
#47521=CARTESIAN_POINT('Ctrl Pts',(47.4587137249811,-5.69930256348713,21.9793503451825));
#47522=CARTESIAN_POINT('Ctrl Pts',(47.3198022344924,-4.05825602460495,24.4643516366976));
#47523=CARTESIAN_POINT('Ctrl Pts',(47.1808907440038,-1.42847839604861,25.8616829470684));
#47524=CARTESIAN_POINT('Ctrl Pts',(47.0419792535151,1.54932582119811,25.8309061901086));
#47525=CARTESIAN_POINT('Ctrl Pts',(46.9030677630265,4.14966085031285,24.3795196456277));
#47526=CARTESIAN_POINT('Ctrl Pts',(46.7641562725379,5.73899542293203,21.861131116882));
#47527=CARTESIAN_POINT('Ctrl Pts',(46.6252447820492,5.93011283962871,18.8893068794517));
#47528=CARTESIAN_POINT('Ctrl Pts',(46.4863332915607,4.67645030826474,16.1880857809881));
#47529=CARTESIAN_POINT('Ctrl Pts',(46.347421801072,2.28344324566841,14.4155784146835));
#47530=CARTESIAN_POINT('Ctrl Pts',(46.2085103105834,-0.665889320858256,
14.0036286880202));
#47531=CARTESIAN_POINT('Ctrl Pts',(46.0695988200947,-3.45298829007873,15.052601757759));
#47532=CARTESIAN_POINT('Ctrl Pts',(45.9306873296061,-5.39882025860657,17.3069316172779));
#47533=CARTESIAN_POINT('Ctrl Pts',(45.7917758391174,-6.02931346989326,20.2173857872984));
#47534=CARTESIAN_POINT('Ctrl Pts',(45.6528643486288,-5.19085803932404,23.074877284436));
#47535=CARTESIAN_POINT('Ctrl Pts',(45.5139528581402,-3.08773061831874,25.183222658487));
#47536=CARTESIAN_POINT('Ctrl Pts',(45.3750413676515,-0.232325558931368,
26.0287562841288));
#47537=CARTESIAN_POINT('Ctrl Pts',(45.2361298771629,2.67968201680631,25.4054770175777));
#47538=CARTESIAN_POINT('Ctrl Pts',(45.0972183866742,4.93882666231995,23.4652371777865));
#47539=CARTESIAN_POINT('Ctrl Pts',(44.9583068961857,5.99470285045386,20.6807460859354));
#47540=CARTESIAN_POINT('Ctrl Pts',(44.819395405697,5.59006273694311,17.7304017765701));
#47541=CARTESIAN_POINT('Ctrl Pts',(44.6804839152084,3.82349060474963,15.3330098463627));
#47542=CARTESIAN_POINT('Ctrl Pts',(44.5415724247197,1.12538433371236,14.0726576275543));
#47543=CARTESIAN_POINT('Ctrl Pts',(44.4026609342311,-1.84690436237671,14.2564103754716));
#47544=CARTESIAN_POINT('Ctrl Pts',(44.2637494437424,-4.36922347763402,15.8394995852365));
#47545=CARTESIAN_POINT('Ctrl Pts',(44.1248379532538,-5.82704911026108,18.436230143096));
#47546=CARTESIAN_POINT('Ctrl Pts',(43.9859264627652,-5.86520467277351,21.4139489542525));
#47547=CARTESIAN_POINT('Ctrl Pts',(43.8470149722765,-4.47439415460361,24.0471810495708));
#47548=CARTESIAN_POINT('Ctrl Pts',(43.7081034817879,-1.99346695078559,25.6943803012164));
#47549=CARTESIAN_POINT('Ctrl Pts',(43.5691919912993,0.973137533632203,25.9542321788281));
#47550=CARTESIAN_POINT('Ctrl Pts',(43.4302805008106,3.70265216271139,24.7634278057639));
#47551=CARTESIAN_POINT('Ctrl Pts',(43.291369010322,5.53007306373358,22.4120881842347));
#47552=CARTESIAN_POINT('Ctrl Pts',(43.1524575198334,6.01017749880994,19.4730807162811));
#47553=CARTESIAN_POINT('Ctrl Pts',(43.0135460293447,5.02599547436225,16.6624489531326));
#47554=CARTESIAN_POINT('Ctrl Pts',(42.8746345388561,2.81730766448726,14.6649596981487));
#47555=CARTESIAN_POINT('Ctrl Pts',(42.7357230483674,-0.0777734284877525,
13.9672702039146));
#47556=CARTESIAN_POINT('Ctrl Pts',(42.5968115578788,-2.95390623278611,14.739361686386));
#47557=CARTESIAN_POINT('Ctrl Pts',(42.4579000673901,-5.11036563305792,16.7931260400171));
#47558=CARTESIAN_POINT('Ctrl Pts',(42.3189885769016,-6.02176376830294,19.6281954579217));
#47559=CARTESIAN_POINT('Ctrl Pts',(42.1800770864129,-5.46605262930032,22.553849281472));
#47560=CARTESIAN_POINT('Ctrl Pts',(42.0411655959243,-3.57862260949675,24.8572973676269));
#47561=CARTESIAN_POINT('Ctrl Pts',(41.9022541054356,-0.819316737129712,
25.9773403435821));
#47562=CARTESIAN_POINT('Ctrl Pts',(41.763342614947,2.13960294106554,25.6410971231969));
#47563=CARTESIAN_POINT('Ctrl Pts',(41.6244311244583,4.57724157290559,23.9304881480575));
#47564=CARTESIAN_POINT('Ctrl Pts',(41.4855196339698,5.8997063419931,21.2622767434293));
#47565=CARTESIAN_POINT('Ctrl Pts',(41.346608143481,5.78479923421689,18.286531202922));
#47566=CARTESIAN_POINT('Ctrl Pts',(41.2076966529925,4.26051558283505,15.7282457389059));
#47567=CARTESIAN_POINT('Ctrl Pts',(41.0687851625038,1.69822344006145,14.2107068957962));
#47568=CARTESIAN_POINT('Ctrl Pts',(40.9298736720152,-1.27781448459974,14.103639457962));
#47569=CARTESIAN_POINT('Ctrl Pts',(40.7909621815266,-3.94253274391769,15.4331287447649));
#47570=CARTESIAN_POINT('Ctrl Pts',(40.6520506910379,-5.6467140949177,17.8752653273847));
#47571=CARTESIAN_POINT('Ctrl Pts',(40.5131392005493,-5.97516120318881,20.8350605335323));
#47572=CARTESIAN_POINT('Ctrl Pts',(40.3742277100606,-4.84785302885217,23.5914062022284));
#47573=CARTESIAN_POINT('Ctrl Pts',(40.235316219572,-2.53944071086646,25.4727614944149));
#47574=CARTESIAN_POINT('Ctrl Pts',(40.0964047290833,0.387666919931939,26.020763394948));
#47575=CARTESIAN_POINT('Ctrl Pts',(39.9574932385947,3.22032552293136,25.1018997466741));
#47576=CARTESIAN_POINT('Ctrl Pts',(39.8185817481061,5.26840179713572,22.9400374151859));
#47577=CARTESIAN_POINT('Ctrl Pts',(39.6796702576175,6.03291374792276,20.0618806018121));
#47578=CARTESIAN_POINT('Ctrl Pts',(39.5407587671288,5.32759990499422,17.1686475402978));
#47579=CARTESIAN_POINT('Ctrl Pts',(39.4018472766402,3.32429903852281,14.9652295582388));
#47580=CARTESIAN_POINT('Ctrl Pts',(39.2629357861515,0.511084310026281,13.9884552462116));
#47581=CARTESIAN_POINT('Ctrl Pts',(39.1240242956629,-2.42664817772029,14.4763005041618));
#47582=CARTESIAN_POINT('Ctrl Pts',(38.9851128051743,-4.77316550262547,16.3099094071687));
#47583=CARTESIAN_POINT('Ctrl Pts',(38.8462013146856,-5.95677514037071,19.0425516067079));
#47584=CARTESIAN_POINT('Ctrl Pts',(38.707289824197,-5.68910897433122,22.0084612460638));
#47585=CARTESIAN_POINT('Ctrl Pts',(38.5683783337084,-4.03537971123355,24.4850404775119));
#47586=CARTESIAN_POINT('Ctrl Pts',(38.4294668432197,-1.39849281737248,25.8689092119843));
#47587=CARTESIAN_POINT('Ctrl Pts',(38.2905553527311,1.57911514448126,25.8229093122962));
#47588=CARTESIAN_POINT('Ctrl Pts',(38.1516438622424,4.17199621190449,24.3582479400111));
#47589=CARTESIAN_POINT('Ctrl Pts',(38.0127323717538,5.7484351586937,21.8317671044787));
#47590=CARTESIAN_POINT('Ctrl Pts',(37.8738208812651,5.92435710444692,18.8590046460457));
#47591=CARTESIAN_POINT('Ctrl Pts',(37.7349093907765,4.6569013976858,16.1642279954371));
#47592=CARTESIAN_POINT('Ctrl Pts',(37.5959979002879,2.25486394831888,14.4039776561089));
#47593=CARTESIAN_POINT('Ctrl Pts',(37.4570864097993,-0.696536102775852,
14.0071113011932));
#47594=CARTESIAN_POINT('Ctrl Pts',(37.3181749193106,-3.47823594384081,15.070319258032));
#47595=CARTESIAN_POINT('Ctrl Pts',(37.179263428822,-5.41251758525951,17.3345674107169));
#47596=CARTESIAN_POINT('Ctrl Pts',(37.0403519383333,-6.0281233284039,20.2482068417848));
#47597=CARTESIAN_POINT('Ctrl Pts',(36.9014404478447,-5.17507038919311,23.1013745284394));
#47598=CARTESIAN_POINT('Ctrl Pts',(36.7625289573561,-3.06119187544985,25.1989404497874));
#47599=CARTESIAN_POINT('Ctrl Pts',(36.6236174668674,-0.20150147609856,26.0298652268426));
#47600=CARTESIAN_POINT('Ctrl Pts',(36.4847059763788,2.7072816302624,25.3917069350253));
#47601=CARTESIAN_POINT('Ctrl Pts',(36.3457944858901,4.95647758897316,23.4399429368469));
#47602=CARTESIAN_POINT('Ctrl Pts',(36.2068829954015,5.99810471599718,20.6500902358045));
#47603=CARTESIAN_POINT('Ctrl Pts',(36.0679715049129,5.57838672963962,17.7018531393018));
#47604=CARTESIAN_POINT('Ctrl Pts',(35.9290600144242,3.79958140254752,15.3135238543047));
#47605=CARTESIAN_POINT('Ctrl Pts',(35.7901485239356,1.09506704261718,14.0669817402161));
#47606=CARTESIAN_POINT('Ctrl Pts',(35.651237033447,-1.87624340496498,14.2659274347039));
#47607=CARTESIAN_POINT('Ctrl Pts',(35.5123255429584,-4.39043626938002,15.861890907278));
#47608=CARTESIAN_POINT('Ctrl Pts',(35.3734140524697,-5.83496748371407,18.4660404298824));
#47609=CARTESIAN_POINT('Ctrl Pts',(35.2345025619811,-5.85789943914815,21.443915392114));
#47610=CARTESIAN_POINT('Ctrl Pts',(35.0955910714924,-4.45364512068325,24.0700027810519));
#47611=CARTESIAN_POINT('Ctrl Pts',(34.9566795810038,-1.96432929662502,25.7044971656735));
#47612=CARTESIAN_POINT('Ctrl Pts',(34.8177680905152,1.00356487086217,25.9491793592669));
#47613=CARTESIAN_POINT('Ctrl Pts',(34.6788566000265,3.7269560345781,24.7444363432422));
#47614=CARTESIAN_POINT('Ctrl Pts',(34.5399451095379,5.54233220909366,22.3837850538165));
#47615=CARTESIAN_POINT('Ctrl Pts',(34.4010336190493,6.00740516717897,19.4423615363808));
#47616=CARTESIAN_POINT('Ctrl Pts',(34.2621221285606,5.00886710131083,16.6367979751193));
#47617=CARTESIAN_POINT('Ctrl Pts',(34.123210638072,2.78999631224823,14.6506263846692));
#47618=CARTESIAN_POINT('Ctrl Pts',(33.9842991475834,-0.10861377285947,13.967746644321));
#47619=CARTESIAN_POINT('Ctrl Pts',(33.8453876570947,-2.98076179807835,14.7545318033685));
#47620=CARTESIAN_POINT('Ctrl Pts',(33.706476166606,-5.12669347763074,16.8192938700385));
#47621=CARTESIAN_POINT('Ctrl Pts',(33.5675646761175,-6.0235858662618,19.6589856153662));
#47622=CARTESIAN_POINT('Ctrl Pts',(33.4286531856287,-5.45292505475955,22.5817602223931));
#47623=CARTESIAN_POINT('Ctrl Pts',(33.2897416951402,-3.55374369223119,24.875529024494));
#47624=CARTESIAN_POINT('Ctrl Pts',(33.1508302046515,-0.788747839168509,
25.9814508561855));
#47625=CARTESIAN_POINT('Ctrl Pts',(33.0119187141629,2.16841418221486,25.6300850289428));
#47626=CARTESIAN_POINT('Ctrl Pts',(32.8730072236743,4.59727574553591,23.9070363727848));
#47627=CARTESIAN_POINT('Ctrl Pts',(32.7340957331856,5.90608243090708,21.232098948172));
#47628=CARTESIAN_POINT('Ctrl Pts',(32.595184242697,5.77596380431826,18.2569797390846));
#47629=CARTESIAN_POINT('Ctrl Pts',(32.4562727522083,4.23862124947789,15.7065203619639));
#47630=CARTESIAN_POINT('Ctrl Pts',(32.3173612617197,1.66860441773134,14.2021006566271));
#47631=CARTESIAN_POINT('Ctrl Pts',(32.1784497712311,-1.3079419808491,14.1102491331561));
#47632=CARTESIAN_POINT('Ctrl Pts',(32.0395382807424,-3.96582861725453,15.4533439895544));
#47633=CARTESIAN_POINT('Ctrl Pts',(31.9006267902538,-5.65750266739463,17.9041610111513));
#47634=CARTESIAN_POINT('Ctrl Pts',(31.7617152997651,-5.97081400657861,20.8655966714357));
#47635=CARTESIAN_POINT('Ctrl Pts',(31.6228038092766,-4.82942919013311,23.6161431382409));
#47636=CARTESIAN_POINT('Ctrl Pts',(31.4838923187878,-2.51142891237346,25.4856724580356));
#47637=CARTESIAN_POINT('Ctrl Pts',(31.3449808282993,0.418442038286222,26.0187028302909));
#47638=CARTESIAN_POINT('Ctrl Pts',(31.2060693378106,3.24636608124152,25.0853696783341));
#47639=CARTESIAN_POINT('Ctrl Pts',(31.067157847322,5.28336341756275,22.9130651377399));
#47640=CARTESIAN_POINT('Ctrl Pts',(30.9282463568333,6.03315126387911,20.0310374920047));
#47641=CARTESIAN_POINT('Ctrl Pts',(30.7893348663447,5.31305544940377,17.1414480430965));
#47642=CARTESIAN_POINT('Ctrl Pts',(30.650423375856,3.29851614223578,14.9483004089548));
#47643=CARTESIAN_POINT('Ctrl Pts',(30.5115118853675,0.480344575529053,13.9859209692991));
#47644=CARTESIAN_POINT('Ctrl Pts',(30.3726003948788,-2.45485549124979,14.4887785368544));
#47645=CARTESIAN_POINT('Ctrl Pts',(30.2336889043902,-4.79196812107072,16.3343596704807));
#47646=CARTESIAN_POINT('Ctrl Pts',(30.0947774139015,-5.96159209759578,19.0730171734927));
#47647=CARTESIAN_POINT('Ctrl Pts',(29.9558659234129,-5.67876669347553,22.037519653851));
#47648=CARTESIAN_POINT('Ctrl Pts',(29.8169544329242,-4.01239792849797,24.5056120962796));
#47649=CARTESIAN_POINT('Ctrl Pts',(29.6780429424356,-1.36847068740464,25.8759820861257));
#47650=CARTESIAN_POINT('Ctrl Pts',(29.539131451947,1.60886319570866,25.8147602458098));
#47651=CARTESIAN_POINT('Ctrl Pts',(29.4002199614584,4.19422253344966,24.336862326459));
#47652=CARTESIAN_POINT('Ctrl Pts',(29.2613084709697,5.75772465230203,21.8023552166622));
#47653=CARTESIAN_POINT('Ctrl Pts',(29.1223969804811,5.91844652918931,18.8287322339093));
#47654=CARTESIAN_POINT('Ctrl Pts',(28.9834854899924,4.63723077348171,16.1404704623192));
#47655=CARTESIAN_POINT('Ctrl Pts',(28.8445739995038,2.22622571743447,14.3925231561968));
#47656=CARTESIAN_POINT('Ctrl Pts',(28.7056625090152,-0.72716467989911,14.0107505455973));
#47657=CARTESIAN_POINT('Ctrl Pts',(28.5667510185265,-3.50339268979386,15.0881656013405));
#47658=CARTESIAN_POINT('Ctrl Pts',(28.4278395280379,-5.42607344936586,17.3622728683879));
#47659=CARTESIAN_POINT('Ctrl Pts',(28.2889280375493,-6.02677563478385,20.279021409092));
#47660=CARTESIAN_POINT('Ctrl Pts',(28.1500165470606,-5.15914748247874,23.1277907143524));
#47661=CARTESIAN_POINT('Ctrl Pts',(28.011105056572,-3.03457312471181,25.2145223606322));
#47662=CARTESIAN_POINT('Ctrl Pts',(27.8721935660833,-0.170672126786414,
26.0308165718992));
#47663=CARTESIAN_POINT('Ctrl Pts',(27.7332820755947,2.73481048571209,25.3777959338371));
#47664=CARTESIAN_POINT('Ctrl Pts',(27.5943705851061,4.97399897222422,23.4145587889313));
#47665=CARTESIAN_POINT('Ctrl Pts',(27.4554590946174,6.00134981398182,20.6194173947965));
#47666=CARTESIAN_POINT('Ctrl Pts',(27.3165476041288,5.5665649246032,17.673364566819));
#47667=CARTESIAN_POINT('Ctrl Pts',(27.1776361136402,3.77557289379296,15.2941603488419));
#47668=CARTESIAN_POINT('Ctrl Pts',(27.0387246231515,1.06472113065006,14.0614609193251));
#47669=CARTESIAN_POINT('Ctrl Pts',(26.8998131326629,-1.90553340971345,14.2755943607024));
#47670=CARTESIAN_POINT('Ctrl Pts',(26.7609016421742,-4.41153431188298,15.8843903836934));
#47671=CARTESIAN_POINT('Ctrl Pts',(26.6219901516856,-5.84273335339281,18.4958908085158));
#47672=CARTESIAN_POINT('Ctrl Pts',(26.483078661197,-5.85044110239477,21.4738440915395));
#47673=CARTESIAN_POINT('Ctrl Pts',(26.3441671707084,-4.43277968548176,24.0927181381982));
#47674=CARTESIAN_POINT('Ctrl Pts',(26.2052556802197,-1.93514030239562,25.7144649363523));
#47675=CARTESIAN_POINT('Ctrl Pts',(26.0663441897311,1.03396597873771,25.943971050869));
#47676=CARTESIAN_POINT('Ctrl Pts',(25.9274326992424,3.75116249804223,24.7253208792671));
#47677=CARTESIAN_POINT('Ctrl Pts',(25.7885212087538,5.5544464990484,22.3554196203575));
#47678=CARTESIAN_POINT('Ctrl Pts',(25.6496097182652,6.00447582491098,19.4116569310209));
#47679=CARTESIAN_POINT('Ctrl Pts',(25.5106982277765,4.99160781559538,16.6112348983674));
#47680=CARTESIAN_POINT('Ctrl Pts',(25.3717867372879,2.76261204015674,14.636432883394));
#47681=CARTESIAN_POINT('Ctrl Pts',(25.2328752467992,-0.13945127848183,13.9683807448011));
#47682=CARTESIAN_POINT('Ctrl Pts',(25.0939637563106,-3.00753945763662,14.7698390168643));
#47683=CARTESIAN_POINT('Ctrl Pts',(24.955052265822,-5.1428873300079,16.8455448315755));
#47684=CARTESIAN_POINT('Ctrl Pts',(24.8161407753333,-6.02525053068195,19.6897846856248));
#47685=CARTESIAN_POINT('Ctrl Pts',(24.6772292848447,-5.43965496157513,22.6096036859583));
#47686=CARTESIAN_POINT('Ctrl Pts',(24.538317794356,-3.5287718936724,24.8936332536454));
#47687=CARTESIAN_POINT('Ctrl Pts',(24.3994063038674,-0.758158326349866,
25.9854050364986));
#47688=CARTESIAN_POINT('Ctrl Pts',(24.2604948133788,2.19716874929574,25.6189257857596));
#47689=CARTESIAN_POINT('Ctrl Pts',(24.1215833228901,4.61718976292897,23.8834824824969));
#47690=CARTESIAN_POINT('Ctrl Pts',(23.9826718324015,5.91230415737359,21.201888950552));
#47691=CARTESIAN_POINT('Ctrl Pts',(23.8437603419129,5.76697741277629,18.2274738311427));
#47692=CARTESIAN_POINT('Ctrl Pts',(23.7048488514242,4.21661613474277,15.6849072001887));
#47693=CARTESIAN_POINT('Ctrl Pts',(23.5659373609356,1.63894178445187,14.1936459524127));
#47694=CARTESIAN_POINT('Ctrl Pts',(23.427025870447,-1.3380352924883,14.117012743953));
#47695=CARTESIAN_POINT('Ctrl Pts',(23.2881143799583,-3.9890208389714,15.4736780665746));
#47696=CARTESIAN_POINT('Ctrl Pts',(23.1492028894697,-5.6681433743501,17.9331114721478));
#47697=CARTESIAN_POINT('Ctrl Pts',(23.0102913989811,-5.96631075568467,20.8961101859467));
#47698=CARTESIAN_POINT('Ctrl Pts',(22.8713799084924,-4.81087912857205,23.6407855620767));
#47699=CARTESIAN_POINT('Ctrl Pts',(22.7324684180038,-2.48335147471651,25.4984400471206));
#47700=CARTESIAN_POINT('Ctrl Pts',(22.5935569275151,0.449206220163045,26.0164849597188));
#47701=CARTESIAN_POINT('Ctrl Pts',(22.4546454370265,3.27232179193575,25.068706697845));
#47702=CARTESIAN_POINT('Ctrl Pts',(22.3157339465378,5.29818695103998,22.8860167238922));
#47703=CARTESIAN_POINT('Ctrl Pts',(22.1768224560493,6.03323109629379,20.0001935709956));
#47704=CARTESIAN_POINT('Ctrl Pts',(22.0379109655606,5.29837213082718,17.1143232575304));
#47705=CARTESIAN_POINT('Ctrl Pts',(21.898999475072,3.27264703532933,14.9315032918126));
#47706=CARTESIAN_POINT('Ctrl Pts',(21.7600879845833,0.44959228665845,13.983543877453));
#47707=CARTESIAN_POINT('Ctrl Pts',(21.6211764940947,-2.48299864422846,14.5014006118362));
#47708=CARTESIAN_POINT('Ctrl Pts',(21.4822650036061,-4.81064549576327,16.358905739637));
#47709=CARTESIAN_POINT('Ctrl Pts',(21.3433535131174,-5.96625324156263,19.1035069680698));
#47710=CARTESIAN_POINT('Ctrl Pts',(21.2044420226288,-5.6682759913379,22.066524808653));
#47711=CARTESIAN_POINT('Ctrl Pts',(21.0655305321402,-3.9893112769984,24.5260659555479));
#47712=CARTESIAN_POINT('Ctrl Pts',(20.9266190416515,-1.33841279083736,25.8829013845278));
#47713=CARTESIAN_POINT('Ctrl Pts',(20.7877075511629,1.63856919739414,25.8064592036892));
#47714=CARTESIAN_POINT('Ctrl Pts',(20.6487960606742,4.21633923402979,24.3153633638823));
#47715=CARTESIAN_POINT('Ctrl Pts',(20.5098845701856,5.76686366096883,21.7728962221611));
#47716=CARTESIAN_POINT('Ctrl Pts',(20.370973079697,5.91238126833391,18.798490434241));
#47717=CARTESIAN_POINT('Ctrl Pts',(20.2320615892084,4.61743894976846,16.1168138025692));
#47718=CARTESIAN_POINT('Ctrl Pts',(20.0931500987197,2.19752930150873,14.381215214322));
#47719=CARTESIAN_POINT('Ctrl Pts',(19.9542386082311,-0.757774251713633,
14.0145463261173));
#47720=CARTESIAN_POINT('Ctrl Pts',(19.8153271177424,-3.52845787043656,15.1061403212485));
#47721=CARTESIAN_POINT('Ctrl Pts',(19.6764156272538,-5.43948749662697,17.3900472661761));
#47722=CARTESIAN_POINT('Ctrl Pts',(19.5375041367651,-6.02527042425674,20.3098286838448));
#47723=CARTESIAN_POINT('Ctrl Pts',(19.3985926462765,-5.14308973534492,23.1541251517569));
#47724=CARTESIAN_POINT('Ctrl Pts',(19.2596811557879,-3.0078750618172,25.2299679837695));
#47725=CARTESIAN_POINT('Ctrl Pts',(19.1207696652993,-0.139838316756449,
26.0316102944341));
#47726=CARTESIAN_POINT('Ctrl Pts',(18.9818581748106,2.76226786365617,25.3637443775937));
#47727=CARTESIAN_POINT('Ctrl Pts',(18.842946684322,4.99139035413101,23.3890853974847));
#47728=CARTESIAN_POINT('Ctrl Pts',(18.7040351938333,6.00443805959323,20.5887283645827));
#47729=CARTESIAN_POINT('Ctrl Pts',(18.5651237033447,5.55459763081084,17.6449368037043));
#47730=CARTESIAN_POINT('Ctrl Pts',(18.426212212856,3.75146570597672,15.2749198360624));
#47731=CARTESIAN_POINT('Ctrl Pts',(18.2873007223674,1.03434739093725,14.0560953091745));
#47732=CARTESIAN_POINT('Ctrl Pts',(18.1483892318788,-1.93477361109326,14.2854109008107));
#47733=CARTESIAN_POINT('Ctrl Pts',(18.0094777413902,-4.43251705372066,15.9069974264324));
#47734=CARTESIAN_POINT('Ctrl Pts',(17.8705662509015,-5.85034651632709,18.5257804988213));
#47735=CARTESIAN_POINT('Ctrl Pts',(17.7316547604129,-5.84282985744584,21.5037342703069));
#47736=CARTESIAN_POINT('Ctrl Pts',(17.5927432699242,-4.41179839434207,24.1153265273167));
#47737=CARTESIAN_POINT('Ctrl Pts',(17.4538317794356,-1.90590073098647,25.7242833527334));
#47738=CARTESIAN_POINT('Ctrl Pts',(17.314920288947,1.06434006268985,25.9386073897598));
#47739=CARTESIAN_POINT('Ctrl Pts',(17.1760087984583,3.77527092043926,24.7060819134437));
#47740=CARTESIAN_POINT('Ctrl Pts',(17.0370973079697,5.56641561697647,22.3269926252217));
#47741=CARTESIAN_POINT('Ctrl Pts',(16.8981858174811,6.00138954856782,19.3809677027029));
#47742=CARTESIAN_POINT('Ctrl Pts',(16.7592743269924,4.97421806830788,16.5857603909984));
#47743=CARTESIAN_POINT('Ctrl Pts',(16.6203628365038,2.73515556393329,14.6223795652872));
#47744=CARTESIAN_POINT('Ctrl Pts',(16.4814513460151,-0.170285139380104,
13.9691724887821));
#47745=CARTESIAN_POINT('Ctrl Pts',(16.3425398555265,-3.03423851159519,14.7852829268014));
#47746=CARTESIAN_POINT('Ctrl Pts',(16.2036283650379,-5.15894676694387,16.8718782385279));
#47747=CARTESIAN_POINT('Ctrl Pts',(16.0647168745492,-6.02675771805542,19.7205918637273));
#47748=CARTESIAN_POINT('Ctrl Pts',(15.9258053840606,-5.42624269657667,22.6373789444455));
#47749=CARTESIAN_POINT('Ctrl Pts',(15.786893893572,-3.50370786648795,24.9116095819056));
#47750=CARTESIAN_POINT('Ctrl Pts',(15.6479824030833,-0.727548998167088,
25.989202781174));
#47751=CARTESIAN_POINT('Ctrl Pts',(15.5090709125947,2.22586589077336,25.6076196853075));
#47752=CARTESIAN_POINT('Ctrl Pts',(15.3701594221061,4.63698310460833,23.8598270928026));
#47753=CARTESIAN_POINT('Ctrl Pts',(15.2312479316174,5.91837135878041,21.1716475401432));
#47754=CARTESIAN_POINT('Ctrl Pts',(15.0923364411288,5.75784029446099,18.1980142502679));
#47755=CARTESIAN_POINT('Ctrl Pts',(14.9534249506401,4.19450081375939,15.6634068184659));
#47756=CARTESIAN_POINT('Ctrl Pts',(14.8145134601515,1.60923631549108,14.1853430041265));
#47757=CARTESIAN_POINT('Ctrl Pts',(14.6756019696629,-1.36809363299307,14.1239301135776));
#47758=CARTESIAN_POINT('Ctrl Pts',(14.5366904791742,-4.01210880291211,15.4941304443702));
#47759=CARTESIAN_POINT('Ctrl Pts',(14.3977789886856,-5.67863593767664,17.9621159537198));
#47760=CARTESIAN_POINT('Ctrl Pts',(14.258867498197,-5.96165156820477,20.9266002795585));
#47761=CARTESIAN_POINT('Ctrl Pts',(14.1199560077083,-4.7922033289967,23.6653328296771));
#47762=CARTESIAN_POINT('Ctrl Pts',(13.9810445172197,-2.45520913173245,25.5110639279737));
#47763=CARTESIAN_POINT('Ctrl Pts',(13.8421330267311,0.479958661504232,26.0141098411987));
#47764=CARTESIAN_POINT('Ctrl Pts',(13.7032215362424,3.29819197663088,25.0519112407131));
#47765=CARTESIAN_POINT('Ctrl Pts',(13.5643100457538,5.31287201013686,22.8588928805851));
#47766=CARTESIAN_POINT('Ctrl Pts',(13.4253985552651,6.03315324308028,19.9693496449273));
#47767=CARTESIAN_POINT('Ctrl Pts',(13.2864870647765,5.28355033303033,17.087273892538));
#47768=CARTESIAN_POINT('Ctrl Pts',(13.1475755742879,3.24669239392315,14.9148386458247));
#47769=CARTESIAN_POINT('Ctrl Pts',(13.0086640837993,0.418828247161937,13.9813240328013));
#47770=CARTESIAN_POINT('Ctrl Pts',(12.8697525933106,-2.51107690110167,14.5141663992143));
#47771=CARTESIAN_POINT('Ctrl Pts',(12.730841102822,-4.82919713854782,16.3835469730967));
#47772=CARTESIAN_POINT('Ctrl Pts',(12.5919296123333,-5.9707584504467,19.1340201935521));
#47773=CARTESIAN_POINT('Ctrl Pts',(12.4530181218447,-5.65763714210527,22.0954759523857));
#47774=CARTESIAN_POINT('Ctrl Pts',(12.314106631356,-3.96612036013178,24.5464015207309));
#47775=CARTESIAN_POINT('Ctrl Pts',(12.1751951408674,-1.30831991326933,25.8896669263464));
#47776=CARTESIAN_POINT('Ctrl Pts',(12.0362836503788,1.66823237313624,25.798006402892));
#47777=CARTESIAN_POINT('Ctrl Pts',(11.8973721598901,4.23834573559875,24.2937516141817));
#47778=CARTESIAN_POINT('Ctrl Pts',(11.7584606694015,5.77585194583529,21.7433908909211));
#47779=CARTESIAN_POINT('Ctrl Pts',(11.6195491789129,5.90616148040345,18.7682800374458));
#47780=CARTESIAN_POINT('Ctrl Pts',(11.4806376884242,4.59752644382878,16.0932586344818));
#47781=CARTESIAN_POINT('Ctrl Pts',(11.3417261979356,2.16877545055644,14.3700541260311));
#47782=CARTESIAN_POINT('Ctrl Pts',(11.202814707447,-0.788364018202142,14.0184985435461));
#47783=CARTESIAN_POINT('Ctrl Pts',(11.0639032169583,-3.55343083066098,15.1242429479655));
#47784=CARTESIAN_POINT('Ctrl Pts',(10.9249917264697,-5.45275937645092,17.417889878165));
#47785=CARTESIAN_POINT('Ctrl Pts',(10.786080235981,-6.02360773616301,20.3406278608587));
#47786=CARTESIAN_POINT('Ctrl Pts',(10.6471687454924,-5.12689756747983,23.1803771523713));
#47787=CARTESIAN_POINT('Ctrl Pts',(10.5082572550038,-2.9810983845514,25.2452769155099));
#47788=CARTESIAN_POINT('Ctrl Pts',(10.3693457645151,-0.109000851886715,
26.0322463737023));
#47789=CARTESIAN_POINT('Ctrl Pts',(10.2304342740265,2.78965304646366,25.3495526335491));
#47790=CARTESIAN_POINT('Ctrl Pts',(10.0915227835379,5.00865128014925,23.363523428284));
#47791=CARTESIAN_POINT('Ctrl Pts',(9.95261129304924,6.00736937211653,20.5580239472569));
#47792=CARTESIAN_POINT('Ctrl Pts',(9.8136998025606,5.5424851610418,17.6165705929506));
#47793=CARTESIAN_POINT('Ctrl Pts',(9.67478831207196,3.72726046916863,15.2558028188397));
#47794=CARTESIAN_POINT('Ctrl Pts',(9.53587682158333,1.00394661733243,14.0508850500009));
#47795=CARTESIAN_POINT('Ctrl Pts',(9.39696533109468,-1.96396324487712,14.2953767984618));
#47796=CARTESIAN_POINT('Ctrl Pts',(9.25805384060606,-4.45338394648429,15.929711444633));
#47797=CARTESIAN_POINT('Ctrl Pts',(9.11914235011741,-5.85780677353792,18.5557087195966));
#47798=CARTESIAN_POINT('Ctrl Pts',(8.98023085962879,-5.83506590323019,21.5335851472013));
#47799=CARTESIAN_POINT('Ctrl Pts',(8.84131936914014,-4.39070179563497,24.1378273575107));
#47800=CARTESIAN_POINT('Ctrl Pts',(8.7024078786515,-1.87661134660821,25.7339521582009));
#47801=CARTESIAN_POINT('Ctrl Pts',(8.56349638816287,1.09468632885601,25.9330885161248));
#47802=CARTESIAN_POINT('Ctrl Pts',(8.42458489767425,3.79928067166699,24.6867199486051));
#47803=CARTESIAN_POINT('Ctrl Pts',(8.2856734071856,5.57823925005091,22.2985048113823));
#47804=CARTESIAN_POINT('Ctrl Pts',(8.14676191669697,5.99814641881297,19.3502946535258));
#47805=CARTESIAN_POINT('Ctrl Pts',(8.00785042620833,4.95669831394964,16.5603751188182));
#47806=CARTESIAN_POINT('Ctrl Pts',(7.86893893571969,2.70762760118508,14.6084667976487));
#47807=CARTESIAN_POINT('Ctrl Pts',(7.73002744523105,-0.201114549674929,
13.9701218555708));
#47808=CARTESIAN_POINT('Ctrl Pts',(7.59111595474242,-3.06085826214264,14.800863129535));
#47809=CARTESIAN_POINT('Ctrl Pts',(7.45220446425378,-5.17487136870639,16.8982934026413));
#47810=CARTESIAN_POINT('Ctrl Pts',(7.31329297376514,-6.02810738899013,19.7514063444921));
#47811=CARTESIAN_POINT('Ctrl Pts',(7.1743814832765,-5.41268861030941,22.6650852719158));
#47812=CARTESIAN_POINT('Ctrl Pts',(7.03546999278787,-3.47855226575563,24.9294575394421));
#47813=CARTESIAN_POINT('Ctrl Pts',(6.89655850229923,-0.696920654630925,
25.9928439909533));
#47814=CARTESIAN_POINT('Ctrl Pts',(6.7576470118106,2.25450485661422,25.5961670230846));
#47815=CARTESIAN_POINT('Ctrl Pts',(6.61873552132196,4.65665525325171,23.8360708219635));
#47816=CARTESIAN_POINT('Ctrl Pts',(6.47982403083332,5.92428387655414,21.1413755073405));
#47817=CARTESIAN_POINT('Ctrl Pts',(6.34091254034468,5.74855268818165,18.1686017664212));
#47818=CARTESIAN_POINT('Ctrl Pts',(6.20200104985605,4.17227586453774,15.6420197787333));
#47819=CARTESIAN_POINT('Ctrl Pts',(6.06308955936741,1.57948878723643,14.177192028776));
#47820=CARTESIAN_POINT('Ctrl Pts',(5.92417806887878,-1.39811621675317,14.1310010612364));
#47821=CARTESIAN_POINT('Ctrl Pts',(5.78526657839015,-4.0350919056455,15.5147005883943));
#47822=CARTESIAN_POINT('Ctrl Pts',(5.64635508790151,-5.68898008313875,17.991173697801));
#47823=CARTESIAN_POINT('Ctrl Pts',(5.50744359741287,-5.95683656591226,20.9570661553763));
#47824=CARTESIAN_POINT('Ctrl Pts',(5.36853210692424,-4.77340227952123,23.6897842994703));
#47825=CARTESIAN_POINT('Ctrl Pts',(5.2296206164356,-2.4270026189548,25.5235437706551));
#47826=CARTESIAN_POINT('Ctrl Pts',(5.09070912594696,0.510698558558281,26.011577536807));
#47827=CARTESIAN_POINT('Ctrl Pts',(4.95179763545832,3.32397595917902,25.0349837459078));
#47828=CARTESIAN_POINT('Ctrl Pts',(4.81288614496969,5.32741821104193,22.8316943167324));
#47829=CARTESIAN_POINT('Ctrl Pts',(4.67397465448105,6.03291770627337,19.9385065199425));
#47830=CARTESIAN_POINT('Ctrl Pts',(4.53506316399242,5.26859044339846,17.0603006550862));
#47831=CARTESIAN_POINT('Ctrl Pts',(4.39615167350378,3.22065289637257,14.8983069065414));
#47832=CARTESIAN_POINT('Ctrl Pts',(4.25724018301514,0.388053261093601,13.9792614933621));
#47833=CARTESIAN_POINT('Ctrl Pts',(4.1183286925265,-2.53908952801089,14.5270755653402));
#47834=CARTESIAN_POINT('Ctrl Pts',(3.97941720203786,-4.84762256455593,16.4082827268317));
#47835=CARTESIAN_POINT('Ctrl Pts',(3.84050571154924,-5.97510760649766,19.1645560524418));
#47836=CARTESIAN_POINT('Ctrl Pts',(3.70159422106059,-5.64685042383923,22.1243723283741));
#47837=CARTESIAN_POINT('Ctrl Pts',(3.56268273057196,-3.94282578401499,24.5666182603398));
#47838=CARTESIAN_POINT('Ctrl Pts',(3.42377124008332,-1.27819284122356,25.896278534746));
#47839=CARTESIAN_POINT('Ctrl Pts',(3.28485974959469,1.6978519476731,25.7894020643622));
#47840=CARTESIAN_POINT('Ctrl Pts',(3.14594825910605,4.26024146295097,24.272027642166));
#47841=CARTESIAN_POINT('Ctrl Pts',(3.00703676861741,5.78468927206021,21.7138399941772));
#47842=CARTESIAN_POINT('Ctrl Pts',(2.86812527812878,5.89978732780536,18.7381018329537));
#47843=CARTESIAN_POINT('Ctrl Pts',(2.72921378764015,4.57749377640302,16.0698055740032));
#47844=CARTESIAN_POINT('Ctrl Pts',(2.59030229715151,2.13996491549558,14.3590401824333));
#47845=CARTESIAN_POINT('Ctrl Pts',(2.45139080666287,-0.818933178687291,
14.0226070957675));
#47846=CARTESIAN_POINT('Ctrl Pts',(2.31247931617423,-3.57831092008871,15.1424730060344));
#47847=CARTESIAN_POINT('Ctrl Pts',(2.1735678256856,-5.46588873739256,17.4457999812319));
#47848=CARTESIAN_POINT('Ctrl Pts',(2.03465633519696,-6.02178762295823,20.3714181261455));
#47849=CARTESIAN_POINT('Ctrl Pts',(1.89574484470832,-5.11057138435912,23.2065460478256));
#47850=CARTESIAN_POINT('Ctrl Pts',(1.75683335421969,-2.95424382766933,25.2604487207597));
#47851=CARTESIAN_POINT('Ctrl Pts',(1.61792186373105,-0.0781604693793413,
26.0327248619724));
#47852=CARTESIAN_POINT('Ctrl Pts',(1.47901037324242,2.81696518293041,25.3352209369218));
#47853=CARTESIAN_POINT('Ctrl Pts',(1.34009888275377,5.02578156596024,23.3378738167095));
#47854=CARTESIAN_POINT('Ctrl Pts',(1.20118739226514,6.01014314938957,20.527304418837));
#47855=CARTESIAN_POINT('Ctrl Pts',(1.0622759017765,5.53022886704606,17.5882677129498));
#47856=CARTESIAN_POINT('Ctrl Pts',(0.923364411287864,3.7029557770085,15.2368077542205));
#47857=CARTESIAN_POINT('Ctrl Pts',(0.784452920799229,0.973523620615991,
14.0458343013086));
#47858=CARTESIAN_POINT('Ctrl Pts',(0.645541430310594,-1.99310945899281,
14.3054838683065));
#47859=CARTESIAN_POINT('Ctrl Pts',(0.506629939821949,-4.47411886205269,
15.9525474555556));
#47860=CARTESIAN_POINT('Ctrl Pts',(0.367718449333321,-5.86514463181102,
18.5856439254866));
#47861=CARTESIAN_POINT('Ctrl Pts',(0.228806958844683,-5.82708887344388,
21.5634566994412));
#47862=CARTESIAN_POINT('Ctrl Pts',(0.089895468356049,-4.36961084196237,
24.1600984966641));
#47863=CARTESIAN_POINT('Ctrl Pts',(-0.049016022132584,-1.8470232551417,
25.7437316612543));
#47864=CARTESIAN_POINT('Ctrl Pts',(-0.141623682458342,0.133898761891108,
25.8656596766911));
#47865=CARTESIAN_POINT('Ctrl Pts',(-0.187927512621222,1.07922963693981,
25.6862389549904));
#47866=CARTESIAN_POINT('Ctrl Pts',(50.5637825378637,4.61752854196214,24.0062770406782));
#47867=CARTESIAN_POINT('Ctrl Pts',(50.5174787077008,5.28356762518215,23.2386180781043));
#47868=CARTESIAN_POINT('Ctrl Pts',(50.424871047375,6.22471038456146,21.3654729984245));
#47869=CARTESIAN_POINT('Ctrl Pts',(50.2859595568864,6.11925893083018,18.221252859719));
#47870=CARTESIAN_POINT('Ctrl Pts',(50.1470480663978,4.52315605456026,15.511157237809));
#47871=CARTESIAN_POINT('Ctrl Pts',(50.0081365759091,1.82495675592641,13.894325809954));
#47872=CARTESIAN_POINT('Ctrl Pts',(49.8692250854205,-1.31781499742106,13.7652351533052));
#47873=CARTESIAN_POINT('Ctrl Pts',(49.7303135949318,-4.13954687382562,15.1550528216166));
#47874=CARTESIAN_POINT('Ctrl Pts',(49.5914021044433,-5.95272957145251,17.7253150705105));
#47875=CARTESIAN_POINT('Ctrl Pts',(49.4524906139545,-6.31562862148528,20.849744422951));
#47876=CARTESIAN_POINT('Ctrl Pts',(49.313579123466,-5.13981947893865,23.7671592113954));
#47877=CARTESIAN_POINT('Ctrl Pts',(49.1746676329772,-2.71177477849166,25.7667577971016));
#47878=CARTESIAN_POINT('Ctrl Pts',(49.0357561424887,0.376952608096762,26.3613785707909));
#47879=CARTESIAN_POINT('Ctrl Pts',(48.896844652,3.37384090977041,25.4061465625371));
#47880=CARTESIAN_POINT('Ctrl Pts',(48.7579331615114,5.54874546123675,23.1337916855913));
#47881=CARTESIAN_POINT('Ctrl Pts',(48.6190216710227,6.37178419535544,20.0979366854017));
#47882=CARTESIAN_POINT('Ctrl Pts',(48.4801101805342,5.64243666772738,17.0382211455748));
#47883=CARTESIAN_POINT('Ctrl Pts',(48.3411986900455,3.53839699735355,14.7000969433883));
#47884=CARTESIAN_POINT('Ctrl Pts',(48.2022871995569,0.572281835046422,13.653211912598));
#47885=CARTESIAN_POINT('Ctrl Pts',(48.0633757090682,-2.53326092100598,14.1526232585264));
#47886=CARTESIAN_POINT('Ctrl Pts',(47.9244642185796,-5.02161397036119,16.0766572005871));
#47887=CARTESIAN_POINT('Ctrl Pts',(47.7855527280909,-6.28652872164122,18.9565527116423));
#47888=CARTESIAN_POINT('Ctrl Pts',(47.6466412376024,-6.01982832642006,22.0906679621073));
#47889=CARTESIAN_POINT('Ctrl Pts',(47.5077297471136,-4.28649019781716,24.71542441243));
#47890=CARTESIAN_POINT('Ctrl Pts',(47.3688182566251,-1.50881526580176,26.1913408969229));
#47891=CARTESIAN_POINT('Ctrl Pts',(47.2299067661364,1.63645908624929,26.1588332714235));
#47892=CARTESIAN_POINT('Ctrl Pts',(47.0909952756477,4.38303558259688,24.6258215150332));
#47893=CARTESIAN_POINT('Ctrl Pts',(46.9520837851591,6.06175349129441,21.9658001469101));
#47894=CARTESIAN_POINT('Ctrl Pts',(46.8131722946704,6.26361925046179,18.8268420855787));
#47895=CARTESIAN_POINT('Ctrl Pts',(46.6742608041818,4.93945140114888,15.9737057406808));
#47896=CARTESIAN_POINT('Ctrl Pts',(46.5353493136932,2.41186288654182,14.1015134972249));
#47897=CARTESIAN_POINT('Ctrl Pts',(46.3964378232046,-0.703338584205735,
13.6663959357331));
#47898=CARTESIAN_POINT('Ctrl Pts',(46.257526332716,-3.64718252590797,14.7743626963189));
#47899=CARTESIAN_POINT('Ctrl Pts',(46.1186148422273,-5.70244705557887,17.1554748752666));
#47900=CARTESIAN_POINT('Ctrl Pts',(45.9797033517387,-6.36839887172476,20.2296114490435));
#47901=CARTESIAN_POINT('Ctrl Pts',(45.84079186125,-5.48278915103411,23.2478067572163));
#47902=CARTESIAN_POINT('Ctrl Pts',(45.7018803707614,-3.26138295580096,25.4747243604157));
#47903=CARTESIAN_POINT('Ctrl Pts',(45.5629688802727,-0.245391425534477,
26.3678103501275));
#47904=CARTESIAN_POINT('Ctrl Pts',(45.4240573897841,2.83038591667594,25.7094781871552));
#47905=CARTESIAN_POINT('Ctrl Pts',(45.2851458992955,5.21658366263703,23.6601202845843));
#47906=CARTESIAN_POINT('Ctrl Pts',(45.1462344088069,6.33184176934682,20.719030885896));
#47907=CARTESIAN_POINT('Ctrl Pts',(45.0073229183182,5.90444490978662,17.6027607724275));
#47908=CARTESIAN_POINT('Ctrl Pts',(44.8684114278296,4.03852169487032,15.0705407875732));
#47909=CARTESIAN_POINT('Ctrl Pts',(44.7294999373409,1.18867535364643,13.7393070263308));
#47910=CARTESIAN_POINT('Ctrl Pts',(44.5905884468523,-1.95077328725316,13.9333939316404));
#47911=CARTESIAN_POINT('Ctrl Pts',(44.4516769563636,-4.61494629599519,15.6055152415786));
#47912=CARTESIAN_POINT('Ctrl Pts',(44.3127654658751,-6.15475927144461,18.3482845531133));
#47913=CARTESIAN_POINT('Ctrl Pts',(44.1738539753864,-6.19506068261978,21.4934686958809));
#47914=CARTESIAN_POINT('Ctrl Pts',(44.0349424848978,-4.72603171623352,24.2747923720425));
#47915=CARTESIAN_POINT('Ctrl Pts',(43.8960309944091,-2.10557847814608,26.0146292387217));
#47916=CARTESIAN_POINT('Ctrl Pts',(43.7571195039205,1.02786627402308,26.2890950485458));
#47917=CARTESIAN_POINT('Ctrl Pts',(43.6182080134318,3.91088736273947,25.0313204671222));
#47918=CARTESIAN_POINT('Ctrl Pts',(43.4792965229432,5.84108144907249,22.5477427484381));
#47919=CARTESIAN_POINT('Ctrl Pts',(43.3403850324546,6.34818670374496,19.4434470543486));
#47920=CARTESIAN_POINT('Ctrl Pts',(43.2014735419659,5.30865480258217,16.4747468468295));
#47921=CARTESIAN_POINT('Ctrl Pts',(43.0625620514773,2.9757515580194,14.3649198522237));
#47922=CARTESIAN_POINT('Ctrl Pts',(42.9236505609886,-0.0821473649868688,
13.6279926697042));
#47923=CARTESIAN_POINT('Ctrl Pts',(42.7847390705,-3.12003235757933,14.4435061689429));
#47924=CARTESIAN_POINT('Ctrl Pts',(42.6458275800114,-5.39776989439614,16.6127731439911));
#47925=CARTESIAN_POINT('Ctrl Pts',(42.5069160895228,-6.36042457890855,19.6072853670493));
#47926=CARTESIAN_POINT('Ctrl Pts',(42.3680045990341,-5.77346053925448,22.6974764148346));
#47927=CARTESIAN_POINT('Ctrl Pts',(42.2290931085455,-3.77988245302682,25.1304692035152));
#47928=CARTESIAN_POINT('Ctrl Pts',(42.0901816180568,-0.865394677250782,
26.3135028042683));
#47929=CARTESIAN_POINT('Ctrl Pts',(41.9512701275682,2.25993307925686,25.9583494429412));
#47930=CARTESIAN_POINT('Ctrl Pts',(41.8123586370795,4.83466321896507,24.151536723444));
#47931=CARTESIAN_POINT('Ctrl Pts',(41.673447146591,6.23150270747516,21.3332665201104));
#47932=CARTESIAN_POINT('Ctrl Pts',(41.5345356561023,6.11013328470932,18.1901666236902));
#47933=CARTESIAN_POINT('Ctrl Pts',(41.3956241656137,4.5001247266669,15.4880045377507));
#47934=CARTESIAN_POINT('Ctrl Pts',(41.256712675125,1.79373062847491,13.8851201124316));
#47935=CARTESIAN_POINT('Ctrl Pts',(41.1178011846364,-1.34967809562946,13.7720312585004));
#47936=CARTESIAN_POINT('Ctrl Pts',(40.9788896941477,-4.16425870100727,15.1762903198884));
#47937=CARTESIAN_POINT('Ctrl Pts',(40.8399782036591,-5.96428231018196,17.7557713727501));
#47938=CARTESIAN_POINT('Ctrl Pts',(40.7010667131705,-6.31120111017131,20.8820238964393));
#47939=CARTESIAN_POINT('Ctrl Pts',(40.5621552226819,-5.12049372012104,23.793384988255));
#47940=CARTESIAN_POINT('Ctrl Pts',(40.4232437321932,-2.68225751383601,25.7805467073961));
#47941=CARTESIAN_POINT('Ctrl Pts',(40.2843322417046,0.409469102548303,26.3593679450851));
#47942=CARTESIAN_POINT('Ctrl Pts',(40.145420751216,3.4014349277457,25.388827891038));
#47943=CARTESIAN_POINT('Ctrl Pts',(40.0065092607273,5.56469392878752,23.1053835650098));
#47944=CARTESIAN_POINT('Ctrl Pts',(39.8675977702387,6.37220162748716,20.0653607341416));
#47945=CARTESIAN_POINT('Ctrl Pts',(39.72868627975,5.62722130693377,17.0094137749083));
#47946=CARTESIAN_POINT('Ctrl Pts',(39.5897747892614,3.51125585888291,14.6820767304917));
#47947=CARTESIAN_POINT('Ctrl Pts',(39.4508632987728,0.539827421410421,13.6503691475795));
#47948=CARTESIAN_POINT('Ctrl Pts',(39.3119518082841,-2.56312158825944,14.1656505649116));
#47949=CARTESIAN_POINT('Ctrl Pts',(39.1730403177955,-5.04160580690685,16.1023806631893));
#47950=CARTESIAN_POINT('Ctrl Pts',(39.0341288273068,-6.29178102490108,18.9887052152749));
#47951=CARTESIAN_POINT('Ctrl Pts',(38.8952173368182,-6.0090614551994,22.1214160446631));
#47952=CARTESIAN_POINT('Ctrl Pts',(38.7563058463296,-4.26232733267651,24.7372767827135));
#47953=CARTESIAN_POINT('Ctrl Pts',(38.6173943558409,-1.47714331403435,26.1989735631571));
#47954=CARTESIAN_POINT('Ctrl Pts',(38.4784828653523,1.66792374532418,26.1503866534309));
#47955=CARTESIAN_POINT('Ctrl Pts',(38.3395713748636,4.40662707311566,24.6033534999391));
#47956=CARTESIAN_POINT('Ctrl Pts',(38.200659884375,6.0717241128045,21.9347847179741));
#47957=CARTESIAN_POINT('Ctrl Pts',(38.0617483938864,6.25753981577645,18.7948356705868));
#47958=CARTESIAN_POINT('Ctrl Pts',(37.9228369033978,4.91880307017454,15.9485062058842));
#47959=CARTESIAN_POINT('Ctrl Pts',(37.7839254129091,2.3816763046193,14.0892603181216));
#47960=CARTESIAN_POINT('Ctrl Pts',(37.6450139224205,-0.735708924935337,
13.6700744092298));
#47961=CARTESIAN_POINT('Ctrl Pts',(37.5061024319318,-3.67385009436911,14.7930766194401));
#47962=CARTESIAN_POINT('Ctrl Pts',(37.3671909414432,-5.71691471264096,17.1846648911174));
#47963=CARTESIAN_POINT('Ctrl Pts',(37.2282794509546,-6.36714179730726,20.2621658633391));
#47964=CARTESIAN_POINT('Ctrl Pts',(37.0893679604659,-5.46611361180679,23.2757941922132));
#47965=CARTESIAN_POINT('Ctrl Pts',(36.9504564699773,-3.23335168806423,25.4913261119888));
#47966=CARTESIAN_POINT('Ctrl Pts',(36.8115449794887,-0.212833812579934,
26.3689816591933));
#47967=CARTESIAN_POINT('Ctrl Pts',(36.672633489,2.85953771780081,25.6949336824402));
#47968=CARTESIAN_POINT('Ctrl Pts',(36.5337219985114,5.23522726807311,23.6334035089075));
#47969=CARTESIAN_POINT('Ctrl Pts',(36.3948105080228,6.33543495400973,20.6866509669615));
#47970=CARTESIAN_POINT('Ctrl Pts',(36.2558990175341,5.8921122500055,17.572606574893));
#47971=CARTESIAN_POINT('Ctrl Pts',(36.1169875270455,4.01326785177723,15.0499589136242));
#47972=CARTESIAN_POINT('Ctrl Pts',(35.9780760365568,1.15665303412888,13.7333119300896));
#47973=CARTESIAN_POINT('Ctrl Pts',(35.8391645460682,-1.98176234208496,13.9434462252522));
#47974=CARTESIAN_POINT('Ctrl Pts',(35.7002530555796,-4.63735208393372,15.6291658397334));
#47975=CARTESIAN_POINT('Ctrl Pts',(35.5613415650909,-6.16312297003413,18.3797713546678));
#47976=CARTESIAN_POINT('Ctrl Pts',(35.4224300746023,-6.18734460651764,21.5251204303643));
#47977=CARTESIAN_POINT('Ctrl Pts',(35.2835185841137,-4.70411576761554,24.2988975856361));
#47978=CARTESIAN_POINT('Ctrl Pts',(35.144607093625,-2.07480213772069,26.025315070287));
#47979=CARTESIAN_POINT('Ctrl Pts',(35.0056956031364,1.06000482861184,26.2837580610839));
#47980=CARTESIAN_POINT('Ctrl Pts',(34.8667841126477,3.93655807151044,25.0112609347891));
#47981=CARTESIAN_POINT('Ctrl Pts',(34.7278726221591,5.85403004228618,22.5178478649292));
#47982=CARTESIAN_POINT('Ctrl Pts',(34.5889611316705,6.34525845764879,19.4110002440119));
#47983=CARTESIAN_POINT('Ctrl Pts',(34.4500496411818,5.29056313888617,16.4476532713745));
#47984=CARTESIAN_POINT('Ctrl Pts',(34.3111381506932,2.94690422977004,14.3497804407721));
#47985=CARTESIAN_POINT('Ctrl Pts',(34.1722266602045,-0.114722154020674,
13.6284959048672));
#47986=CARTESIAN_POINT('Ctrl Pts',(34.033315169716,-3.14839826566498,14.459529445284));
#47987=CARTESIAN_POINT('Ctrl Pts',(33.8944036792273,-5.41501600831516,16.6404126389379));
#47988=CARTESIAN_POINT('Ctrl Pts',(33.7554921887387,-6.36234915069327,19.6398071466696));
#47989=CARTESIAN_POINT('Ctrl Pts',(33.61658069825,-5.75959467686212,22.7269570523165));
#47990=CARTESIAN_POINT('Ctrl Pts',(33.4776692077614,-3.75360435860782,25.1497261991253));
#47991=CARTESIAN_POINT('Ctrl Pts',(33.3387577172728,-0.833106600630097,
26.3178444899273));
#47992=CARTESIAN_POINT('Ctrl Pts',(33.1998462267841,2.29036464937583,25.9467180343284));
#47993=CARTESIAN_POINT('Ctrl Pts',(33.0609347362955,4.855824102872,24.1267660327289));
#47994=CARTESIAN_POINT('Ctrl Pts',(32.9220232458069,6.2382373842586,21.301391541603));
#47995=CARTESIAN_POINT('Ctrl Pts',(32.7831117553182,6.10080095490451,18.1589532011506));
#47996=CARTESIAN_POINT('Ctrl Pts',(32.6442002648296,4.47699906757734,15.4650573370957));
#47997=CARTESIAN_POINT('Ctrl Pts',(32.5052887743409,1.76244584798862,13.8760298629218));
#47998=CARTESIAN_POINT('Ctrl Pts',(32.3663772838523,-1.38149994633938,13.779012658333));
#47999=CARTESIAN_POINT('Ctrl Pts',(32.2274657933637,-4.18886472194398,15.197642459357));
#48000=CARTESIAN_POINT('Ctrl Pts',(32.088554302875,-5.97567762627104,17.7862921344945));
#48001=CARTESIAN_POINT('Ctrl Pts',(31.9496428123864,-6.30660942952213,20.9142773705939));
#48002=CARTESIAN_POINT('Ctrl Pts',(31.8107313218978,-5.10103373445315,23.8195131164703));
#48003=CARTESIAN_POINT('Ctrl Pts',(31.6718198314091,-2.65267034660569,25.7941837767848));
#48004=CARTESIAN_POINT('Ctrl Pts',(31.5329083409205,0.441974997287937,26.357191495361));
#48005=CARTESIAN_POINT('Ctrl Pts',(31.3939968504318,3.4289399932875,25.3713681803941));
#48006=CARTESIAN_POINT('Ctrl Pts',(31.2550853599432,5.58049698283711,23.0768943809405));
#48007=CARTESIAN_POINT('Ctrl Pts',(31.1161738694545,6.37245250121533,20.0327830241454));
#48008=CARTESIAN_POINT('Ctrl Pts',(30.977262378966,5.6118588788506,16.9806845923648));
#48009=CARTESIAN_POINT('Ctrl Pts',(30.8383508884773,3.48402294614019,14.6641954948025));
#48010=CARTESIAN_POINT('Ctrl Pts',(30.6994393979887,0.507358900497252,13.6476923442733));
#48011=CARTESIAN_POINT('Ctrl Pts',(30.5605279075,-2.59291526618855,14.1788303555657));
#48012=CARTESIAN_POINT('Ctrl Pts',(30.4216164170114,-5.06146587467247,16.1282059963831));
#48013=CARTESIAN_POINT('Ctrl Pts',(30.2827049265227,-6.29686888525375,19.0208841494284));
#48014=CARTESIAN_POINT('Ctrl Pts',(30.1437934360341,-5.99813752993638,22.1521086819411));
#48015=CARTESIAN_POINT('Ctrl Pts',(30.0048819455455,-4.23805306663042,24.7590053384444));
#48016=CARTESIAN_POINT('Ctrl Pts',(29.8659704550568,-1.4454327553499,26.2064442120009));
#48017=CARTESIAN_POINT('Ctrl Pts',(29.7270589645682,1.69934481122473,26.1417792877538));
#48018=CARTESIAN_POINT('Ctrl Pts',(29.5881474740796,4.43010339123342,24.5807651707875));
#48019=CARTESIAN_POINT('Ctrl Pts',(29.4492359835909,6.08153604262198,21.9037187211369));
#48020=CARTESIAN_POINT('Ctrl Pts',(29.3103244931023,6.2512968328913,18.762860753997));
#48021=CARTESIAN_POINT('Ctrl Pts',(29.1714130026136,4.89802618046513,15.9234125616644));
#48022=CARTESIAN_POINT('Ctrl Pts',(29.032501512125,2.35142747477107,14.0771616231904));
#48023=CARTESIAN_POINT('Ctrl Pts',(28.8935900216364,-0.76806003704259,13.673918322815));
#48024=CARTESIAN_POINT('Ctrl Pts',(28.7546785311478,-3.70042164241411,14.8119266316608));
#48025=CARTESIAN_POINT('Ctrl Pts',(28.6157670406591,-5.73123295137762,17.2139284890799));
#48026=CARTESIAN_POINT('Ctrl Pts',(28.4768555501705,-6.36571831011055,20.29471342562));
#48027=CARTESIAN_POINT('Ctrl Pts',(28.3379440596818,-5.4492952092373,23.3036960104557));
#48028=CARTESIAN_POINT('Ctrl Pts',(28.1990325691932,-3.2052359128581,25.5077843412612));
#48029=CARTESIAN_POINT('Ctrl Pts',(28.0601210787046,-0.180270636962042,
26.3699865073929));
#48030=CARTESIAN_POINT('Ctrl Pts',(27.9212095882159,2.88861478152641,25.6802403339));
#48031=CARTESIAN_POINT('Ctrl Pts',(27.7822980977273,5.2537340446546,23.6065917699339));
#48032=CARTESIAN_POINT('Ctrl Pts',(27.6433866072386,6.33886255458932,20.6542531015921));
#48033=CARTESIAN_POINT('Ctrl Pts',(27.50447511675,5.87962559290408,17.5425158201557));
#48034=CARTESIAN_POINT('Ctrl Pts',(27.3655636262614,3.98790911718367,15.0295064148517));
#48035=CARTESIAN_POINT('Ctrl Pts',(27.2266521357728,1.12460048411671,13.7274806211505));
#48036=CARTESIAN_POINT('Ctrl Pts',(27.0877406452841,-2.01269960121476,13.953656814058));
#48037=CARTESIAN_POINT('Ctrl Pts',(26.9488291547955,-4.65963666919246,15.6529306748069));
#48038=CARTESIAN_POINT('Ctrl Pts',(26.8099176643068,-6.17132558811776,18.4113005028136));
#48039=CARTESIAN_POINT('Ctrl Pts',(26.6710061738182,-6.17946681684849,21.556732304022));
#48040=CARTESIAN_POINT('Ctrl Pts',(26.5320946833296,-4.68207687136995,24.3228904424587));
#48041=CARTESIAN_POINT('Ctrl Pts',(26.3931831928409,-2.04397156988813,26.0358434231188));
#48042=CARTESIAN_POINT('Ctrl Pts',(26.2542717023523,1.09211567872115,26.2782568401754));
#48043=CARTESIAN_POINT('Ctrl Pts',(26.1153602118636,3.96212589368178,24.9910704272264));
#48044=CARTESIAN_POINT('Ctrl Pts',(25.976448721375,5.86682563350311,22.4878871744893));
#48045=CARTESIAN_POINT('Ctrl Pts',(25.8375372308864,6.34216437072042,19.3785688278802));
#48046=CARTESIAN_POINT('Ctrl Pts',(25.6986257403977,5.27233320006711,16.4206525407014));
#48047=CARTESIAN_POINT('Ctrl Pts',(25.5597142499091,2.91797988069426,14.3347887044894));
#48048=CARTESIAN_POINT('Ctrl Pts',(25.4208027594205,-0.147293944655354,
13.6291656668231));
#48049=CARTESIAN_POINT('Ctrl Pts',(25.2818912689318,-3.17668188663938,14.4756975283739));
#48050=CARTESIAN_POINT('Ctrl Pts',(25.1429797784432,-5.43212059438828,16.6681399406727));
#48051=CARTESIAN_POINT('Ctrl Pts',(25.0040682879545,-6.3641074349603,19.672338340356));
#48052=CARTESIAN_POINT('Ctrl Pts',(24.8651567974659,-5.74557828065295,22.7563664175516));
#48053=CARTESIAN_POINT('Ctrl Pts',(24.7262453069773,-3.72722815930074,25.1688486005525));
#48054=CARTESIAN_POINT('Ctrl Pts',(24.5873338164887,-0.800796749783299,
26.3220210512505));
#48055=CARTESIAN_POINT('Ctrl Pts',(24.448422326,2.32073635810671,25.9349312012086));
#48056=CARTESIAN_POINT('Ctrl Pts',(24.3095108355114,4.87685807407465,24.1018874841042));
#48057=CARTESIAN_POINT('Ctrl Pts',(24.1705993450227,6.24480901733213,21.2694825496889));
#48058=CARTESIAN_POINT('Ctrl Pts',(24.0316878545341,6.09130917345336,18.1277878965458));
#48059=CARTESIAN_POINT('Ctrl Pts',(23.8927763640454,4.45375639682368,15.4422286625293));
#48060=CARTESIAN_POINT('Ctrl Pts',(23.7538648735569,1.73111500389623,13.8670996706124));
#48061=CARTESIAN_POINT('Ctrl Pts',(23.6149533830682,-1.41328568991475,13.7861566510251));
#48062=CARTESIAN_POINT('Ctrl Pts',(23.4760418925796,-4.21336126194841,15.2191201141181));
#48063=CARTESIAN_POINT('Ctrl Pts',(23.3371304020909,-5.98691676095991,17.8168707541113));
#48064=CARTESIAN_POINT('Ctrl Pts',(23.1982189116023,-6.30185291817879,20.9465069490283));
#48065=CARTESIAN_POINT('Ctrl Pts',(23.0593074211136,-5.08144042723737,23.8455414171941));
#48066=CARTESIAN_POINT('Ctrl Pts',(22.920395930625,-2.62301384869953,25.8076694083296));
#48067=CARTESIAN_POINT('Ctrl Pts',(22.7814844401364,0.474469340488402,26.3548488929206));
#48068=CARTESIAN_POINT('Ctrl Pts',(22.6425729496477,3.45635543942831,25.353768082692));
#48069=CARTESIAN_POINT('Ctrl Pts',(22.5036614591591,5.59615418399987,23.0483247785986));
#48070=CARTESIAN_POINT('Ctrl Pts',(22.3647499686705,6.37253682336279,20.0002044573261));
#48071=CARTESIAN_POINT('Ctrl Pts',(22.2258384781818,5.59634977820039,16.9520343231995));
#48072=CARTESIAN_POINT('Ctrl Pts',(22.0869269876932,3.45669897433838,14.6464537166729));
#48073=CARTESIAN_POINT('Ctrl Pts',(21.9480154972045,0.474877119159393,13.6451815660385));
#48074=CARTESIAN_POINT('Ctrl Pts',(21.8091040067159,-2.62264117521137,14.1921622893711));
#48075=CARTESIAN_POINT('Ctrl Pts',(21.6701925162273,-5.08119365504295,16.1541325234911));
#48076=CARTESIAN_POINT('Ctrl Pts',(21.5312810257387,-6.30179216949294,19.0530886739324));
#48077=CARTESIAN_POINT('Ctrl Pts',(21.39236953525,-5.98705683625699,22.1827450713141));
#48078=CARTESIAN_POINT('Ctrl Pts',(21.2534580447614,-4.21366803405649,24.7806095119438));
#48079=CARTESIAN_POINT('Ctrl Pts',(21.1145465542727,-1.41368441857138,26.2137526480868));
#48080=CARTESIAN_POINT('Ctrl Pts',(20.9756350637841,1.73072146273936,26.1330113994131));
#48081=CARTESIAN_POINT('Ctrl Pts',(20.8367235732955,4.453463923361,24.5580571179221));
#48082=CARTESIAN_POINT('Ctrl Pts',(20.6978120828068,6.09118902430437,21.8726029683601));
#48083=CARTESIAN_POINT('Ctrl Pts',(20.5589005923182,6.2448904649721,18.7309181715043));
#48084=CARTESIAN_POINT('Ctrl Pts',(20.4199891018296,4.87712127505025,15.8984254638773));
#48085=CARTESIAN_POINT('Ctrl Pts',(20.2810776113409,2.32111718758555,14.0652177286431));
#48086=CARTESIAN_POINT('Ctrl Pts',(20.1421661208523,-0.800391074992589,
13.6779275760247));
#48087=CARTESIAN_POINT('Ctrl Pts',(20.0032546303637,-3.72689647556414,14.8309122403131));
#48088=CARTESIAN_POINT('Ctrl Pts',(19.864343139875,-5.74540139756466,17.2432649043154));
#48089=CARTESIAN_POINT('Ctrl Pts',(19.7254316493864,-6.36412844733921,20.3272532852169));
#48090=CARTESIAN_POINT('Ctrl Pts',(19.5865201588977,-5.43233438289444,23.3315114826968));
#48091=CARTESIAN_POINT('Ctrl Pts',(19.4476086684091,-3.17703636502164,25.5240986180776));
#48092=CARTESIAN_POINT('Ctrl Pts',(19.3086971779205,-0.14770274975791,26.3708248684634));
#48093=CARTESIAN_POINT('Ctrl Pts',(19.1697856874318,2.91761634788927,25.6653985255625));
#48094=CARTESIAN_POINT('Ctrl Pts',(19.0308741969432,5.27210350868496,23.5796857684201));
#48095=CARTESIAN_POINT('Ctrl Pts',(18.8919627064546,6.34212448150116,20.6218381365444));
#48096=CARTESIAN_POINT('Ctrl Pts',(18.7530512159659,5.86698526483596,17.5124892946733));
#48097=CARTESIAN_POINT('Ctrl Pts',(18.6141397254773,3.96244615387019,15.0091838258059));
#48098=CARTESIAN_POINT('Ctrl Pts',(18.4752282349886,1.09251854134113,13.7218132519219));
#48099=CARTESIAN_POINT('Ctrl Pts',(18.3363167445,-2.0435842560608,13.9640254311919));
#48100=CARTESIAN_POINT('Ctrl Pts',(18.1974052540114,-4.68179946933745,15.6768091256771));
#48101=CARTESIAN_POINT('Ctrl Pts',(18.0584937635227,-6.17936691131037,18.4428711734991));
#48102=CARTESIAN_POINT('Ctrl Pts',(17.9195822730341,-6.17142751950771,21.5883034906404));
#48103=CARTESIAN_POINT('Ctrl Pts',(17.7806707825455,-4.65991560350942,24.3467703154281));
#48104=CARTESIAN_POINT('Ctrl Pts',(17.6417592920568,-2.01308758044197,26.0462140220462));
#48105=CARTESIAN_POINT('Ctrl Pts',(17.5028478015682,1.12419798509589,26.2725915296011));
#48106=CARTESIAN_POINT('Ctrl Pts',(17.3639363110796,3.98759016100821,24.9707494721368));
#48107=CARTESIAN_POINT('Ctrl Pts',(17.2250248205909,5.87946788829534,22.4578614601765));
#48108=CARTESIAN_POINT('Ctrl Pts',(17.0861133301023,6.33890452382744,19.3461536535871));
#48109=CARTESIAN_POINT('Ctrl Pts',(16.9472018396136,5.25396546258616,16.3937453605064));
#48110=CARTESIAN_POINT('Ctrl Pts',(16.808290349125,2.88897926676432,14.3199450352023));
#48111=CARTESIAN_POINT('Ctrl Pts',(16.6693788586364,-0.179861885588608,
13.630001938067));
#48112=CARTESIAN_POINT('Ctrl Pts',(16.5304673681478,-3.2048824812767,14.4920099956406));
#48113=CARTESIAN_POINT('Ctrl Pts',(16.3915558776591,-5.44908320556687,16.6959543245097));
#48114=CARTESIAN_POINT('Ctrl Pts',(16.2526443871705,-6.36569938575479,19.7048780978672));
#48115=CARTESIAN_POINT('Ctrl Pts',(16.1137328966818,-5.73141171696209,22.7857037418913));
#48116=CARTESIAN_POINT('Ctrl Pts',(15.9748214061932,-3.70075454447885,25.1878359080099));
#48117=CARTESIAN_POINT('Ctrl Pts',(15.8359099157046,-0.768465969166765,
26.3260323790785));
#48118=CARTESIAN_POINT('Ctrl Pts',(15.6969984252159,2.35104741164878,25.9229892516446));
#48119=CARTESIAN_POINT('Ctrl Pts',(15.5580869347273,4.89776458282526,24.0769017278002));
#48120=CARTESIAN_POINT('Ctrl Pts',(15.4191754442386,6.25121743493832,21.2375403783475));
#48121=CARTESIAN_POINT('Ctrl Pts',(15.28026395375,6.08165818843483,18.096671524418));
#48122=CARTESIAN_POINT('Ctrl Pts',(15.1413524632613,4.43039732188061,15.4195191107057));
#48123=CARTESIAN_POINT('Ctrl Pts',(15.0024409727728,1.69973891506645,13.8583297689044));
#48124=CARTESIAN_POINT('Ctrl Pts',(14.8635294822841,-1.44503449559759,13.7934630498602));
#48125=CARTESIAN_POINT('Ctrl Pts',(14.7246179917955,-4.23774768077446,15.2407227228278));
#48126=CARTESIAN_POINT('Ctrl Pts',(14.5857065013068,-5.99799942050051,17.8475064323922));
#48127=CARTESIAN_POINT('Ctrl Pts',(14.4467950108182,-6.29693170045833,20.9787117893846));
#48128=CARTESIAN_POINT('Ctrl Pts',(14.3078835203295,-5.06171431056786,23.8714692101462));
#48129=CARTESIAN_POINT('Ctrl Pts',(14.1689720298409,-2.59328879522498,25.8210032495677));
#48130=CARTESIAN_POINT('Ctrl Pts',(14.0300605393523,0.506951282871708,26.3523401989906));
#48131=CARTESIAN_POINT('Ctrl Pts',(13.8911490488636,3.48368054963307,25.3360280579309));
#48132=CARTESIAN_POINT('Ctrl Pts',(13.752237558375,5.6116651230563,23.0196755046844));
#48133=CARTESIAN_POINT('Ctrl Pts',(13.6133260678864,6.37245459172572,19.967625885163));
#48134=CARTESIAN_POINT('Ctrl Pts',(13.4744145773977,5.58069441033177,16.9234637162209));
#48135=CARTESIAN_POINT('Ctrl Pts',(13.3355030869091,3.42928465762181,14.6288518598053));
#48136=CARTESIAN_POINT('Ctrl Pts',(13.1965915964205,0.442382926346631,13.6428368784973));
#48137=CARTESIAN_POINT('Ctrl Pts',(13.0576801059318,-2.65229853840607,14.205646017882));
#48138=CARTESIAN_POINT('Ctrl Pts',(12.9187686154432,-5.10078863240939,16.1801595668928));
#48139=CARTESIAN_POINT('Ctrl Pts',(12.7798571249545,-6.30655074894272,19.0853179470835));
#48140=CARTESIAN_POINT('Ctrl Pts',(12.6409456344659,-5.97581966376832,22.2133244120638));
#48141=CARTESIAN_POINT('Ctrl Pts',(12.5020341439773,-4.1891728722864,24.8020887385612));
#48142=CARTESIAN_POINT('Ctrl Pts',(12.3631226534886,-1.38189913347912,26.2208986804004));
#48143=CARTESIAN_POINT('Ctrl Pts',(12.224211163,1.76205287980219,26.124083217568));
#48144=CARTESIAN_POINT('Ctrl Pts',(12.0852996725114,4.4767080589433,24.5352299348445));
#48145=CARTESIAN_POINT('Ctrl Pts',(11.9463881820227,6.1006828055596,21.8414382728907));
#48146=CARTESIAN_POINT('Ctrl Pts',(11.8074766915341,6.23832087945686,18.6990087579656));
#48147=CARTESIAN_POINT('Ctrl Pts',(11.6685652010455,4.85608890030431,15.8735455655904));
#48148=CARTESIAN_POINT('Ctrl Pts',(11.5296537105568,2.29074623525794,14.0534289466476));
#48149=CARTESIAN_POINT('Ctrl Pts',(11.3907422200682,-0.832701193775514,
13.6821020640721));
#48150=CARTESIAN_POINT('Ctrl Pts',(11.2518307295795,-3.75327390186831,14.8500329491858));
#48151=CARTESIAN_POINT('Ctrl Pts',(11.1129192390909,-5.75941968089301,17.272673370082));
#48152=CARTESIAN_POINT('Ctrl Pts',(10.9740077486023,-6.36237225054617,20.3597845916624));
#48153=CARTESIAN_POINT('Ctrl Pts',(10.8350962581136,-5.41523157606947,23.3592398819462));
#48154=CARTESIAN_POINT('Ctrl Pts',(10.696184767625,-3.14875378158332,25.5402685160452));
#48155=CARTESIAN_POINT('Ctrl Pts',(10.5572732771364,-0.115131002167762,
26.3714967204933));
#48156=CARTESIAN_POINT('Ctrl Pts',(10.4183617866477,2.94654165889923,25.6504086453361));
#48157=CARTESIAN_POINT('Ctrl Pts',(10.2794502961591,5.29033518005657,23.5526862075862));
#48158=CARTESIAN_POINT('Ctrl Pts',(10.1405388056704,6.34522064949098,20.5894069190218));
#48159=CARTESIAN_POINT('Ctrl Pts',(10.0016273151818,5.854191596171,17.4825277832241));
#48160=CARTESIAN_POINT('Ctrl Pts',(9.86271582469318,3.9368796273414,14.9889916776419));
#48161=CARTESIAN_POINT('Ctrl Pts',(9.72380433420454,1.06040804430175,13.716309970527));
#48162=CARTESIAN_POINT('Ctrl Pts',(9.58489284371591,-2.07441549941601,13.974551805658));
#48163=CARTESIAN_POINT('Ctrl Pts',(9.44598135322726,-4.70383990511773,15.7008005682523));
#48164=CARTESIAN_POINT('Ctrl Pts',(9.30706986273865,-6.18724672944247,18.4744825415877));
#48165=CARTESIAN_POINT('Ctrl Pts',(9.16815837224999,-6.16322692461181,21.6198331650691));
#48166=CARTESIAN_POINT('Ctrl Pts',(9.02924688176137,-4.63763254324486,24.3705365804159));
#48167=CARTESIAN_POINT('Ctrl Pts',(8.89033539127272,-1.98215097657166,26.0564265960212));
#48168=CARTESIAN_POINT('Ctrl Pts',(8.7514239007841,1.15625090922707,26.2667622774308));
#48169=CARTESIAN_POINT('Ctrl Pts',(8.61251241029546,4.01295020795098,24.9502986006324));
#48170=CARTESIAN_POINT('Ctrl Pts',(8.47360091980683,5.8919564762427,22.4277715067483));
#48171=CARTESIAN_POINT('Ctrl Pts',(8.33468942931819,6.33547900216983,19.3137555683411));
#48172=CARTESIAN_POINT('Ctrl Pts',(8.19577793882954,5.23546040650557,16.3669324340401));
#48173=CARTESIAN_POINT('Ctrl Pts',(8.05686644834092,2.85990314594527,14.3052498208675));
#48174=CARTESIAN_POINT('Ctrl Pts',(7.91795495785227,-0.212425125618811,
13.6310046967419));
#48175=CARTESIAN_POINT('Ctrl Pts',(7.77904346736364,-3.23299931252101,14.5084664207386));
#48176=CARTESIAN_POINT('Ctrl Pts',(7.64013197687499,-5.46590339851313,16.7238550634869));
#48177=CARTESIAN_POINT('Ctrl Pts',(7.50122048638637,-6.3671249614693,19.7374255687385));
#48178=CARTESIAN_POINT('Ctrl Pts',(7.36230899589772,-5.71709535604924,22.8149682585701));
#48179=CARTESIAN_POINT('Ctrl Pts',(7.2233975054091,-3.67418420606118,25.206687625242));
#48180=CARTESIAN_POINT('Ctrl Pts',(7.08448601492046,-0.73611510378342,26.3298783685707));
#48181=CARTESIAN_POINT('Ctrl Pts',(6.94557452443182,2.38129701778703,25.9108924977533));
#48182=CARTESIAN_POINT('Ctrl Pts',(6.80666303394318,4.91854308270761,24.0518094168491));
#48183=CARTESIAN_POINT('Ctrl Pts',(6.66775154345454,6.2574624695857,21.2055658624248));
#48184=CARTESIAN_POINT('Ctrl Pts',(6.5288400529659,6.07184825208871,18.0656048980302));
#48185=CARTESIAN_POINT('Ctrl Pts',(6.38992856247727,4.40692245326515,15.3969292751659));
#48186=CARTESIAN_POINT('Ctrl Pts',(6.25101707198863,1.66831840155036,13.8497203870096));
#48187=CARTESIAN_POINT('Ctrl Pts',(6.11210558150001,-1.47674553359532,13.8009316638769));
#48188=CARTESIAN_POINT('Ctrl Pts',(5.97319409101137,-4.26202334105436,15.2624497208763));
#48189=CARTESIAN_POINT('Ctrl Pts',(5.83428260052273,-6.0089253152344,17.8781983686375));
#48190=CARTESIAN_POINT('Ctrl Pts',(5.6953711100341,-6.29184590498261,21.0108910499511));
#48191=CARTESIAN_POINT('Ctrl Pts',(5.55645961954546,-5.04185590001004,23.897295817673));
#48192=CARTESIAN_POINT('Ctrl Pts',(5.41754812905682,-2.56349596308158,25.8341849520033));
#48193=CARTESIAN_POINT('Ctrl Pts',(5.27863663856818,0.539419975483812,26.3496654791388));
#48194=CARTESIAN_POINT('Ctrl Pts',(5.13972514807955,3.51091460972764,25.3181485697674));
#48195=CARTESIAN_POINT('Ctrl Pts',(5.00081365759091,5.62702939460967,22.9909473079805));
#48196=CARTESIAN_POINT('Ctrl Pts',(4.86190216710228,6.37220580845331,19.9350481591359));
#48197=CARTESIAN_POINT('Ctrl Pts',(4.72299067661364,5.56489318441634,16.8949735181558));
#48198=CARTESIAN_POINT('Ctrl Pts',(4.584079186125,3.40178071249615,14.6113903842451));
#48199=CARTESIAN_POINT('Ctrl Pts',(4.44516769563636,0.409877171332637,13.6406583429304));
#48200=CARTESIAN_POINT('Ctrl Pts',(4.30625620514773,-2.68188658064232,14.2192811886858));
#48201=CARTESIAN_POINT('Ctrl Pts',(4.16734471465908,-5.12025029463462,16.2062864463399));
#48202=CARTESIAN_POINT('Ctrl Pts',(4.02843322417046,-6.31114449923059,19.1175711265328));
#48203=CARTESIAN_POINT('Ctrl Pts',(3.88952173368181,-5.96442630616995,22.24384590496));
#48204=CARTESIAN_POINT('Ctrl Pts',(3.75061024319318,-4.16456822152471,24.8234424569172));
#48205=CARTESIAN_POINT('Ctrl Pts',(3.61169875270454,-1.35007773082975,26.2278821221607));
#48206=CARTESIAN_POINT('Ctrl Pts',(3.47278726221591,1.79333824355105,26.1149949755885));
#48207=CARTESIAN_POINT('Ctrl Pts',(3.33387577172728,4.49983519042547,24.5122842181282));
#48208=CARTESIAN_POINT('Ctrl Pts',(3.19496428123863,6.11001713833909,21.8102254493376));
#48209=CARTESIAN_POINT('Ctrl Pts',(3.05605279075,6.23158824788668,18.6671333472082));
#48210=CARTESIAN_POINT('Ctrl Pts',(2.91714130026136,4.83492960625386,15.8487735173902));
#48211=CARTESIAN_POINT('Ctrl Pts',(2.77822980977273,2.26031541093747,14.041795584685));
#48212=CARTESIAN_POINT('Ctrl Pts',(2.63931831928409,-0.864989547684349,
13.6864416790982));
#48213=CARTESIAN_POINT('Ctrl Pts',(2.50040682879546,-3.77955323437126,14.8692882560822));
#48214=CARTESIAN_POINT('Ctrl Pts',(2.36149533830682,-5.7732874301525,17.3021531225892));
#48215=CARTESIAN_POINT('Ctrl Pts',(2.22258384781818,-6.36044977513704,20.3923064851901));
#48216=CARTESIAN_POINT('Ctrl Pts',(2.08367235732954,-5.39798721704175,23.3868805022452));
#48217=CARTESIAN_POINT('Ctrl Pts',(1.94476086684091,-3.12038893862028,25.556293575601));
#48218=CARTESIAN_POINT('Ctrl Pts',(1.80584937635227,-0.0825561728535726,
26.3720021186908));
#48219=CARTESIAN_POINT('Ctrl Pts',(1.66693788586364,2.97538981548086,25.6352709416678));
#48220=CARTESIAN_POINT('Ctrl Pts',(1.528026395375,5.30842886408474,23.5255940754177));
#48221=CARTESIAN_POINT('Ctrl Pts',(1.38911490488636,6.34815042253135,20.5569597405651));
#48222=CARTESIAN_POINT('Ctrl Pts',(1.25020341439772,5.84124601468089,17.4526331642158));
#48223=CARTESIAN_POINT('Ctrl Pts',(1.11129192390908,3.91120805214414,14.9689283406313));
#48224=CARTESIAN_POINT('Ctrl Pts',(0.972380433420452,1.02827407433471,13.7109751703986));
#48225=CARTESIAN_POINT('Ctrl Pts',(0.833468942931815,-2.10520088120389,
13.985227291767));
#48226=CARTESIAN_POINT('Ctrl Pts',(0.694557452443171,-4.72574094137507,
15.7249208643558));
#48227=CARTESIAN_POINT('Ctrl Pts',(0.555645961954543,-6.19499726498531,
18.5061012876301));
#48228=CARTESIAN_POINT('Ctrl Pts',(0.416734471465905,-6.15480127088778,
21.6513846776137));
#48229=CARTESIAN_POINT('Ctrl Pts',(0.277822980977271,-4.61535544548857,
24.3940602366606));
#48230=CARTESIAN_POINT('Ctrl Pts',(0.138911490488638,-1.95089886648438,
26.0667560931559));
#48231=CARTESIAN_POINT('Ctrl Pts',(0.0463038301628798,0.141429157467205,
26.1955412757171));
#48232=CARTESIAN_POINT('Ctrl Pts',(0.,1.1399249411295,26.0060300274883));
#48233=CARTESIAN_POINT('Ctrl Pts',(0.,1.1399249411295,26.0060300274883));
#48234=CARTESIAN_POINT('Ctrl Pts',(-4.24882758481919E-16,0.972331625605204,
26.024339235968));
#48235=CARTESIAN_POINT('Ctrl Pts',(-9.68713354198481E-15,0.804333349730088,
26.0355246893388));
#48236=CARTESIAN_POINT('Ctrl Pts',(-7.21644966006352E-15,0.636361653837589,
26.0397009622082));
#48237=CARTESIAN_POINT('Ctrl Pts',(-4.72622945714007E-15,0.467061763353201,
26.0439102579212));
#48238=CARTESIAN_POINT('Ctrl Pts',(7.46066107244459E-15,0.297788121924876,
26.0409989699337));
#48239=CARTESIAN_POINT('Ctrl Pts',(6.88338275267597E-15,0.128984633759083,
26.0310315656805));
#48240=CARTESIAN_POINT('Ctrl Pts',(6.30997977578734E-15,-0.038685655092656,
26.0211310738815));
#48241=CARTESIAN_POINT('Ctrl Pts',(-8.19789119918948E-15,-0.205892792351831,
26.0042686578037));
#48242=CARTESIAN_POINT('Ctrl Pts',(-7.105427357601E-15,-0.372188805166806,
25.9804583393351));
#48243=CARTESIAN_POINT('Ctrl Pts',(-6.02607596443286E-15,-0.536488827077978,
25.9569338075084));
#48244=CARTESIAN_POINT('Ctrl Pts',(1.21781657491819E-14,-0.699900099394016,
25.9266269150383));
#48245=CARTESIAN_POINT('Ctrl Pts',(1.3988810110277E-14,-0.861967977673184,
25.8895065880249));
#48246=CARTESIAN_POINT('Ctrl Pts',(1.48816567000726E-14,-0.941885246655507,
25.8712021887192));
#48247=CARTESIAN_POINT('Ctrl Pts',(-8.6069672340652E-15,-1.02147545165873,
25.8512403873111));
#48248=CARTESIAN_POINT('Ctrl Pts',(-8.60422844084496E-15,-1.10068130521252,
25.8296136588393));
#48249=CARTESIAN_POINT('Ctrl Pts',(-8.60343716793459E-15,-1.12356490438221,
25.8233654162727));
#48250=CARTESIAN_POINT('Ctrl Pts',(1.17899233680487E-14,-1.14641640818171,
25.8169781854097));
#48251=CARTESIAN_POINT('Ctrl Pts',(1.21569421196455E-14,-1.16923440163958,
25.8104517468483));
#48252=CARTESIAN_POINT('Ctrl Pts',(1.24890717527468E-14,-1.18988329699519,
25.8045457171552));
#48253=CARTESIAN_POINT('Ctrl Pts',(-4.94407272871347E-15,-1.21049718097962,
25.7985278328021));
#48254=CARTESIAN_POINT('Ctrl Pts',(-4.94049245958195E-15,-1.23107002624393,
25.7923997285709));
#48255=CARTESIAN_POINT('Ctrl Pts',(-4.91294908986661E-15,-1.38933898938462,
25.7452556077536));
#48256=CARTESIAN_POINT('Ctrl Pts',(-6.72206345910563E-15,-1.54527720466299,
25.6915646759272));
#48257=CARTESIAN_POINT('Ctrl Pts',(-5.71764857681956E-15,-1.69847023449156,
25.6313756857849));
#48258=CARTESIAN_POINT('Ctrl Pts',(-5.49877947596065E-15,-1.73185207827719,
25.6182600794887));
#48259=CARTESIAN_POINT('Ctrl Pts',(1.85007413129516E-16,-1.76510349913815,
25.6048357400391));
#48260=CARTESIAN_POINT('Ctrl Pts',(4.44089209850063E-16,-1.79822007618261,
25.5911028699638));
#48261=CARTESIAN_POINT('Ctrl Pts',(1.63842330494031E-15,-1.95076548408182,
25.5278449352909));
#48262=CARTESIAN_POINT('Ctrl Pts',(7.40213603062554E-15,-2.10045211587673,
25.45804398787));
#48263=CARTESIAN_POINT('Ctrl Pts',(8.27116153345742E-15,-2.24691457271093,
25.3819733194664));
#48264=CARTESIAN_POINT('Ctrl Pts',(9.13853574229822E-15,-2.39309872634908,
25.3060471980723));
#48265=CARTESIAN_POINT('Ctrl Pts',(-3.10245225034387E-15,-2.53607151765369,
25.2238746247319));
#48266=CARTESIAN_POINT('Ctrl Pts',(-5.05151476204446E-15,-2.67543507353407,
25.1356889048841));
#48267=CARTESIAN_POINT('Ctrl Pts',(-6.91182822640314E-15,-2.80845281816195,
25.0515186532825));
#48268=CARTESIAN_POINT('Ctrl Pts',(2.53114930940398E-15,-2.9381827322964,
24.9618697543865));
#48269=CARTESIAN_POINT('Ctrl Pts',(3.88578058618805E-15,-3.064242236503,
24.866918929929));
#48270=CARTESIAN_POINT('Ctrl Pts',(4.27484187305284E-15,-3.10044756688972,
24.8396482692071));
#48271=CARTESIAN_POINT('Ctrl Pts',(-4.44149303582884E-16,-3.13634988015047,
24.8119401207576));
#48272=CARTESIAN_POINT('Ctrl Pts',(-8.88178419700125E-16,-3.17193948309244,
24.7837983555989));
#48273=CARTESIAN_POINT('Ctrl Pts',(-1.0931195317057E-15,-3.18836582212746,
24.770809557261));
#48274=CARTESIAN_POINT('Ctrl Pts',(7.56942218681223E-15,-3.20471920206644,
24.757733375776));
#48275=CARTESIAN_POINT('Ctrl Pts',(7.27196081129478E-15,-3.22099520798022,
24.7445733686326));
#48276=CARTESIAN_POINT('Ctrl Pts',(4.97510987807207E-15,-3.34667054753367,
24.6429582441954));
#48277=CARTESIAN_POINT('Ctrl Pts',(-7.27529725750927E-15,-3.46780653688132,
24.536292406256));
#48278=CARTESIAN_POINT('Ctrl Pts',(-8.32667268468867E-15,-3.58406520205367,
24.4248373445186));
#48279=CARTESIAN_POINT('Ctrl Pts',(-9.36930803468661E-15,-3.69935740968825,
24.3143088079944));
#48280=CARTESIAN_POINT('Ctrl Pts',(-7.79923338847808E-15,-3.8098535192748,
24.1990697852018));
#48281=CARTESIAN_POINT('Ctrl Pts',(-4.55191440096314E-15,-3.91518516086881,
24.0793423741378));
#48282=CARTESIAN_POINT('Ctrl Pts',(-2.81924743660761E-15,-3.97138680178951,
24.0154596047899));
#48283=CARTESIAN_POINT('Ctrl Pts',(-9.87932414299166E-15,-4.02611744048476,
23.9502985023543));
#48284=CARTESIAN_POINT('Ctrl Pts',(-9.76996261670138E-15,-4.07931584475367,
23.8838897354569));
#48285=CARTESIAN_POINT('Ctrl Pts',(-9.55902562552653E-15,-4.17974198312324,
23.7585255237847));
#48286=CARTESIAN_POINT('Ctrl Pts',(-1.21509664281812E-14,-4.27471073087482,
23.628715679372));
#48287=CARTESIAN_POINT('Ctrl Pts',(-1.31006316905768E-14,-4.36398437993495,
23.4948506002188));
#48288=CARTESIAN_POINT('Ctrl Pts',(-1.36609359328008E-14,-4.41665599620636,
23.4158699586126));
#48289=CARTESIAN_POINT('Ctrl Pts',(7.87054257710942E-15,-4.46734420575991,
23.3354773858304));
#48290=CARTESIAN_POINT('Ctrl Pts',(7.49400541621981E-15,-4.51599174705983,
23.2537516282698));
#48291=CARTESIAN_POINT('Ctrl Pts',(7.35114473953617E-15,-4.53444894435924,
23.2227443380464));
#48292=CARTESIAN_POINT('Ctrl Pts',(-7.55359812461929E-15,-4.55261232233179,
23.1915451316209));
#48293=CARTESIAN_POINT('Ctrl Pts',(-8.02136135291676E-15,-4.57047850650274,
23.1601583000966));
#48294=CARTESIAN_POINT('Ctrl Pts',(-8.37371801685389E-15,-4.58393674492536,
23.1365152290332));
#48295=CARTESIAN_POINT('Ctrl Pts',(1.01309155042277E-14,-4.59722854667126,
23.1127615325227));
#48296=CARTESIAN_POINT('Ctrl Pts',(1.00475183728577E-14,-4.61033840937547,
23.0889249821437));
#48297=CARTESIAN_POINT('Ctrl Pts',(9.56418682075062E-15,-4.68631716529486,
22.9507792605549));
#48298=CARTESIAN_POINT('Ctrl Pts',(2.3597456518294E-14,-4.75627611708813,
22.8097036647301));
#48299=CARTESIAN_POINT('Ctrl Pts',(2.0344836926256E-14,-4.82005887673718,
22.6660968272704));
#48300=CARTESIAN_POINT('Ctrl Pts',(1.71010815115263E-14,-4.88366781289573,
22.5228813532745));
#48301=CARTESIAN_POINT('Ctrl Pts',(1.36041559436968E-15,-4.94113438033816,
22.3771476702801));
#48302=CARTESIAN_POINT('Ctrl Pts',(1.11022302462516E-15,-4.99225431533367,
22.2292753801568));
#48303=CARTESIAN_POINT('Ctrl Pts',(8.64348697063786E-16,-5.04249193691787,
22.08395531755));
#48304=CARTESIAN_POINT('Ctrl Pts',(-1.64081607249733E-14,-5.08660018806323,
21.9365691476464));
#48305=CARTESIAN_POINT('Ctrl Pts',(-1.94566585065559E-14,-5.12433580930953,
21.7874725054075));
#48306=CARTESIAN_POINT('Ctrl Pts',(-2.2091841268231E-14,-5.15695523885615,
21.6585903707951));
#48307=CARTESIAN_POINT('Ctrl Pts',(-7.63174605915859E-15,-5.18481220829848,
21.5284298183699));
#48308=CARTESIAN_POINT('Ctrl Pts',(-7.52176099183544E-15,-5.20771827252021,
21.3972234452764));
#48309=CARTESIAN_POINT('Ctrl Pts',(-7.50414181272803E-15,-5.21716825578637,
21.3430937607464));
#48310=CARTESIAN_POINT('Ctrl Pts',(-4.48361323931463E-15,-5.22577522782904,
21.2887861341176));
#48311=CARTESIAN_POINT('Ctrl Pts',(-4.30211422042248E-15,-5.2335367160805,
21.2343205788571));
#48312=CARTESIAN_POINT('Ctrl Pts',(-4.19823060416723E-15,-5.23797911732325,
21.2031464222344));
#48313=CARTESIAN_POINT('Ctrl Pts',(-1.42660523996842E-14,-5.24214452334437,
21.1719205330544));
#48314=CARTESIAN_POINT('Ctrl Pts',(-1.46271883494364E-14,-5.24603236151472,
21.1406467100027));
#48315=CARTESIAN_POINT('Ctrl Pts',(-1.48771345015575E-14,-5.24872317695809,
21.1190017540263));
#48316=CARTESIAN_POINT('Ctrl Pts',(-6.99848150814512E-16,-5.2512806964718,
21.0973361625274));
#48317=CARTESIAN_POINT('Ctrl Pts',(-1.16573417585641E-15,-5.25370371263287,
21.0756621094304));
#48318=CARTESIAN_POINT('Ctrl Pts',(-4.46481939510917E-15,-5.27086185083263,
20.9221813343688));
#48319=CARTESIAN_POINT('Ctrl Pts',(-7.07482054458005E-15,-5.28129916922496,
20.7681211137086));
#48320=CARTESIAN_POINT('Ctrl Pts',(-4.09394740330526E-15,-5.28504682504941,
20.6139250846838));
#48321=CARTESIAN_POINT('Ctrl Pts',(-1.11160171993656E-15,-5.28879633220422,
20.4596528832985));
#48322=CARTESIAN_POINT('Ctrl Pts',(6.57889777690792E-15,-5.28584942273906,
20.305243947736));
#48323=CARTESIAN_POINT('Ctrl Pts',(9.49240686054509E-15,-5.27618637882583,
20.1511539648283));
#48324=CARTESIAN_POINT('Ctrl Pts',(1.0584972766909E-14,-5.27256273735838,
20.093370221238));
#48325=CARTESIAN_POINT('Ctrl Pts',(-8.75513436052681E-15,-5.26799413779765,
20.0356315059054));
#48326=CARTESIAN_POINT('Ctrl Pts',(-9.64506252643105E-15,-5.26247775735231,
19.9779626095996));
#48327=CARTESIAN_POINT('Ctrl Pts',(-1.01099037057859E-14,-5.25959635535805,
19.9478400909538));
#48328=CARTESIAN_POINT('Ctrl Pts',(-4.21799155701331E-16,-5.25645635018643,
19.9177366294551));
#48329=CARTESIAN_POINT('Ctrl Pts',(-1.33226762955019E-15,-5.25305723633443,
19.887655815811));
#48330=CARTESIAN_POINT('Ctrl Pts',(-2.13988741696045E-15,-5.25004209447572,
19.8609730024922));
#48331=CARTESIAN_POINT('Ctrl Pts',(-1.97866480786439E-17,-5.24682284854293,
19.8343067979969));
#48332=CARTESIAN_POINT('Ctrl Pts',(2.77555756156289E-17,-5.24340155368231,
19.8076771713483));
#48333=CARTESIAN_POINT('Ctrl Pts',(2.95714117697871E-16,-5.22411837524327,
19.6575866753963));
#48334=CARTESIAN_POINT('Ctrl Pts',(-1.67002099626319E-14,-5.19840717094589,
19.5085293113512));
#48335=CARTESIAN_POINT('Ctrl Pts',(-1.40998324127395E-14,-5.16626585321672,
19.3609354592565));
#48336=CARTESIAN_POINT('Ctrl Pts',(-1.15393273258269E-14,-5.13461736911524,
19.2156047133035));
#48337=CARTESIAN_POINT('Ctrl Pts',(-3.45941278228998E-15,-5.09673418838306,
19.0716922997645));
#48338=CARTESIAN_POINT('Ctrl Pts',(-2.55004350968591E-15,-5.05256917177841,
18.9296313323074));
#48339=CARTESIAN_POINT('Ctrl Pts',(-2.25598581474793E-15,-5.0382877754624,
18.8836938656593));
#48340=CARTESIAN_POINT('Ctrl Pts',(-1.39822119446523E-14,-5.02334918104501,
18.8379502101177));
#48341=CARTESIAN_POINT('Ctrl Pts',(-1.50521956010508E-14,-5.00775082964022,
18.7924156868194));
#48342=CARTESIAN_POINT('Ctrl Pts',(-1.61762705543893E-14,-4.99145691331742,
18.7448506786229));
#48343=CARTESIAN_POINT('Ctrl Pts',(-8.99370074056487E-17,-4.97444308272645,
18.697513865944));
#48344=CARTESIAN_POINT('Ctrl Pts',(8.32667268468867E-17,-4.95671627827806,
18.6504206457069));
#48345=CARTESIAN_POINT('Ctrl Pts',(50.,3.87994761181434,23.3663343702128));
#48346=CARTESIAN_POINT('Ctrl Pts',(50.,3.98673757809611,23.2643222420238));
#48347=CARTESIAN_POINT('Ctrl Pts',(50.,4.08880253645321,23.1578171274895));
#48348=CARTESIAN_POINT('Ctrl Pts',(50.,4.18601999315063,23.0472591141687));
#48349=CARTESIAN_POINT('Ctrl Pts',(50.,4.28495878527548,22.9347435570942));
#48350=CARTESIAN_POINT('Ctrl Pts',(50.,4.37887739050272,22.8180299104541));
#48351=CARTESIAN_POINT('Ctrl Pts',(50.,4.46762356605889,22.6975330565356));
#48352=CARTESIAN_POINT('Ctrl Pts',(50.,4.55766271640646,22.5752806408298));
#48353=CARTESIAN_POINT('Ctrl Pts',(50.,4.64237816685758,22.4491334930856));
#48354=CARTESIAN_POINT('Ctrl Pts',(50.,4.72157940439616,22.3194816713432));
#48355=CARTESIAN_POINT('Ctrl Pts',(50.,4.80065560169515,22.1900345395192));
#48356=CARTESIAN_POINT('Ctrl Pts',(50.,4.87423546656432,22.0570931764291));
#48357=CARTESIAN_POINT('Ctrl Pts',(50.,4.94209057403842,21.9210114696859));
#48358=CARTESIAN_POINT('Ctrl Pts',(50.,4.96154268599091,21.8820007497446));
#48359=CARTESIAN_POINT('Ctrl Pts',(50.,4.98052406523496,21.8427317710976));
#48360=CARTESIAN_POINT('Ctrl Pts',(50.,4.99902865333407,21.8032124599192));
#48361=CARTESIAN_POINT('Ctrl Pts',(50.,5.00999309769487,21.7797962516647));
#48362=CARTESIAN_POINT('Ctrl Pts',(50.,5.02079014100455,21.756292151844));
#48363=CARTESIAN_POINT('Ctrl Pts',(50.,5.03141846895726,21.73270178382));
#48364=CARTESIAN_POINT('Ctrl Pts',(50.,5.03934295940047,21.7151127851751));
#48365=CARTESIAN_POINT('Ctrl Pts',(50.,5.04717318872179,21.6974767538246));
#48366=CARTESIAN_POINT('Ctrl Pts',(50.,5.05490365729456,21.6798060792548));
#48367=CARTESIAN_POINT('Ctrl Pts',(50.,5.11733467588189,21.5370982728475));
#48368=CARTESIAN_POINT('Ctrl Pts',(50.,5.17335281141187,21.3919340172648));
#48369=CARTESIAN_POINT('Ctrl Pts',(50.,5.22279492351638,21.2447432489076));
#48370=CARTESIAN_POINT('Ctrl Pts',(50.,5.23314291494296,21.2139369434283));
#48371=CARTESIAN_POINT('Ctrl Pts',(50.,5.24320272739019,21.1830417306106));
#48372=CARTESIAN_POINT('Ctrl Pts',(50.,5.2529726674319,21.1520613441281));
#48373=CARTESIAN_POINT('Ctrl Pts',(50.,5.2991582979104,21.0056071513642));
#48374=CARTESIAN_POINT('Ctrl Pts',(50.,5.33886957351671,20.857251867747));
#48375=CARTESIAN_POINT('Ctrl Pts',(50.,5.37217407103346,20.7074371580895));
#48376=CARTESIAN_POINT('Ctrl Pts',(50.,5.40587044985943,20.5558596359311));
#48377=CARTESIAN_POINT('Ctrl Pts',(50.,5.43300860662334,20.4027874704091));
#48378=CARTESIAN_POINT('Ctrl Pts',(50.,5.45361092314426,20.2486538959499));
#48379=CARTESIAN_POINT('Ctrl Pts',(50.,5.47374677556284,20.0980101125235));
#48380=CARTESIAN_POINT('Ctrl Pts',(50.,5.48763934473341,19.9463517039926));
#48381=CARTESIAN_POINT('Ctrl Pts',(50.,5.4952635449959,19.794070763421));
#48382=CARTESIAN_POINT('Ctrl Pts',(50.,5.49686470975424,19.7620901140394));
#48383=CARTESIAN_POINT('Ctrl Pts',(50.,5.49818924741761,19.7300819857573));
#48384=CARTESIAN_POINT('Ctrl Pts',(50.,5.49923666289681,19.6980499851575));
#48385=CARTESIAN_POINT('Ctrl Pts',(50.,5.49987642324748,19.6784848705075));
#48386=CARTESIAN_POINT('Ctrl Pts',(50.,5.50041270196756,19.6589123700862));
#48387=CARTESIAN_POINT('Ctrl Pts',(50.,5.50084527831566,19.6393453886745));
#48388=CARTESIAN_POINT('Ctrl Pts',(50.,5.50435921646177,19.4803973493558));
#48389=CARTESIAN_POINT('Ctrl Pts',(50.,5.50104151508177,19.3215990804738));
#48390=CARTESIAN_POINT('Ctrl Pts',(50.,5.4909705479201,19.1634131964696));
#48391=CARTESIAN_POINT('Ctrl Pts',(50.,5.48078634391211,19.0034486877963));
#48392=CARTESIAN_POINT('Ctrl Pts',(50.,5.46369634889609,18.8441096739535));
#48393=CARTESIAN_POINT('Ctrl Pts',(50.,5.43973189107444,18.6858559372003));
#48394=CARTESIAN_POINT('Ctrl Pts',(50.,5.42686001032611,18.6008540881027));
#48395=CARTESIAN_POINT('Ctrl Pts',(50.,5.41200396913525,18.5161650932381));
#48396=CARTESIAN_POINT('Ctrl Pts',(50.,5.39516250342907,18.4318591808605));
#48397=CARTESIAN_POINT('Ctrl Pts',(50.,5.36396597336624,18.2756939173468));
#48398=CARTESIAN_POINT('Ctrl Pts',(50.,5.32596009918743,18.1208426670828));
#48399=CARTESIAN_POINT('Ctrl Pts',(50.,5.28136854987424,17.9676705715706));
#48400=CARTESIAN_POINT('Ctrl Pts',(50.,5.25350309477334,17.8719526560474));
#48401=CARTESIAN_POINT('Ctrl Pts',(50.,5.22306483730966,17.7768905017353));
#48402=CARTESIAN_POINT('Ctrl Pts',(50.,5.19009824063749,17.6825750879815));
#48403=CARTESIAN_POINT('Ctrl Pts',(50.,5.17761685929209,17.6468666204828));
#48404=CARTESIAN_POINT('Ctrl Pts',(50.,5.16477298038166,17.6112652149274));
#48405=CARTESIAN_POINT('Ctrl Pts',(50.,5.15156873790798,17.5757759000135));
#48406=CARTESIAN_POINT('Ctrl Pts',(50.,5.14404034706544,17.5555416886274));
#48407=CARTESIAN_POINT('Ctrl Pts',(50.,5.13639438080441,17.5353429478627));
#48408=CARTESIAN_POINT('Ctrl Pts',(50.,5.12863752106129,17.5151965619237));
#48409=CARTESIAN_POINT('Ctrl Pts',(50.,5.07015508167858,17.3633039361097));
#48410=CARTESIAN_POINT('Ctrl Pts',(50.,5.00529636697242,17.2141769687293));
#48411=CARTESIAN_POINT('Ctrl Pts',(50.,4.93436661664131,17.0681831171989));
#48412=CARTESIAN_POINT('Ctrl Pts',(50.,4.86274846547203,16.9207723385076));
#48413=CARTESIAN_POINT('Ctrl Pts',(50.,4.78494068080824,16.7765550865127));
#48414=CARTESIAN_POINT('Ctrl Pts',(50.,4.70120368491443,16.6359121753525));
#48415=CARTESIAN_POINT('Ctrl Pts',(50.,4.61735315197323,16.4950785697364));
#48416=CARTESIAN_POINT('Ctrl Pts',(50.,4.52755705979088,16.3578282816204));
#48417=CARTESIAN_POINT('Ctrl Pts',(50.,4.43202664990479,16.2245569418224));
#48418=CARTESIAN_POINT('Ctrl Pts',(50.,4.34556725909594,16.1039402830544));
#48419=CARTESIAN_POINT('Ctrl Pts',(50.,4.25441008172596,15.9865825841098));
#48420=CARTESIAN_POINT('Ctrl Pts',(50.,4.15867898536816,15.8727940124341));
#48421=CARTESIAN_POINT('Ctrl Pts',(50.,4.11861293335795,15.8251704188017));
#48422=CARTESIAN_POINT('Ctrl Pts',(50.,4.07774532870654,15.7781722486037));
#48423=CARTESIAN_POINT('Ctrl Pts',(50.,4.03609486664093,15.7318124329449));
#48424=CARTESIAN_POINT('Ctrl Pts',(50.,4.01339708741421,15.7065482507815));
#48425=CARTESIAN_POINT('Ctrl Pts',(50.,3.9904668008218,15.6814736593072));
#48426=CARTESIAN_POINT('Ctrl Pts',(50.,3.96730693292679,15.6565908429678));
#48427=CARTESIAN_POINT('Ctrl Pts',(50.,3.95229484852802,15.6404619539491));
#48428=CARTESIAN_POINT('Ctrl Pts',(50.,3.93719275896563,15.6244205832957));
#48429=CARTESIAN_POINT('Ctrl Pts',(50.,3.92200238339549,15.6084678404505));
#48430=CARTESIAN_POINT('Ctrl Pts',(50.,3.80788414784779,15.4886222936937));
#48431=CARTESIAN_POINT('Ctrl Pts',(50.,3.68877507270694,15.3737638929061));
#48432=CARTESIAN_POINT('Ctrl Pts',(50.,3.56510260126303,15.2640814626229));
#48433=CARTESIAN_POINT('Ctrl Pts',(50.,3.43994735694197,15.1530839932624));
#48434=CARTESIAN_POINT('Ctrl Pts',(50.,3.31011817858053,15.0473868234606));
#48435=CARTESIAN_POINT('Ctrl Pts',(50.,3.17601311849488,14.947214065385));
#48436=CARTESIAN_POINT('Ctrl Pts',(50.,3.12100973291315,14.9061280628605));
#48437=CARTESIAN_POINT('Ctrl Pts',(50.,3.06528655998735,14.8659717741899));
#48438=CARTESIAN_POINT('Ctrl Pts',(50.,3.00886919673059,14.8267623442652));
#48439=CARTESIAN_POINT('Ctrl Pts',(50.,2.96664655543823,14.7974180856998));
#48440=CARTESIAN_POINT('Ctrl Pts',(50.,2.92403507641734,14.7686041826055));
#48441=CARTESIAN_POINT('Ctrl Pts',(50.,2.88104513961241,14.7403282232461));
#48442=CARTESIAN_POINT('Ctrl Pts',(50.,2.85826547946661,14.7253452576412));
#48443=CARTESIAN_POINT('Ctrl Pts',(50.,2.8353875118122,14.7105185891356));
#48444=CARTESIAN_POINT('Ctrl Pts',(50.,2.81241516289751,14.6958504281824));
#48445=CARTESIAN_POINT('Ctrl Pts',(50.,2.66893410381596,14.6042357972118));
#48446=CARTESIAN_POINT('Ctrl Pts',(50.,2.52174774822922,14.518784282482));
#48447=CARTESIAN_POINT('Ctrl Pts',(50.,2.3712759493438,14.4397157364412));
#48448=CARTESIAN_POINT('Ctrl Pts',(50.,2.22051092714072,14.3604931100906));
#48449=CARTESIAN_POINT('Ctrl Pts',(50.,2.06644706727002,14.2876778434072));
#48450=CARTESIAN_POINT('Ctrl Pts',(50.,1.90947068911084,14.2215285485816));
#48451=CARTESIAN_POINT('Ctrl Pts',(50.,1.85559389300112,14.1988250557891));
#48452=CARTESIAN_POINT('Ctrl Pts',(50.,1.80137373893839,14.1769071549062));
#48453=CARTESIAN_POINT('Ctrl Pts',(50.,1.74682506104155,14.1557864850509));
#48454=CARTESIAN_POINT('Ctrl Pts',(50.,1.69123832588192,14.134263890427));
#48455=CARTESIAN_POINT('Ctrl Pts',(50.,1.63531044223963,14.1135691537265));
#48456=CARTESIAN_POINT('Ctrl Pts',(50.,1.57906037163134,14.0937031294847));
#48457=CARTESIAN_POINT('Ctrl Pts',(47.1759584946969,-5.13650480025366,19.9998861825852));
#48458=CARTESIAN_POINT('Ctrl Pts',(47.1912290598737,-5.13673309193899,19.718218970967));
#48459=CARTESIAN_POINT('Ctrl Pts',(47.2064996250505,-5.11395904926684,19.4365882959574));
#48460=CARTESIAN_POINT('Ctrl Pts',(47.2217701902273,-5.06785627834494,19.1588297576462));
#48461=CARTESIAN_POINT('Ctrl Pts',(47.2680740203902,-4.92806218100213,18.3166026340693));
#48462=CARTESIAN_POINT('Ctrl Pts',(47.314377850553,-4.57377431728328,17.5099775019703));
#48463=CARTESIAN_POINT('Ctrl Pts',(47.3606816807159,-4.04815105701765,16.8372152064567));
#48464=CARTESIAN_POINT('Ctrl Pts',(47.4069855108788,-3.52252779675202,16.164452910943));
#48465=CARTESIAN_POINT('Ctrl Pts',(47.4532893410417,-2.82556913993962,15.6255534520147));
#48466=CARTESIAN_POINT('Ctrl Pts',(47.4995931712046,-2.04217666516686,15.2861640769393));
#48467=CARTESIAN_POINT('Ctrl Pts',(47.5458970013674,-1.2587841903941,14.9467747018639));
#48468=CARTESIAN_POINT('Ctrl Pts',(47.5922008315303,-0.388957897660963,
14.8068954106414));
#48469=CARTESIAN_POINT('Ctrl Pts',(47.6385046616932,0.461342373938519,14.8835659064419));
#48470=CARTESIAN_POINT('Ctrl Pts',(47.6848084918561,1.311642645538,14.9602364022424));
#48471=CARTESIAN_POINT('Ctrl Pts',(47.7311123220189,2.14241689600384,15.2534566850659));
#48472=CARTESIAN_POINT('Ctrl Pts',(47.7774161521818,2.85246250286255,15.7275074812189));
#48473=CARTESIAN_POINT('Ctrl Pts',(47.8237199823447,3.56250810972125,16.2015582773719));
#48474=CARTESIAN_POINT('Ctrl Pts',(47.8700238125076,4.15182507297281,16.8564395868543));
#48475=CARTESIAN_POINT('Ctrl Pts',(47.9163276426705,4.54862442109196,17.6123755536693));
#48476=CARTESIAN_POINT('Ctrl Pts',(47.9626314728334,4.9454237692111,18.3683115204842));
#48477=CARTESIAN_POINT('Ctrl Pts',(48.0089353029962,5.14970550219783,19.2253021446315));
#48478=CARTESIAN_POINT('Ctrl Pts',(48.0552391331591,5.13658459528959,20.0789512393964));
#48479=CARTESIAN_POINT('Ctrl Pts',(48.101542963322,5.12346368838135,20.9326003341614));
#48480=CARTESIAN_POINT('Ctrl Pts',(48.1478467934848,4.89294014157814,21.7829078995439));
#48481=CARTESIAN_POINT('Ctrl Pts',(48.1941506236477,4.47309567335396,22.526291726651));
#48482=CARTESIAN_POINT('Ctrl Pts',(48.2404544538106,4.05325120512978,23.2696755537581));
#48483=CARTESIAN_POINT('Ctrl Pts',(48.2867582839735,3.44408581548462,23.9061356425898));
#48484=CARTESIAN_POINT('Ctrl Pts',(48.3330621141364,2.71980639678025,24.3581403572819));
#48485=CARTESIAN_POINT('Ctrl Pts',(48.3793659442993,1.99552697807589,24.810145071974));
#48486=CARTESIAN_POINT('Ctrl Pts',(48.4256697744621,1.15613353031231,25.0776944125265));
#48487=CARTESIAN_POINT('Ctrl Pts',(48.471973604625,0.30387855446258,25.1281959122511));
#48488=CARTESIAN_POINT('Ctrl Pts',(48.5182774347879,-0.548376421387151,
25.1786974119757));
#48489=CARTESIAN_POINT('Ctrl Pts',(48.5645812649507,-1.41349292532303,25.0121510708724));
#48490=CARTESIAN_POINT('Ctrl Pts',(48.6108850951136,-2.18608467324978,24.648845783331));
#48491=CARTESIAN_POINT('Ctrl Pts',(48.6571889252765,-2.95867642117653,24.2855404957896));
#48492=CARTESIAN_POINT('Ctrl Pts',(48.7034927554394,-3.63874341309414,23.7254762618102));
#48493=CARTESIAN_POINT('Ctrl Pts',(48.7497965856023,-4.1434421202193,23.0368772228465));
#48494=CARTESIAN_POINT('Ctrl Pts',(48.7961004157652,-4.64814082734447,22.3482781838828));
#48495=CARTESIAN_POINT('Ctrl Pts',(48.842404245928,-4.97747124967718,21.531144339935));
#48496=CARTESIAN_POINT('Ctrl Pts',(48.8887080760909,-5.09131456590888,20.685019313948));
#48497=CARTESIAN_POINT('Ctrl Pts',(48.9011248822929,-5.12184271854912,20.4581229549778));
#48498=CARTESIAN_POINT('Ctrl Pts',(48.9135416884949,-5.13687531170795,20.2291418560254));
#48499=CARTESIAN_POINT('Ctrl Pts',(48.9259584946969,-5.13665113575917,20.0001315872378));
#48500=CARTESIAN_POINT('Ctrl Pts',(50.,-1.57888188187519,14.0941590297752));
#48501=CARTESIAN_POINT('Ctrl Pts',(49.9536961698371,-2.56072134667313,14.356646379112));
#48502=CARTESIAN_POINT('Ctrl Pts',(49.8610885095113,-4.38996617743935,15.3805039208954));
#48503=CARTESIAN_POINT('Ctrl Pts',(49.7221770190227,-6.06480273625955,18.0436167196139));
#48504=CARTESIAN_POINT('Ctrl Pts',(49.5832655285342,-6.26179330940861,21.1826217130423));
#48505=CARTESIAN_POINT('Ctrl Pts',(49.4443540380453,-4.93332128443375,24.0338649607667));
#48506=CARTESIAN_POINT('Ctrl Pts',(49.3054425475569,-2.40285814042326,25.9021352451997));
#48507=CARTESIAN_POINT('Ctrl Pts',(49.1665310570681,0.712991615200806,26.332535419579));
#48508=CARTESIAN_POINT('Ctrl Pts',(49.0276195665795,3.65514852614605,25.2200641339167));
#48509=CARTESIAN_POINT('Ctrl Pts',(48.8887080760909,5.70677685429529,22.8358293701168));
#48510=CARTESIAN_POINT('Ctrl Pts',(48.7497965856023,6.36804183630338,19.7606765440198));
#48511=CARTESIAN_POINT('Ctrl Pts',(48.6108850951136,5.47783010606213,16.7438373869472));
#48512=CARTESIAN_POINT('Ctrl Pts',(48.471973604625,3.25303119352331,14.5203085482529));
#48513=CARTESIAN_POINT('Ctrl Pts',(48.3330621141364,0.235681165538501,13.6318230833962));
#48514=CARTESIAN_POINT('Ctrl Pts',(48.1941506236477,-2.83908863701214,14.2948442639057));
#48515=CARTESIAN_POINT('Ctrl Pts',(48.0552391331592,-5.22215870445453,16.3478385001443));
#48516=CARTESIAN_POINT('Ctrl Pts',(47.9163276426704,-6.33293078716528,19.2906249877314));
#48517=CARTESIAN_POINT('Ctrl Pts',(47.7774161521818,-5.90078261843499,22.4062397932344));
#48518=CARTESIAN_POINT('Ctrl Pts',(47.6385046616932,-4.03100033593876,24.9356115677216));
#48519=CARTESIAN_POINT('Ctrl Pts',(47.4995931712046,-1.17912739907028,26.2624982202955));
#48520=CARTESIAN_POINT('Ctrl Pts',(47.3606816807159,1.96002163140553,26.0636243719931));
#48521=CARTESIAN_POINT('Ctrl Pts',(47.2217701902273,4.62164181175045,24.387442570214));
#48522=CARTESIAN_POINT('Ctrl Pts',(47.0828586997386,6.15727070156947,21.6423284830756));
#48523=CARTESIAN_POINT('Ctrl Pts',(46.94394720925,6.19277615550858,18.4970865545706));
#48524=CARTESIAN_POINT('Ctrl Pts',(46.8050357187613,4.71950782178093,15.7180061583685));
#48525=CARTESIAN_POINT('Ctrl Pts',(46.6661242282728,2.09640466180927,13.9821670984087));
#48526=CARTESIAN_POINT('Ctrl Pts',(46.527212737784,-1.03745495420322,13.7124796177954));
#48527=CARTESIAN_POINT('Ctrl Pts',(46.3883012472955,-3.91855477371191,14.9746488855395));
#48528=CARTESIAN_POINT('Ctrl Pts',(46.2493897568068,-5.84495954514333,17.4611669503603));
#48529=CARTESIAN_POINT('Ctrl Pts',(46.1104782663183,-6.34733064701209,20.5662322807994));
#48530=CARTESIAN_POINT('Ctrl Pts',(45.9715667758295,-5.30327315797554,23.5333439048828));
#48531=CARTESIAN_POINT('Ctrl Pts',(45.832655285341,-2.96715547971806,25.6396111299885));
#48532=CARTESIAN_POINT('Ctrl Pts',(45.6937437948522,0.0918635759318163,
26.371874639516));
#48533=CARTESIAN_POINT('Ctrl Pts',(45.5548323043637,3.12850149718234,25.5517297953366));
#48534=CARTESIAN_POINT('Ctrl Pts',(45.4159208138749,5.40292858824861,23.3789921587039));
#48535=CARTESIAN_POINT('Ctrl Pts',(45.2770093233864,6.36101599132474,20.3830155302438));
#48536=CARTESIAN_POINT('Ctrl Pts',(45.1380978328977,5.76934058177901,17.2937231128846));
#48537=CARTESIAN_POINT('Ctrl Pts',(44.9991863424091,3.77205488934985,14.8637730531032));
#48538=CARTESIAN_POINT('Ctrl Pts',(44.8602748519205,0.855766571765285,13.6851849660543));
#48539=CARTESIAN_POINT('Ctrl Pts',(44.7213633614318,-2.26901598809372,14.0451035454785));
#48540=CARTESIAN_POINT('Ctrl Pts',(44.5824518709432,-4.84098802139722,15.8558402160407));
#48541=CARTESIAN_POINT('Ctrl Pts',(44.4435403804545,-6.23352846356157,18.6762370936362));
#48542=CARTESIAN_POINT('Ctrl Pts',(44.3046288899659,-6.10736645042269,21.819148256341));
#48543=CARTESIAN_POINT('Ctrl Pts',(44.1657173994773,-4.49323939823524,24.5188521826282));
#48544=CARTESIAN_POINT('Ctrl Pts',(44.0268059089887,-1.78440430929869,26.1176079148025));
#48545=CARTESIAN_POINT('Ctrl Pts',(43.8878944185,1.35917319264309,26.2259034340967));
#48546=CARTESIAN_POINT('Ctrl Pts',(43.7489829280113,4.1716092428508,24.8173542181636));
#48547=CARTESIAN_POINT('Ctrl Pts',(43.6100714375227,5.967697451428,22.2351314204129));
#48548=CARTESIAN_POINT('Ctrl Pts',(43.4711599470341,6.309848804664,19.1083535450766));
#48549=CARTESIAN_POINT('Ctrl Pts',(43.3322484565454,5.11470343610716,16.1988114886301));
#48550=CARTESIAN_POINT('Ctrl Pts',(43.1933369660568,2.67343996414062,14.2153700121414));
#48551=CARTESIAN_POINT('Ctrl Pts',(43.0544254755682,-0.419165658805117,
13.6412638450101));
#48552=CARTESIAN_POINT('Ctrl Pts',(42.9155139850796,-3.40964807513886,14.6163650437647));
#48553=CARTESIAN_POINT('Ctrl Pts',(42.7766024945909,-5.56942266143649,16.9031053365388));
#48554=CARTESIAN_POINT('Ctrl Pts',(42.6376910041023,-6.37229386307993,19.9443559450525));
#48555=CARTESIAN_POINT('Ctrl Pts',(42.4987795136136,-5.62265457369981,22.999163363865));
#48556=CARTESIAN_POINT('Ctrl Pts',(42.3598680231251,-3.5031427704913,25.3232711811303));
#48557=CARTESIAN_POINT('Ctrl Pts',(42.2209565326363,-0.530144605918972,
26.350446601233));
#48558=CARTESIAN_POINT('Ctrl Pts',(42.0820450421478,2.57201506314977,25.8304342765551));
#48559=CARTESIAN_POINT('Ctrl Pts',(41.943133551659,5.04754318408075,23.8899271385383));
#48560=CARTESIAN_POINT('Ctrl Pts',(41.8042220611705,6.2933157545682,21.001699631427));
#48561=CARTESIAN_POINT('Ctrl Pts',(41.6653105706818,6.00581962429792,17.869423557181));
#48562=CARTESIAN_POINT('Ctrl Pts',(41.5263990801932,4.25509876298692,15.256229363099));
#48563=CARTESIAN_POINT('Ctrl Pts',(41.3874875897045,1.46768913436197,13.7987812534008));
#48564=CARTESIAN_POINT('Ctrl Pts',(41.248576099216,-1.67730017084697,13.8521638379692));
#48565=CARTESIAN_POINT('Ctrl Pts',(41.1096646087272,-4.41364132394809,15.4033712786614));
#48566=CARTESIAN_POINT('Ctrl Pts',(40.9707531182387,-6.07466727560423,18.0744759599007));
#48567=CARTESIAN_POINT('Ctrl Pts',(40.83184162775,-6.25569483461017,21.2147046861393));
#48568=CARTESIAN_POINT('Ctrl Pts',(40.6929301372614,-4.91261944606622,24.0589894698594));
#48569=CARTESIAN_POINT('Ctrl Pts',(40.5540186467727,-2.37266058160269,25.91436447159));
#48570=CARTESIAN_POINT('Ctrl Pts',(40.4151071562841,0.745360205886424,26.3287963706994));
#48571=CARTESIAN_POINT('Ctrl Pts',(40.2761956657955,3.68178554845507,25.2013152676496));
#48572=CARTESIAN_POINT('Ctrl Pts',(40.1372841753068,5.72120098964531,22.806614432796));
#48573=CARTESIAN_POINT('Ctrl Pts',(39.9983726848182,6.36673461236813,19.728125554767));
#48574=CARTESIAN_POINT('Ctrl Pts',(39.8594611943296,5.46111216921441,16.7158746653705));
#48575=CARTESIAN_POINT('Ctrl Pts',(39.7205497038409,3.22497451167542,14.5037499386089));
#48576=CARTESIAN_POINT('Ctrl Pts',(39.5816382133523,0.203121871393965,13.6307012282624));
#48577=CARTESIAN_POINT('Ctrl Pts',(39.4427267228636,-2.86821826005961,14.3094333014226));
#48578=CARTESIAN_POINT('Ctrl Pts',(39.303815232375,-5.24076153202002,16.3745836235273));
#48579=CARTESIAN_POINT('Ctrl Pts',(39.1649037418863,-6.33647460213517,19.3230103732012));
#48580=CARTESIAN_POINT('Ctrl Pts',(39.0259922513978,-5.88840398818078,22.4363751374273));
#48581=CARTESIAN_POINT('Ctrl Pts',(38.8870807609091,-4.00571514043749,24.9561549160581));
#48582=CARTESIAN_POINT('Ctrl Pts',(38.7481692704204,-1.14709597416125,26.2684444772495));
#48583=CARTESIAN_POINT('Ctrl Pts',(38.6092577799318,1.990995321361,26.0535248383579));
#48584=CARTESIAN_POINT('Ctrl Pts',(38.4703462894431,4.64401151042891,24.3637578334849));
#48585=CARTESIAN_POINT('Ctrl Pts',(38.3314347989546,6.16558637784845,21.6108289653426));
#48586=CARTESIAN_POINT('Ctrl Pts',(38.1925233084659,6.18501182457331,18.4654466225688));
#48587=CARTESIAN_POINT('Ctrl Pts',(38.0536118179773,4.69755514202461,15.6939343913573));
#48588=CARTESIAN_POINT('Ctrl Pts',(37.9147003274886,2.06561206307644,13.9715282083127));
#48589=CARTESIAN_POINT('Ctrl Pts',(37.775788837,-1.06958533326773,13.7178656052934));
#48590=CARTESIAN_POINT('Ctrl Pts',(37.6368773465114,-3.94419486492413,14.9947475382551));
#48591=CARTESIAN_POINT('Ctrl Pts',(37.4979658560227,-5.85786253827827,17.4910815435863));
#48592=CARTESIAN_POINT('Ctrl Pts',(37.3590543655341,-6.34435292805762,20.5986745881895));
#48593=CARTESIAN_POINT('Ctrl Pts',(37.2201428750454,-5.2851402019413,23.5604098618166));
#48594=CARTESIAN_POINT('Ctrl Pts',(37.0812313845568,-2.93828509988496,25.6547065361601));
#48595=CARTESIAN_POINT('Ctrl Pts',(36.9423198940682,0.124437559632812,26.371321733522));
#48596=CARTESIAN_POINT('Ctrl Pts',(36.8034084035795,3.15684293922622,25.5356632841381));
#48597=CARTESIAN_POINT('Ctrl Pts',(36.6644969130909,5.42013253618787,23.3513263983764));
#48598=CARTESIAN_POINT('Ctrl Pts',(36.5255854226022,6.36289097027834,20.3504908538714));
#48599=CARTESIAN_POINT('Ctrl Pts',(36.3866739321137,5.75542978222766,17.2642636530279));
#48600=CARTESIAN_POINT('Ctrl Pts',(36.247762441625,3.74574746168526,14.844556149896));
#48601=CARTESIAN_POINT('Ctrl Pts',(36.1088509511364,0.823471912402398,13.6808925196843));
#48602=CARTESIAN_POINT('Ctrl Pts',(35.9699394606477,-2.29942978666854,14.0567813438779));
#48603=CARTESIAN_POINT('Ctrl Pts',(35.8310279701591,-4.86211110923449,15.8806431448883));
#48604=CARTESIAN_POINT('Ctrl Pts',(35.6921164796705,-6.24021452817564,18.7081223043017));
#48605=CARTESIAN_POINT('Ctrl Pts',(35.5532049891818,-6.09798653594926,21.8503474121577));
#48606=CARTESIAN_POINT('Ctrl Pts',(35.4142934986932,-4.47007877524375,24.5417640935448));
#48607=CARTESIAN_POINT('Ctrl Pts',(35.2753820082045,-1.7531057040892,26.1266504493554));
#48608=CARTESIAN_POINT('Ctrl Pts',(35.1364705177159,1.39098436071829,26.2188735190977));
#48609=CARTESIAN_POINT('Ctrl Pts',(34.9975590272273,4.19618267645299,24.7959645832859));
#48610=CARTESIAN_POINT('Ctrl Pts',(34.8586475367386,5.97904621488101,22.2045933181914));
#48611=CARTESIAN_POINT('Ctrl Pts',(34.7197360462499,6.3052079479044,19.0761071101149));
#48612=CARTESIAN_POINT('Ctrl Pts',(34.5808245557615,5.09520363185058,16.1727130642877));
#48613=CARTESIAN_POINT('Ctrl Pts',(34.4419130652726,2.64383203702432,14.2017780744179));
#48614=CARTESIAN_POINT('Ctrl Pts',(34.3030015747841,-0.451668196904035,
13.6434898585621));
#48615=CARTESIAN_POINT('Ctrl Pts',(34.1640900842954,-3.43712648530661,14.6338666749417));
#48616=CARTESIAN_POINT('Ctrl Pts',(34.0251785938068,-5.58518225554684,16.9316185845593));
#48617=CARTESIAN_POINT('Ctrl Pts',(33.8862671033181,-6.37249506064328,19.9769339996099));
#48618=CARTESIAN_POINT('Ctrl Pts',(33.7473556128295,-5.60724835605281,23.0278690876325));
#48619=CARTESIAN_POINT('Ctrl Pts',(33.6084441223409,-3.47588262343321,25.341110870073));
#48620=CARTESIAN_POINT('Ctrl Pts',(33.4695326318522,-0.497672041157185,
26.3530738920422));
#48621=CARTESIAN_POINT('Ctrl Pts',(33.3306211413636,2.60178860923987,25.8172090706048));
#48622=CARTESIAN_POINT('Ctrl Pts',(33.191709650875,5.0673638491298,23.8640715519811));
#48623=CARTESIAN_POINT('Ctrl Pts',(33.0527981603864,6.29835454118703,20.9695129766052));
#48624=CARTESIAN_POINT('Ctrl Pts',(32.9138866698977,5.99484891033732,17.8387476129511));
#48625=CARTESIAN_POINT('Ctrl Pts',(32.774975179409,4.23079139261945,15.2345378471302));
#48626=CARTESIAN_POINT('Ctrl Pts',(32.6360636889205,1.43596722108643,13.7913589668703));
#48627=CARTESIAN_POINT('Ctrl Pts',(32.4971521984318,-1.70870807523846,13.8608191057836));
#48628=CARTESIAN_POINT('Ctrl Pts',(32.3582407079432,-4.43708317105403,15.4259953791621));
#48629=CARTESIAN_POINT('Ctrl Pts',(32.2193292174545,-6.08443182323413,18.1055568821649));
#48630=CARTESIAN_POINT('Ctrl Pts',(32.0804177269659,-6.24940310229619,21.2466700458854));
#48631=CARTESIAN_POINT('Ctrl Pts',(31.9415062364773,-4.8918043167284,24.0840514033414));
#48632=CARTESIAN_POINT('Ctrl Pts',(31.8025947459886,-2.34239333841841,25.9264170277183));
#48633=CARTESIAN_POINT('Ctrl Pts',(31.6636832554999,0.777705418913837,26.3249031312495));
#48634=CARTESIAN_POINT('Ctrl Pts',(31.5247717650114,3.70832832222358,25.1824247599837));
#48635=CARTESIAN_POINT('Ctrl Pts',(31.3858602745226,5.73547458931472,22.7773290358944));
#48636=CARTESIAN_POINT('Ctrl Pts',(31.2469487840341,6.36526149692924,19.6955802010263));
#48637=CARTESIAN_POINT('Ctrl Pts',(31.1080372935454,5.44425124037868,16.6879985250709));
#48638=CARTESIAN_POINT('Ctrl Pts',(30.9691258030568,3.19683367304369,14.48733460065));
#48639=CARTESIAN_POINT('Ctrl Pts',(30.8302143125682,0.170557201505726,13.629746034944));
#48640=CARTESIAN_POINT('Ctrl Pts',(30.6913028220795,-2.8972728848445,14.3241709707707));
#48641=CARTESIAN_POINT('Ctrl Pts',(30.5523913315909,-5.25922740334937,16.4014235511586));
#48642=CARTESIAN_POINT('Ctrl Pts',(30.4134798411023,-6.33985279708097,19.3554134273491));
#48643=CARTESIAN_POINT('Ctrl Pts',(30.2745683506136,-5.87587146197975,22.4664468168986));
#48644=CARTESIAN_POINT('Ctrl Pts',(30.135656860125,-3.98032524857262,24.9765687229126));
#48645=CARTESIAN_POINT('Ctrl Pts',(29.9967453696363,-1.11503456969162,26.2742269043038));
#48646=CARTESIAN_POINT('Ctrl Pts',(29.8578338791477,2.02191697488329,26.0432670870131));
#48647=CARTESIAN_POINT('Ctrl Pts',(29.7189223886591,4.6662598320792,24.3399590456387));
#48648=CARTESIAN_POINT('Ctrl Pts',(29.5800108981704,6.17374090938801,21.5792873462565));
#48649=CARTESIAN_POINT('Ctrl Pts',(29.4410994076818,6.17708584096459,18.4338467981542));
#48650=CARTESIAN_POINT('Ctrl Pts',(29.3021879171932,4.6754796861493,15.6699751683504));
#48651=CARTESIAN_POINT('Ctrl Pts',(29.1632764267045,2.03476547711032,13.9610468795116));
#48652=CARTESIAN_POINT('Ctrl Pts',(29.0243649362159,-1.10168775744487,13.7234157837727));
#48653=CARTESIAN_POINT('Ctrl Pts',(28.8854534457272,-3.96973186994514,15.0149770091765));
#48654=CARTESIAN_POINT('Ctrl Pts',(28.7465419552386,-5.87061242924704,17.5210617103551));
#48655=CARTESIAN_POINT('Ctrl Pts',(28.60763046475,-6.34120939193935,20.6311012485152));
#48656=CARTESIAN_POINT('Ctrl Pts',(28.4687189742614,-5.26686911251823,23.587382763227));
#48657=CARTESIAN_POINT('Ctrl Pts',(28.3298074837727,-2.90933792449704,25.6696541498914));
#48658=CARTESIAN_POINT('Ctrl Pts',(28.1908959932841,0.157008291011193,26.3706023055007));
#48659=CARTESIAN_POINT('Ctrl Pts',(28.0519845027954,3.18510187344724,25.5194520918348));
#48660=CARTESIAN_POINT('Ctrl Pts',(27.9130730123068,5.43719482255474,23.3235730471709));
#48661=CARTESIAN_POINT('Ctrl Pts',(27.7741615218181,6.36459964755315,20.3179570170062));
#48662=CARTESIAN_POINT('Ctrl Pts',(27.6352500313296,5.74136855771394,17.2348756948754));
#48663=CARTESIAN_POINT('Ctrl Pts',(27.4963385408409,3.71934213448194,14.8254739903094));
#48664=CARTESIAN_POINT('Ctrl Pts',(27.3574270503523,0.791155730627478,13.6767652306598));
#48665=CARTESIAN_POINT('Ctrl Pts',(27.2185155598636,-2.3297834869271,14.0686144753238));
#48666=CARTESIAN_POINT('Ctrl Pts',(27.079604069375,-4.88310712004916,15.905553737998));
#48667=CARTESIAN_POINT('Ctrl Pts',(26.9406925788864,-6.24673749740478,18.7400412797182));
#48668=CARTESIAN_POINT('Ctrl Pts',(26.8017810883977,-6.08844724338766,21.881498206957));
#48669=CARTESIAN_POINT('Ctrl Pts',(26.6628695979091,-4.44680132145817,24.5645573000867));
#48670=CARTESIAN_POINT('Ctrl Pts',(26.5239581074204,-1.7217612793893,26.135532856655));
#48671=CARTESIAN_POINT('Ctrl Pts',(26.3850466169318,1.42275917377253,26.2116810664862));
#48672=CARTESIAN_POINT('Ctrl Pts',(26.2461351264432,4.22064643785949,24.7744496002033));
#48673=CARTESIAN_POINT('Ctrl Pts',(26.1072236359545,5.99023870889178,22.1739975963169));
#48674=CARTESIAN_POINT('Ctrl Pts',(25.968312145466,6.30040229708003,19.0438848221863));
#48675=CARTESIAN_POINT('Ctrl Pts',(25.8294006549772,5.07557065842261,16.1467146706146));
#48676=CARTESIAN_POINT('Ctrl Pts',(25.6904891644886,2.61415501023178,14.18833768008));
#48677=CARTESIAN_POINT('Ctrl Pts',(25.551577674,-0.484158930120513,13.6458820070224));
#48678=CARTESIAN_POINT('Ctrl Pts',(25.4126661835113,-3.46451506210964,14.6515085563579));
#48679=CARTESIAN_POINT('Ctrl Pts',(25.2737546930227,-5.60079587431515,16.960212028356));
#48680=CARTESIAN_POINT('Ctrl Pts',(25.1348432025341,-6.37252970551363,20.0095126570244));
#48681=CARTESIAN_POINT('Ctrl Pts',(24.9959317120454,-5.59169558634022,23.0564956744613));
#48682=CARTESIAN_POINT('Ctrl Pts',(24.8570202215568,-3.44853163007304,25.358810962768));
#48683=CARTESIAN_POINT('Ctrl Pts',(24.7181087310682,-0.465186469148229,
26.3555351377534));
#48684=CARTESIAN_POINT('Ctrl Pts',(24.5791972405795,2.63149415450833,25.8038318250175));
#48685=CARTESIAN_POINT('Ctrl Pts',(24.4402857500909,5.08705207263311,23.8381149733452));
#48686=CARTESIAN_POINT('Ctrl Pts',(24.3013742596023,6.30322871286294,20.9373009824156));
#48687=CARTESIAN_POINT('Ctrl Pts',(24.1624627691136,5.98372151391236,17.8081281556077));
#48688=CARTESIAN_POINT('Ctrl Pts',(24.023551278625,4.20637344551665,15.2129708821494));
#48689=CARTESIAN_POINT('Ctrl Pts',(23.8846397881363,1.40420777710976,13.784098950514));
#48690=CARTESIAN_POINT('Ctrl Pts',(23.7457282976477,-1.74007132052403,13.8696348283494));
#48691=CARTESIAN_POINT('Ctrl Pts',(23.6068168071591,-4.46040904974499,15.4487390266817));
#48692=CARTESIAN_POINT('Ctrl Pts',(23.4679053166705,-6.09403734704428,18.1366873179397));
#48693=CARTESIAN_POINT('Ctrl Pts',(23.3289938261818,-6.24294803444307,21.2786028224357));
#48694=CARTESIAN_POINT('Ctrl Pts',(23.1900823356932,-4.87086133430093,24.109006595311));
#48695=CARTESIAN_POINT('Ctrl Pts',(23.0511708452045,-2.31206487401468,25.9383146899305));
#48696=CARTESIAN_POINT('Ctrl Pts',(22.9122593547159,0.810030305690605,26.3208445829778));
#48697=CARTESIAN_POINT('Ctrl Pts',(22.7733478642273,3.73477417444681,25.1633988035191));
#48698=CARTESIAN_POINT('Ctrl Pts',(22.6344363737386,5.74959828557432,22.7479710502147));
#48699=CARTESIAN_POINT('Ctrl Pts',(22.49552488325,6.36362201785506,19.6630428036569));
#48700=CARTESIAN_POINT('Ctrl Pts',(22.3566133927613,5.42724801959969,16.6602089478459));
#48701=CARTESIAN_POINT('Ctrl Pts',(22.2177019022727,3.16860928138414,14.4710633427192));
#48702=CARTESIAN_POINT('Ctrl Pts',(22.0787904117841,0.137988073903447,13.628957335745));
#48703=CARTESIAN_POINT('Ctrl Pts',(21.9398789212955,-2.9262517859769,14.3390569846214));
#48704=CARTESIAN_POINT('Ctrl Pts',(21.8009674308068,-5.27755581855221,16.4283575318402));
#48705=CARTESIAN_POINT('Ctrl Pts',(21.6620559403182,-6.34306529247789,19.3878333285293));
#48706=CARTESIAN_POINT('Ctrl Pts',(21.5231444498295,-5.86318536293062,22.496454032866));
#48707=CARTESIAN_POINT('Ctrl Pts',(21.3842329593409,-3.95483132620118,24.9968524612595));
#48708=CARTESIAN_POINT('Ctrl Pts',(21.2453214688522,-1.08294402247514,26.2798453470195));
#48709=CARTESIAN_POINT('Ctrl Pts',(21.1064099783636,2.05278578321474,26.0328513877377));
#48710=CARTESIAN_POINT('Ctrl Pts',(20.967498487875,4.68838619551153,24.3160468278314));
#48711=CARTESIAN_POINT('Ctrl Pts',(20.8285869973864,6.18173408290928,21.5477044506284));
#48712=CARTESIAN_POINT('Ctrl Pts',(20.6896755068977,6.16899841191383,18.4022879070052));
#48713=CARTESIAN_POINT('Ctrl Pts',(20.5507640164091,4.65328203108421,15.646129115662));
#48714=CARTESIAN_POINT('Ctrl Pts',(20.4118525259204,2.00386571014259,13.9507233858905));
#48715=CARTESIAN_POINT('Ctrl Pts',(20.2729410354318,-1.13376138770991,13.7291300082018));
#48716=CARTESIAN_POINT('Ctrl Pts',(20.1340295449432,-3.99516512133005,15.0353367695678));
#48717=CARTESIAN_POINT('Ctrl Pts',(19.9951180544545,-5.88320888481873,17.5511066671072));
#48718=CARTESIAN_POINT('Ctrl Pts',(19.8562065639659,-6.33790012081599,20.6635114142635));
#48719=CARTESIAN_POINT('Ctrl Pts',(19.7172950734772,-5.24846036724355,23.6142619041474));
#48720=CARTESIAN_POINT('Ctrl Pts',(19.5783835829886,-2.8803147101225,25.6844535805079));
#48721=CARTESIAN_POINT('Ctrl Pts',(19.4394720925,0.189574918792307,26.3697163742558));
#48722=CARTESIAN_POINT('Ctrl Pts',(19.3005606020113,3.21327756126488,25.5030966421251));
#48723=CARTESIAN_POINT('Ctrl Pts',(19.1616491115227,5.45411500140619,23.2957328304541));
#48724=CARTESIAN_POINT('Ctrl Pts',(19.0227376210341,6.36614197849088,20.2854148699583));
#48725=CARTESIAN_POINT('Ctrl Pts',(18.8838261305454,5.72715727574455,17.2055600065159));
#48726=CARTESIAN_POINT('Ctrl Pts',(18.7449146400568,3.69283959787427,14.8065270730783));
#48727=CARTESIAN_POINT('Ctrl Pts',(18.6060031495682,0.758818871062057,13.6728032068524));
#48728=CARTESIAN_POINT('Ctrl Pts',(18.4670916590795,-2.36007629553962,14.0806026305434));
#48729=CARTESIAN_POINT('Ctrl Pts',(18.3281801685909,-4.90397550508568,15.9305713443019));
#48730=CARTESIAN_POINT('Ctrl Pts',(18.1892686781022,-6.2530972007635,18.7719931856456));
#48731=CARTESIAN_POINT('Ctrl Pts',(18.0503571876136,-6.07874882205854,21.9125998265761));
#48732=CARTESIAN_POINT('Ctrl Pts',(17.911445697125,-4.42340764526233,24.5872312065266));
#48733=CARTESIAN_POINT('Ctrl Pts',(17.7725342066364,-1.6903718544226,26.1442549045489));
#48734=CARTESIAN_POINT('Ctrl Pts',(17.6336227161477,1.45449680133364,26.2043262642456));
#48735=CARTESIAN_POINT('Ctrl Pts',(17.4947112256591,4.24499988768104,24.7528098312351));
#48736=CARTESIAN_POINT('Ctrl Pts',(17.3557997351704,6.00127464093126,22.1433450544447));
#48737=CARTESIAN_POINT('Ctrl Pts',(17.2168882446818,6.29543197779222,19.0116875234582));
#48738=CARTESIAN_POINT('Ctrl Pts',(17.0779767541932,5.05580502895429,16.1208169871096));
#48739=CARTESIAN_POINT('Ctrl Pts',(16.9390652637045,2.5844096594071,14.1750491804084));
#48740=CARTESIAN_POINT('Ctrl Pts',(16.8001537732159,-0.516637009270994,
13.6484402278693));
#48741=CARTESIAN_POINT('Ctrl Pts',(16.6612422827273,-3.49181308971526,14.6692902269219));
#48742=CARTESIAN_POINT('Ctrl Pts',(16.5223307922386,-5.61626310966114,16.9888849206056));
#48743=CARTESIAN_POINT('Ctrl Pts',(16.38341930175,-6.37239779678543,20.0420910658145));
#48744=CARTESIAN_POINT('Ctrl Pts',(16.2445078112613,-5.57599667105201,23.0850423761618));
#48745=CARTESIAN_POINT('Ctrl Pts',(16.1055963207727,-3.42109050526117,25.3763709966026));
#48746=CARTESIAN_POINT('Ctrl Pts',(15.9666848302841,-0.432688738940727,
26.3578302740393));
#48747=CARTESIAN_POINT('Ctrl Pts',(15.8277733397954,2.66113092256575,25.7903028894231));
#48748=CARTESIAN_POINT('Ctrl Pts',(15.6888618493068,5.10660734001576,23.8120580810363));
#48749=CARTESIAN_POINT('Ctrl Pts',(15.5499503588182,6.30793814220377,20.9050644907565));
#48750=CARTESIAN_POINT('Ctrl Pts',(15.4110388683295,5.97243772585063,17.7775659854265));
#48751=CARTESIAN_POINT('Ctrl Pts',(15.2721273778409,4.1818455598703,15.1915290318346));
#48752=CARTESIAN_POINT('Ctrl Pts',(15.1332158873523,1.37241163250246,13.777001394081));
#48753=CARTESIAN_POINT('Ctrl Pts',(14.9943043968636,-1.77138908698832,13.8786107752573));
#48754=CARTESIAN_POINT('Ctrl Pts',(14.855392906375,-4.48361835037166,15.4716016267882));
#48755=CARTESIAN_POINT('Ctrl Pts',(14.7164814158863,-6.10348359598301,18.1678664535947));
#48756=CARTESIAN_POINT('Ctrl Pts',(14.5775699253977,-6.2363297997616,21.3105021811896));
#48757=CARTESIAN_POINT('Ctrl Pts',(14.4386584349091,-4.84979104615329,24.133854393535));
#48758=CARTESIAN_POINT('Ctrl Pts',(14.2997469444204,-2.28167598106183,25.950057147267));
#48759=CARTESIAN_POINT('Ctrl Pts',(14.1608354539318,0.842334021367499,26.3166208319594));
#48760=CARTESIAN_POINT('Ctrl Pts',(14.0219239634432,3.7611224139311,25.1442378955218));
#48761=CARTESIAN_POINT('Ctrl Pts',(13.8830124729545,5.76357170928461,22.7185412430624));
#48762=CARTESIAN_POINT('Ctrl Pts',(13.7441009824659,6.36181621799531,19.6305142130623));
#48763=CARTESIAN_POINT('Ctrl Pts',(13.6051894919773,5.41010295127669,16.6325066600089));
#48764=CARTESIAN_POINT('Ctrl Pts',(13.4662780014886,3.14030207437455,14.4549365900852));
#48765=CARTESIAN_POINT('Ctrl Pts',(13.327366511,0.105415339819669,13.6283351512789));
#48766=CARTESIAN_POINT('Ctrl Pts',(13.1884550205113,-2.95515420605895,14.354090953911));
#48767=CARTESIAN_POINT('Ctrl Pts',(13.0495435300227,-5.29574629859371,16.4553848616206));
#48768=CARTESIAN_POINT('Ctrl Pts',(12.9106320395341,-6.34611200436357,19.4202692294091));
#48769=CARTESIAN_POINT('Ctrl Pts',(12.7717205490454,-5.8503460225996,22.5263960010557));
#48770=CARTESIAN_POINT('Ctrl Pts',(12.6328090585568,-3.92923403963699,25.0170056009591));
#48771=CARTESIAN_POINT('Ctrl Pts',(12.4938975680681,-1.05082517123617,26.285299658552));
#48772=CARTESIAN_POINT('Ctrl Pts',(12.3549860775795,2.0836009395627,26.0222780127582));
#48773=CARTESIAN_POINT('Ctrl Pts',(12.2160745870909,4.71039002242726,24.2920218050372));
#48774=CARTESIAN_POINT('Ctrl Pts',(12.0771630966022,6.1895656895012,21.5160811039145));
#48775=CARTESIAN_POINT('Ctrl Pts',(11.9382516061136,6.1607497487956,18.370770773951));
#48776=CARTESIAN_POINT('Ctrl Pts',(11.799340115625,4.63096275699136,15.6223968565371));
#48777=CARTESIAN_POINT('Ctrl Pts',(11.6604286251363,1.97291356977519,13.9405579972662));
#48778=CARTESIAN_POINT('Ctrl Pts',(11.5215171346477,-1.1658053857806,13.7350081292326));
#48779=CARTESIAN_POINT('Ctrl Pts',(11.3826056441591,-4.02049395435078,15.0558262873028));
#48780=CARTESIAN_POINT('Ctrl Pts',(11.2436941536704,-5.89565157577014,17.5812156285819));
#48781=CARTESIAN_POINT('Ctrl Pts',(11.1047826631818,-6.33442520117924,20.6959042383565));
#48782=CARTESIAN_POINT('Ctrl Pts',(10.9658711726931,-5.22991444725156,23.6410465820594));
#48783=CARTESIAN_POINT('Ctrl Pts',(10.8269596822045,-2.85121621531744,25.699104441209));
#48784=CARTESIAN_POINT('Ctrl Pts',(10.6880481917159,0.222136591808738,26.3686639629421));
#48785=CARTESIAN_POINT('Ctrl Pts',(10.5491367012273,3.24136926627416,25.486597362478));
#48786=CARTESIAN_POINT('Ctrl Pts',(10.4102252107386,5.47089263051329,23.267806475863));
#48787=CARTESIAN_POINT('Ctrl Pts',(10.27131372025,6.36751792278091,20.2528652632554));
#48788=CARTESIAN_POINT('Ctrl Pts',(10.1324022297613,5.71279630774815,17.1763173541497));
#48789=CARTESIAN_POINT('Ctrl Pts',(9.99349073927272,3.66624054453745,14.7877158934027));
#48790=CARTESIAN_POINT('Ctrl Pts',(9.85457924878407,0.726462178868265,13.6690065518142));
#48791=CARTESIAN_POINT('Ctrl Pts',(9.71566775829543,-2.39030742076759,14.0927454962123));
#48792=CARTESIAN_POINT('Ctrl Pts',(9.5767562678068,-4.92471571892393,15.9556953099351));
#48793=CARTESIAN_POINT('Ctrl Pts',(9.43784477731815,-6.25929347203341,18.803977186983));
#48794=CARTESIAN_POINT('Ctrl Pts',(9.29893328682952,-6.06889152544171,21.9436514581372));
#48795=CARTESIAN_POINT('Ctrl Pts',(9.16002179634088,-4.39989835807759,24.6097852202552));
#48796=CARTESIAN_POINT('Ctrl Pts',(9.02111030585225,-1.65893824958895,26.152816365076));
#48797=CARTESIAN_POINT('Ctrl Pts',(8.88219881536361,1.48619641390095,26.1968093046023));
#48798=CARTESIAN_POINT('Ctrl Pts',(8.74328732487498,4.26924238941132,24.7310458419625));
#48799=CARTESIAN_POINT('Ctrl Pts',(8.60437583438633,6.01215372256228,22.1126364937154));
#48800=CARTESIAN_POINT('Ctrl Pts',(8.4654643438977,6.29029711994617,18.9795160554453));
#48801=CARTESIAN_POINT('Ctrl Pts',(8.32655285340906,5.03590726004376,16.0950206906393));
#48802=CARTESIAN_POINT('Ctrl Pts',(8.18764136292043,2.55459676198038,14.1619129227137));
#48803=CARTESIAN_POINT('Ctrl Pts',(8.04872987243179,-0.549101585502231,
13.6511644542408));
#48804=CARTESIAN_POINT('Ctrl Pts',(7.90981838194317,-3.51901985465715,14.6872112218886));
#48805=CARTESIAN_POINT('Ctrl Pts',(7.77090689145451,-5.63158355733028,17.017636511908));
#48806=CARTESIAN_POINT('Ctrl Pts',(7.63199540096589,-6.37209933790631,20.0746683745047));
#48807=CARTESIAN_POINT('Ctrl Pts',(7.49308391047725,-5.56015202049796,23.1135084466321));
#48808=CARTESIAN_POINT('Ctrl Pts',(7.35417241998862,-3.39355996620412,25.3937905126241));
#48809=CARTESIAN_POINT('Ctrl Pts',(7.21526092949997,-0.400179699901651,
26.3599592409137));
#48810=CARTESIAN_POINT('Ctrl Pts',(7.07634943901134,2.69069813882,25.7766226174165));
#48811=CARTESIAN_POINT('Ctrl Pts',(6.93743794852271,5.12602914017768,23.7859015560823));
#48812=CARTESIAN_POINT('Ctrl Pts',(6.79852645803408,6.31248270612288,20.8728043441669));
#48813=CARTESIAN_POINT('Ctrl Pts',(6.65961496754543,5.96099784106742,17.7470619011862));
#48814=CARTESIAN_POINT('Ctrl Pts',(6.5207034770568,4.15720837674583,15.1702128565938));
#48815=CARTESIAN_POINT('Ctrl Pts',(6.38179198656816,1.34057961829449,13.7700664830746));
#48816=CARTESIAN_POINT('Ctrl Pts',(6.24288049607952,-1.80266055610438,13.8877467119104));
#48817=CARTESIAN_POINT('Ctrl Pts',(6.10396900559088,-4.50671046633138,15.4945825819403));
#48818=CARTESIAN_POINT('Ctrl Pts',(5.96505751510225,-6.11277032316134,18.1990934742261));
#48819=CARTESIAN_POINT('Ctrl Pts',(5.82614602461361,-6.22954857122723,21.3423672884193));
#48820=CARTESIAN_POINT('Ctrl Pts',(5.68723453412497,-4.82859400298248,24.1585941485866));
#48821=CARTESIAN_POINT('Ctrl Pts',(5.54832304363634,-2.25122745380935,25.9616440928248));
#48822=CARTESIAN_POINT('Ctrl Pts',(5.4094115531477,0.874615721648888,26.3122319885871));
#48823=CARTESIAN_POINT('Ctrl Pts',(5.27050006265906,3.78737235203403,25.1249425367847));
#48824=CARTESIAN_POINT('Ctrl Pts',(5.13158857217043,5.77739449523354,22.6890403836206));
#48825=CARTESIAN_POINT('Ctrl Pts',(4.99267708168179,6.35984414454672,19.5979952794158));
#48826=CARTESIAN_POINT('Ctrl Pts',(4.85376559119316,5.39281648351639,16.604892385592));
#48827=CARTESIAN_POINT('Ctrl Pts',(4.71485410070452,3.11191279185723,14.4389547642397));
#48828=CARTESIAN_POINT('Ctrl Pts',(4.57594261021589,0.0728398505813112,
13.6278794978073));
#48829=CARTESIAN_POINT('Ctrl Pts',(4.43703111972725,-2.98397938969178,14.3692724857092));
#48830=CARTESIAN_POINT('Ctrl Pts',(4.29811962923861,-5.31379836804421,16.4825048341088));
#48831=CARTESIAN_POINT('Ctrl Pts',(4.15920813874997,-6.34899285310857,19.4527202822382));
#48832=CARTESIAN_POINT('Ctrl Pts',(4.02029664826134,-5.83735377655805,22.5562719388986));
#48833=CARTESIAN_POINT('Ctrl Pts',(3.8813851577727,-3.90353405789533,25.0370276152856));
#48834=CARTESIAN_POINT('Ctrl Pts',(3.74247366728407,-1.01867885543911,26.2905896963458));
#48835=CARTESIAN_POINT('Ctrl Pts',(3.60356217679543,2.11436163853657,26.0115472384233));
#48836=CARTESIAN_POINT('Ctrl Pts',(3.46465068630679,4.73227073773,24.2678846051763));
#48837=CARTESIAN_POINT('Ctrl Pts',(3.32573919581815,6.19723552447633,21.4844181326321));
#48838=CARTESIAN_POINT('Ctrl Pts',(3.18682770532951,6.15234006719685,18.3392962227209));
#48839=CARTESIAN_POINT('Ctrl Pts',(3.04791621484088,4.60852244721424,15.5987790112615));
#48840=CARTESIAN_POINT('Ctrl Pts',(2.90900472435224,1.94190986497335,13.9305509792932));
#48841=CARTESIAN_POINT('Ctrl Pts',(2.77009323386361,-1.19781891413772,13.7410499932924));
#48842=CARTESIAN_POINT('Ctrl Pts',(2.63118174337496,-4.04571770703044,15.0764450267472));
#48843=CARTESIAN_POINT('Ctrl Pts',(2.49227025288634,-5.90794017685321,17.6113878080752));
#48844=CARTESIAN_POINT('Ctrl Pts',(2.3533587623977,-6.33078472393609,20.7282788737186));
#48845=CARTESIAN_POINT('Ctrl Pts',(2.21444727190907,-5.2112318370928,23.6677360978016));
#48846=CARTESIAN_POINT('Ctrl Pts',(2.07553578142043,-2.82204320093811,25.7136063473297));
#48847=CARTESIAN_POINT('Ctrl Pts',(1.93662429093179,0.254692459677778,26.3674451025059));
#48848=CARTESIAN_POINT('Ctrl Pts',(1.79771280044316,3.26937625297555,25.4699546773483));
#48849=CARTESIAN_POINT('Ctrl Pts',(1.65880130995452,5.48752727391192,23.2397947266211));
#48850=CARTESIAN_POINT('Ctrl Pts',(1.51988981946589,6.36872743946243,20.220309021366));
#48851=CARTESIAN_POINT('Ctrl Pts',(1.38097832897725,5.69828603890732,17.1471485537567));
#48852=CARTESIAN_POINT('Ctrl Pts',(1.24206683848861,3.63954565029315,14.7690408411714));
#48853=CARTESIAN_POINT('Ctrl Pts',(1.10315534799997,0.694086537873731,13.6653755651264));
#48854=CARTESIAN_POINT('Ctrl Pts',(0.964243857511333,-2.4204761475888,14.1050423605135));
#48855=CARTESIAN_POINT('Ctrl Pts',(0.8253323670227,-4.94532707163062,15.9809257548385));
#48856=CARTESIAN_POINT('Ctrl Pts',(0.686420876534066,-6.26532644037927,
18.8359909188598));
#48857=CARTESIAN_POINT('Ctrl Pts',(0.547509386045428,-6.05887503803249,
21.9746553002093));
#48858=CARTESIAN_POINT('Ctrl Pts',(0.408597895556788,-4.37627520273034,
24.6322128254603));
#48859=CARTESIAN_POINT('Ctrl Pts',(0.269686405068149,-1.62745906490466,
26.1612286823026));
#48860=CARTESIAN_POINT('Ctrl Pts',(0.13077491457951,1.51785280933213,26.1891074109947));
#48861=CARTESIAN_POINT('Ctrl Pts',(-0.00813657590912298,4.29338191907513,
24.7092034479418));
#48862=CARTESIAN_POINT('Ctrl Pts',(-0.147048066397757,6.02285873175444,
22.0817834333193));
#48863=CARTESIAN_POINT('Ctrl Pts',(-0.285959556886395,6.28503105744338,
18.9475493472432));
#48864=CARTESIAN_POINT('Ctrl Pts',(-0.42487104737502,5.01581409828515,16.0689497592415));
#48865=CARTESIAN_POINT('Ctrl Pts',(-0.51747870770078,3.35514622044529,14.789651859508));
#48866=CARTESIAN_POINT('Ctrl Pts',(-0.563782537863657,2.4219910006092,14.3869985608885));
#48867=CARTESIAN_POINT('Ctrl Pts',(50.1879275126212,-1.49481431510623,14.4086155358576));
#48868=CARTESIAN_POINT('Ctrl Pts',(50.1416236824583,-2.42437573699871,14.657126746118));
#48869=CARTESIAN_POINT('Ctrl Pts',(50.0490160221326,-4.15622242562869,15.626468992461));
#48870=CARTESIAN_POINT('Ctrl Pts',(49.9101045316439,-5.74188231084713,18.1477843485781));
#48871=CARTESIAN_POINT('Ctrl Pts',(49.7711930411553,-5.92838412080803,21.119653019206));
#48872=CARTESIAN_POINT('Ctrl Pts',(49.6322815506666,-4.67064658961787,23.8190818184562));
#48873=CARTESIAN_POINT('Ctrl Pts',(49.4933700601781,-2.27491795726246,25.5878760504486));
#48874=CARTESIAN_POINT('Ctrl Pts',(49.3544585696894,0.675028376212077,25.9953595672789));
#48875=CARTESIAN_POINT('Ctrl Pts',(49.2155470792007,3.46053014062925,24.9421218159042));
#48876=CARTESIAN_POINT('Ctrl Pts',(49.0766355887121,5.40291951718768,22.6848356335654));
#48877=CARTESIAN_POINT('Ctrl Pts',(48.9377240982235,6.02897544482311,19.7734193215803));
#48878=CARTESIAN_POINT('Ctrl Pts',(48.7988126077348,5.18616303870463,16.9172117672766));
#48879=CARTESIAN_POINT('Ctrl Pts',(48.6599011172463,3.07982354562869,14.8120747229625));
#48880=CARTESIAN_POINT('Ctrl Pts',(48.5209896267576,0.223132321734829,13.9708966672272));
#48881=CARTESIAN_POINT('Ctrl Pts',(48.3820781362689,-2.68792136079287,14.5986152845737));
#48882=CARTESIAN_POINT('Ctrl Pts',(48.2431666457803,-4.94410486103247,16.5422978414445));
#48883=CARTESIAN_POINT('Ctrl Pts',(48.1042551552916,-5.99573388351791,19.3283956606948));
#48884=CARTESIAN_POINT('Ctrl Pts',(47.965343664803,-5.58659544429675,22.2781195539676));
#48885=CARTESIAN_POINT('Ctrl Pts',(47.8264321743144,-3.81636972057899,24.6728149267706));
#48886=CARTESIAN_POINT('Ctrl Pts',(47.6875206838257,-1.11634475998348,25.9290514987144));
#48887=CARTESIAN_POINT('Ctrl Pts',(47.5486091933372,1.85566027843902,25.7407666885868));
#48888=CARTESIAN_POINT('Ctrl Pts',(47.4096977028485,4.37556249064878,24.1538331878717));
#48889=CARTESIAN_POINT('Ctrl Pts',(47.2707862123599,5.8294268192874,21.5548827019868));
#48890=CARTESIAN_POINT('Ctrl Pts',(47.1318747218713,5.86304178530974,18.5771091818944));
#48891=CARTESIAN_POINT('Ctrl Pts',(46.9929632313825,4.46821762491516,15.9460009230928));
#48892=CARTESIAN_POINT('Ctrl Pts',(46.854051740894,1.98478159430525,14.3025866149454));
#48893=CARTESIAN_POINT('Ctrl Pts',(46.7151402504053,-0.982215664530275,
14.0472586444028));
#48894=CARTESIAN_POINT('Ctrl Pts',(46.5762287599167,-3.70991132238189,15.2422237087116));
#48895=CARTESIAN_POINT('Ctrl Pts',(46.437317269428,-5.53374467057676,17.5963471176458));
#48896=CARTESIAN_POINT('Ctrl Pts',(46.2984057789394,-6.00936702281833,20.5360832426609));
#48897=CARTESIAN_POINT('Ctrl Pts',(46.1594942884507,-5.02090037542599,23.3452110064999));
#48898=CARTESIAN_POINT('Ctrl Pts',(46.0205827979622,-2.80916928438035,25.3393300319128));
#48899=CARTESIAN_POINT('Ctrl Pts',(45.8816713074734,0.0869722997749769,
26.0326041704263));
#48900=CARTESIAN_POINT('Ctrl Pts',(45.7427598169849,2.96192443304577,25.2561279389783));
#48901=CARTESIAN_POINT('Ctrl Pts',(45.6038483264962,5.11524965225304,23.1990777191409));
#48902=CARTESIAN_POINT('Ctrl Pts',(45.4649368360076,6.02232369096466,20.362621868101));
#48903=CARTESIAN_POINT('Ctrl Pts',(45.3260253455189,5.46215203896315,17.4378188273991));
#48904=CARTESIAN_POINT('Ctrl Pts',(45.1871138550303,3.57121182445256,15.1372514600414));
#48905=CARTESIAN_POINT('Ctrl Pts',(45.0482023645417,0.810201280126699,14.0214172964104));
#48906=CARTESIAN_POINT('Ctrl Pts',(44.909290874053,-2.14820223041581,14.3621720108524));
#48907=CARTESIAN_POINT('Ctrl Pts',(44.7703793835644,-4.58322961122835,16.0764960062797));
#48908=CARTESIAN_POINT('Ctrl Pts',(44.6314678930757,-5.90162423669546,18.7467208503976));
#48909=CARTESIAN_POINT('Ctrl Pts',(44.4925564025871,-5.78217972002354,21.7222877063162));
#48910=CARTESIAN_POINT('Ctrl Pts',(44.3536449120985,-4.25399686371996,24.2782458953922));
#48911=CARTESIAN_POINT('Ctrl Pts',(44.2147334216098,-1.68939370075548,25.7918758776261));
#48912=CARTESIAN_POINT('Ctrl Pts',(44.0758219311212,1.28680401516706,25.8944052019291));
#48913=CARTESIAN_POINT('Ctrl Pts',(43.9369104406326,3.94949190615626,24.5608541898624));
#48914=CARTESIAN_POINT('Ctrl Pts',(43.7979989501439,5.649947396966,22.1161218465619));
#48915=CARTESIAN_POINT('Ctrl Pts',(43.6590874596554,5.97388090118906,19.1558292611159));
#48916=CARTESIAN_POINT('Ctrl Pts',(43.5201759691666,4.84237104851417,16.4012057732497));
#48917=CARTESIAN_POINT('Ctrl Pts',(43.3812644786781,2.53109265161001,14.5233726393934));
#48918=CARTESIAN_POINT('Ctrl Pts',(43.2423529881893,-0.396847183044917,
13.9798347554831));
#48919=CARTESIAN_POINT('Ctrl Pts',(43.1034414977008,-3.22810136128653,14.9030166903119));
#48920=CARTESIAN_POINT('Ctrl Pts',(42.9645300072121,-5.27287874841191,17.0679994947944));
#48921=CARTESIAN_POINT('Ctrl Pts',(42.8256185167235,-6.03300107243133,19.9473187127923));
#48922=CARTESIAN_POINT('Ctrl Pts',(42.6867070262348,-5.32327632747411,22.8394729087162));
#48923=CARTESIAN_POINT('Ctrl Pts',(42.5477955357463,-3.31661793152758,25.0398336038256));
#48924=CARTESIAN_POINT('Ctrl Pts',(42.4088840452575,-0.501917056051616,
26.0123170680549));
#48925=CARTESIAN_POINT('Ctrl Pts',(42.269972554769,2.43506811953463,25.5199927999233));
#48926=CARTESIAN_POINT('Ctrl Pts',(42.1310610642802,4.7787867441481,23.6828079656607));
#48927=CARTESIAN_POINT('Ctrl Pts',(41.9921495737917,5.95822815335576,20.9483641339372));
#48928=CARTESIAN_POINT('Ctrl Pts',(41.853238083303,5.68603975471807,17.9828661011859));
#48929=CARTESIAN_POINT('Ctrl Pts',(41.7143265928144,4.02853602674152,15.5088114335707));
#48930=CARTESIAN_POINT('Ctrl Pts',(41.5754151023257,1.38954202550255,14.1289651493675));
#48931=CARTESIAN_POINT('Ctrl Pts',(41.4365036118372,-1.58799232222133,14.1795053781877));
#48932=CARTESIAN_POINT('Ctrl Pts',(41.2975921213485,-4.17863698894705,15.6481187777488));
#48933=CARTESIAN_POINT('Ctrl Pts',(41.1586806308599,-5.75122161278835,18.177000488597));
#48934=CARTESIAN_POINT('Ctrl Pts',(41.0197691403712,-5.92261035930397,21.1500277343807));
#48935=CARTESIAN_POINT('Ctrl Pts',(40.8808576498826,-4.65104702064691,23.8428685730469));
#48936=CARTESIAN_POINT('Ctrl Pts',(40.7419461593939,-2.24632826747982,25.5994541316722));
#48937=CARTESIAN_POINT('Ctrl Pts',(40.6030346689053,0.705673501266786,25.9918196040593));
#48938=CARTESIAN_POINT('Ctrl Pts',(40.4641231784166,3.48574887466908,24.924371233033));
#48939=CARTESIAN_POINT('Ctrl Pts',(40.3252116879281,5.41657563944215,22.6571762456001));
#48940=CARTESIAN_POINT('Ctrl Pts',(40.1863001974394,6.02773782402709,19.7426015097702));
#48941=CARTESIAN_POINT('Ctrl Pts',(40.0473887069508,5.17033524841463,16.8907379208274));
#48942=CARTESIAN_POINT('Ctrl Pts',(39.9084772164621,3.05326074182299,14.7963977764992));
#48943=CARTESIAN_POINT('Ctrl Pts',(39.7695657259735,0.192306647226999,13.9698345452706));
#48944=CARTESIAN_POINT('Ctrl Pts',(39.6306542354848,-2.71549997704331,14.6124275287791));
#48945=CARTESIAN_POINT('Ctrl Pts',(39.4917427449962,-4.96171718103282,16.5676189207165));
#48946=CARTESIAN_POINT('Ctrl Pts',(39.3528312545075,-5.99908900805755,19.3590566862954));
#48947=CARTESIAN_POINT('Ctrl Pts',(39.213919764019,-5.57487591421802,22.3066503417405));
#48948=CARTESIAN_POINT('Ctrl Pts',(39.0750082735303,-3.7924308353277,24.6922644445124));
#48949=CARTESIAN_POINT('Ctrl Pts',(38.9360967830417,-1.08601884831338,25.9346811472132));
#48950=CARTESIAN_POINT('Ctrl Pts',(38.797185292553,1.88498477425381,25.7312049046261));
#48951=CARTESIAN_POINT('Ctrl Pts',(38.6582738020644,4.39674111470739,24.1314095449642));
#48952=CARTESIAN_POINT('Ctrl Pts',(38.5193623115757,5.8372997273778,21.5250603760948));
#48953=CARTESIAN_POINT('Ctrl Pts',(38.3804508210871,5.85569086617989,18.5471539180915));
#48954=CARTESIAN_POINT('Ctrl Pts',(38.2415393305985,4.44743381560593,15.9232108573309));
#48955=CARTESIAN_POINT('Ctrl Pts',(38.1026278401099,1.95562854751085,14.292514192559));
#48956=CARTESIAN_POINT('Ctrl Pts',(37.9637163496212,-1.01263526154179,14.0523578549931));
#48957=CARTESIAN_POINT('Ctrl Pts',(37.8248048591326,-3.73418620692178,15.2612522086511));
#48958=CARTESIAN_POINT('Ctrl Pts',(37.6858933686439,-5.54596064383431,17.6246689083371));
#48959=CARTESIAN_POINT('Ctrl Pts',(37.5469818781554,-6.00654785251142,20.5667981593741));
#48960=CARTESIAN_POINT('Ctrl Pts',(37.4080703876666,-5.00373290864692,23.3708358365401));
#48961=CARTESIAN_POINT('Ctrl Pts',(37.2691588971781,-2.78183610793918,25.3536216831735));
#48962=CARTESIAN_POINT('Ctrl Pts',(37.1302474066894,0.11781188169383,26.0320807039123));
#48963=CARTESIAN_POINT('Ctrl Pts',(36.9913359162008,2.98875683499064,25.2409168891785));
#48964=CARTESIAN_POINT('Ctrl Pts',(36.8524244257121,5.13153757597372,23.1728850222391));
#48965=CARTESIAN_POINT('Ctrl Pts',(36.7135129352235,6.02409883666274,20.331828968142));
#48966=CARTESIAN_POINT('Ctrl Pts',(36.5746014447349,5.44898191994243,17.4099279365006));
#48967=CARTESIAN_POINT('Ctrl Pts',(36.4356899542462,3.54630513579011,15.1190577608572));
#48968=CARTESIAN_POINT('Ctrl Pts',(36.2967784637576,0.779626149921396,14.01735340135));
#48969=CARTESIAN_POINT('Ctrl Pts',(36.1578669732689,-2.17699664626686,14.3732280248688));
#48970=CARTESIAN_POINT('Ctrl Pts',(36.0189554827803,-4.60322800024078,16.0999783031656));
#48971=CARTESIAN_POINT('Ctrl Pts',(35.8800439922917,-5.90795430179505,18.7769083330016));
#48972=CARTESIAN_POINT('Ctrl Pts',(35.741132501803,-5.773299239102,21.7518256630623));
#48973=CARTESIAN_POINT('Ctrl Pts',(35.6022210113144,-4.23206942811386,24.299937861598));
#48974=CARTESIAN_POINT('Ctrl Pts',(35.4633095208257,-1.65976158979958,25.8004369424213));
#48975=CARTESIAN_POINT('Ctrl Pts',(35.3243980303371,1.31692139757858,25.8877495947585));
#48976=CARTESIAN_POINT('Ctrl Pts',(35.1854865398485,3.97275692727123,24.5406034461069));
#48977=CARTESIAN_POINT('Ctrl Pts',(35.0465750493599,5.66069189550199,22.0872097456119));
#48978=CARTESIAN_POINT('Ctrl Pts',(34.9076635588712,5.96948714685048,19.1252997876036));
#48979=CARTESIAN_POINT('Ctrl Pts',(34.7687520683826,4.82390951134718,16.3764969595275));
#48980=CARTESIAN_POINT('Ctrl Pts',(34.6298405778939,2.50306119859119,14.5105044044023));
#48981=CARTESIAN_POINT('Ctrl Pts',(34.4909290874054,-0.427619123482817,
13.9819422449422));
#48982=CARTESIAN_POINT('Ctrl Pts',(34.3520175969166,-3.25411668348805,14.9195864471262));
#48983=CARTESIAN_POINT('Ctrl Pts',(34.2131061064281,-5.28779922292417,17.0949945549067));
#48984=CARTESIAN_POINT('Ctrl Pts',(34.0741946159393,-6.03319155723031,19.9781621488148));
#48985=CARTESIAN_POINT('Ctrl Pts',(33.9352831254508,-5.30869041389517,22.8666501962041));
#48986=CARTESIAN_POINT('Ctrl Pts',(33.7963716349621,-3.29080925101633,25.0567234185196));
#48987=CARTESIAN_POINT('Ctrl Pts',(33.6574601444735,-0.471173493020488,
26.0148044687633));
#48988=CARTESIAN_POINT('Ctrl Pts',(33.5185486539849,2.4632563731449,25.507471770072));
#48989=CARTESIAN_POINT('Ctrl Pts',(33.3796371634962,4.79755205787445,23.6583290598256));
#48990=CARTESIAN_POINT('Ctrl Pts',(33.2407256730076,5.96299864977798,20.9178912575711));
#48991=CARTESIAN_POINT('Ctrl Pts',(33.1018141825189,5.67565317642903,17.9538234976253));
#48992=CARTESIAN_POINT('Ctrl Pts',(32.9629026920303,4.00552290232418,15.488274882383));
#48993=CARTESIAN_POINT('Ctrl Pts',(32.8239912015417,1.35950914551882,14.1219380624878));
#48994=CARTESIAN_POINT('Ctrl Pts',(32.685079711053,-1.61772791272423,14.187699796262));
#48995=CARTESIAN_POINT('Ctrl Pts',(32.5461682205644,-4.20083067488945,15.6695382580044));
#48996=CARTESIAN_POINT('Ctrl Pts',(32.4072567300758,-5.76046624707371,18.2064265071361));
#48997=CARTESIAN_POINT('Ctrl Pts',(32.2683452395871,-5.91665363028091,21.1802910985275));
#48998=CARTESIAN_POINT('Ctrl Pts',(32.1294337490985,-4.63134019288346,23.8665960838652));
#48999=CARTESIAN_POINT('Ctrl Pts',(31.9905222586099,-2.21767260367744,25.6108649494421));
#49000=CARTESIAN_POINT('Ctrl Pts',(31.8516107681212,0.736296493406706,25.9881336601462));
#49001=CARTESIAN_POINT('Ctrl Pts',(31.7126992776326,3.51087837843202,24.9064865504593));
#49002=CARTESIAN_POINT('Ctrl Pts',(31.5737877871439,5.4300892412884,22.6294501496745));
#49003=CARTESIAN_POINT('Ctrl Pts',(31.4348762966553,6.02634314462065,19.7117890334094));
#49004=CARTESIAN_POINT('Ctrl Pts',(31.2959648061666,5.1543720797451,16.8643460456352));
#49005=CARTESIAN_POINT('Ctrl Pts',(31.157053315678,3.02661826216146,14.7808564732199));
#49006=CARTESIAN_POINT('Ctrl Pts',(31.0181418251894,0.161475883206934,13.9689302112211));
#49007=CARTESIAN_POINT('Ctrl Pts',(30.8792303347008,-2.74300758831371,14.6263804909137));
#49008=CARTESIAN_POINT('Ctrl Pts',(30.7403188442121,-4.9791998370319,16.5930297563846));
#49009=CARTESIAN_POINT('Ctrl Pts',(30.6014073537235,-6.00228733101139,19.3897344398054));
#49010=CARTESIAN_POINT('Ctrl Pts',(30.4624958632348,-5.56301068238225,22.3351208546198));
#49011=CARTESIAN_POINT('Ctrl Pts',(30.3235843727462,-3.76839282827076,24.7115913182084));
#49012=CARTESIAN_POINT('Ctrl Pts',(30.1846728822576,-1.0556645533444,25.9401556889354));
#49013=CARTESIAN_POINT('Ctrl Pts',(30.0457613917689,1.91426000431534,25.721493327258));
#49014=CARTESIAN_POINT('Ctrl Pts',(29.9068499012803,4.41780482445776,24.1088779235914));
#49015=CARTESIAN_POINT('Ctrl Pts',(29.7679384107917,5.84502007088054,21.4951981905363));
#49016=CARTESIAN_POINT('Ctrl Pts',(29.629026920303,5.84818690157327,18.5172366263472));
#49017=CARTESIAN_POINT('Ctrl Pts',(29.4901154298144,4.42653376739224,15.9005273431677));
#49018=CARTESIAN_POINT('Ctrl Pts',(29.3512039393257,1.92642438803342,14.2825909421164));
#49019=CARTESIAN_POINT('Ctrl Pts',(29.2122924488371,-1.04302839212392,14.0576125142159));
#49020=CARTESIAN_POINT('Ctrl Pts',(29.0733809583485,-3.75836349409478,15.2804045613808));
#49021=CARTESIAN_POINT('Ctrl Pts',(28.9344694678598,-5.55803166685062,17.6530527811079));
#49022=CARTESIAN_POINT('Ctrl Pts',(28.7955579773712,-6.00357169397569,20.5974982621509));
#49023=CARTESIAN_POINT('Ctrl Pts',(28.6566464868826,-4.9864346633914,23.3963725657984));
#49024=CARTESIAN_POINT('Ctrl Pts',(28.5177349963939,-2.75443022492254,25.3677734112025));
#49025=CARTESIAN_POINT('Ctrl Pts',(28.3788235059053,0.148648384459986,26.0313995818365));
#49026=CARTESIAN_POINT('Ctrl Pts',(28.2399120154167,3.01551112224173,25.2255688618193));
#49027=CARTESIAN_POINT('Ctrl Pts',(28.101000524928,5.14769138089252,23.1466093982356));
#49028=CARTESIAN_POINT('Ctrl Pts',(27.9620890344394,6.02571653541499,20.3010273954406));
#49029=CARTESIAN_POINT('Ctrl Pts',(27.8231775439507,5.43566938533659,17.3821047401979));
#49030=CARTESIAN_POINT('Ctrl Pts',(27.6842660534621,3.52130576024992,15.1009916308696));
#49031=CARTESIAN_POINT('Ctrl Pts',(27.5453545629735,0.749030643264908,14.0134458698321));
#49032=CARTESIAN_POINT('Ctrl Pts',(27.4064430724849,-2.20573416373653,14.3844311012236));
#49033=CARTESIAN_POINT('Ctrl Pts',(27.2675315819962,-4.62310607844673,16.1235625317299));
#49034=CARTESIAN_POINT('Ctrl Pts',(27.1286200915076,-5.91412995552358,18.8071277825525));
#49035=CARTESIAN_POINT('Ctrl Pts',(26.9897086010189,-5.76426786617869,21.7813178337734));
#49036=CARTESIAN_POINT('Ctrl Pts',(26.8507971105303,-4.21003138236937,24.3215174438436));
#49037=CARTESIAN_POINT('Ctrl Pts',(26.7118856200417,-1.63008609901205,25.8088464059387));
#49038=CARTESIAN_POINT('Ctrl Pts',(26.572974129553,1.34700436069226,25.8809401042907));
#49039=CARTESIAN_POINT('Ctrl Pts',(26.4340626390644,3.99591811568663,24.5202340283117));
#49040=CARTESIAN_POINT('Ctrl Pts',(26.2951511485758,5.67128844516229,22.0582430929674));
#49041=CARTESIAN_POINT('Ctrl Pts',(26.1562396580871,5.9649373729072,19.0947931754155));
#49042=CARTESIAN_POINT('Ctrl Pts',(26.0173281675985,4.80532189560143,16.3518828503414));
#49043=CARTESIAN_POINT('Ctrl Pts',(25.8784166771098,2.47496432510841,14.4977796438692));
#49044=CARTESIAN_POINT('Ctrl Pts',(25.7395051866212,-0.458379887589252,
13.9842070234562));
#49045=CARTESIAN_POINT('Ctrl Pts',(25.6005936961326,-3.28004695550241,14.9362889865555));
#49046=CARTESIAN_POINT('Ctrl Pts',(25.4616822056439,-5.30258149455159,17.1220655407709));
#49047=CARTESIAN_POINT('Ctrl Pts',(25.3227707151553,-6.03322435743451,20.0090061555954));
#49048=CARTESIAN_POINT('Ctrl Pts',(25.1838592246667,-5.29396575141546,22.8937525603996));
#49049=CARTESIAN_POINT('Ctrl Pts',(25.044947734178,-3.2649145613144,25.0734810697683));
#49050=CARTESIAN_POINT('Ctrl Pts',(24.9060362436894,-0.440417615313074,
26.0171346654451));
#49051=CARTESIAN_POINT('Ctrl Pts',(24.7671247532008,2.49138024663732,25.4948067959342));
#49052=CARTESIAN_POINT('Ctrl Pts',(24.6282132627121,4.81619198190525,23.633754539235));
#49053=CARTESIAN_POINT('Ctrl Pts',(24.4893017722235,5.96761329618002,20.8873943910319));
#49054=CARTESIAN_POINT('Ctrl Pts',(24.3503902817348,5.66511825823355,17.9248343733069));
#49055=CARTESIAN_POINT('Ctrl Pts',(24.2114787912462,3.98240508882984,15.4678562504658));
#49056=CARTESIAN_POINT('Ctrl Pts',(24.0725673007576,1.32944073315618,14.1150646057068));
#49057=CARTESIAN_POINT('Ctrl Pts',(23.9336558102689,-1.64742122199533,14.1960461256744));
#49058=CARTESIAN_POINT('Ctrl Pts',(23.7947443197803,-4.2229145671552,15.6910709199979));
#49059=CARTESIAN_POINT('Ctrl Pts',(23.6558328292916,-5.7695603247627,18.235899402839));
#49060=CARTESIAN_POINT('Ctrl Pts',(23.516921338803,-5.91054226251958,21.2105236143708));
#49061=CARTESIAN_POINT('Ctrl Pts',(23.3780098483144,-4.61151231956818,23.8902225366231));
#49062=CARTESIAN_POINT('Ctrl Pts',(23.2390983578258,-2.1889589783795,25.6221291206225));
#49063=CARTESIAN_POINT('Ctrl Pts',(23.1001868673371,0.766900241567219,25.9842912092798));
#49064=CARTESIAN_POINT('Ctrl Pts',(22.9612753768485,3.5359161212374,24.8884736310584));
#49065=CARTESIAN_POINT('Ctrl Pts',(22.8223638863598,5.44346092133198,22.6016553299603));
#49066=CARTESIAN_POINT('Ctrl Pts',(22.6834523958712,6.02479095961078,19.6809840897829));
#49067=CARTESIAN_POINT('Ctrl Pts',(22.5445409053826,5.13827419546692,16.8380361244666));
#49068=CARTESIAN_POINT('Ctrl Pts',(22.4056294148939,2.99989667825315,14.7654515784277));
#49069=CARTESIAN_POINT('Ctrl Pts',(22.2667179244053,0.130640898823814,13.9681835063114));
#49070=CARTESIAN_POINT('Ctrl Pts',(22.1278064339167,-2.77044350783753,14.6404738989477));
#49071=CARTESIAN_POINT('Ctrl Pts',(21.988894943428,-4.99655235575603,16.6185296372483));
#49072=CARTESIAN_POINT('Ctrl Pts',(21.8499834529394,-6.00532877708893,19.4204281433272));
#49073=CARTESIAN_POINT('Ctrl Pts',(21.7110719624507,-5.55100005468478,22.3635303363547));
#49074=CARTESIAN_POINT('Ctrl Pts',(21.5721604719621,-3.74425632981162,24.7307950488945));
#49075=CARTESIAN_POINT('Ctrl Pts',(21.4332489814735,-1.02528266733415,25.9454749776653));
#49076=CARTESIAN_POINT('Ctrl Pts',(21.2943374909848,1.94348520292825,25.7116322118969));
#49077=CARTESIAN_POINT('Ctrl Pts',(21.1554260004962,4.43875306965556,24.0862389118361));
#49078=CARTESIAN_POINT('Ctrl Pts',(21.0165145100075,5.85258764787277,21.4652969262053));
#49079=CARTESIAN_POINT('Ctrl Pts',(20.877603019519,5.84053008768728,18.4873580883768));
#49080=CARTESIAN_POINT('Ctrl Pts',(20.7386915290303,4.4055180264847,15.8779509735693));
#49081=CARTESIAN_POINT('Ctrl Pts',(20.5997800385417,1.89716987917683,14.2728171229195));
#49082=CARTESIAN_POINT('Ctrl Pts',(20.460868548053,-1.07339426192582,14.0630224847618));
#49083=CARTESIAN_POINT('Ctrl Pts',(20.3219570575644,-3.78244255199411,15.2996802663177));
#49084=CARTESIAN_POINT('Ctrl Pts',(20.1830455670757,-5.56995742413767,17.6814979941192));
#49085=CARTESIAN_POINT('Ctrl Pts',(20.0441340765871,-6.00043862499533,20.628182748604));
#49086=CARTESIAN_POINT('Ctrl Pts',(19.9052225860985,-4.96900609177015,23.421820526844));
#49087=CARTESIAN_POINT('Ctrl Pts',(19.7663110956098,-2.72695235161518,25.3817848461268));
#49088=CARTESIAN_POINT('Ctrl Pts',(19.6273996051212,0.179481002124917,26.0305608220012));
#49089=CARTESIAN_POINT('Ctrl Pts',(19.4884881146326,3.04218659554424,25.2100842580395));
#49090=CARTESIAN_POINT('Ctrl Pts',(19.3495766241439,5.16371064481064,23.1202515338749));
#49091=CARTESIAN_POINT('Ctrl Pts',(19.2106651336553,6.02717674494101,20.2702179550323));
#49092=CARTESIAN_POINT('Ctrl Pts',(19.0717536431667,5.42221478308436,17.3543499656831));
#49093=CARTESIAN_POINT('Ctrl Pts',(18.932842152678,3.49621435122019,15.083053542258));
#49094=CARTESIAN_POINT('Ctrl Pts',(18.7939306621894,0.718415559806878,14.0096948039848));
#49095=CARTESIAN_POINT('Ctrl Pts',(18.6550191717007,-2.23441403173588,14.3957809471112));
#49096=CARTESIAN_POINT('Ctrl Pts',(18.5161076812121,-4.6428633263092,16.1472480755708));
#49097=CARTESIAN_POINT('Ctrl Pts',(18.3771961907235,-5.92015103647305,18.8373784092292));
#49098=CARTESIAN_POINT('Ctrl Pts',(18.2382847002349,-5.7550858372992,21.8107634476368));
#49099=CARTESIAN_POINT('Ctrl Pts',(18.0993732097462,-4.18788330247692,24.3429840781212));
#49100=CARTESIAN_POINT('Ctrl Pts',(17.9604617192576,-1.60036800399696,25.8171040483872));
#49101=CARTESIAN_POINT('Ctrl Pts',(17.8215502287689,1.37705211825441,25.8739769084999));
#49102=CARTESIAN_POINT('Ctrl Pts',(17.6826387382803,4.01897486605748,24.4997464688555));
#49103=CARTESIAN_POINT('Ctrl Pts',(17.5437272477917,5.68173676899357,22.029222645706));
#49104=CARTESIAN_POINT('Ctrl Pts',(17.404815757303,5.96023169827291,19.0643102218779));
#49105=CARTESIAN_POINT('Ctrl Pts',(17.2659042668144,4.78660868708628,16.3273640890105));
#49106=CARTESIAN_POINT('Ctrl Pts',(17.1269927763257,2.44680276550663,14.4851986903707));
#49107=CARTESIAN_POINT('Ctrl Pts',(16.9880812858371,-0.489128671395442,
13.9866290318326));
#49108=CARTESIAN_POINT('Ctrl Pts',(16.8491697953485,-3.30589149961142,14.9531238720594));
#49109=CARTESIAN_POINT('Ctrl Pts',(16.7102583048598,-5.31722517694209,17.149211744855));
#49110=CARTESIAN_POINT('Ctrl Pts',(16.5713468143712,-6.03309947218664,20.0398499269894));
#49111=CARTESIAN_POINT('Ctrl Pts',(16.4324353238826,-5.27910272488139,22.9207792929506));
#49112=CARTESIAN_POINT('Ctrl Pts',(16.2935238333939,-3.23893453920998,25.0901061195905));
#49113=CARTESIAN_POINT('Ctrl Pts',(16.1546123429053,-0.409650226770401,
26.019307597198));
#49114=CARTESIAN_POINT('Ctrl Pts',(16.0157008524167,2.51943900496133,25.4819982085239));
#49115=CARTESIAN_POINT('Ctrl Pts',(15.876789361928,4.83470602906412,23.6090850461731));
#49116=CARTESIAN_POINT('Ctrl Pts',(15.7378778714394,5.9720719719527,20.856874331391));
#49117=CARTESIAN_POINT('Ctrl Pts',(15.5989663809507,5.65443527547411,17.8958994858958));
#49118=CARTESIAN_POINT('Ctrl Pts',(15.4600548904621,3.95918319046976,15.4475560714841));
#49119=CARTESIAN_POINT('Ctrl Pts',(15.3211433999735,1.299337574288,14.1083449586705));
#49120=CARTESIAN_POINT('Ctrl Pts',(15.1822319094849,-1.67707147396502,14.2045441482838));
#49121=CARTESIAN_POINT('Ctrl Pts',(15.0433204189962,-4.24488808855577,15.7127162009476));
#49122=CARTESIAN_POINT('Ctrl Pts',(14.9044089285076,-5.77850360817088,18.265418405397));
#49123=CARTESIAN_POINT('Ctrl Pts',(14.7654974380189,-5.90427641574779,21.2407244917482));
#49124=CARTESIAN_POINT('Ctrl Pts',(14.6265859475303,-4.59156391892589,23.9137473138154));
#49125=CARTESIAN_POINT('Ctrl Pts',(14.4876744570417,-2.16018814205056,25.6332463508108));
#49126=CARTESIAN_POINT('Ctrl Pts',(14.348762966553,0.797483945883081,25.980292351887));
#49127=CARTESIAN_POINT('Ctrl Pts',(14.2098514760644,3.56086144869418,24.8703329456191));
#49128=CARTESIAN_POINT('Ctrl Pts',(14.0709399855757,5.45669033008824,22.573792512908));
#49129=CARTESIAN_POINT('Ctrl Pts',(13.9320284950871,6.02308130956567,19.6501874840145));
#49130=CARTESIAN_POINT('Ctrl Pts',(13.7931170045985,5.12204201631729,16.8118088449625));
#49131=CARTESIAN_POINT('Ctrl Pts',(13.6542055141098,2.97309668849815,14.7501834947476));
#49132=CARTESIAN_POINT('Ctrl Pts',(13.5152940236212,0.0998024999863045,
13.9675944500576));
#49133=CARTESIAN_POINT('Ctrl Pts',(13.3763825331326,-2.79780701854458,14.6547073845334));
#49134=CARTESIAN_POINT('Ctrl Pts',(13.2374710426439,-5.01377428367657,16.644117896838));
#49135=CARTESIAN_POINT('Ctrl Pts',(13.0985595521553,-6.00821326679838,19.4511369946448));
#49136=CARTESIAN_POINT('Ctrl Pts',(12.9596480616667,-5.53884434503756,22.3918780444297));
#49137=CARTESIAN_POINT('Ctrl Pts',(12.820736571178,-3.72002197078624,24.7498751346585));
#49138=CARTESIAN_POINT('Ctrl Pts',(12.6818250806894,-0.994873984349104,
25.9506388743768));
#49139=CARTESIAN_POINT('Ctrl Pts',(12.5429135902007,1.97265960625756,25.7016218162747));
#49140=CARTESIAN_POINT('Ctrl Pts',(12.4040020997121,4.45958530279366,24.0634931013951));
#49141=CARTESIAN_POINT('Ctrl Pts',(12.2650906092235,5.8600022605669,21.4353573646065));
#49142=CARTESIAN_POINT('Ctrl Pts',(12.1261791187349,5.83272062464183,18.4575190850913));
#49143=CARTESIAN_POINT('Ctrl Pts',(11.9872676282462,4.38438714215463,15.8554823385961));
#49144=CARTESIAN_POINT('Ctrl Pts',(11.8483561377576,1.86786578554228,14.2631929904188));
#49145=CARTESIAN_POINT('Ctrl Pts',(11.7094446472689,-1.10373207729958,14.0685876252347));
#49146=CARTESIAN_POINT('Ctrl Pts',(11.5705331567803,-3.80642275128512,15.3190788196683));
#49147=CARTESIAN_POINT('Ctrl Pts',(11.4316216662916,-5.58173760400173,17.7100038039218));
#49148=CARTESIAN_POINT('Ctrl Pts',(11.292710175803,-5.99714872745679,20.6588508167584));
#49149=CARTESIAN_POINT('Ctrl Pts',(11.1537986853144,-4.9514476492995,23.4471790545641));
#49150=CARTESIAN_POINT('Ctrl Pts',(11.0148871948257,-2.69940320618387,25.3956556217409));
#49151=CARTESIAN_POINT('Ctrl Pts',(10.8759757043371,0.210308928841623,26.0295644463285));
#49152=CARTESIAN_POINT('Ctrl Pts',(10.7370642138485,3.06878255770306,25.1944634825473));
#49153=CARTESIAN_POINT('Ctrl Pts',(10.5981527233599,5.17959494904565,23.0938121180512));
#49154=CARTESIAN_POINT('Ctrl Pts',(10.4592412328712,6.02847942707646,20.2394014521583));
#49155=CARTESIAN_POINT('Ctrl Pts',(10.3203297423826,5.40861846483775,17.3266643383601));
#49156=CARTESIAN_POINT('Ctrl Pts',(10.1814182518939,3.4710315644946,15.0652439638558));
#49157=CARTESIAN_POINT('Ctrl Pts',(10.0425067614053,0.687781699708797,14.0061003018464));
#49158=CARTESIAN_POINT('Ctrl Pts',(9.90359527091665,-2.26303550068255,14.4072772658901));
#49159=CARTESIAN_POINT('Ctrl Pts',(9.76468378042802,-4.66249922744889,16.1710343156385));
#49160=CARTESIAN_POINT('Ctrl Pts',(9.62577228993938,-5.92601738727541,18.8676594223957));
#49161=CARTESIAN_POINT('Ctrl Pts',(9.48686079945074,-5.74575339244678,21.8401617350564));
#49162=CARTESIAN_POINT('Ctrl Pts',(9.34794930896211,-4.16562576730276,24.364337203375));
#49163=CARTESIAN_POINT('Ctrl Pts',(9.20903781847347,-1.57060808147196,25.8252096539433));
#49164=CARTESIAN_POINT('Ctrl Pts',(9.07012632798484,1.40706388493112,25.8668601893775));
#49165=CARTESIAN_POINT('Ctrl Pts',(8.9312148374962,4.04192657576827,24.4791413032051));
#49166=CARTESIAN_POINT('Ctrl Pts',(8.79230334700756,5.69203659391647,22.0001491623115));
#49167=CARTESIAN_POINT('Ctrl Pts',(8.65339185651892,5.95537024593603,19.0338517236991));
#49168=CARTESIAN_POINT('Ctrl Pts',(8.51448036603028,4.7677703748936,16.3029413163616));
#49169=CARTESIAN_POINT('Ctrl Pts',(8.37556887554165,2.41857725582169,14.472761872725));
#49170=CARTESIAN_POINT('Ctrl Pts',(8.23665738505301,-0.519864671245333,
13.9892082067692));
#49171=CARTESIAN_POINT('Ctrl Pts',(8.09774589456439,-3.33164964033728,14.9700906636381));
#49172=CARTESIAN_POINT('Ctrl Pts',(7.95883440407574,-5.3317298873657,17.1764324576609));
#49173=CARTESIAN_POINT('Ctrl Pts',(7.8199229135871,-6.03281690475071,20.0706926568584));
#49174=CARTESIAN_POINT('Ctrl Pts',(7.68101142309848,-5.26410172275582,22.9477296874813));
#49175=CARTESIAN_POINT('Ctrl Pts',(7.54209993260984,-3.21286986372191,25.1065981334708));
#49176=CARTESIAN_POINT('Ctrl Pts',(7.4031884421212,-0.378872131534907,26.0213232072299));
#49177=CARTESIAN_POINT('Ctrl Pts',(7.26427695163256,2.547431914768,25.4690463426086));
#49178=CARTESIAN_POINT('Ctrl Pts',(7.12536546114393,4.8530937154645,23.5843212254063));
#49179=CARTESIAN_POINT('Ctrl Pts',(6.98645397065529,5.97637456056316,20.8263318763263));
#49180=CARTESIAN_POINT('Ctrl Pts',(6.84754248016666,5.64360450736318,17.8670195916395));
#49181=CARTESIAN_POINT('Ctrl Pts',(6.70863098967801,3.93585781417588,15.4273748760072));
#49182=CARTESIAN_POINT('Ctrl Pts',(6.56971949918939,1.26920045569606,14.1017792970049));
#49183=CARTESIAN_POINT('Ctrl Pts',(6.43080800870073,-1.7066778936888,14.2131936419841));
#49184=CARTESIAN_POINT('Ctrl Pts',(6.29189651821211,-4.26675066478705,15.7344735351286));
#49185=CARTESIAN_POINT('Ctrl Pts',(6.15298502772347,-5.7872958635549,18.2949827432956));
#49186=CARTESIAN_POINT('Ctrl Pts',(6.01407353723484,-5.8978562537309,21.270892941324));
#49187=CARTESIAN_POINT('Ctrl Pts',(5.87516204674619,-4.57149551233171,23.9371698005941));
#49188=CARTESIAN_POINT('Ctrl Pts',(5.73625055625756,-2.13136084665032,25.6442163494453));
#49189=CARTESIAN_POINT('Ctrl Pts',(5.59733906576892,0.82804680701318,25.9761371924827));
#49190=CARTESIAN_POINT('Ctrl Pts',(5.45842757528028,3.58571370882673,24.8520649682698));
#49191=CARTESIAN_POINT('Ctrl Pts',(5.31951608479165,5.46977712179084,22.5458624267452));
#49192=CARTESIAN_POINT('Ctrl Pts',(5.18060459430302,6.02121423916907,19.6194000210098));
#49193=CARTESIAN_POINT('Ctrl Pts',(5.04169310381438,5.10567596654349,16.7856648926038));
#49194=CARTESIAN_POINT('Ctrl Pts',(4.90278161332574,2.94621899334588,14.735052621229));
#49195=CARTESIAN_POINT('Ctrl Pts',(4.76387012283711,0.0689614926924268,
13.9671630578554));
#49196=CARTESIAN_POINT('Ctrl Pts',(4.62495863234847,-2.8250974052572,14.6690805756616));
#49197=CARTESIAN_POINT('Ctrl Pts',(4.48604714185984,-5.03086517067809,16.6697938663744));
#49198=CARTESIAN_POINT('Ctrl Pts',(4.34713565137119,-6.01094072475019,19.4818601911461));
#49199=CARTESIAN_POINT('Ctrl Pts',(4.20822416088256,-5.52654387114446,22.4201632379438));
#49200=CARTESIAN_POINT('Ctrl Pts',(4.06931267039393,-3.69569038458819,24.76883107682));
#49201=CARTESIAN_POINT('Ctrl Pts',(3.93040117990529,-0.964439299156375,
25.9556472441051));
#49202=CARTESIAN_POINT('Ctrl Pts',(3.79148968941666,2.0017824517957,25.6914624020259));
#49203=CARTESIAN_POINT('Ctrl Pts',(3.65257819892801,4.48030097939669,24.0406410867557));
#49204=CARTESIAN_POINT('Ctrl Pts',(3.51366670843938,5.86726371517407,21.4053802882495));
#49205=CARTESIAN_POINT('Ctrl Pts',(3.37475521795074,5.82475871654497,18.4277203963609));
#49206=CARTESIAN_POINT('Ctrl Pts',(3.2358437274621,4.36314166668535,15.8331220255067));
#49207=CARTESIAN_POINT('Ctrl Pts',(3.09693223697347,1.83851287302163,14.2537187961239));
#49208=CARTESIAN_POINT('Ctrl Pts',(2.95802074648483,-1.13404104531969,14.074307790239));
#49209=CARTESIAN_POINT('Ctrl Pts',(2.81910925599619,-3.83030346523787,15.3385997143183));
#49210=CARTESIAN_POINT('Ctrl Pts',(2.68019776550755,-5.5933718985126,17.7385694656995));
#49211=CARTESIAN_POINT('Ctrl Pts',(2.54128627501892,-5.99370208742667,20.6895016646407));
#49212=CARTESIAN_POINT('Ctrl Pts',(2.40237478453029,-4.93375979473011,23.4724474870243));
#49213=CARTESIAN_POINT('Ctrl Pts',(2.26346329404166,-2.67178350897306,25.4093853738612));
#49214=CARTESIAN_POINT('Ctrl Pts',(2.12455180355301,0.241131359505999,26.028410484117));
#49215=CARTESIAN_POINT('Ctrl Pts',(1.98564031306438,3.09529831238036,25.1787069371976));
#49216=CARTESIAN_POINT('Ctrl Pts',(1.84672882257574,5.19534388084631,23.0672918544148));
#49217=CARTESIAN_POINT('Ctrl Pts',(1.70781733208711,6.02962454304153,20.2085786673882));
#49218=CARTESIAN_POINT('Ctrl Pts',(1.56890584159847,5.39488079527025,17.2990486307619));
#49219=CARTESIAN_POINT('Ctrl Pts',(1.42999435110983,3.44575803991071,15.047563264792));
#49220=CARTESIAN_POINT('Ctrl Pts',(1.2910828606212,0.65712989973888,14.0026626470471));
#49221=CARTESIAN_POINT('Ctrl Pts',(1.15217137013255,-2.29159789362567,14.4189193836441));
#49222=CARTESIAN_POINT('Ctrl Pts',(1.01325987964392,-4.68201312866807,16.1949213654875));
#49223=CARTESIAN_POINT('Ctrl Pts',(0.874348389155287,-5.93172913021799,
18.8979685830992));
#49224=CARTESIAN_POINT('Ctrl Pts',(0.735436898666651,-5.73627023291581,
21.8695147775384));
#49225=CARTESIAN_POINT('Ctrl Pts',(0.596525408178009,-4.14326042687647,
24.3855706507271));
#49226=CARTESIAN_POINT('Ctrl Pts',(0.457613917689371,-1.54080500599549,
25.833174057334));
#49227=CARTESIAN_POINT('Ctrl Pts',(0.318702427200732,1.43703473556815,25.8595683830997));
#49228=CARTESIAN_POINT('Ctrl Pts',(0.179790936712099,4.06478079616032,24.4584619074674));
#49229=CARTESIAN_POINT('Ctrl Pts',(0.0408794462234644,5.70217161488762,
21.9709388731352));
#49230=CARTESIAN_POINT('Ctrl Pts',(-0.0980320442651723,5.95038457493443,
19.0035870828949));
#49231=CARTESIAN_POINT('Ctrl Pts',(-0.236943534753798,4.74874707354515,
16.278258531722));
#49232=CARTESIAN_POINT('Ctrl Pts',(-0.329551195079558,3.17650145787956,
15.0670768494447));
#49233=CARTESIAN_POINT('Ctrl Pts',(-0.375855025242435,2.29303208829606,
14.6858628259571));
#49234=CARTESIAN_POINT('Ctrl Pts',(50.3758550252424,-1.41074674833726,14.7230720419399));
#49235=CARTESIAN_POINT('Ctrl Pts',(50.3295511950796,-2.2880301273243,14.9576071131239));
#49236=CARTESIAN_POINT('Ctrl Pts',(50.2369435347538,-3.92247867381803,15.8724340640267));
#49237=CARTESIAN_POINT('Ctrl Pts',(50.0980320442652,-5.41896188543471,18.2519519775424));
#49238=CARTESIAN_POINT('Ctrl Pts',(49.9591205537766,-5.59497493220745,21.0566843253696));
#49239=CARTESIAN_POINT('Ctrl Pts',(49.8202090632879,-4.40797189480199,23.6042986761457));
#49240=CARTESIAN_POINT('Ctrl Pts',(49.6812975727993,-2.14697777410166,25.2736168556974));
#49241=CARTESIAN_POINT('Ctrl Pts',(49.5423860823106,0.637065137223345,25.6581837149789));
#49242=CARTESIAN_POINT('Ctrl Pts',(49.403474591822,3.26591175511246,24.6641794978917));
#49243=CARTESIAN_POINT('Ctrl Pts',(49.2645631013333,5.09906218008006,22.533841897014));
#49244=CARTESIAN_POINT('Ctrl Pts',(49.1256516108447,5.68990905334285,19.7861620991407));
#49245=CARTESIAN_POINT('Ctrl Pts',(48.9867401203561,4.89449597134713,17.090586147606));
#49246=CARTESIAN_POINT('Ctrl Pts',(48.8478286298675,2.90661589773406,15.1038408976722));
#49247=CARTESIAN_POINT('Ctrl Pts',(48.7089171393788,0.210583477931158,14.3099702510581));
#49248=CARTESIAN_POINT('Ctrl Pts',(48.5700056488901,-2.5367540845736,14.9023863052417));
#49249=CARTESIAN_POINT('Ctrl Pts',(48.4310941584015,-4.6660510176104,16.7367571827446));
#49250=CARTESIAN_POINT('Ctrl Pts',(48.2921826679129,-5.65853697987053,19.3661663336582));
#49251=CARTESIAN_POINT('Ctrl Pts',(48.1532711774243,-5.27240827015851,22.1499993147008));
#49252=CARTESIAN_POINT('Ctrl Pts',(48.0143596869356,-3.60173910521923,24.4100182858197));
#49253=CARTESIAN_POINT('Ctrl Pts',(47.8754481964471,-1.05356212089668,25.5956047771332));
#49254=CARTESIAN_POINT('Ctrl Pts',(47.7365367059583,1.75129892547251,25.4179090051804));
#49255=CARTESIAN_POINT('Ctrl Pts',(47.5976252154698,4.12948316954712,23.9202238055293));
#49256=CARTESIAN_POINT('Ctrl Pts',(47.458713724981,5.50158293700532,21.467436920898));
#49257=CARTESIAN_POINT('Ctrl Pts',(47.3198022344925,5.53330741511091,18.6571318092182));
#49258=CARTESIAN_POINT('Ctrl Pts',(47.1808907440037,4.21692742804939,16.1739956878171));
#49259=CARTESIAN_POINT('Ctrl Pts',(47.0419792535153,1.87315852680124,14.6230061314821));
#49260=CARTESIAN_POINT('Ctrl Pts',(46.9030677630264,-0.926976374857329,
14.3820376710101));
#49261=CARTESIAN_POINT('Ctrl Pts',(46.764156272538,-3.50126787105187,15.5097985318837));
#49262=CARTESIAN_POINT('Ctrl Pts',(46.6252447820492,-5.22252979601018,17.7315272849312));
#49263=CARTESIAN_POINT('Ctrl Pts',(46.4863332915607,-5.67140339862458,20.5059342045224));
#49264=CARTESIAN_POINT('Ctrl Pts',(46.3474218010719,-4.73852759287644,23.157078108117));
#49265=CARTESIAN_POINT('Ctrl Pts',(46.2085103105834,-2.65118308904264,25.0390489338371));
#49266=CARTESIAN_POINT('Ctrl Pts',(46.0695988200946,0.0820810236181339,
25.6933337013367));
#49267=CARTESIAN_POINT('Ctrl Pts',(45.9306873296062,2.79534736890921,24.9605260826201));
#49268=CARTESIAN_POINT('Ctrl Pts',(45.7917758391174,4.82757071625747,23.019163279578));
#49269=CARTESIAN_POINT('Ctrl Pts',(45.6528643486289,5.68363139060459,20.3422282059583));
#49270=CARTESIAN_POINT('Ctrl Pts',(45.5139528581401,5.15496349614729,17.5819145419136));
#49271=CARTESIAN_POINT('Ctrl Pts',(45.3750413676516,3.37036875955527,15.4107298669796));
#49272=CARTESIAN_POINT('Ctrl Pts',(45.2361298771628,0.764635988488109,14.3576496267665));
#49273=CARTESIAN_POINT('Ctrl Pts',(45.0972183866743,-2.02738847273789,14.6792404762263));
#49274=CARTESIAN_POINT('Ctrl Pts',(44.9583068961856,-4.32547120105949,16.2971517965187));
#49275=CARTESIAN_POINT('Ctrl Pts',(44.819395405697,-5.56972000982934,18.8172046071589));
#49276=CARTESIAN_POINT('Ctrl Pts',(44.6804839152083,-5.45699298962439,21.6254271562914));
#49277=CARTESIAN_POINT('Ctrl Pts',(44.5415724247197,-4.01475432920467,24.0376396081562));
#49278=CARTESIAN_POINT('Ctrl Pts',(44.4026609342311,-1.59438309221228,25.4661438404498));
#49279=CARTESIAN_POINT('Ctrl Pts',(44.2637494437424,1.21443483769103,25.5629069697615));
#49280=CARTESIAN_POINT('Ctrl Pts',(44.1248379532538,3.72737456946171,24.3043541615613));
#49281=CARTESIAN_POINT('Ctrl Pts',(43.9859264627651,5.33219734250401,21.9971122727109));
#49282=CARTESIAN_POINT('Ctrl Pts',(43.8470149722766,5.63791299771413,19.2033049771553));
#49283=CARTESIAN_POINT('Ctrl Pts',(43.7081034817879,4.57003866092117,16.6036000578693));
#49284=CARTESIAN_POINT('Ctrl Pts',(43.5691919912993,2.3887453390794,14.8313752666453));
#49285=CARTESIAN_POINT('Ctrl Pts',(43.4302805008106,-0.374528707284711,
14.3184056659561));
#49286=CARTESIAN_POINT('Ctrl Pts',(43.291369010322,-3.04655464743421,15.189668336859));
#49287=CARTESIAN_POINT('Ctrl Pts',(43.1524575198333,-4.97633483538731,17.2328936530502));
#49288=CARTESIAN_POINT('Ctrl Pts',(43.0135460293447,-5.69370828178274,19.9502814805321));
#49289=CARTESIAN_POINT('Ctrl Pts',(42.8746345388561,-5.0238980812484,22.6797824535675));
#49290=CARTESIAN_POINT('Ctrl Pts',(42.7357230483674,-3.13009309256387,24.7563960265209));
#49291=CARTESIAN_POINT('Ctrl Pts',(42.5968115578789,-0.473689506184257,
25.6741875348767));
#49292=CARTESIAN_POINT('Ctrl Pts',(42.4579000673901,2.29812117591949,25.2095513232916));
#49293=CARTESIAN_POINT('Ctrl Pts',(42.3189885769016,4.51003030421545,23.4756887927831));
#49294=CARTESIAN_POINT('Ctrl Pts',(42.1800770864129,5.62314055214332,20.8950286364474));
#49295=CARTESIAN_POINT('Ctrl Pts',(42.0411655959243,5.36625988513824,18.0963086451907));
#49296=CARTESIAN_POINT('Ctrl Pts',(41.9022541054356,3.8019732904961,15.7613935040425));
#49297=CARTESIAN_POINT('Ctrl Pts',(41.763342614947,1.31139491664314,14.4591490453341));
#49298=CARTESIAN_POINT('Ctrl Pts',(41.6244311244583,-1.49868447359569,14.5068469184063));
#49299=CARTESIAN_POINT('Ctrl Pts',(41.4855196339697,-3.94363265394602,15.8928662768361));
#49300=CARTESIAN_POINT('Ctrl Pts',(41.3466081434811,-5.42777594997247,18.2795250172932));
#49301=CARTESIAN_POINT('Ctrl Pts',(41.2076966529924,-5.58952588399778,21.0853507826221));
#49302=CARTESIAN_POINT('Ctrl Pts',(41.0687851625038,-4.38947459522761,23.6267476762343));
#49303=CARTESIAN_POINT('Ctrl Pts',(40.9298736720151,-2.11999595335694,25.2845437917544));
#49304=CARTESIAN_POINT('Ctrl Pts',(40.7909621815266,0.665986796647139,25.6548428374192));
#49305=CARTESIAN_POINT('Ctrl Pts',(40.6520506910379,3.28971220088311,24.6474271984164));
#49306=CARTESIAN_POINT('Ctrl Pts',(40.5131392005492,5.11195028923897,22.5077380584042));
#49307=CARTESIAN_POINT('Ctrl Pts',(40.3742277100607,5.68874103568606,19.7570774647734));
#49308=CARTESIAN_POINT('Ctrl Pts',(40.235316219572,4.87955832761485,17.0656011762843));
#49309=CARTESIAN_POINT('Ctrl Pts',(40.0964047290834,2.88154697197056,15.0890456143895));
#49310=CARTESIAN_POINT('Ctrl Pts',(39.9574932385947,0.181491423060029,14.3089678622789));
#49311=CARTESIAN_POINT('Ctrl Pts',(39.8185817481061,-2.56278169402701,14.9154217561356));
#49312=CARTESIAN_POINT('Ctrl Pts',(39.6796702576174,-4.68267283004561,16.7606542179057));
#49313=CARTESIAN_POINT('Ctrl Pts',(39.5407587671288,-5.66170341397994,19.3951029993896));
#49314=CARTESIAN_POINT('Ctrl Pts',(39.4018472766402,-5.26134784025525,22.1769255460536));
#49315=CARTESIAN_POINT('Ctrl Pts',(39.2629357861515,-3.57914653021792,24.4283739729666));
#49316=CARTESIAN_POINT('Ctrl Pts',(39.1240242956629,-1.02494172246551,25.6009178171769));
#49317=CARTESIAN_POINT('Ctrl Pts',(38.9851128051742,1.77897422714662,25.4088849708944));
#49318=CARTESIAN_POINT('Ctrl Pts',(38.8462013146857,4.14947071898586,23.8990612564435));
#49319=CARTESIAN_POINT('Ctrl Pts',(38.707289824197,5.50901307690715,21.4392917868471));
#49320=CARTESIAN_POINT('Ctrl Pts',(38.5683783337084,5.52636990778647,18.6288612136141));
#49321=CARTESIAN_POINT('Ctrl Pts',(38.4294668432197,4.19731248918724,16.1524873233045));
#49322=CARTESIAN_POINT('Ctrl Pts',(38.2905553527311,1.84564503194526,14.6135001768054));
#49323=CARTESIAN_POINT('Ctrl Pts',(38.1516438622425,-0.955685189815839,
14.3868501046929));
#49324=CARTESIAN_POINT('Ctrl Pts',(38.0127323717538,-3.52417754891945,15.527756879047));
#49325=CARTESIAN_POINT('Ctrl Pts',(37.8738208812652,-5.23405874939034,17.7582562730879));
#49326=CARTESIAN_POINT('Ctrl Pts',(37.7349093907765,-5.66874277696523,20.5349217305587));
#49327=CARTESIAN_POINT('Ctrl Pts',(37.5959979002879,-4.72232561535253,23.1812618112637));
#49328=CARTESIAN_POINT('Ctrl Pts',(37.4570864097993,-2.62538711599339,25.0525368301869));
#49329=CARTESIAN_POINT('Ctrl Pts',(37.3181749193106,0.111186203754847,25.6928396743027));
#49330=CARTESIAN_POINT('Ctrl Pts',(37.179263428822,2.82067073075507,24.9461704942188));
#49331=CARTESIAN_POINT('Ctrl Pts',(37.0403519383333,4.84294261575957,22.9944436461018));
#49332=CARTESIAN_POINT('Ctrl Pts',(36.9014404478447,5.68530670304713,20.3131670824126));
#49333=CARTESIAN_POINT('Ctrl Pts',(36.7625289573561,5.14253405765722,17.5555922199733));
#49334=CARTESIAN_POINT('Ctrl Pts',(36.6236174668674,3.34686280989496,15.3935593718185));
#49335=CARTESIAN_POINT('Ctrl Pts',(36.4847059763788,0.735780387440389,14.3538142830157));
#49336=CARTESIAN_POINT('Ctrl Pts',(36.3457944858902,-2.05456350586516,14.6896747058597));
#49337=CARTESIAN_POINT('Ctrl Pts',(36.2068829954015,-4.34434489124707,16.3193134614429));
#49338=CARTESIAN_POINT('Ctrl Pts',(36.0679715049129,-5.57569407541445,18.8456943617015));
#49339=CARTESIAN_POINT('Ctrl Pts',(35.9290600144243,-5.44861194225475,21.6533039139669));
#49340=CARTESIAN_POINT('Ctrl Pts',(35.7901485239356,-3.99406008098396,24.0581116296512));
#49341=CARTESIAN_POINT('Ctrl Pts',(35.651237033447,-1.56641747550996,25.4742234354871));
#49342=CARTESIAN_POINT('Ctrl Pts',(35.5123255429583,1.24285843443888,25.5566256704194));
#49343=CARTESIAN_POINT('Ctrl Pts',(35.3734140524697,3.74933117808945,24.2852423089279));
#49344=CARTESIAN_POINT('Ctrl Pts',(35.2345025619811,5.34233757612298,21.9698261730325));
#49345=CARTESIAN_POINT('Ctrl Pts',(35.0955910714924,5.63376634579655,19.1744924650922));
#49346=CARTESIAN_POINT('Ctrl Pts',(34.9566795810039,4.55261539084379,16.5802808547672));
#49347=CARTESIAN_POINT('Ctrl Pts',(34.8177680905151,2.36229036015804,14.8192307343866));
#49348=CARTESIAN_POINT('Ctrl Pts',(34.6788566000265,-0.403570050061598,
14.3203946313223));
#49349=CARTESIAN_POINT('Ctrl Pts',(34.5399451095379,-3.07110688166949,15.2053062193106));
#49350=CARTESIAN_POINT('Ctrl Pts',(34.4010336190492,-4.99041619030151,17.258370525254));
#49351=CARTESIAN_POINT('Ctrl Pts',(34.2621221285606,-5.69388805381733,19.9793902980198));
#49352=CARTESIAN_POINT('Ctrl Pts',(34.123210638072,-5.01013247173753,22.7054313047758));
#49353=CARTESIAN_POINT('Ctrl Pts',(33.9842991475833,-3.10573587859945,24.7723359669663));
#49354=CARTESIAN_POINT('Ctrl Pts',(33.8453876570947,-0.444674944883789,
25.6765350454843));
#49355=CARTESIAN_POINT('Ctrl Pts',(33.7064761666061,2.32472413704993,25.1977344695393));
#49356=CARTESIAN_POINT('Ctrl Pts',(33.5675646761174,4.5277402666191,23.45258656767));
#49357=CARTESIAN_POINT('Ctrl Pts',(33.4286531856288,5.62764275836893,20.8662695385371));
#49358=CARTESIAN_POINT('Ctrl Pts',(33.2897416951401,5.35645744252075,18.0688993822994));
#49359=CARTESIAN_POINT('Ctrl Pts',(33.1508302046515,3.78025441202889,15.7420119176358));
#49360=CARTESIAN_POINT('Ctrl Pts',(33.0119187141629,1.28305106995122,14.4525171581053));
#49361=CARTESIAN_POINT('Ctrl Pts',(32.8730072236743,-1.52674775021,14.5145804867405));
#49362=CARTESIAN_POINT('Ctrl Pts',(32.7340957331856,-3.96457817872488,15.9130811368468));
#49363=CARTESIAN_POINT('Ctrl Pts',(32.595184242697,-5.43650067091328,18.3072961321073));
#49364=CARTESIAN_POINT('Ctrl Pts',(32.4562727522083,-5.58390415826564,21.1139121511696));
#49365=CARTESIAN_POINT('Ctrl Pts',(32.3173612617197,-4.37087606903851,23.6491407643891));
#49366=CARTESIAN_POINT('Ctrl Pts',(32.1784497712311,-2.09295186893649,25.2953128711658));
#49367=CARTESIAN_POINT('Ctrl Pts',(32.0395382807424,0.694887567899583,25.651364189043));
#49368=CARTESIAN_POINT('Ctrl Pts',(31.9006267902538,3.31342843464045,24.630548340935));
#49369=CARTESIAN_POINT('Ctrl Pts',(31.7617152997652,5.12470389326207,22.4815712634547));
#49370=CARTESIAN_POINT('Ctrl Pts',(31.6228038092765,5.68742479231206,19.7279978657925));
#49371=CARTESIAN_POINT('Ctrl Pts',(31.4838923187879,4.86449291911151,17.0406935661994));
#49372=CARTESIAN_POINT('Ctrl Pts',(31.3449808282992,2.85640285127925,15.0743783457899));
#49373=CARTESIAN_POINT('Ctrl Pts',(31.2060693378107,0.15239456490814,14.3081143874981));
#49374=CARTESIAN_POINT('Ctrl Pts',(31.0671578473219,-2.58874229178292,14.9285900110567));
#49375=CARTESIAN_POINT('Ctrl Pts',(30.9282463568333,-4.69917227071445,16.7846359616106));
#49376=CARTESIAN_POINT('Ctrl Pts',(30.7893348663447,-5.66472186494181,19.4240554522615));
#49377=CARTESIAN_POINT('Ctrl Pts',(30.6504233758561,-5.25014990278475,22.2037948923411));
#49378=CARTESIAN_POINT('Ctrl Pts',(30.5115118853674,-3.55646040796889,24.4466139135042));
#49379=CARTESIAN_POINT('Ctrl Pts',(30.3726003948788,-0.996294536997184,
25.606084473567));
#49380=CARTESIAN_POINT('Ctrl Pts',(30.2336889043902,1.80660303374739,25.3997195675029));
#49381=CARTESIAN_POINT('Ctrl Pts',(30.0947774139015,4.16934981683632,23.8777968015442));
#49382=CARTESIAN_POINT('Ctrl Pts',(29.9558659234129,5.51629923237306,21.4111090348162));
#49383=CARTESIAN_POINT('Ctrl Pts',(29.8169544329242,5.51928796218196,18.6006264545402));
#49384=CARTESIAN_POINT('Ctrl Pts',(29.6780429424356,4.17758784863518,16.131079517985));
#49385=CARTESIAN_POINT('Ctrl Pts',(29.539131451947,1.81808329895651,14.6041350047212));
#49386=CARTESIAN_POINT('Ctrl Pts',(29.4002199614583,-0.984369026802969,
14.3918092446592));
#49387=CARTESIAN_POINT('Ctrl Pts',(29.2613084709697,-3.54699511824443,15.5458321135851));
#49388=CARTESIAN_POINT('Ctrl Pts',(29.122396980481,-5.24545090445421,17.7850438518607));
#49389=CARTESIAN_POINT('Ctrl Pts',(28.9834854899925,-5.66593399601205,20.5638952757866));
#49390=CARTESIAN_POINT('Ctrl Pts',(28.8445739995038,-4.70600021426455,23.2053623683698));
#49391=CARTESIAN_POINT('Ctrl Pts',(28.7056625090152,-2.59952252534805,25.0658926725136));
#49392=CARTESIAN_POINT('Ctrl Pts',(28.5667510185265,0.140288477908783,25.6921968581722));
#49393=CARTESIAN_POINT('Ctrl Pts',(28.4278395280379,2.84592037103622,24.9316856318038));
#49394=CARTESIAN_POINT('Ctrl Pts',(28.2889280375492,4.8581879392303,22.9696457493002));
#49395=CARTESIAN_POINT('Ctrl Pts',(28.1500165470606,5.68683342327686,20.2840977738751));
#49396=CARTESIAN_POINT('Ctrl Pts',(28.0111050565719,5.12997021295922,17.5293337855205));
#49397=CARTESIAN_POINT('Ctrl Pts',(27.8721935660834,3.32326938601791,15.3765092714297));
#49398=CARTESIAN_POINT('Ctrl Pts',(27.7332820755947,0.706905555902332,14.3501265090045));
#49399=CARTESIAN_POINT('Ctrl Pts',(27.5943705851061,-2.08168484054595,14.7002477271234));
#49400=CARTESIAN_POINT('Ctrl Pts',(27.4554590946174,-4.36310503684432,16.3415713254618));
#49401=CARTESIAN_POINT('Ctrl Pts',(27.3165476041288,-5.58152241364238,18.8742142853867));
#49402=CARTESIAN_POINT('Ctrl Pts',(27.1776361136402,-5.44008848896973,21.6811374605898));
#49403=CARTESIAN_POINT('Ctrl Pts',(27.0387246231515,-3.97326144328056,24.0784775876005));
#49404=CARTESIAN_POINT('Ctrl Pts',(26.8998131326629,-1.53841091863481,25.4821599552224));
#49405=CARTESIAN_POINT('Ctrl Pts',(26.7609016421743,1.27124954761199,25.5501991420953));
#49406=CARTESIAN_POINT('Ctrl Pts',(26.6219901516856,3.77118979351376,24.2660184564201));
#49407=CARTESIAN_POINT('Ctrl Pts',(26.483078661197,5.35233818143281,21.942488589618));
#49408=CARTESIAN_POINT('Ctrl Pts',(26.3441671707083,5.62947244873437,19.1457015286446));
#49409=CARTESIAN_POINT('Ctrl Pts',(26.2052556802197,4.53507313278025,16.5570510300682));
#49410=CARTESIAN_POINT('Ctrl Pts',(26.066344189731,2.33577363998504,14.8072216076583));
#49411=CARTESIAN_POINT('Ctrl Pts',(25.9274326992424,-0.432600845057991,
14.3225320398901));
#49412=CARTESIAN_POINT('Ctrl Pts',(25.7885212087538,-3.09557884889517,15.2210694167531));
#49413=CARTESIAN_POINT('Ctrl Pts',(25.6496097182651,-5.00436711478803,17.2839190531857));
#49414=CARTESIAN_POINT('Ctrl Pts',(25.5106982277766,-5.69391900935539,20.0084996541662));
#49415=CARTESIAN_POINT('Ctrl Pts',(25.3717867372879,-4.99623591649071,22.7310094463381));
#49416=CARTESIAN_POINT('Ctrl Pts',(25.2328752467993,-3.08129749255576,24.7881511767684));
#49417=CARTESIAN_POINT('Ctrl Pts',(25.0939637563106,-0.415648761477922,
25.6787341931368));
#49418=CARTESIAN_POINT('Ctrl Pts',(24.955052265822,2.35126633876631,25.1857817668509));
#49419=CARTESIAN_POINT('Ctrl Pts',(24.8161407753333,4.54533189117739,23.4293941051249));
#49420=CARTESIAN_POINT('Ctrl Pts',(24.6772292848448,5.6319978794971,20.8374877996482));
#49421=CARTESIAN_POINT('Ctrl Pts',(24.538317794356,5.34651500255474,18.0415405910062));
#49422=CARTESIAN_POINT('Ctrl Pts',(24.3994063038675,3.75843673214303,15.7227416187822));
#49423=CARTESIAN_POINT('Ctrl Pts',(24.2604948133787,1.25467368920259,14.4460302608997));
#49424=CARTESIAN_POINT('Ctrl Pts',(24.1215833228902,-1.55477112346663,14.5224574229995));
#49425=CARTESIAN_POINT('Ctrl Pts',(23.9826718324015,-3.98542008456542,15.9334028133141));
#49426=CARTESIAN_POINT('Ctrl Pts',(23.8437603419129,-5.4450833024811,18.3351114877383));
#49427=CARTESIAN_POINT('Ctrl Pts',(23.7048488514242,-5.57813649059611,21.1424444063059));
#49428=CARTESIAN_POINT('Ctrl Pts',(23.5659373609356,-4.35216330483543,23.6714384779352));
#49429=CARTESIAN_POINT('Ctrl Pts',(23.4270258704469,-2.06585308274432,25.3059435513144));
#49430=CARTESIAN_POINT('Ctrl Pts',(23.2881143799584,0.723770177443836,25.6477378355818));
#49431=CARTESIAN_POINT('Ctrl Pts',(23.1492028894697,3.33705806802798,24.6135484585977));
#49432=CARTESIAN_POINT('Ctrl Pts',(23.0102913989811,5.13732355708965,22.455339609706));
#49433=CARTESIAN_POINT('Ctrl Pts',(22.8713799084924,5.68595990136651,19.6989253759089));
#49434=CARTESIAN_POINT('Ctrl Pts',(22.7324684180038,4.84930037133414,17.0158633010872));
#49435=CARTESIAN_POINT('Ctrl Pts',(22.5935569275151,2.83118407512215,15.0598398141362));
#49436=CARTESIAN_POINT('Ctrl Pts',(22.4546454370266,0.123293723744183,14.3074096768778));
#49437=CARTESIAN_POINT('Ctrl Pts',(22.3157339465378,-2.61463522969817,14.9418908132741));
#49438=CARTESIAN_POINT('Ctrl Pts',(22.1768224560493,-4.71554889295985,16.8087017426564));
#49439=CARTESIAN_POINT('Ctrl Pts',(22.0379109655606,-5.66759226169997,19.4530229581252));
#49440=CARTESIAN_POINT('Ctrl Pts',(21.898999475072,-5.23881474643893,22.2306066398434));
#49441=CARTESIAN_POINT('Ctrl Pts',(21.7600879845833,-3.53368133342206,24.4647376365296));
#49442=CARTESIAN_POINT('Ctrl Pts',(21.6211764940947,-0.967621312193158,
25.611104608311));
#49443=CARTESIAN_POINT('Ctrl Pts',(21.4822650036061,1.83418462264175,25.3904130360561));
#49444=CARTESIAN_POINT('Ctrl Pts',(21.3433535131174,4.1891199437996,23.8564309958406));
#49445=CARTESIAN_POINT('Ctrl Pts',(21.2044420226288,5.52344121283625,21.3828894017822));
#49446=CARTESIAN_POINT('Ctrl Pts',(21.0655305321402,5.51206176346074,18.5724282697484));
#49447=CARTESIAN_POINT('Ctrl Pts',(20.9266190416515,4.1577540218852,16.1097728314767));
#49448=CARTESIAN_POINT('Ctrl Pts',(20.7877075511629,1.79047404821108,14.5949108599485));
#49449=CARTESIAN_POINT('Ctrl Pts',(20.6487960606742,-1.01302713614174,14.3969149613218));
#49450=CARTESIAN_POINT('Ctrl Pts',(20.5098845701856,-3.56971998265816,15.5640237630674));
#49451=CARTESIAN_POINT('Ctrl Pts',(20.3709730796969,-5.25670596345662,17.8118893211313));
#49452=CARTESIAN_POINT('Ctrl Pts',(20.2320615892084,-5.66297712917468,20.5928540829446));
#49453=CARTESIAN_POINT('Ctrl Pts',(20.0931500987197,-4.68955181629675,23.2293791495406));
#49454=CARTESIAN_POINT('Ctrl Pts',(19.9542386082311,-2.57358999310786,25.0791161117457));
#49455=CARTESIAN_POINT('Ctrl Pts',(19.8153271177424,0.169387085457532,25.6914052697466));
#49456=CARTESIAN_POINT('Ctrl Pts',(19.6764156272538,2.8710956298236,24.9170718739538));
#49457=CARTESIAN_POINT('Ctrl Pts',(19.5375041367652,4.87330628821509,22.9447702372957));
#49458=CARTESIAN_POINT('Ctrl Pts',(19.3985926462765,5.68821151139114,20.2550210401063));
#49459=CARTESIAN_POINT('Ctrl Pts',(19.2596811557879,5.11727229042419,17.5031399248504));
#49460=CARTESIAN_POINT('Ctrl Pts',(19.1207696652992,3.2995891045661,15.3595800114377));
#49461=CARTESIAN_POINT('Ctrl Pts',(18.9818581748106,0.678012248551709,14.3465864011172));
#49462=CARTESIAN_POINT('Ctrl Pts',(18.8429466843219,-2.10875176793216,14.710959263679));
#49463=CARTESIAN_POINT('Ctrl Pts',(18.7040351938334,-4.38175114753269,16.3639248068398));
#49464=CARTESIAN_POINT('Ctrl Pts',(18.5651237033447,-5.58720487218263,18.9027636328128));
#49465=CARTESIAN_POINT('Ctrl Pts',(18.4262122128561,-5.43142285253985,21.7089270686976));
#49466=CARTESIAN_POINT('Ctrl Pts',(18.2873007223674,-3.95235895969151,24.0987369497158));
#49467=CARTESIAN_POINT('Ctrl Pts',(18.1483892318788,-1.51036415357132,25.4899531922255));
#49468=CARTESIAN_POINT('Ctrl Pts',(18.0094777413901,1.29960743517518,25.5436275527543));
#49469=CARTESIAN_POINT('Ctrl Pts',(17.8705662509015,3.79294984443393,24.2466831064759));
#49470=CARTESIAN_POINT('Ctrl Pts',(17.7316547604129,5.36219889705587,21.9151002369674));
#49471=CARTESIAN_POINT('Ctrl Pts',(17.5927432699243,5.62503141875362,19.1169329202976));
#49472=CARTESIAN_POINT('Ctrl Pts',(17.4538317794356,4.51741234521826,16.5339111909114));
#49473=CARTESIAN_POINT('Ctrl Pts',(17.314920288947,2.30919587160617,14.795348200333));
#49474=CARTESIAN_POINT('Ctrl Pts',(17.1760087984583,-0.461620333519894,
14.3248178357959));
#49475=CARTESIAN_POINT('Ctrl Pts',(17.0370973079697,-3.11996990950757,15.236957517197));
#49476=CARTESIAN_POINT('Ctrl Pts',(16.8981858174811,-5.01818724422305,17.3095385691044));
#49477=CARTESIAN_POINT('Ctrl Pts',(16.7592743269924,-5.69380114758782,20.0376087881643));
#49478=CARTESIAN_POINT('Ctrl Pts',(16.6203628365038,-4.98220877871081,22.7565162097395));
#49479=CARTESIAN_POINT('Ctrl Pts',(16.4814513460152,-3.05677857315876,24.8038412425784));
#49480=CARTESIAN_POINT('Ctrl Pts',(16.3425398555265,-0.386611714600087,
25.6807849203568));
#49481=CARTESIAN_POINT('Ctrl Pts',(16.2036283650379,2.37774708735693,25.1736935276246));
#49482=CARTESIAN_POINT('Ctrl Pts',(16.0647168745492,4.56280471811248,23.40611201131));
#49483=CARTESIAN_POINT('Ctrl Pts',(15.9258053840606,5.63620580170163,20.8086841720254));
#49484=CARTESIAN_POINT('Ctrl Pts',(15.786893893572,5.33643282509756,18.0142329863651));
#49485=CARTESIAN_POINT('Ctrl Pts',(15.6479824030833,3.73652082106924,15.7035831111337));
#49486=CARTESIAN_POINT('Ctrl Pts',(15.5090709125947,1.22626351607354,14.43968852326));
#49487=CARTESIAN_POINT('Ctrl Pts',(15.3701594221061,-1.58275386094172,14.5304775213102));
#49488=CARTESIAN_POINT('Ctrl Pts',(15.2312479316174,-4.00615782673987,15.9538307751071));
#49489=CARTESIAN_POINT('Ctrl Pts',(15.0923364411288,-5.45352362035877,18.3629703571992));
#49490=CARTESIAN_POINT('Ctrl Pts',(14.9534249506401,-5.57222303173398,21.1709468023069));
#49491=CARTESIAN_POINT('Ctrl Pts',(14.8145134601515,-4.3333367916985,23.6936402340958));
#49492=CARTESIAN_POINT('Ctrl Pts',(14.6756019696629,-2.03870030303929,25.3164355543547));
#49493=CARTESIAN_POINT('Ctrl Pts',(14.5366904791742,0.752633870398657,25.6439638718146));
#49494=CARTESIAN_POINT('Ctrl Pts',(14.3977789886856,3.36060048345727,24.5964279957165));
#49495=CARTESIAN_POINT('Ctrl Pts',(14.258867498197,5.14980895089188,22.4290437827535));
#49496=CARTESIAN_POINT('Ctrl Pts',(14.1199560077083,5.68434640113603,19.6698607549666));
#49497=CARTESIAN_POINT('Ctrl Pts',(13.9810445172197,4.83398108135788,16.991111029916));
#49498=CARTESIAN_POINT('Ctrl Pts',(13.842133026731,2.80589130262175,15.0454303994099));
#49499=CARTESIAN_POINT('Ctrl Pts',(13.7032215362424,0.094189660152942,14.3068537488363));
#49500=CARTESIAN_POINT('Ctrl Pts',(13.5643100457538,-2.64045983103022,14.9553238151557));
#49501=CARTESIAN_POINT('Ctrl Pts',(13.4253985552652,-4.73180226875942,16.8328509320553));
#49502=CARTESIAN_POINT('Ctrl Pts',(13.2864870647765,-5.67031452923321,19.4820047598806));
#49503=CARTESIAN_POINT('Ctrl Pts',(13.1475755742879,-5.22734266747552,22.2573600878037));
#49504=CARTESIAN_POINT('Ctrl Pts',(13.0086640837993,-3.51080990193549,24.4827446683579));
#49505=CARTESIAN_POINT('Ctrl Pts',(12.8697525933106,-0.938922797462035,
25.6159780902017));
#49506=CARTESIAN_POINT('Ctrl Pts',(12.730841102822,1.86171827295241,25.3809656197912));
#49507=CARTESIAN_POINT('Ctrl Pts',(12.5919296123333,4.20878058316006,23.8349643977531));
#49508=CARTESIAN_POINT('Ctrl Pts',(12.4530181218447,5.5304388316326,21.3546336252986));
#49509=CARTESIAN_POINT('Ctrl Pts',(12.3141066313561,5.50469150048808,18.5442673962318));
#49510=CARTESIAN_POINT('Ctrl Pts',(12.1751951408674,4.13781152731789,16.0885678206551));
#49511=CARTESIAN_POINT('Ctrl Pts',(12.0362836503788,1.76281800130937,14.5858279835714));
#49512=CARTESIAN_POINT('Ctrl Pts',(11.8973721598901,-1.04165876881856,14.4021671212367));
#49513=CARTESIAN_POINT('Ctrl Pts',(11.7584606694015,-3.59235154821945,15.5823313520337));
#49514=CARTESIAN_POINT('Ctrl Pts',(11.6195491789129,-5.26782363223333,17.8387919792617));
#49515=CARTESIAN_POINT('Ctrl Pts',(11.4806376884243,-5.65987225373433,20.6217973951602));
#49516=CARTESIAN_POINT('Ctrl Pts',(11.3417261979356,-4.67298085134745,23.2533115270689));
#49517=CARTESIAN_POINT('Ctrl Pts',(11.202814707447,-2.5475901970503,25.0922068022728));
#49518=CARTESIAN_POINT('Ctrl Pts',(11.0639032169583,0.198481265874501,25.690464929715));
#49519=CARTESIAN_POINT('Ctrl Pts',(10.9249917264697,2.89619584913197,24.9023296026165));
#49520=CARTESIAN_POINT('Ctrl Pts',(10.7860802359811,4.888297267578,22.9198177602393));
#49521=CARTESIAN_POINT('Ctrl Pts',(10.6471687454924,5.68944093137202,20.2259376410611));
#49522=CARTESIAN_POINT('Ctrl Pts',(10.5082572550038,5.10444062192735,17.4770113225705));
#49523=CARTESIAN_POINT('Ctrl Pts',(10.3693457645152,3.27582258445175,15.3427720343089));
#49524=CARTESIAN_POINT('Ctrl Pts',(10.2304342740265,0.649101220549331,14.3431940518787));
#49525=CARTESIAN_POINT('Ctrl Pts',(10.0915227835379,-2.13576358059751,14.7218090355679));
#49526=CARTESIAN_POINT('Ctrl Pts',(9.95261129304924,-4.40028273597386,16.3863733213419));
#49527=CARTESIAN_POINT('Ctrl Pts',(9.8136998025606,-5.5927413025174,18.9313416578085));
#49528=CARTESIAN_POINT('Ctrl Pts',(9.67478831207196,-5.42261525945185,21.7366720119756));
#49529=CARTESIAN_POINT('Ctrl Pts',(9.53587682158334,-3.93135317652793,24.1188891864947));
#49530=CARTESIAN_POINT('Ctrl Pts',(9.3969653310947,-1.48227791335496,25.4976029428106));
#49531=CARTESIAN_POINT('Ctrl Pts',(9.25805384060606,1.3279313559613,25.5369110741526));
#49532=CARTESIAN_POINT('Ctrl Pts',(9.11914235011741,3.81461076212522,24.2272367644477));
#49533=CARTESIAN_POINT('Ctrl Pts',(8.98023085962878,5.37191946527065,21.8876618309077));
#49534=CARTESIAN_POINT('Ctrl Pts',(8.84131936914014,5.62044337192589,19.0881873919529));
#49535=CARTESIAN_POINT('Ctrl Pts',(8.70240787865151,4.49963348974343,16.5108619420839));
#49536=CARTESIAN_POINT('Ctrl Pts',(8.56349638816287,2.282557749663,14.7836108227364));
#49537=CARTESIAN_POINT('Ctrl Pts',(8.42458489767425,-0.490627756988433,
14.3272519592977));
#49538=CARTESIAN_POINT('Ctrl Pts',(8.2856734071856,-3.14427942601743,15.2529701053877));
#49539=CARTESIAN_POINT('Ctrl Pts',(8.14676191669697,-5.03187621740111,17.3352284034138));
#49540=CARTESIAN_POINT('Ctrl Pts',(8.00785042620833,-5.6935344715951,20.0667169392121));
#49541=CARTESIAN_POINT('Ctrl Pts',(7.8689389357197,-4.96805142501369,22.7819509283305));
#49542=CARTESIAN_POINT('Ctrl Pts',(7.73002744523106,-3.03217976123968,24.8194057543175));
#49543=CARTESIAN_POINT('Ctrl Pts',(7.59111595474241,-0.357564563168171,
25.6826871735461));
#49544=CARTESIAN_POINT('Ctrl Pts',(7.45220446425379,2.404165690716,25.1614700678008));
#49545=CARTESIAN_POINT('Ctrl Pts',(7.31329297376515,4.58015829075132,23.3827408947304));
#49546=CARTESIAN_POINT('Ctrl Pts',(7.17438148327652,5.64026641500344,20.7798594084857));
#49547=CARTESIAN_POINT('Ctrl Pts',(7.03546999278788,5.32621117365894,17.9869772820929));
#49548=CARTESIAN_POINT('Ctrl Pts',(6.89655850229923,3.71450725160592,15.6845368954205));
#49549=CARTESIAN_POINT('Ctrl Pts',(6.7576470118106,1.19782129309763,14.4334921109351));
#49550=CARTESIAN_POINT('Ctrl Pts',(6.61873552132196,-1.61069523127324,14.5386405720578));
#49551=CARTESIAN_POINT('Ctrl Pts',(6.47982403083333,-4.02679086324272,15.9743644883169));
#49552=CARTESIAN_POINT('Ctrl Pts',(6.34091254034469,-5.46182140394848,18.3908720123652));
#49553=CARTESIAN_POINT('Ctrl Pts',(6.20200104985606,-5.56616393623456,21.1994185942286));
#49554=CARTESIAN_POINT('Ctrl Pts',(6.06308955936741,-4.31439702168094,23.7157454526016));
#49555=CARTESIAN_POINT('Ctrl Pts',(5.92417806887878,-2.01149423949129,25.3267886060659));
#49556=CARTESIAN_POINT('Ctrl Pts',(5.78526657839015,0.781477892377476,25.6400423963783));
#49557=CARTESIAN_POINT('Ctrl Pts',(5.6463550879015,3.38405506561942,24.579187399755));
#49558=CARTESIAN_POINT('Ctrl Pts',(5.50744359741287,5.16215974834815,22.4026844698698));
#49559=CARTESIAN_POINT('Ctrl Pts',(5.36853210692423,5.68258433379142,19.640804762604));
#49560=CARTESIAN_POINT('Ctrl Pts',(5.22962061643561,4.81853544957058,16.9664373996156));
#49561=CARTESIAN_POINT('Ctrl Pts',(5.09070912594697,2.78052519483453,15.0311504782184));
#49562=CARTESIAN_POINT('Ctrl Pts',(4.95179763545833,0.0650831348035412,
14.3064466179034));
#49563=CARTESIAN_POINT('Ctrl Pts',(4.81288614496969,-2.66621542082262,14.968888665614));
#49564=CARTESIAN_POINT('Ctrl Pts',(4.67397465448106,-4.74793197331199,16.85708289864));
#49565=CARTESIAN_POINT('Ctrl Pts',(4.53506316399242,-5.67288859639181,19.5110001000541));
#49566=CARTESIAN_POINT('Ctrl Pts',(4.39615167350378,-5.21573396573087,22.2840545369891));
#49567=CARTESIAN_POINT('Ctrl Pts',(4.25724018301514,-3.48784671128103,24.5006345383542));
#49568=CARTESIAN_POINT('Ctrl Pts',(4.11832869252652,-0.910199742873642,
25.6207047918644));
#49569=CARTESIAN_POINT('Ctrl Pts',(3.97941720203787,1.88920326505482,25.3713775656284));
#49570=CARTESIAN_POINT('Ctrl Pts',(3.84050571154924,4.22833122106338,23.8133975683351));
#49571=CARTESIAN_POINT('Ctrl Pts',(3.70159422106059,5.5372919058718,21.3263424438669));
#49572=CARTESIAN_POINT('Ctrl Pts',(3.56268273057196,5.4971773658931,18.5161445700008));
#49573=CARTESIAN_POINT('Ctrl Pts',(3.42377124008332,4.11776088615646,16.0674650397519));
#49574=CARTESIAN_POINT('Ctrl Pts',(3.28485974959469,1.73511588106992,14.5768866129545));
#49575=CARTESIAN_POINT('Ctrl Pts',(3.14594825910605,-1.07026317650166,14.4075655871855));
#49576=CARTESIAN_POINT('Ctrl Pts',(3.00703676861742,-3.6148892234453,15.6007544018894));
#49577=CARTESIAN_POINT('Ctrl Pts',(2.86812527812878,-5.27880362017199,17.8657511233237));
#49578=CARTESIAN_POINT('Ctrl Pts',(2.72921378764014,-5.65661945091725,20.6507244555628));
#49579=CARTESIAN_POINT('Ctrl Pts',(2.59030229715152,-4.65628775236742,23.277158876247));
#49580=CARTESIAN_POINT('Ctrl Pts',(2.45139080666287,-2.521523817008,25.1051644003928));
#49581=CARTESIAN_POINT('Ctrl Pts',(2.31247931617424,0.227570259334219,25.6893758657282));
#49582=CARTESIAN_POINT('Ctrl Pts',(2.1735678256856,2.92122037178518,24.8874591970467));
#49583=CARTESIAN_POINT('Ctrl Pts',(2.03465633519697,4.9031604877807,22.8947889822085));
#49584=CARTESIAN_POINT('Ctrl Pts',(1.89574484470833,5.69052164662065,20.1968483134104));
#49585=CARTESIAN_POINT('Ctrl Pts',(1.7568333542197,5.09147555163317,17.4509487077672));
#49586=CARTESIAN_POINT('Ctrl Pts',(1.61792186373106,3.25197042952828,15.3260856884126));
#49587=CARTESIAN_POINT('Ctrl Pts',(1.47901037324242,0.620173261604023,14.3399497289677));
#49588=CARTESIAN_POINT('Ctrl Pts',(1.34009888275378,-2.16271963966253,14.7327964067747));
#49589=CARTESIAN_POINT('Ctrl Pts',(1.20118739226515,-4.41869918570553,16.4089169761365));
#49590=CARTESIAN_POINT('Ctrl Pts',(1.06227590177651,-5.5981318200567,18.9599462473385));
#49591=CARTESIAN_POINT('Ctrl Pts',(0.923364411287872,-5.41366542779912,
21.7643742548674));
#49592=CARTESIAN_POINT('Ctrl Pts',(0.784452920799232,-3.91024565102259,
24.138928475994));
#49593=CARTESIAN_POINT('Ctrl Pts',(0.645541430310592,-1.45415094708632,
25.5051194323653));
#49594=CARTESIAN_POINT('Ctrl Pts',(0.506629939821954,1.35621666180418,25.5300293552048));
#49595=CARTESIAN_POINT('Ctrl Pts',(0.367718449333321,3.83617967324551,24.207720366993));
#49596=CARTESIAN_POINT('Ctrl Pts',(0.228806958844687,5.38148449802081,21.8600943129511));
#49597=CARTESIAN_POINT('Ctrl Pts',(0.0898954683560495,5.61573809242548,
19.0596248185465));
#49598=CARTESIAN_POINT('Ctrl Pts',(-0.0490160221325763,4.48168004880515,
16.4875673042026));
#49599=CARTESIAN_POINT('Ctrl Pts',(-0.141623682458336,2.99785669531383,
15.3445018393813));
#49600=CARTESIAN_POINT('Ctrl Pts',(-0.187927512621213,2.16407317598292,
14.9847270910257));
#49601=CARTESIAN_POINT('Ctrl Pts',(50.5637825378637,-1.32667918156829,15.0375285480223));
#49602=CARTESIAN_POINT('Ctrl Pts',(50.5174787077008,-2.15168451764989,15.2580874801298));
#49603=CARTESIAN_POINT('Ctrl Pts',(50.4248710473751,-3.68873492200737,16.1183991355923));
#49604=CARTESIAN_POINT('Ctrl Pts',(50.2859595568864,-5.09604146002229,18.3561196065066));
#49605=CARTESIAN_POINT('Ctrl Pts',(50.1470480663978,-5.26156574360687,20.9937156315332));
#49606=CARTESIAN_POINT('Ctrl Pts',(50.0081365759091,-4.14529719998611,23.3895155338352));
#49607=CARTESIAN_POINT('Ctrl Pts',(49.8692250854205,-2.01903759094086,24.9593576609462));
#49608=CARTESIAN_POINT('Ctrl Pts',(49.7303135949318,0.599101898234613,25.321007862679));
#49609=CARTESIAN_POINT('Ctrl Pts',(49.5914021044432,3.07129336959566,24.3862371798792));
#49610=CARTESIAN_POINT('Ctrl Pts',(49.4524906139546,4.79520484297246,22.3828481604625));
#49611=CARTESIAN_POINT('Ctrl Pts',(49.3135791234659,5.35084266186257,19.7989048767012));
#49612=CARTESIAN_POINT('Ctrl Pts',(49.1746676329773,4.60282890398964,17.2639605279354));
#49613=CARTESIAN_POINT('Ctrl Pts',(49.0357561424887,2.73340824983943,15.3956070723818));
#49614=CARTESIAN_POINT('Ctrl Pts',(48.8968446520001,0.19803463412749,14.6490438348891));
#49615=CARTESIAN_POINT('Ctrl Pts',(48.7579331615113,-2.38558680835433,15.2061573259097));
#49616=CARTESIAN_POINT('Ctrl Pts',(48.6190216710228,-4.38799717418834,16.9312165240447));
#49617=CARTESIAN_POINT('Ctrl Pts',(48.4801101805341,-5.32134007622315,19.4039370066215));
#49618=CARTESIAN_POINT('Ctrl Pts',(48.3411986900456,-4.95822109602027,22.021879075434));
#49619=CARTESIAN_POINT('Ctrl Pts',(48.2022871995568,-3.38710848985947,24.1472216448687));
#49620=CARTESIAN_POINT('Ctrl Pts',(48.0633757090683,-0.990779481809887,
25.262158055552));
#49621=CARTESIAN_POINT('Ctrl Pts',(47.9244642185795,1.64693757250601,25.0950513217741));
#49622=CARTESIAN_POINT('Ctrl Pts',(47.785552728091,3.88340384844544,23.6866144231869));
#49623=CARTESIAN_POINT('Ctrl Pts',(47.6466412376023,5.17373905472326,21.3799911398092));
#49624=CARTESIAN_POINT('Ctrl Pts',(47.5077297471137,5.20357304491207,18.7371544365421));
#49625=CARTESIAN_POINT('Ctrl Pts',(47.368818256625,3.96563723118361,16.4019904525415));
#49626=CARTESIAN_POINT('Ctrl Pts',(47.2299067661365,1.76153545929722,14.9434256480188));
#49627=CARTESIAN_POINT('Ctrl Pts',(47.0909952756476,-0.871737085184379,
14.7168166976175));
#49628=CARTESIAN_POINT('Ctrl Pts',(46.9520837851592,-3.29262441972186,15.7773733550559));
#49629=CARTESIAN_POINT('Ctrl Pts',(46.8131722946704,-4.91131492144359,17.8667074522167));
#49630=CARTESIAN_POINT('Ctrl Pts',(46.6742608041819,-5.33343977443084,20.4757851663839));
#49631=CARTESIAN_POINT('Ctrl Pts',(46.5353493136931,-4.45615481032689,22.9689452097341));
#49632=CARTESIAN_POINT('Ctrl Pts',(46.3964378232046,-2.49319689370494,24.7387678357613));
#49633=CARTESIAN_POINT('Ctrl Pts',(46.2575263327159,0.0771897474612934,
25.354063232247));
#49634=CARTESIAN_POINT('Ctrl Pts',(46.1186148422274,2.62877030477265,24.6649242262618));
#49635=CARTESIAN_POINT('Ctrl Pts',(45.9797033517386,4.5398917802619,22.8392488400151));
#49636=CARTESIAN_POINT('Ctrl Pts',(45.8407918612501,5.34493909024452,20.3218345438155));
#49637=CARTESIAN_POINT('Ctrl Pts',(45.7018803707613,4.84777495333142,17.7260102564282));
#49638=CARTESIAN_POINT('Ctrl Pts',(45.5629688802728,3.16952569465798,15.6842082739178));
#49639=CARTESIAN_POINT('Ctrl Pts',(45.4240573897841,0.71907069684952,14.6938819571226));
#49640=CARTESIAN_POINT('Ctrl Pts',(45.2851458992955,-1.90657471505998,14.9963089416001));
#49641=CARTESIAN_POINT('Ctrl Pts',(45.1462344088068,-4.06771279089063,16.5178075867578));
#49642=CARTESIAN_POINT('Ctrl Pts',(45.0073229183182,-5.23781578296322,18.8876883639203));
#49643=CARTESIAN_POINT('Ctrl Pts',(44.8684114278295,-5.13180625922525,21.5285666062667));
#49644=CARTESIAN_POINT('Ctrl Pts',(44.7294999373409,-3.77551179468938,23.7970333209202));
#49645=CARTESIAN_POINT('Ctrl Pts',(44.5905884468524,-1.49937248366909,25.1404118032734));
#49646=CARTESIAN_POINT('Ctrl Pts',(44.4516769563636,1.14206566021501,25.231408737594));
#49647=CARTESIAN_POINT('Ctrl Pts',(44.312765465875,3.50525723276716,24.0478541332601));
#49648=CARTESIAN_POINT('Ctrl Pts',(44.1738539753864,5.01444728804201,21.87810269886));
#49649=CARTESIAN_POINT('Ctrl Pts',(44.0349424848978,5.3019450942392,19.2507806931946));
#49650=CARTESIAN_POINT('Ctrl Pts',(43.8960309944091,4.29770627332817,16.805994342489));
#49651=CARTESIAN_POINT('Ctrl Pts',(43.7571195039205,2.24639802654879,15.1393778938973));
#49652=CARTESIAN_POINT('Ctrl Pts',(43.6182080134318,-0.35221023152451,14.6569765764292));
#49653=CARTESIAN_POINT('Ctrl Pts',(43.4792965229433,-2.86500793358189,15.4763199834063));
#49654=CARTESIAN_POINT('Ctrl Pts',(43.3403850324545,-4.67979092236272,17.3977878113058));
#49655=CARTESIAN_POINT('Ctrl Pts',(43.201473541966,-5.35441549113415,19.953244248272));
#49656=CARTESIAN_POINT('Ctrl Pts',(43.0625620514773,-4.7245198350227,22.5200919984187));
#49657=CARTESIAN_POINT('Ctrl Pts',(42.9236505609887,-2.94356825360016,24.4729584492162));
#49658=CARTESIAN_POINT('Ctrl Pts',(42.7847390705,-0.445461956316902,25.3360580016986));
#49659=CARTESIAN_POINT('Ctrl Pts',(42.6458275800114,2.16117423230435,24.89910984666));
#49660=CARTESIAN_POINT('Ctrl Pts',(42.5069160895227,4.2412738642828,23.2685696199054));
#49661=CARTESIAN_POINT('Ctrl Pts',(42.3680045990342,5.28805295093088,20.8416931389576));
#49662=CARTESIAN_POINT('Ctrl Pts',(42.2290931085454,5.04648001555839,18.2097511891956));
#49663=CARTESIAN_POINT('Ctrl Pts',(42.0901816180569,3.5754105542507,16.0139755745141));
#49664=CARTESIAN_POINT('Ctrl Pts',(41.9512701275682,1.23324780778372,14.7893329413007));
#49665=CARTESIAN_POINT('Ctrl Pts',(41.8123586370796,-1.40937662497005,14.8341884586248));
#49666=CARTESIAN_POINT('Ctrl Pts',(41.6734471465909,-3.70862831894497,16.1376137759235));
#49667=CARTESIAN_POINT('Ctrl Pts',(41.5345356561023,-5.10433028715659,18.3820495459895));
#49668=CARTESIAN_POINT('Ctrl Pts',(41.3956241656136,-5.25644140869157,21.0206738308635));
#49669=CARTESIAN_POINT('Ctrl Pts',(41.2567126751251,-4.12790216980831,23.4106267794218));
#49670=CARTESIAN_POINT('Ctrl Pts',(41.1178011846363,-1.99366363923406,24.9696334518365));
#49671=CARTESIAN_POINT('Ctrl Pts',(40.9788896941478,0.626300092027496,25.3178660707791));
#49672=CARTESIAN_POINT('Ctrl Pts',(40.8399782036591,3.09367552709713,24.3704831637998));
#49673=CARTESIAN_POINT('Ctrl Pts',(40.7010667131705,4.8073249390358,22.3582998712084));
#49674=CARTESIAN_POINT('Ctrl Pts',(40.5621552226818,5.34974424734503,19.7715534197766));
#49675=CARTESIAN_POINT('Ctrl Pts',(40.4232437321932,4.58878140681505,17.2404644317412));
#49676=CARTESIAN_POINT('Ctrl Pts',(40.2843322417046,2.70983320211814,15.3816934522798));
#49677=CARTESIAN_POINT('Ctrl Pts',(40.1454207512159,0.170676198893053,14.6481011792871));
#49678=CARTESIAN_POINT('Ctrl Pts',(40.0065092607273,-2.4100634110107,15.218415983492));
#49679=CARTESIAN_POINT('Ctrl Pts',(39.8675977702387,-4.40362847905842,16.9536895150949));
#49680=CARTESIAN_POINT('Ctrl Pts',(39.72868627975,-5.32431781990231,19.4311493124838));
#49681=CARTESIAN_POINT('Ctrl Pts',(39.5897747892614,-4.9478197662925,22.0472007503668));
#49682=CARTESIAN_POINT('Ctrl Pts',(39.4508632987728,-3.36586222510812,24.1644835014209));
#49683=CARTESIAN_POINT('Ctrl Pts',(39.3119518082841,-0.963864596617645,
25.2671544871405));
#49684=CARTESIAN_POINT('Ctrl Pts',(39.1730403177955,1.67296368003944,25.0865650371627));
#49685=CARTESIAN_POINT('Ctrl Pts',(39.0341288273068,3.90220032326434,23.6667129679227));
#49686=CARTESIAN_POINT('Ctrl Pts',(38.8952173368182,5.18072642643651,21.3535231975993));
#49687=CARTESIAN_POINT('Ctrl Pts',(38.7563058463296,5.19704894939304,18.7105685091368));
#49688=CARTESIAN_POINT('Ctrl Pts',(38.617394355841,3.94719116276856,16.3817637892781));
#49689=CARTESIAN_POINT('Ctrl Pts',(38.4784828653523,1.73566151637966,14.9344861610518));
#49690=CARTESIAN_POINT('Ctrl Pts',(38.3395713748637,-0.898735118089893,
14.7213423543926));
#49691=CARTESIAN_POINT('Ctrl Pts',(38.200659884375,-3.3141688909171,15.7942615494429));
#49692=CARTESIAN_POINT('Ctrl Pts',(38.0617483938864,-4.92215685494637,17.8918436378386));
#49693=CARTESIAN_POINT('Ctrl Pts',(37.9228369033977,-5.33093770141904,20.5030453017433));
#49694=CARTESIAN_POINT('Ctrl Pts',(37.7839254129091,-4.44091832205815,22.9916877859873));
#49695=CARTESIAN_POINT('Ctrl Pts',(37.6450139224205,-2.46893812404761,24.7514519772004));
#49696=CARTESIAN_POINT('Ctrl Pts',(37.5061024319319,0.104560525815868,25.353598644693));
#49697=CARTESIAN_POINT('Ctrl Pts',(37.3671909414432,2.65258462651949,24.6514240992592));
#49698=CARTESIAN_POINT('Ctrl Pts',(37.2282794509546,4.55434765554542,22.8160022699645));
#49699=CARTESIAN_POINT('Ctrl Pts',(37.0893679604659,5.34651456943153,20.2945051966832));
#49700=CARTESIAN_POINT('Ctrl Pts',(36.9504564699773,4.83608619537201,17.701256503446));
#49701=CARTESIAN_POINT('Ctrl Pts',(36.8115449794886,3.1474204839998,15.6680609827797));
#49702=CARTESIAN_POINT('Ctrl Pts',(36.6726334890001,0.691934624959393,14.6902751646814));
#49703=CARTESIAN_POINT('Ctrl Pts',(36.5337219985113,-1.93213036546348,15.0061213868506));
#49704=CARTESIAN_POINT('Ctrl Pts',(36.3948105080228,-4.08546178225335,16.5386486197203));
#49705=CARTESIAN_POINT('Ctrl Pts',(36.2558990175341,-5.24343384903385,18.9144803904014));
#49706=CARTESIAN_POINT('Ctrl Pts',(36.1169875270455,-5.1239246454075,21.5547821648715));
#49707=CARTESIAN_POINT('Ctrl Pts',(35.9780760365568,-3.75605073385406,23.8162853977043));
#49708=CARTESIAN_POINT('Ctrl Pts',(35.8391645460682,-1.47307336122034,25.148009928553));
#49709=CARTESIAN_POINT('Ctrl Pts',(35.7002530555796,1.16879547129917,25.2255017460802));
#49710=CARTESIAN_POINT('Ctrl Pts',(35.5613415650909,3.52590542890769,24.0298811717489));
#49711=CARTESIAN_POINT('Ctrl Pts',(35.4224300746023,5.02398325674396,21.8524426004531));
#49712=CARTESIAN_POINT('Ctrl Pts',(35.2835185841136,5.29804554474264,19.2236851425809));
#49713=CARTESIAN_POINT('Ctrl Pts',(35.1446070936251,4.28132127034039,16.784064750007));
#49714=CARTESIAN_POINT('Ctrl Pts',(35.0056956031363,2.2215195217249,15.127957064371));
#49715=CARTESIAN_POINT('Ctrl Pts',(34.8667841126478,-0.379520976640382,
14.6588470177024));
#49716=CARTESIAN_POINT('Ctrl Pts',(34.7278726221591,-2.88809707985093,15.491025991495));
#49717=CARTESIAN_POINT('Ctrl Pts',(34.5889611316705,-4.69303315767885,17.4217464956014));
#49718=CARTESIAN_POINT('Ctrl Pts',(34.4500496411818,-5.35458455040435,19.9806184472246));
#49719=CARTESIAN_POINT('Ctrl Pts',(34.3111381506932,-4.7115745295799,22.5442124133474));
#49720=CARTESIAN_POINT('Ctrl Pts',(34.1722266602045,-2.92066250618256,24.4879485154128));
#49721=CARTESIAN_POINT('Ctrl Pts',(34.0333151697159,-0.418176396747093,
25.3382656222055));
#49722=CARTESIAN_POINT('Ctrl Pts',(33.8944036792273,2.18619190095496,24.8879971690065));
#49723=CARTESIAN_POINT('Ctrl Pts',(33.7554921887387,4.25792847536376,23.2468440755145));
#49724=CARTESIAN_POINT('Ctrl Pts',(33.61658069825,5.29228686695988,20.814647819503));
#49725=CARTESIAN_POINT('Ctrl Pts',(33.4776692077614,5.03726170861247,18.1839752669736));
#49726=CARTESIAN_POINT('Ctrl Pts',(33.3387577172727,3.55498592173361,15.9957489528886));
#49727=CARTESIAN_POINT('Ctrl Pts',(33.1998462267842,1.20659299438363,14.7830962537228));
#49728=CARTESIAN_POINT('Ctrl Pts',(33.0609347362954,-1.43576758769577,14.841461177219));
#49729=CARTESIAN_POINT('Ctrl Pts',(32.9220232458069,-3.7283256825603,16.156624015689));
#49730=CARTESIAN_POINT('Ctrl Pts',(32.7831117553182,-5.11253509475286,18.4081657570785));
#49731=CARTESIAN_POINT('Ctrl Pts',(32.6442002648296,-5.25115468625036,21.0475332038116));
#49732=CARTESIAN_POINT('Ctrl Pts',(32.5052887743409,-4.11041194519357,23.4316854449129));
#49733=CARTESIAN_POINT('Ctrl Pts',(32.3663772838523,-1.96823113419552,24.9797607928896));
#49734=CARTESIAN_POINT('Ctrl Pts',(32.2274657933636,0.65347864239245,25.3145947179398));
#49735=CARTESIAN_POINT('Ctrl Pts',(32.0885543028751,3.11597849084889,24.3546101314106));
#49736=CARTESIAN_POINT('Ctrl Pts',(31.9496428123863,4.81931854523574,22.3336923772348));
#49737=CARTESIAN_POINT('Ctrl Pts',(31.8107313218978,5.34850644000348,19.7442066981756));
#49738=CARTESIAN_POINT('Ctrl Pts',(31.6718198314091,4.57461375847793,17.2170410867637));
#49739=CARTESIAN_POINT('Ctrl Pts',(31.5329083409205,2.68618744039703,15.3679002183599));
#49740=CARTESIAN_POINT('Ctrl Pts',(31.3939968504318,0.143313246609341,14.6472985637752));
#49741=CARTESIAN_POINT('Ctrl Pts',(31.2550853599433,-2.43447699525212,15.2307995311997));
#49742=CARTESIAN_POINT('Ctrl Pts',(31.1161738694545,-4.41914470439699,16.9762421668366));
#49743=CARTESIAN_POINT('Ctrl Pts',(30.977262378966,-5.32715639887223,19.4583764647177));
#49744=CARTESIAN_POINT('Ctrl Pts',(30.8383508884772,-4.93728912318725,22.0724689300624));
#49745=CARTESIAN_POINT('Ctrl Pts',(30.6994393979887,-3.34452798766702,24.1816365088));
#49746=CARTESIAN_POINT('Ctrl Pts',(30.5605279075,-0.93692452064997,25.2720132581986));
#49747=CARTESIAN_POINT('Ctrl Pts',(30.4216164170114,1.69894606317944,25.0779458077478));
#49748=CARTESIAN_POINT('Ctrl Pts',(30.2827049265227,3.92089480921487,23.646715679497));
#49749=CARTESIAN_POINT('Ctrl Pts',(30.1437934360341,5.18757839386559,21.327019879096));
#49750=CARTESIAN_POINT('Ctrl Pts',(30.0048819455454,5.19038902279063,18.6840162827332));
#49751=CARTESIAN_POINT('Ctrl Pts',(29.8659704550569,3.92864192987812,16.3616316928023));
#49752=CARTESIAN_POINT('Ctrl Pts',(29.7270589645682,1.7097422098796,14.925679067326));
#49753=CARTESIAN_POINT('Ctrl Pts',(29.5881474740796,-0.925709661482013,
14.7260059751024));
#49754=CARTESIAN_POINT('Ctrl Pts',(29.4492359835909,-3.33562674239409,15.8112596657894));
#49755=CARTESIAN_POINT('Ctrl Pts',(29.3103244931023,-4.93287014205778,17.9170349226135));
#49756=CARTESIAN_POINT('Ctrl Pts',(29.1714130026136,-5.3282962980484,20.5302922894222));
#49757=CARTESIAN_POINT('Ctrl Pts',(29.0325015121251,-4.4255657651377,23.0143521709412));
#49758=CARTESIAN_POINT('Ctrl Pts',(28.8935900216363,-2.44461482577355,24.7640119338248));
#49759=CARTESIAN_POINT('Ctrl Pts',(28.7546785311478,0.13192857135758,25.352994134508));
#49760=CARTESIAN_POINT('Ctrl Pts',(28.6157670406591,2.67632961983071,24.6378024017883));
#49761=CARTESIAN_POINT('Ctrl Pts',(28.4768555501705,4.56868449756808,22.7926821003648));
#49762=CARTESIAN_POINT('Ctrl Pts',(28.3379440596818,5.3479503111387,20.2671681523096));
#49763=CARTESIAN_POINT('Ctrl Pts',(28.1990325691932,4.82427104058186,17.676562830843));
#49764=CARTESIAN_POINT('Ctrl Pts',(28.0601210787045,3.12523301178589,15.6520269119898));
#49765=CARTESIAN_POINT('Ctrl Pts',(27.9212095882159,0.664780468539763,14.6868071481768));
#49766=CARTESIAN_POINT('Ctrl Pts',(27.7822980977273,-1.95763551735538,15.0160643530232));
#49767=CARTESIAN_POINT('Ctrl Pts',(27.6433866072387,-4.10310399524189,16.5595801191937));
#49768=CARTESIAN_POINT('Ctrl Pts',(27.50447511675,-5.24891487176117,18.941300788221));
#49769=CARTESIAN_POINT('Ctrl Pts',(27.3655636262614,-5.11590911176077,21.5809570874062));
#49770=CARTESIAN_POINT('Ctrl Pts',(27.2266521357728,-3.73649150419176,23.8354377313574));
#49771=CARTESIAN_POINT('Ctrl Pts',(27.0877406452841,-1.44673573825756,25.1554735045062));
#49772=CARTESIAN_POINT('Ctrl Pts',(26.9488291547955,1.19549473453172,25.2194581798999));
#49773=CARTESIAN_POINT('Ctrl Pts',(26.8099176643069,3.5464614713409,24.0118028845286));
#49774=CARTESIAN_POINT('Ctrl Pts',(26.6710061738182,5.03338791770333,21.8267340862685));
#49775=CARTESIAN_POINT('Ctrl Pts',(26.5320946833296,5.29400752456154,19.1966098818738));
#49776=CARTESIAN_POINT('Ctrl Pts',(26.3931831928409,4.26482436995908,16.762219209795));
#49777=CARTESIAN_POINT('Ctrl Pts',(26.2542717023523,2.19658295486167,15.1166635714475));
#49778=CARTESIAN_POINT('Ctrl Pts',(26.1153602118636,-0.40682180252673,14.6608570563239));
#49779=CARTESIAN_POINT('Ctrl Pts',(25.976448721375,-2.91111074228793,15.5058498469507));
#49780=CARTESIAN_POINT('Ctrl Pts',(25.8375372308863,-4.70615273502447,17.4457725656006));
#49781=CARTESIAN_POINT('Ctrl Pts',(25.6986257403978,-5.35461366127627,20.0079931527372));
#49782=CARTESIAN_POINT('Ctrl Pts',(25.5597142499091,-4.69850608156596,22.5682663322764));
#49783=CARTESIAN_POINT('Ctrl Pts',(25.4208027594205,-2.89768042379711,24.5028212837687));
#49784=CARTESIAN_POINT('Ctrl Pts',(25.2818912689318,-0.39087990764277,25.3403337208285));
#49785=CARTESIAN_POINT('Ctrl Pts',(25.1429797784432,2.2111524308953,24.8767567377677));
#49786=CARTESIAN_POINT('Ctrl Pts',(25.0040682879546,4.27447180044954,23.2250336710147));
#49787=CARTESIAN_POINT('Ctrl Pts',(24.8651567974659,5.29638246281417,20.7875812082645));
#49788=CARTESIAN_POINT('Ctrl Pts',(24.7262453069773,5.02791174687594,18.1582468087054));
#49789=CARTESIAN_POINT('Ctrl Pts',(24.5873338164886,3.53446837545621,15.9776269870987));
#49790=CARTESIAN_POINT('Ctrl Pts',(24.448422326,1.17990664524902,14.7769959160925));
#49791=CARTESIAN_POINT('Ctrl Pts',(24.3095108355114,-1.46212102493793,14.8488687203245));
#49792=CARTESIAN_POINT('Ctrl Pts',(24.1705993450227,-3.74792560197564,16.1757347066302));
#49793=CARTESIAN_POINT('Ctrl Pts',(24.0316878545341,-5.12060628019952,18.4343235726376));
#49794=CARTESIAN_POINT('Ctrl Pts',(23.8927763640455,-5.24573071867263,21.074365198241));
#49795=CARTESIAN_POINT('Ctrl Pts',(23.7538648735568,-4.09281429010269,23.4526544192474));
#49796=CARTESIAN_POINT('Ctrl Pts',(23.6149533830683,-1.94274718710914,24.9897579820064));
#49797=CARTESIAN_POINT('Ctrl Pts',(23.4760418925795,0.680640113320448,25.3111844618838));
#49798=CARTESIAN_POINT('Ctrl Pts',(23.337130402091,3.13820001481857,24.3386232861369));
#49799=CARTESIAN_POINT('Ctrl Pts',(23.1982189116023,4.83118619284732,22.3090238894517));
#49800=CARTESIAN_POINT('Ctrl Pts',(23.0593074211137,5.34712884312223,19.7168666620349));
#49801=CARTESIAN_POINT('Ctrl Pts',(22.920395930625,4.56032654720136,17.1936904777079));
#49802=CARTESIAN_POINT('Ctrl Pts',(22.7814844401364,2.66247147199116,15.3542280498446));
#49803=CARTESIAN_POINT('Ctrl Pts',(22.6425729496478,0.11594654866455,14.6466358474442));
#49804=CARTESIAN_POINT('Ctrl Pts',(22.5036614591591,-2.4588269515588,15.2433077276005));
#49805=CARTESIAN_POINT('Ctrl Pts',(22.3647499686705,-4.43454543016366,16.9988738480645));
#49806=CARTESIAN_POINT('Ctrl Pts',(22.2258384781818,-5.32985574631102,19.4856177729232));
#49807=CARTESIAN_POINT('Ctrl Pts',(22.0869269876932,-4.92662943819308,22.097682943332));
#49808=CARTESIAN_POINT('Ctrl Pts',(21.9480154972046,-3.3231063370325,24.1986802241647));
#49809=CARTESIAN_POINT('Ctrl Pts',(21.8091040067159,-0.90995995705217,25.2767342389567));
#49810=CARTESIAN_POINT('Ctrl Pts',(21.6701925162273,1.72488404235526,25.0691938602154));
#49811=CARTESIAN_POINT('Ctrl Pts',(21.5312810257386,3.93948681794363,23.6266230798452));
#49812=CARTESIAN_POINT('Ctrl Pts',(21.39236953525,5.19429477779974,21.3004818773591));
#49813=CARTESIAN_POINT('Ctrl Pts',(21.2534580447613,5.18359343923419,18.65749845112));
#49814=CARTESIAN_POINT('Ctrl Pts',(21.1145465542728,3.9099900172857,16.341594689384));
#49815=CARTESIAN_POINT('Ctrl Pts',(20.9756350637841,1.68377821724532,14.9170045969775));
#49816=CARTESIAN_POINT('Ctrl Pts',(20.8367235732955,-0.952660010357647,
14.7308074378818));
#49817=CARTESIAN_POINT('Ctrl Pts',(20.6978120828068,-3.35699741332223,15.8283672598172));
#49818=CARTESIAN_POINT('Ctrl Pts',(20.5589005923182,-4.94345450277555,17.9422806481434));
#49819=CARTESIAN_POINT('Ctrl Pts',(20.4199891018296,-5.32551563335403,20.5575254172851));
#49820=CARTESIAN_POINT('Ctrl Pts',(20.2810776113409,-4.41009754082334,23.0369377722372));
#49821=CARTESIAN_POINT('Ctrl Pts',(20.1421661208523,-2.42022763460054,24.7764473773646));
#49822=CARTESIAN_POINT('Ctrl Pts',(20.0032546303637,0.159293168790149,25.3522497174921));
#49823=CARTESIAN_POINT('Ctrl Pts',(19.864343139875,2.70000466410295,24.6240594898681));
#49824=CARTESIAN_POINT('Ctrl Pts',(19.7254316493864,4.58290193161955,22.7692889407165));
#49825=CARTESIAN_POINT('Ctrl Pts',(19.5865201588977,5.34924627784126,20.2398241251803));
#49826=CARTESIAN_POINT('Ctrl Pts',(19.4476086684091,4.812329797764,17.6519298840176));
#49827=CARTESIAN_POINT('Ctrl Pts',(19.3086971779205,3.10296385791202,15.6361064806175));
#49828=CARTESIAN_POINT('Ctrl Pts',(19.1697856874318,0.63760893729653,14.6834779982496));
#49829=CARTESIAN_POINT('Ctrl Pts',(19.0308741969432,-1.98308950412843,15.0261375802468));
#49830=CARTESIAN_POINT('Ctrl Pts',(18.8919627064546,-4.12063896875621,16.5806015381087));
#49831=CARTESIAN_POINT('Ctrl Pts',(18.7530512159659,-5.25425870789218,18.9681488563963));
#49832=CARTESIAN_POINT('Ctrl Pts',(18.6141397254773,-5.10775986778052,21.6070906897583));
#49833=CARTESIAN_POINT('Ctrl Pts',(18.4752282349886,-3.7168346169061,23.8544898213103));
#49834=CARTESIAN_POINT('Ctrl Pts',(18.3363167445,-1.42036030314568,25.1628023360638));
#49835=CARTESIAN_POINT('Ctrl Pts',(18.1974052540114,1.22216275209595,25.2132781970087));
#49836=CARTESIAN_POINT('Ctrl Pts',(18.0584937635228,3.56692482281038,23.9936197440964));
#49837=CARTESIAN_POINT('Ctrl Pts',(17.9195822730341,5.04266102511817,21.8009778282287));
#49838=CARTESIAN_POINT('Ctrl Pts',(17.7806707825454,5.28983113923432,19.1695556187174));
#49839=CARTESIAN_POINT('Ctrl Pts',(17.6417592920568,4.24821600335025,16.7404582928123));
#49840=CARTESIAN_POINT('Ctrl Pts',(17.5028478015682,2.17158897770571,15.1054977102953));
#49841=CARTESIAN_POINT('Ctrl Pts',(17.3639363110796,-0.434111995644343,
14.6630066397592));
#49842=CARTESIAN_POINT('Ctrl Pts',(17.2250248205909,-2.93404831940373,15.5207911623345));
#49843=CARTESIAN_POINT('Ctrl Pts',(17.0861133301023,-4.719149311504,17.4698653933539));
#49844=CARTESIAN_POINT('Ctrl Pts',(16.9472018396136,-5.35450282298902,20.0353676493391));
#49845=CARTESIAN_POINT('Ctrl Pts',(16.808290349125,-4.6853148325402,22.5922531265283));
#49846=CARTESIAN_POINT('Ctrl Pts',(16.6693788586364,-2.87462260710757,24.5175763655663));
#49847=CARTESIAN_POINT('Ctrl Pts',(16.5304673681477,-0.363573202429767,
25.3422622435156));
#49848=CARTESIAN_POINT('Ctrl Pts',(16.3915558776591,2.23605516975252,24.8653888467254));
#49849=CARTESIAN_POINT('Ctrl Pts',(16.2526443871705,4.29090340716083,23.2031389764468));
#49850=CARTESIAN_POINT('Ctrl Pts',(16.1137328966818,5.30033963145057,20.7604940126599));
#49851=CARTESIAN_POINT('Ctrl Pts',(15.9748214061932,5.01843037472102,18.1325664868343));
#49852=CARTESIAN_POINT('Ctrl Pts',(15.8359099157046,3.51385845166871,15.9596101507833));
#49853=CARTESIAN_POINT('Ctrl Pts',(15.6969984252159,1.15318945785908,14.7710320878495));
#49854=CARTESIAN_POINT('Ctrl Pts',(15.5580869347273,-1.48843624791842,14.8564108943366));
#49855=CARTESIAN_POINT('Ctrl Pts',(15.4191754442387,-3.76742756492399,16.1949453492666));
#49856=CARTESIAN_POINT('Ctrl Pts',(15.28026395375,-5.12854363254664,18.4605223090014));
#49857=CARTESIAN_POINT('Ctrl Pts',(15.1413524632614,-5.24016964772018,21.1011691128656));
#49858=CARTESIAN_POINT('Ctrl Pts',(15.0024409727727,-4.07510966447109,23.4735331543762));
#49859=CARTESIAN_POINT('Ctrl Pts',(14.8635294822841,-1.91721246402803,24.9996247578986));
#49860=CARTESIAN_POINT('Ctrl Pts',(14.7246179917955,0.707783794914243,25.3076353917422));
#49861=CARTESIAN_POINT('Ctrl Pts',(14.5857065013068,3.16033951822035,24.3225230458138));
#49862=CARTESIAN_POINT('Ctrl Pts',(14.4467950108182,4.84292757169553,22.284295052599));
#49863=CARTESIAN_POINT('Ctrl Pts',(14.3078835203295,5.3456114927064,19.6895340259188));
#49864=CARTESIAN_POINT('Ctrl Pts',(14.1689720298409,4.54592014639849,17.1704132148695));
#49865=CARTESIAN_POINT('Ctrl Pts',(14.0300605393523,2.63868591674534,15.3406773040723));
#49866=CARTESIAN_POINT('Ctrl Pts',(13.8911490488637,0.0885768203195806,
14.6461130476149));
#49867=CARTESIAN_POINT('Ctrl Pts',(13.752237558375,-2.48311264351585,15.255940245778));
#49868=CARTESIAN_POINT('Ctrl Pts',(13.6133260678864,-4.44983025384227,17.0215839672727));
#49869=CARTESIAN_POINT('Ctrl Pts',(13.4744145773977,-5.33241579166802,19.5128725251163));
#49870=CARTESIAN_POINT('Ctrl Pts',(13.3355030869091,-4.91584098991347,22.1228421311778));
#49871=CARTESIAN_POINT('Ctrl Pts',(13.1965915964205,-3.30159783308474,24.2156142020573));
#49872=CARTESIAN_POINT('Ctrl Pts',(13.0576801059318,-0.882971610574968,
25.2813173060266));
#49873=CARTESIAN_POINT('Ctrl Pts',(12.9187686154432,1.75077693964727,25.0603094233076));
#49874=CARTESIAN_POINT('Ctrl Pts',(12.7798571249545,3.95797586352647,23.6064356941111));
#49875=CARTESIAN_POINT('Ctrl Pts',(12.6409456344659,5.20087540269829,21.2739098859907));
#49876=CARTESIAN_POINT('Ctrl Pts',(12.5020341439773,5.17666237633432,18.6310157073721));
#49877=CARTESIAN_POINT('Ctrl Pts',(12.3631226534886,3.89123591248115,16.3216533027141));
#49878=CARTESIAN_POINT('Ctrl Pts',(12.224211163,1.65777021707646,14.9084629767239));
#49879=CARTESIAN_POINT('Ctrl Pts',(12.0852996725114,-0.979585460337544,
14.7357466172389));
#49880=CARTESIAN_POINT('Ctrl Pts',(11.9463881820227,-3.37828034515378,15.8455838843991));
#49881=CARTESIAN_POINT('Ctrl Pts',(11.8074766915341,-4.95390966046493,17.9675801546016));
#49882=CARTESIAN_POINT('Ctrl Pts',(11.6685652010455,-5.32259578001186,20.584743973562));
#49883=CARTESIAN_POINT('Ctrl Pts',(11.5296537105568,-4.3945140533954,23.0594439995737));
#49884=CARTESIAN_POINT('Ctrl Pts',(11.3907422200682,-2.39577718791672,24.7887579828046));
#49885=CARTESIAN_POINT('Ctrl Pts',(11.2518307295796,0.18665360290738,25.3513654131015));
#49886=CARTESIAN_POINT('Ctrl Pts',(11.1129192390909,2.72360914056088,24.6101957226858));
#49887=CARTESIAN_POINT('Ctrl Pts',(10.9740077486023,4.59699958611036,22.7458234024274));
#49888=CARTESIAN_POINT('Ctrl Pts',(10.8350962581136,5.35040243566758,20.212473829964));
#49889=CARTESIAN_POINT('Ctrl Pts',(10.696184767625,4.80026277901695,17.6273583067809));
#49890=CARTESIAN_POINT('Ctrl Pts',(10.5572732771364,3.0806136044089,15.620300104762));
#49891=CARTESIAN_POINT('Ctrl Pts',(10.4183617866477,0.610420741389864,14.6802878019109));
#49892=CARTESIAN_POINT('Ctrl Pts',(10.2794502961591,-2.00849166051248,15.0363408052457));
#49893=CARTESIAN_POINT('Ctrl Pts',(10.1405388056705,-4.13806624449883,16.6017123270453));
#49894=CARTESIAN_POINT('Ctrl Pts',(10.0016273151818,-5.2594652177594,18.9950238932212));
#49895=CARTESIAN_POINT('Ctrl Pts',(9.86271582469318,-5.09947712645691,21.6331822888948));
#49896=CARTESIAN_POINT('Ctrl Pts',(9.72380433420456,-3.6970805857531,23.8734411696145));
#49897=CARTESIAN_POINT('Ctrl Pts',(9.58489284371592,-1.39394774523797,25.1699962316778));
#49898=CARTESIAN_POINT('Ctrl Pts',(9.44598135322729,1.24879882699148,25.2069619589279));
#49899=CARTESIAN_POINT('Ctrl Pts',(9.30706986273864,3.58729494848217,23.9753322256902));
#49900=CARTESIAN_POINT('Ctrl Pts',(9.16815837225,5.05180233662483,21.775174499504));
#49901=CARTESIAN_POINT('Ctrl Pts',(9.02924688176137,5.28551649791576,19.1425230602066));
#49902=CARTESIAN_POINT('Ctrl Pts',(8.89033539127272,4.23149660459327,16.7187825678062));
#49903=CARTESIAN_POINT('Ctrl Pts',(8.7514239007841,2.14653824350431,15.0944597727477));
#49904=CARTESIAN_POINT('Ctrl Pts',(8.61251241029546,-0.461390842731537,
14.6652957118262));
#49905=CARTESIAN_POINT('Ctrl Pts',(8.47360091980683,-2.95690921169756,15.5358495471372));
#49906=CARTESIAN_POINT('Ctrl Pts',(8.33468942931818,-4.73202254743652,17.4940243491667));
#49907=CARTESIAN_POINT('Ctrl Pts',(8.19577793882955,-5.3542520384395,20.0627412215658));
#49908=CARTESIAN_POINT('Ctrl Pts',(8.05686644834092,-4.67200112727156,22.6161721691797));
#49909=CARTESIAN_POINT('Ctrl Pts',(7.91795495785228,-2.85148965875746,24.5322133751641));
#49910=CARTESIAN_POINT('Ctrl Pts',(7.77904346736365,-0.336256994801425,
25.3440511398624));
#49911=CARTESIAN_POINT('Ctrl Pts',(7.640131976875,2.26089946666399,24.8538937929929));
#49912=CARTESIAN_POINT('Ctrl Pts',(7.50122048638638,4.30722286603815,23.1811605640544));
#49913=CARTESIAN_POINT('Ctrl Pts',(7.36230899589773,5.30415826944371,20.7333869406452));
#49914=CARTESIAN_POINT('Ctrl Pts',(7.22339750540911,5.00881783995471,18.1069349725462));
#49915=CARTESIAN_POINT('Ctrl Pts',(7.08448601492045,3.49315668903596,15.9416989148339));
#49916=CARTESIAN_POINT('Ctrl Pts',(6.94557452443183,1.1264421304992,14.7652049248654));
#49917=CARTESIAN_POINT('Ctrl Pts',(6.80666303394318,-1.51471256885767,14.8640875021315));
#49918=CARTESIAN_POINT('Ctrl Pts',(6.66775154345456,-3.78683106169839,16.2142554415052));
#49919=CARTESIAN_POINT('Ctrl Pts',(6.52884005296591,-5.13634694434205,18.4867612814347));
#49920=CARTESIAN_POINT('Ctrl Pts',(6.38992856247729,-5.23447161873823,21.1279442471333));
#49921=CARTESIAN_POINT('Ctrl Pts',(6.25101707198864,-4.05729853103018,23.4943211046092));
#49922=CARTESIAN_POINT('Ctrl Pts',(6.11210558150001,-1.89162763233226,25.0093608626864));
#49923=CARTESIAN_POINT('Ctrl Pts',(5.97319409101137,0.734908977741772,25.303947600274));
#49924=CARTESIAN_POINT('Ctrl Pts',(5.83428260052273,3.18239642241211,24.3063098312401));
#49925=CARTESIAN_POINT('Ctrl Pts',(5.69537111003409,4.85454237490546,22.2595065129944));
#49926=CARTESIAN_POINT('Ctrl Pts',(5.55645961954546,5.34395442841376,19.6622095041981));
#49927=CARTESIAN_POINT('Ctrl Pts',(5.41754812905682,4.53139493259768,17.1472099066274));
#49928=CARTESIAN_POINT('Ctrl Pts',(5.27863663856819,2.61483139632318,15.3272483352077));
#49929=CARTESIAN_POINT('Ctrl Pts',(5.13972514807955,0.0612047769146592,
14.6457301779514));
#49930=CARTESIAN_POINT('Ctrl Pts',(5.00081365759091,-2.50733343638805,15.2686967555665));
#49931=CARTESIAN_POINT('Ctrl Pts',(4.86190216710228,-4.46499877594587,17.0443719309055));
#49932=CARTESIAN_POINT('Ctrl Pts',(4.72299067661364,-5.33483646803344,19.540140008962));
#49933=CARTESIAN_POINT('Ctrl Pts',(4.584079186125,-4.90492406031727,22.1479458360344));
#49934=CARTESIAN_POINT('Ctrl Pts',(4.44516769563637,-3.28000303797389,24.2324379998885));
#49935=CARTESIAN_POINT('Ctrl Pts',(4.30625620514774,-0.855960186590904,
25.2857623396237));
#49936=CARTESIAN_POINT('Ctrl Pts',(4.16734471465909,1.77662407831394,25.0512927292309));
#49937=CARTESIAN_POINT('Ctrl Pts',(4.02843322417046,3.97636146273007,23.5861540499144));
#49938=CARTESIAN_POINT('Ctrl Pts',(3.88952173368182,5.20732009656954,21.2473045994844));
#49939=CARTESIAN_POINT('Ctrl Pts',(3.75061024319318,5.16959601524122,18.6045687436407));
#49940=CARTESIAN_POINT('Ctrl Pts',(3.61169875270455,3.87238010562758,16.3018080539971));
#49941=CARTESIAN_POINT('Ctrl Pts',(3.47278726221591,1.6317188891182,14.9000544297852));
#49942=CARTESIAN_POINT('Ctrl Pts',(3.33387577172727,-1.00648530768362,14.740823384132));
#49943=CARTESIAN_POINT('Ctrl Pts',(3.19496428123864,-3.39947498165274,15.8629090894604));
#49944=CARTESIAN_POINT('Ctrl Pts',(3.05605279075,-4.96423534183138,17.992932780948));
#49945=CARTESIAN_POINT('Ctrl Pts',(2.91714130026136,-5.31953681440784,20.611947246485));
#49946=CARTESIAN_POINT('Ctrl Pts',(2.77822980977274,-4.37881571000473,23.0818702654696));
#49947=CARTESIAN_POINT('Ctrl Pts',(2.6393183192841,-2.37126412504296,24.8009434269244));
#49948=CARTESIAN_POINT('Ctrl Pts',(2.50040682879546,0.214009159162442,25.3503412473393));
#49949=CARTESIAN_POINT('Ctrl Pts',(2.36149533830682,2.74714243118999,24.596211456896));
#49950=CARTESIAN_POINT('Ctrl Pts',(2.22258384781819,4.61097709471508,22.7222861100022));
#49951=CARTESIAN_POINT('Ctrl Pts',(2.08367235732956,5.35141875019975,20.1851179594327));
#49952=CARTESIAN_POINT('Ctrl Pts',(1.94476086684092,4.7880703079961,17.6028487847724));
#49953=CARTESIAN_POINT('Ctrl Pts',(1.80584937635228,3.05818281914584,15.6046081120332));
#49954=CARTESIAN_POINT('Ctrl Pts',(1.66693788586364,0.583216623469168,14.6772368108884));
#49955=CARTESIAN_POINT('Ctrl Pts',(1.528026395375,-2.03384138569939,15.0466734299052));
#49956=CARTESIAN_POINT('Ctrl Pts',(1.38911490488637,-4.15538524274299,16.6229125867855));
#49957=CARTESIAN_POINT('Ctrl Pts',(1.25020341439773,-5.26453450989542,19.0219239115778));
#49958=CARTESIAN_POINT('Ctrl Pts',(1.11129192390909,-5.09106062268244,21.6592337321965));
#49959=CARTESIAN_POINT('Ctrl Pts',(0.972380433420454,-3.67723087516871,
23.8922863012608));
#49960=CARTESIAN_POINT('Ctrl Pts',(0.833468942931815,-1.36749688817716,
25.1770648073967));
#49961=CARTESIAN_POINT('Ctrl Pts',(0.694557452443176,1.2753985880402,25.2004903273098));
#49962=CARTESIAN_POINT('Ctrl Pts',(0.555645961954543,3.60757855033071,23.9569788265186));
#49963=CARTESIAN_POINT('Ctrl Pts',(0.416734471465908,5.06079738115399,21.749249752767));
#49964=CARTESIAN_POINT('Ctrl Pts',(0.277822980977272,5.28109160991654,19.1156625541981));
#49965=CARTESIAN_POINT('Ctrl Pts',(0.138911490488646,4.21461302406515,16.6968760766832));
#49966=CARTESIAN_POINT('Ctrl Pts',(0.046303830162886,2.8192119327481,15.6219268293179));
#49967=CARTESIAN_POINT('Ctrl Pts',(8.88178419700125E-15,2.03511426366979,
15.2835913560944));
#49968=CARTESIAN_POINT('Ctrl Pts',(8.88178419700125E-15,2.03511426366979,
15.2835913560944));
#49969=CARTESIAN_POINT('Ctrl Pts',(9.32284291588981E-15,2.1755902259129,
15.3291667179724));
#49970=CARTESIAN_POINT('Ctrl Pts',(2.51669497179419E-15,2.31375853724984,
15.3808402235287));
#49971=CARTESIAN_POINT('Ctrl Pts',(3.88578058618805E-15,2.44931788544433,
15.4382685188975));
#49972=CARTESIAN_POINT('Ctrl Pts',(5.27910699501164E-15,2.58727742414413,
15.4967136297874));
#49973=CARTESIAN_POINT('Ctrl Pts',(1.13067933023619E-14,2.72253541261565,
15.5611192658562));
#49974=CARTESIAN_POINT('Ctrl Pts',(9.76996261670138E-15,2.85477467194667,
15.6311776903917));
#49975=CARTESIAN_POINT('Ctrl Pts',(8.21074211962818E-15,2.98894050139723,
15.702256783585));
#49976=CARTESIAN_POINT('Ctrl Pts',(2.17675697203127E-14,3.11999970392103,
15.7791547732152));
#49977=CARTESIAN_POINT('Ctrl Pts',(2.56461518688411E-14,3.24761139159044,
15.861602893881));
#49978=CARTESIAN_POINT('Ctrl Pts',(2.9518609317083E-14,3.3750215666168,
15.9439208200559));
#49979=CARTESIAN_POINT('Ctrl Pts',(8.03728488918813E-15,3.4989958079745,
16.0317717068427));
#49980=CARTESIAN_POINT('Ctrl Pts',(8.04911692853238E-15,3.6191747643727,
16.1249358268418));
#49981=CARTESIAN_POINT('Ctrl Pts',(8.05250885098475E-15,3.65362678812349,
16.1516434349882));
#49982=CARTESIAN_POINT('Ctrl Pts',(1.34374591162967E-14,3.68776674753865,
16.1787879738458));
#49983=CARTESIAN_POINT('Ctrl Pts',(1.32116539930394E-14,3.72158574495427,
16.2063649308754));
#49984=CARTESIAN_POINT('Ctrl Pts',(1.30778498935537E-14,3.74162568217725,
16.2227060565711));
#49985=CARTESIAN_POINT('Ctrl Pts',(5.34802515091838E-15,3.76155291509913,
16.239199023854));
#49986=CARTESIAN_POINT('Ctrl Pts',(5.16253706450698E-15,3.78136555481421,
16.255842940216));
#49987=CARTESIAN_POINT('Ctrl Pts',(5.02425027734796E-15,3.79613645651655,
16.2682514660894));
#49988=CARTESIAN_POINT('Ctrl Pts',(1.38281244415282E-14,3.81084283987857,
16.2807432594011));
#49989=CARTESIAN_POINT('Ctrl Pts',(1.38777878078145E-14,3.82547437708717,
16.2933095461151));
#49990=CARTESIAN_POINT('Ctrl Pts',(1.42788781872578E-14,3.94364133292775,
16.3947971633111));
#49991=CARTESIAN_POINT('Ctrl Pts',(2.05682746198613E-14,4.05709628359361,
16.5012804183751));
#49992=CARTESIAN_POINT('Ctrl Pts',(1.84297022087776E-14,4.16550570005553,
16.6124427404842));
#49993=CARTESIAN_POINT('Ctrl Pts',(1.79821344800749E-14,4.18819399250913,
16.6357071704216));
#49994=CARTESIAN_POINT('Ctrl Pts',(6.4338797725629E-15,4.21066124423878,
16.6591767169253));
#49995=CARTESIAN_POINT('Ctrl Pts',(6.0507154842071E-15,4.2329043100469,
16.6828487513009));
#49996=CARTESIAN_POINT('Ctrl Pts',(4.23927623984675E-15,4.33806014931527,
16.7947601516193));
#49997=CARTESIAN_POINT('Ctrl Pts',(1.36309249628105E-14,4.4382076506583,
16.9111934994602));
#49998=CARTESIAN_POINT('Ctrl Pts',(1.2490009027033E-14,4.5332160691296,
17.0317215451736));
#49999=CARTESIAN_POINT('Ctrl Pts',(1.1335668032986E-14,4.62934244337141,
17.1536678338847));
#50000=CARTESIAN_POINT('Ctrl Pts',(6.63949211684557E-15,4.72020856568058,
17.2798062617839));
#50001=CARTESIAN_POINT('Ctrl Pts',(6.93889390390723E-15,4.80564662961519,
17.4097367836627));
#50002=CARTESIAN_POINT('Ctrl Pts',(7.23151701427986E-15,4.88915031293694,
17.5367255829536));
#50003=CARTESIAN_POINT('Ctrl Pts',(-4.03556871303723E-15,4.96746921735247,
17.6673373941001));
#50004=CARTESIAN_POINT('Ctrl Pts',(-6.16173778666962E-15,5.0404106198303,
17.8012298339498));
#50005=CARTESIAN_POINT('Ctrl Pts',(-6.60825461783724E-15,5.05572904596076,
17.8293485892739));
#50006=CARTESIAN_POINT('Ctrl Pts',(3.02869902184406E-15,5.07081016404348,
17.8576121252524));
#50007=CARTESIAN_POINT('Ctrl Pts',(3.10862446895044E-15,5.08565196321491,
17.8860174072779));
#50008=CARTESIAN_POINT('Ctrl Pts',(3.15744306202177E-15,5.0947173582853,
17.9033673997332));
#50009=CARTESIAN_POINT('Ctrl Pts',(1.36778384139571E-15,5.10369272421503,
17.9207689458792));
#50010=CARTESIAN_POINT('Ctrl Pts',(1.4432899320127E-15,5.11257226278412,
17.9382105143602));
#50011=CARTESIAN_POINT('Ctrl Pts',(2.05664622361767E-15,5.18470314392759,
18.079893068388));
#50012=CARTESIAN_POINT('Ctrl Pts',(7.16626964594806E-16,5.25061395420093,
18.2244048189638));
#50013=CARTESIAN_POINT('Ctrl Pts',(-1.11022302462516E-15,5.31017458672414,
18.3712949565427));
#50014=CARTESIAN_POINT('Ctrl Pts',(-2.95761469161467E-15,5.37040493779473,
18.519836773182));
#50015=CARTESIAN_POINT('Ctrl Pts',(1.14248619537007E-14,5.42414199716124,
18.6708113453056));
#50016=CARTESIAN_POINT('Ctrl Pts',(9.76996261670138E-15,5.47121450010452,
18.8237908267476));
#50017=CARTESIAN_POINT('Ctrl Pts',(8.88107335987433E-15,5.49649835950476,
18.9059600647965));
#50018=CARTESIAN_POINT('Ctrl Pts',(-1.31658901812416E-14,5.51985879624915,
18.9887083281946));
#50019=CARTESIAN_POINT('Ctrl Pts',(-1.43218770176645E-14,5.54126420042667,
19.0719728906149));
#50020=CARTESIAN_POINT('Ctrl Pts',(-1.64684981599728E-14,5.5809146660826,
19.226208645531));
#50021=CARTESIAN_POINT('Ctrl Pts',(7.69447901493824E-15,5.61385999669503,
19.3822149699441));
#50022=CARTESIAN_POINT('Ctrl Pts',(8.32667268468867E-15,5.64014328124797,
19.5395658386989));
#50023=CARTESIAN_POINT('Ctrl Pts',(8.72173319680612E-15,5.65656781751344,
19.6378950655905));
#50024=CARTESIAN_POINT('Ctrl Pts',(-8.32468647422183E-15,5.67038981606524,
19.7367497662378));
#50025=CARTESIAN_POINT('Ctrl Pts',(-9.04831765069503E-15,5.68160986215254,
19.8360286798643));
#50026=CARTESIAN_POINT('Ctrl Pts',(-9.32229125156183E-15,5.68585787761729,
19.873616614631));
#50027=CARTESIAN_POINT('Ctrl Pts',(-9.03082511654983E-15,5.68973283677329,
19.911265372205));
#50028=CARTESIAN_POINT('Ctrl Pts',(-9.10382880192628E-15,5.69323448040224,
19.948969495901));
#50029=CARTESIAN_POINT('Ctrl Pts',(-9.14545097407185E-15,5.69523090035235,
19.9704660480131));
#50030=CARTESIAN_POINT('Ctrl Pts',(-1.69075485132513E-14,5.69710600165537,
19.991981655482));
#50031=CARTESIAN_POINT('Ctrl Pts',(-1.68198788230711E-14,5.69885847879252,
20.013498207624));
#50032=CARTESIAN_POINT('Ctrl Pts',(-1.61588887191719E-14,5.71207136961703,
20.1757233507338));
#50033=CARTESIAN_POINT('Ctrl Pts',(6.30550755751366E-15,5.71833945842108,
20.3382232791638));
#50034=CARTESIAN_POINT('Ctrl Pts',(3.96904731303493E-15,5.7177783220589,
20.500534488949));
#50035=CARTESIAN_POINT('Ctrl Pts',(1.60991114576845E-15,5.71721173972995,
20.6644209690473));
#50036=CARTESIAN_POINT('Ctrl Pts',(-2.78263791069445E-14,5.70968286987112,
20.8281157599009));
#50037=CARTESIAN_POINT('Ctrl Pts',(-2.39530617562878E-14,5.69526111488175,
20.9911627693061));
#50038=CARTESIAN_POINT('Ctrl Pts',(-2.00744932912372E-14,5.68081980810295,
21.154430823986));
#50039=CARTESIAN_POINT('Ctrl Pts',(-1.1625797255892E-14,5.65946699454297,
21.3170501028641));
#50040=CARTESIAN_POINT('Ctrl Pts',(-1.21846976952611E-14,5.63122133755543,
21.4785725032748));
#50041=CARTESIAN_POINT('Ctrl Pts',(-1.26905279506821E-14,5.60565773645204,
21.6247576040562));
#50042=CARTESIAN_POINT('Ctrl Pts',(1.23920388915437E-16,5.57444757028604,
21.7700447797953));
#50043=CARTESIAN_POINT('Ctrl Pts',(7.49400541621981E-16,5.53756786262954,
21.9141008375364));
#50044=CARTESIAN_POINT('Ctrl Pts',(1.06565608626021E-15,5.52213270144179,
21.9743922176096));
#50045=CARTESIAN_POINT('Ctrl Pts',(-1.01203093583408E-14,5.50570400498667,
22.0344678920767));
#50046=CARTESIAN_POINT('Ctrl Pts',(-1.09356967925578E-14,5.48829300650687,
22.0943080987843));
#50047=CARTESIAN_POINT('Ctrl Pts',(-1.13800492473829E-14,5.4788047318649,
22.1269185384746));
#50048=CARTESIAN_POINT('Ctrl Pts',(-2.68295561497439E-15,5.46902471491014,
22.1594590442228));
#50049=CARTESIAN_POINT('Ctrl Pts',(-2.24820162486594E-15,5.45895464414269,
22.1919263783269));
#50050=CARTESIAN_POINT('Ctrl Pts',(-1.96639678768615E-15,5.45242728679215,
22.2129715027168));
#50051=CARTESIAN_POINT('Ctrl Pts',(-7.76142744149267E-15,5.44578086478645,
22.2339768276455));
#50052=CARTESIAN_POINT('Ctrl Pts',(-7.66053886991358E-15,5.43901644566141,
22.2549406076277));
#50053=CARTESIAN_POINT('Ctrl Pts',(-6.90260989493124E-15,5.38819850688457,
22.4124317488445));
#50054=CARTESIAN_POINT('Ctrl Pts',(-6.54588297085908E-15,5.33072013492139,
22.5675950757115));
#50055=CARTESIAN_POINT('Ctrl Pts',(-5.78703751585863E-15,5.26688451533375,
22.720075001107));
#50056=CARTESIAN_POINT('Ctrl Pts',(-5.01909383498359E-15,5.20228353452266,
22.8743830942717));
#50057=CARTESIAN_POINT('Ctrl Pts',(-2.52391800493359E-15,5.13117177003407,
23.0259437296997));
#50058=CARTESIAN_POINT('Ctrl Pts',(-2.63677968348475E-16,5.05381061639661,
23.1743822794189));
#50059=CARTESIAN_POINT('Ctrl Pts',(6.63362861739138E-16,5.02208082357648,
23.2352645725034));
#50060=CARTESIAN_POINT('Ctrl Pts',(-4.63064774168416E-15,4.98929913677184,
23.295621526562));
#50061=CARTESIAN_POINT('Ctrl Pts',(-4.95437024738976E-15,4.95548117923701,
23.3554265883461));
#50062=CARTESIAN_POINT('Ctrl Pts',(-5.1966435182712E-15,4.9301718879703,
23.4001845760619));
#50063=CARTESIAN_POINT('Ctrl Pts',(-3.73619989753743E-15,4.90428215327493,
23.4446334404272));
#50064=CARTESIAN_POINT('Ctrl Pts',(-3.52495810318487E-15,4.87781803474678,
23.4887618409189));
#50065=CARTESIAN_POINT('Ctrl Pts',(-3.41302455827604E-15,4.86379513454929,
23.5121447529667));
#50066=CARTESIAN_POINT('Ctrl Pts',(-5.11817456332583E-15,4.84961584756207,
23.5354295002362));
#50067=CARTESIAN_POINT('Ctrl Pts',(-5.37070388162419E-15,4.83528275213712,
23.5586123876325));
#50068=CARTESIAN_POINT('Ctrl Pts',(-6.94795543784049E-15,4.74576088110552,
23.7034084274336));
#50069=CARTESIAN_POINT('Ctrl Pts',(9.10527509405812E-15,4.65022657721916,
23.844259359632));
#50070=CARTESIAN_POINT('Ctrl Pts',(6.18255446838134E-15,4.54896272516647,
23.9807849350336));
#50071=CARTESIAN_POINT('Ctrl Pts',(3.25413836088581E-15,4.44750154107212,
24.1175765567093));
#50072=CARTESIAN_POINT('Ctrl Pts',(-5.59205196868429E-15,4.34028815806525,
24.2500266576816));
#50073=CARTESIAN_POINT('Ctrl Pts',(-5.15212872365112E-15,4.22755843067459,
24.3777346172277));
#50074=CARTESIAN_POINT('Ctrl Pts',(-5.0011400422891E-15,4.18886778842919,
24.4215660278862));
#50075=CARTESIAN_POINT('Ctrl Pts',(-3.56011120575155E-15,4.14952693581179,
24.4648386217493));
#50076=CARTESIAN_POINT('Ctrl Pts',(-4.29691004999455E-15,4.10954418789613,
24.5075354759874));
#50077=CARTESIAN_POINT('Ctrl Pts',(-5.03699156543988E-15,4.06880057339034,
24.5510448459126));
#50078=CARTESIAN_POINT('Ctrl Pts',(-5.30426572712612E-15,4.0273904007291,
24.5939563600081));
#50079=CARTESIAN_POINT('Ctrl Pts',(-5.27355936696949E-15,3.98533038287153,
24.6362610213063));
#50080=CARTESIAN_POINT('Ctrl Pts',(48.4490415053031,-5.1367692385953,19.9998673509107));
#50081=CARTESIAN_POINT('Ctrl Pts',(48.4130939002172,-5.13608619358257,20.6628267235351));
#50082=CARTESIAN_POINT('Ctrl Pts',(48.3771462951314,-5.00715967363253,21.3260440301722));
#50083=CARTESIAN_POINT('Ctrl Pts',(48.3411986900455,-4.75688882502728,21.9397791588711));
#50084=CARTESIAN_POINT('Ctrl Pts',(48.2948948598826,-4.43451689396667,22.7303265985789));
#50085=CARTESIAN_POINT('Ctrl Pts',(48.2485910297197,-3.91081269191307,23.4387741217238));
#50086=CARTESIAN_POINT('Ctrl Pts',(48.2022871995568,-3.24957242287801,23.9788206184102));
#50087=CARTESIAN_POINT('Ctrl Pts',(48.155983369394,-2.58833215384294,24.5188671150965));
#50088=CARTESIAN_POINT('Ctrl Pts',(48.1096795392311,-1.78955581782641,24.8905125853242));
#50089=CARTESIAN_POINT('Ctrl Pts',(48.0633757090682,-0.950548140765501,
25.0484841981418));
#50090=CARTESIAN_POINT('Ctrl Pts',(48.0170718789054,-0.111540463704582,
25.2064558109594));
#50091=CARTESIAN_POINT('Ctrl Pts',(47.9707680487424,0.767698554400724,25.1507535663667));
#50092=CARTESIAN_POINT('Ctrl Pts',(47.9244642185796,1.58006244277662,24.8881629609726));
#50093=CARTESIAN_POINT('Ctrl Pts',(47.8781603884167,2.3924263311525,24.6255723555784));
#50094=CARTESIAN_POINT('Ctrl Pts',(47.8318565582538,3.13791508979897,24.1560933893826));
#50095=CARTESIAN_POINT('Ctrl Pts',(47.7855527280909,3.72571533683517,23.5369166923885));
#50096=CARTESIAN_POINT('Ctrl Pts',(47.7392488979281,4.31351558387138,22.9177399953943));
#50097=CARTESIAN_POINT('Ctrl Pts',(47.6929450677652,4.74362731929732,22.1488655676018));
#50098=CARTESIAN_POINT('Ctrl Pts',(47.6466412376023,4.96365551870842,21.3239555698276));
#50099=CARTESIAN_POINT('Ctrl Pts',(47.6003374074394,5.18368371811953,20.4990455720535));
#50100=CARTESIAN_POINT('Ctrl Pts',(47.5540335772765,5.1936283815158,19.6181000042978));
#50101=CARTESIAN_POINT('Ctrl Pts',(47.5077297471137,4.99227807759252,18.7884332230865));
#50102=CARTESIAN_POINT('Ctrl Pts',(47.4614259169508,4.79092777366925,17.9587664418752));
#50103=CARTESIAN_POINT('Ctrl Pts',(47.4151220867879,4.37828250242643,17.1803784472083));
#50104=CARTESIAN_POINT('Ctrl Pts',(47.368818256625,3.80460957149062,16.5480903157878));
#50105=CARTESIAN_POINT('Ctrl Pts',(47.3225144264621,3.23093664055482,15.9158021843672));
#50106=CARTESIAN_POINT('Ctrl Pts',(47.2762105962993,2.49623604992602,15.429613916193));
#50107=CARTESIAN_POINT('Ctrl Pts',(47.2299067661364,1.69000699719802,15.1487516237057));
#50108=CARTESIAN_POINT('Ctrl Pts',(47.1836029359735,0.883777944470023,14.8678893312184));
#50109=CARTESIAN_POINT('Ctrl Pts',(47.1372991058106,0.00602042964282193,
14.7923530144179));
#50110=CARTESIAN_POINT('Ctrl Pts',(47.0909952756477,-0.836339550193692,
14.9313442989241));
#50111=CARTESIAN_POINT('Ctrl Pts',(47.0446914454848,-1.67869953003021,15.0703355834303));
#50112=CARTESIAN_POINT('Ctrl Pts',(46.998387615322,-2.48566197487603,15.4238544692431));
#50113=CARTESIAN_POINT('Ctrl Pts',(46.9520837851592,-3.1589249475859,15.9488362616763));
#50114=CARTESIAN_POINT('Ctrl Pts',(46.9057799549963,-3.83218792029577,16.4738180541095));
#50115=CARTESIAN_POINT('Ctrl Pts',(46.8594761248333,-4.37175142086969,17.1702627531631));
#50116=CARTESIAN_POINT('Ctrl Pts',(46.8131722946705,-4.71188731332118,17.9533313883844));
#50117=CARTESIAN_POINT('Ctrl Pts',(46.7751286982147,-4.99134567750053,18.596706829482));
#50118=CARTESIAN_POINT('Ctrl Pts',(46.7370851017589,-5.13618249371292,19.2985568643818));
#50119=CARTESIAN_POINT('Ctrl Pts',(46.6990415053031,-5.13689122437247,20.0001232958892));
#50120=CARTESIAN_POINT('Ctrl Pts',(50.,-1.57888188187519,14.0941590297752));
#50121=CARTESIAN_POINT('Ctrl Pts',(50.,-1.73782238409694,14.1503790437278));
#50122=CARTESIAN_POINT('Ctrl Pts',(50.,-1.89403686188134,14.2131930374271));
#50123=CARTESIAN_POINT('Ctrl Pts',(50.,-2.04718622138767,14.2823105486562));
#50124=CARTESIAN_POINT('Ctrl Pts',(50.,-2.20154651490249,14.3519745639334));
#50125=CARTESIAN_POINT('Ctrl Pts',(50.,-2.35279365452493,14.4280426063853));
#50126=CARTESIAN_POINT('Ctrl Pts',(50.,-2.50055566660814,14.510263994692));
#50127=CARTESIAN_POINT('Ctrl Pts',(50.,-2.64732566541585,14.5919333824703));
#50128=CARTESIAN_POINT('Ctrl Pts',(50.,-2.79065771652978,14.6796742843768));
#50129=CARTESIAN_POINT('Ctrl Pts',(50.,-2.93015429364071,14.7732797038493));
#50130=CARTESIAN_POINT('Ctrl Pts',(50.,-3.06797652569821,14.8657615991873));
#50131=CARTESIAN_POINT('Ctrl Pts',(50.,-3.20205526958666,14.9639685708035));
#50132=CARTESIAN_POINT('Ctrl Pts',(50.,-3.33196742199994,15.0677313572818));
#50133=CARTESIAN_POINT('Ctrl Pts',(50.,-3.39602842604199,15.1188978429456));
#50134=CARTESIAN_POINT('Ctrl Pts',(50.,-3.45907563529118,15.171415690102));
#50135=CARTESIAN_POINT('Ctrl Pts',(50.,-3.52105417041813,15.2252668229557));
#50136=CARTESIAN_POINT('Ctrl Pts',(50.,-3.53896050140773,15.2408250514144));
#50137=CARTESIAN_POINT('Ctrl Pts',(50.,-3.55677761137173,15.2564945776178));
#50138=CARTESIAN_POINT('Ctrl Pts',(50.,-3.57450413028377,15.2722749853259));
#50139=CARTESIAN_POINT('Ctrl Pts',(50.,-3.59054569823461,15.2865554249204));
#50140=CARTESIAN_POINT('Ctrl Pts',(50.,-3.60650718940738,15.3009214523991));
#50141=CARTESIAN_POINT('Ctrl Pts',(50.,-3.62238388236175,15.3153689794615));
#50142=CARTESIAN_POINT('Ctrl Pts',(50.,-3.74452419973748,15.4265146409519));
#50143=CARTESIAN_POINT('Ctrl Pts',(50.,-3.86172403164677,15.5425475076359));
#50144=CARTESIAN_POINT('Ctrl Pts',(50.,-3.97363113502738,15.6632438417377));
#50145=CARTESIAN_POINT('Ctrl Pts',(50.,-3.99801652637559,15.6895444719252));
#50146=CARTESIAN_POINT('Ctrl Pts',(50.,-4.02215045555051,15.7160666739607));
#50147=CARTESIAN_POINT('Ctrl Pts',(50.,-4.04602902731229,15.7428083472572));
#50148=CARTESIAN_POINT('Ctrl Pts',(50.,-4.15602108936427,15.8659887375226));
#50149=CARTESIAN_POINT('Ctrl Pts',(50.,-4.26059857444806,15.9938238149227));
#50150=CARTESIAN_POINT('Ctrl Pts',(50.,-4.35955084737223,16.1259088074266));
#50151=CARTESIAN_POINT('Ctrl Pts',(50.,-4.45831511238434,16.2577428403221));
#50152=CARTESIAN_POINT('Ctrl Pts',(50.,-4.55147580303531,16.3938113843476));
#50153=CARTESIAN_POINT('Ctrl Pts',(50.,-4.63877567630947,16.5337316036845));
#50154=CARTESIAN_POINT('Ctrl Pts',(50.,-4.72210041196483,16.6672806553821));
#50155=CARTESIAN_POINT('Ctrl Pts',(50.,-4.80008581751703,16.8043392665965));
#50156=CARTESIAN_POINT('Ctrl Pts',(50.,-4.87246387825708,16.9445822178997));
#50157=CARTESIAN_POINT('Ctrl Pts',(50.,-4.89325145258022,16.9848611469523));
#50158=CARTESIAN_POINT('Ctrl Pts',(50.,-4.9135761991606,17.0254027646812));
#50159=CARTESIAN_POINT('Ctrl Pts',(50.,-4.93343106432601,17.0661993776146));
#50160=CARTESIAN_POINT('Ctrl Pts',(50.,-4.94259505699603,17.085029012506));
#50161=CARTESIAN_POINT('Ctrl Pts',(50.,-4.95165540161899,17.1039057211666));
#50162=CARTESIAN_POINT('Ctrl Pts',(50.,-4.96060966400913,17.1228243828118));
#50163=CARTESIAN_POINT('Ctrl Pts',(50.,-5.02975007299816,17.2689049807083));
#50164=CARTESIAN_POINT('Ctrl Pts',(50.,-5.09260924613714,17.4175665636468));
#50165=CARTESIAN_POINT('Ctrl Pts',(50.,-5.14899613636606,17.5684268921343));
#50166=CARTESIAN_POINT('Ctrl Pts',(50.,-5.20491428920055,17.7180331369684));
#50167=CARTESIAN_POINT('Ctrl Pts',(50.,-5.25446750278863,17.8698024305613));
#50168=CARTESIAN_POINT('Ctrl Pts',(50.,-5.29742025272067,18.0233748357436));
#50169=CARTESIAN_POINT('Ctrl Pts',(50.,-5.32033847663536,18.1053161963004));
#50170=CARTESIAN_POINT('Ctrl Pts',(50.,-5.34137672674639,18.1877710486224));
#50171=CARTESIAN_POINT('Ctrl Pts',(50.,-5.3604931415221,18.2706851930074));
#50172=CARTESIAN_POINT('Ctrl Pts',(50.,-5.39658046805671,18.4272077333405));
#50173=CARTESIAN_POINT('Ctrl Pts',(50.,-5.42582196978831,18.5853677668178));
#50174=CARTESIAN_POINT('Ctrl Pts',(50.,-5.44817286598194,18.7447104220605));
#50175=CARTESIAN_POINT('Ctrl Pts',(50.,-5.46135993546014,18.8387228789805));
#50176=CARTESIAN_POINT('Ctrl Pts',(50.,-5.47214740383625,18.9331468712938));
#50177=CARTESIAN_POINT('Ctrl Pts',(50.,-5.48051784692699,19.0278866066674));
#50178=CARTESIAN_POINT('Ctrl Pts',(50.,-5.48369364859717,19.0638314911341));
#50179=CARTESIAN_POINT('Ctrl Pts',(50.,-5.48652145884549,19.0998218024007));
#50180=CARTESIAN_POINT('Ctrl Pts',(50.,-5.48900009920885,19.1358522102154));
#50181=CARTESIAN_POINT('Ctrl Pts',(50.,-5.49086720863181,19.162993184331));
#50182=CARTESIAN_POINT('Ctrl Pts',(50.,-5.49253636532794,19.1901616141891));
#50183=CARTESIAN_POINT('Ctrl Pts',(50.,-5.49400565178386,19.2173257522691));
#50184=CARTESIAN_POINT('Ctrl Pts',(50.,-5.50252096464157,19.3747566829964));
#50185=CARTESIAN_POINT('Ctrl Pts',(50.,-5.50434139752314,19.5322154392954));
#50186=CARTESIAN_POINT('Ctrl Pts',(50.,-5.49949900939921,19.6892750140735));
#50187=CARTESIAN_POINT('Ctrl Pts',(50.,-5.49466981791964,19.845906564642));
#50188=CARTESIAN_POINT('Ctrl Pts',(50.,-5.4832139338339,20.002141867127));
#50189=CARTESIAN_POINT('Ctrl Pts',(50.,-5.46511202446615,20.1575502879913));
#50190=CARTESIAN_POINT('Ctrl Pts',(50.,-5.44732254602162,20.3102764284718));
#50191=CARTESIAN_POINT('Ctrl Pts',(50.,-5.42311424356855,20.4622046334804));
#50192=CARTESIAN_POINT('Ctrl Pts',(50.,-5.39242225163155,20.6129089430498));
#50193=CARTESIAN_POINT('Ctrl Pts',(50.,-5.36589148603084,20.7431807325253));
#50194=CARTESIAN_POINT('Ctrl Pts',(50.,-5.33451520914545,20.8725379853212));
#50195=CARTESIAN_POINT('Ctrl Pts',(50.,-5.29822455763965,21.0006893772657));
#50196=CARTESIAN_POINT('Ctrl Pts',(50.,-5.28325270927048,21.0535587287069));
#50197=CARTESIAN_POINT('Ctrl Pts',(50.,-5.26744412774905,21.1062226322689));
#50198=CARTESIAN_POINT('Ctrl Pts',(50.,-5.25080526889494,21.15866198357));
#50199=CARTESIAN_POINT('Ctrl Pts',(50.,-5.24128177427378,21.1886764145133));
#50200=CARTESIAN_POINT('Ctrl Pts',(50.,-5.23148626960332,21.2186172713547));
#50201=CARTESIAN_POINT('Ctrl Pts',(50.,-5.22141988715224,21.2484808831291));
#50202=CARTESIAN_POINT('Ctrl Pts',(50.,-5.21445283316468,21.269149817228));
#50203=CARTESIAN_POINT('Ctrl Pts',(50.,-5.20735673023832,21.2897795084358));
#50204=CARTESIAN_POINT('Ctrl Pts',(50.,-5.20013577259056,21.3103584645419));
#50205=CARTESIAN_POINT('Ctrl Pts',(50.,-5.14900190778098,21.4560845040486));
#50206=CARTESIAN_POINT('Ctrl Pts',(50.,-5.09156138048567,21.59941655586));
#50207=CARTESIAN_POINT('Ctrl Pts',(50.,-5.02803474960281,21.7399684337231));
#50208=CARTESIAN_POINT('Ctrl Pts',(50.,-4.96447673958616,21.8805897375281));
#50209=CARTESIAN_POINT('Ctrl Pts',(50.,-4.8948261396364,22.0184287712917));
#50210=CARTESIAN_POINT('Ctrl Pts',(50.,-4.81926289989551,22.1530664186381));
#50211=CARTESIAN_POINT('Ctrl Pts',(50.,-4.79092668499267,22.2035555363929));
#50212=CARTESIAN_POINT('Ctrl Pts',(50.,-4.7617586292794,22.2535940833528));
#50213=CARTESIAN_POINT('Ctrl Pts',(50.,-4.73176694583031,22.3031584989639));
#50214=CARTESIAN_POINT('Ctrl Pts',(50.,-4.71610121865025,22.3290477630367));
#50215=CARTESIAN_POINT('Ctrl Pts',(50.,-4.7002107665672,22.3548076534927));
#50216=CARTESIAN_POINT('Ctrl Pts',(50.,-4.6840966920901,22.3804347158741));
#50217=CARTESIAN_POINT('Ctrl Pts',(50.,-4.6698029103653,22.4031668707023));
#50218=CARTESIAN_POINT('Ctrl Pts',(50.,-4.65533244367626,22.4257955041634));
#50219=CARTESIAN_POINT('Ctrl Pts',(50.,-4.6406958078698,22.4483035164937));
#50220=CARTESIAN_POINT('Ctrl Pts',(50.,-4.55820044210185,22.5751637277094));
#50221=CARTESIAN_POINT('Ctrl Pts',(50.,-4.47036188468475,22.6983041039959));
#50222=CARTESIAN_POINT('Ctrl Pts',(50.,-4.37736498984394,22.8173359791823));
#50223=CARTESIAN_POINT('Ctrl Pts',(50.,-4.28579405817417,22.9345426851469));
#50224=CARTESIAN_POINT('Ctrl Pts',(50.,-4.18922125200072,23.0477663844785));
#50225=CARTESIAN_POINT('Ctrl Pts',(50.,-4.08779202142556,23.1565964011001));
#50226=CARTESIAN_POINT('Ctrl Pts',(50.,-4.0549933858478,23.1917881898463));
#50227=CARTESIAN_POINT('Ctrl Pts',(50.,-4.02168672604364,23.2265202123558));
#50228=CARTESIAN_POINT('Ctrl Pts',(50.,-3.98787638414422,23.2607775544223));
#50229=CARTESIAN_POINT('Ctrl Pts',(50.,-3.95255838902044,23.2965624821128));
#50230=CARTESIAN_POINT('Ctrl Pts',(50.,-3.91669078391207,23.3318294533088));
#50231=CARTESIAN_POINT('Ctrl Pts',(50.,-3.88028650238535,23.3665676072239));
#50232=CARTESIAN_POINT('Origin',(50.,-18.,12.));
#50233=CARTESIAN_POINT('',(50.,-18.,12.));
#50234=CARTESIAN_POINT('',(50.,18.,12.));
#50235=CARTESIAN_POINT('',(50.,-18.,12.));
#50236=CARTESIAN_POINT('',(50.,18.,28.));
#50237=CARTESIAN_POINT('',(50.,18.,12.));
#50238=CARTESIAN_POINT('',(50.,12.,28.));
#50239=CARTESIAN_POINT('',(50.,-18.,28.));
#50240=CARTESIAN_POINT('',(50.,12.,48.));
#50241=CARTESIAN_POINT('',(50.,12.,28.));
#50242=CARTESIAN_POINT('',(50.,-12.,48.));
#50243=CARTESIAN_POINT('',(50.,-12.,48.));
#50244=CARTESIAN_POINT('',(50.,-12.,28.));
#50245=CARTESIAN_POINT('',(50.,-12.,28.));
#50246=CARTESIAN_POINT('',(50.,-18.,28.));
#50247=CARTESIAN_POINT('',(50.,-18.,28.));
#50248=CARTESIAN_POINT('',(50.,-18.,12.));
#50249=CARTESIAN_POINT('Origin',(25.,0.,20.));
#50250=CARTESIAN_POINT('Origin',(20.,-12.,48.));
#50251=CARTESIAN_POINT('',(20.,12.,48.));
#50252=CARTESIAN_POINT('',(20.,-12.,48.));
#50253=CARTESIAN_POINT('',(20.,-6.,48.));
#50254=CARTESIAN_POINT('',(20.,12.,73.));
#50255=CARTESIAN_POINT('',(20.,12.,48.));
#50256=CARTESIAN_POINT('',(20.,-12.,73.));
#50257=CARTESIAN_POINT('',(20.,-12.,73.));
#50258=CARTESIAN_POINT('',(20.,-12.,48.));
#50259=CARTESIAN_POINT('Origin',(10.,0.,73.));
#50260=CARTESIAN_POINT('',(0.,12.,73.));
#50261=CARTESIAN_POINT('',(0.,-12.,73.));
#50262=CARTESIAN_POINT('',(0.,12.,73.));
#50263=CARTESIAN_POINT('',(0.,-12.,73.));
#50264=CARTESIAN_POINT('',(20.,12.,73.));
#50265=CARTESIAN_POINT('Origin',(25.,0.,48.));
#50266=CARTESIAN_POINT('',(0.,-12.,48.));
#50267=CARTESIAN_POINT('',(50.,12.,48.));
#50268=CARTESIAN_POINT('Origin',(50.,12.,28.));
#50269=CARTESIAN_POINT('',(0.,12.,28.));
#50270=CARTESIAN_POINT('',(37.5,12.,28.));
#50271=CARTESIAN_POINT('',(0.,12.,28.));
#50272=CARTESIAN_POINT('Origin',(0.,-12.,28.));
#50273=CARTESIAN_POINT('',(0.,-12.,28.));
#50274=CARTESIAN_POINT('',(12.5,-12.,28.));
#50275=CARTESIAN_POINT('',(0.,-12.,28.));
#50276=CARTESIAN_POINT('Origin',(25.,0.,28.));
#50277=CARTESIAN_POINT('',(0.,18.,28.));
#50278=CARTESIAN_POINT('',(50.,18.,28.));
#50279=CARTESIAN_POINT('',(0.,18.,28.));
#50280=CARTESIAN_POINT('Origin',(25.,0.,28.));
#50281=CARTESIAN_POINT('',(0.,-18.,28.));
#50282=CARTESIAN_POINT('',(0.,18.,28.));
#50283=CARTESIAN_POINT('',(0.,-18.,28.));
#50284=CARTESIAN_POINT('Origin',(50.,18.,12.));
#50285=CARTESIAN_POINT('',(0.,18.,12.));
#50286=CARTESIAN_POINT('',(50.,18.,12.));
#50287=CARTESIAN_POINT('',(0.,18.,12.));
#50288=CARTESIAN_POINT('Origin',(0.,-18.,12.));
#50289=CARTESIAN_POINT('',(0.,-18.,12.));
#50290=CARTESIAN_POINT('',(0.,-18.,12.));
#50291=CARTESIAN_POINT('',(0.,-18.,12.));
#50292=CARTESIAN_POINT('Origin',(0.,18.,12.));
#50293=CARTESIAN_POINT('',(0.,18.,12.));
#50294=CARTESIAN_POINT('Origin',(25.,0.,12.));
#50295=CARTESIAN_POINT('',(0.,0.,0.));
#50296=CARTESIAN_POINT('Origin',(92.,-24.,25.));
#50297=CARTESIAN_POINT('',(88.5,-24.,40.));
#50298=CARTESIAN_POINT('Origin',(92.,-24.,40.));
#50299=CARTESIAN_POINT('',(88.5,-24.,10.));
#50300=CARTESIAN_POINT('',(88.5,-24.,25.));
#50301=CARTESIAN_POINT('Origin',(92.,-24.,10.));
#50302=CARTESIAN_POINT('Origin',(92.,24.,25.));
#50303=CARTESIAN_POINT('',(88.5,24.,40.));
#50304=CARTESIAN_POINT('Origin',(92.,24.,40.));
#50305=CARTESIAN_POINT('',(88.5,24.,10.));
#50306=CARTESIAN_POINT('',(88.5,24.,25.));
#50307=CARTESIAN_POINT('Origin',(92.,24.,10.));
#50308=CARTESIAN_POINT('Origin',(90.5,0.,20.));
#50309=CARTESIAN_POINT('',(88.,-4.58257569495584,10.));
#50310=CARTESIAN_POINT('',(93.,-4.58257569495584,10.));
#50311=CARTESIAN_POINT('',(90.5,-4.58257569495584,10.));
#50312=CARTESIAN_POINT('',(88.,-7.54983443527075,12.));
#50313=CARTESIAN_POINT('Origin',(88.,0.,20.));
#50314=CARTESIAN_POINT('',(93.,-7.54983443527075,12.));
#50315=CARTESIAN_POINT('',(90.5,-7.54983443527075,12.));
#50316=CARTESIAN_POINT('Origin',(93.,0.,20.));
#50317=CARTESIAN_POINT('Origin',(90.5,0.,20.));
#50318=CARTESIAN_POINT('',(93.,4.58257569495584,10.));
#50319=CARTESIAN_POINT('',(88.,4.58257569495584,10.));
#50320=CARTESIAN_POINT('',(90.5,4.58257569495584,10.));
#50321=CARTESIAN_POINT('',(93.,7.54983443527075,12.));
#50322=CARTESIAN_POINT('Origin',(93.,0.,20.));
#50323=CARTESIAN_POINT('',(88.,7.54983443527075,12.));
#50324=CARTESIAN_POINT('',(90.5,7.54983443527075,12.));
#50325=CARTESIAN_POINT('Origin',(88.,0.,20.));
#50326=CARTESIAN_POINT('Origin',(93.,12.,40.));
#50327=CARTESIAN_POINT('',(93.,-18.,12.));
#50328=CARTESIAN_POINT('',(93.,-18.,12.));
#50329=CARTESIAN_POINT('',(93.,-18.,28.));
#50330=CARTESIAN_POINT('',(93.,-18.,28.));
#50331=CARTESIAN_POINT('',(93.,-12.,28.));
#50332=CARTESIAN_POINT('',(93.,-18.,28.));
#50333=CARTESIAN_POINT('',(93.,-12.,40.));
#50334=CARTESIAN_POINT('',(93.,-12.,40.));
#50335=CARTESIAN_POINT('',(93.,12.,40.));
#50336=CARTESIAN_POINT('',(93.,6.,40.));
#50337=CARTESIAN_POINT('',(93.,12.,28.));
#50338=CARTESIAN_POINT('',(93.,12.,40.));
#50339=CARTESIAN_POINT('',(93.,18.,28.));
#50340=CARTESIAN_POINT('',(93.,-18.,28.));
#50341=CARTESIAN_POINT('',(93.,18.,12.));
#50342=CARTESIAN_POINT('',(93.,18.,28.));
#50343=CARTESIAN_POINT('',(93.,-18.,12.));
#50344=CARTESIAN_POINT('',(93.,0.,10.));
#50345=CARTESIAN_POINT('',(93.,-7.,20.));
#50346=CARTESIAN_POINT('Origin',(93.,0.,20.));
#50347=CARTESIAN_POINT('Origin',(88.,30.,10.));
#50348=CARTESIAN_POINT('',(88.,-30.,10.));
#50349=CARTESIAN_POINT('',(88.,30.,10.));
#50350=CARTESIAN_POINT('',(88.,-30.,40.));
#50351=CARTESIAN_POINT('',(88.,-30.,10.));
#50352=CARTESIAN_POINT('',(88.,-12.,40.));
#50353=CARTESIAN_POINT('',(88.,30.,40.));
#50354=CARTESIAN_POINT('',(88.,-12.,28.));
#50355=CARTESIAN_POINT('',(88.,-12.,25.));
#50356=CARTESIAN_POINT('',(88.,-18.,28.));
#50357=CARTESIAN_POINT('',(88.,15.,28.));
#50358=CARTESIAN_POINT('',(88.,-18.,12.));
#50359=CARTESIAN_POINT('',(88.,-18.,19.));
#50360=CARTESIAN_POINT('',(88.,15.,12.));
#50361=CARTESIAN_POINT('Origin',(88.,30.,10.));
#50362=CARTESIAN_POINT('',(88.,18.,12.));
#50363=CARTESIAN_POINT('',(88.,15.,12.));
#50364=CARTESIAN_POINT('',(88.,18.,28.));
#50365=CARTESIAN_POINT('',(88.,18.,19.));
#50366=CARTESIAN_POINT('',(88.,12.,28.));
#50367=CARTESIAN_POINT('',(88.,15.,28.));
#50368=CARTESIAN_POINT('',(88.,12.,40.));
#50369=CARTESIAN_POINT('',(88.,12.,25.));
#50370=CARTESIAN_POINT('',(88.,30.,40.));
#50371=CARTESIAN_POINT('',(88.,30.,40.));
#50372=CARTESIAN_POINT('',(88.,30.,10.));
#50373=CARTESIAN_POINT('',(88.,30.,10.));
#50374=CARTESIAN_POINT('',(88.,30.,10.));
#50375=CARTESIAN_POINT('Origin',(90.5,0.,12.));
#50376=CARTESIAN_POINT('',(88.,-18.,12.));
#50377=CARTESIAN_POINT('Origin',(101.,0.,20.));
#50378=CARTESIAN_POINT('',(101.,4.58257569495584,10.));
#50379=CARTESIAN_POINT('',(101.,-4.58257569495584,10.));
#50380=CARTESIAN_POINT('',(101.,0.,10.));
#50381=CARTESIAN_POINT('Origin',(101.,0.,20.));
#50382=CARTESIAN_POINT('',(101.,-7.,20.));
#50383=CARTESIAN_POINT('Origin',(101.,0.,20.));
#50384=CARTESIAN_POINT('Origin',(104.5,0.,20.));
#50385=CARTESIAN_POINT('',(108.,4.58257569495584,10.));
#50386=CARTESIAN_POINT('',(104.5,4.58257569495584,10.));
#50387=CARTESIAN_POINT('',(108.,-4.58257569495584,10.));
#50388=CARTESIAN_POINT('Origin',(108.,0.,20.));
#50389=CARTESIAN_POINT('',(104.5,-4.58257569495584,10.));
#50390=CARTESIAN_POINT('Origin',(98.,0.,10.));
#50391=CARTESIAN_POINT('',(108.,30.,10.));
#50392=CARTESIAN_POINT('',(108.,30.,10.));
#50393=CARTESIAN_POINT('',(108.,-30.,10.));
#50394=CARTESIAN_POINT('',(108.,-30.,10.));
#50395=CARTESIAN_POINT('',(108.,-30.,10.));
#50396=CARTESIAN_POINT('',(88.,-30.,10.));
#50397=CARTESIAN_POINT('Origin',(100.5,0.,20.));
#50398=CARTESIAN_POINT('',(100.5,-7.,20.));
#50399=CARTESIAN_POINT('Origin',(90.5,0.,28.));
#50400=CARTESIAN_POINT('',(88.,-12.,28.));
#50401=CARTESIAN_POINT('',(88.,-18.,28.));
#50402=CARTESIAN_POINT('Origin',(93.,-18.,28.));
#50403=CARTESIAN_POINT('Origin',(88.,18.,28.));
#50404=CARTESIAN_POINT('',(93.,18.,28.));
#50405=CARTESIAN_POINT('',(93.,18.,12.));
#50406=CARTESIAN_POINT('Origin',(90.5,0.,28.));
#50407=CARTESIAN_POINT('',(93.,12.,28.));
#50408=CARTESIAN_POINT('Origin',(90.5,0.,12.));
#50409=CARTESIAN_POINT('Origin',(93.,-12.,40.));
#50410=CARTESIAN_POINT('',(95.5,-12.,40.));
#50411=CARTESIAN_POINT('Origin',(88.,12.,40.));
#50412=CARTESIAN_POINT('',(93.,12.,40.));
#50413=CARTESIAN_POINT('Origin',(108.,30.,10.));
#50414=CARTESIAN_POINT('',(108.,30.,40.));
#50415=CARTESIAN_POINT('',(108.,30.,40.));
#50416=CARTESIAN_POINT('',(108.,30.,10.));
#50417=CARTESIAN_POINT('Origin',(108.,-30.,10.));
#50418=CARTESIAN_POINT('',(108.,-30.,40.));
#50419=CARTESIAN_POINT('',(108.,-30.,40.));
#50420=CARTESIAN_POINT('',(108.,-30.,10.));
#50421=CARTESIAN_POINT('Origin',(88.,-30.,10.));
#50422=CARTESIAN_POINT('',(88.,-30.,40.));
#50423=CARTESIAN_POINT('Origin',(98.,0.,40.));
#50424=CARTESIAN_POINT('',(0.,0.,0.));
#50425=CARTESIAN_POINT('Origin',(0.,0.,0.));
#50426=CARTESIAN_POINT('',(-5.91687703775647,0.000148475150406543,0.563375192204898));
#50427=CARTESIAN_POINT('',(-5.91673042899974,9.84771958866994E-5,0.311624807795177));
#50428=CARTESIAN_POINT('',(-5.91675,-7.2459289488551E-16,0.));
#50429=CARTESIAN_POINT('',(2.58391981634401,5.32271443393357,0.));
#50430=CARTESIAN_POINT('Ctrl Pts',(-5.91687703775647,0.000148475150406543,
0.563375192204898));
#50431=CARTESIAN_POINT('Ctrl Pts',(-5.91706992944422,0.187583717190912,
0.554551266666524));
#50432=CARTESIAN_POINT('Ctrl Pts',(-5.90834010273356,0.37500100085716,0.54572734112815));
#50433=CARTESIAN_POINT('Ctrl Pts',(-5.89055564988372,0.561555006704539,
0.536903415589775));
#50434=CARTESIAN_POINT('Ctrl Pts',(-5.79705517096023,1.54234924530742,0.490512263115791));
#50435=CARTESIAN_POINT('Ctrl Pts',(-5.4532798607574,2.49928201164809,0.444121110641807));
#50436=CARTESIAN_POINT('Ctrl Pts',(-4.90126263075179,3.31535838460278,0.397729958167823));
#50437=CARTESIAN_POINT('Ctrl Pts',(-4.34924540074619,4.13143475755746,0.351338805693839));
#50438=CARTESIAN_POINT('Ctrl Pts',(-3.5889862509378,4.80665473712616,0.304947653219855));
#50439=CARTESIAN_POINT('Ctrl Pts',(-2.71343949032745,5.25844743535226,0.258556500745871));
#50440=CARTESIAN_POINT('Ctrl Pts',(-1.83789272971711,5.71024013357837,0.212165348271887));
#50441=CARTESIAN_POINT('Ctrl Pts',(-0.847058358304818,5.93860555046189,
0.165774195797903));
#50442=CARTESIAN_POINT('Ctrl Pts',(0.137915404672155,5.91564817616819,0.119383043323919));
#50443=CARTESIAN_POINT('Ctrl Pts',(0.982826263370534,5.89595533199605,0.0795886955492792));
#50444=CARTESIAN_POINT('Ctrl Pts',(1.82342476052313,5.69133378081125,0.0397943477746398));
#50445=CARTESIAN_POINT('Ctrl Pts',(2.58415070483638,5.32291852118006,2.34187669256869E-16));
#50446=CARTESIAN_POINT('',(-2.58391981634374,5.3227144339337,0.));
#50447=CARTESIAN_POINT('Origin',(0.,0.,0.));
#50448=CARTESIAN_POINT('Ctrl Pts',(-2.58391981634373,5.3227144339337,-1.4432899320127E-14));
#50449=CARTESIAN_POINT('Ctrl Pts',(-3.47048393011347,4.89233053668302,0.0463911524739698));
#50450=CARTESIAN_POINT('Ctrl Pts',(-4.24698760664896,4.23637732443745,0.0927823049479542));
#50451=CARTESIAN_POINT('Ctrl Pts',(-4.81877652593489,3.43418004707672,0.139173457421938));
#50452=CARTESIAN_POINT('Ctrl Pts',(-5.39056544522082,2.63198276971599,0.185564609895923));
#50453=CARTESIAN_POINT('Ctrl Pts',(-5.7576396072572,1.6835414272401,0.231955762369907));
#50454=CARTESIAN_POINT('Ctrl Pts',(-5.8750816086466,0.705274673425957,0.278346914843891));
#50455=CARTESIAN_POINT('Ctrl Pts',(-5.9031632732299,0.471360413377589,0.289439545827653));
#50456=CARTESIAN_POINT('Ctrl Pts',(-5.91697246107877,0.235740914355538,
0.300532176811415));
#50457=CARTESIAN_POINT('Ctrl Pts',(-5.91673042899974,9.84771958866994E-5,
0.311624807795177));
#50458=CARTESIAN_POINT('Origin',(0.,0.,0.));
#50459=CARTESIAN_POINT('',(-5.91673471741553,-0.000155036278603748,2.3133751922049));
#50460=CARTESIAN_POINT('',(-5.91688804929001,-0.00014628683568293,2.06162480779517));
#50461=CARTESIAN_POINT('',(-5.91675,-7.2459289488551E-16,0.));
#50462=CARTESIAN_POINT('Ctrl Pts',(-5.91673471741553,-0.000155036278603748,
2.3133751922049));
#50463=CARTESIAN_POINT('Ctrl Pts',(-5.91595960263358,0.753200890966211,
2.277911763021));
#50464=CARTESIAN_POINT('Ctrl Pts',(-5.7715386236145,1.50684545302749,2.2424483338371));
#50465=CARTESIAN_POINT('Ctrl Pts',(-5.49078916335747,2.20572500170222,2.2069849046532));
#50466=CARTESIAN_POINT('Ctrl Pts',(-5.12352938849944,3.11995773242299,2.16059375217922));
#50467=CARTESIAN_POINT('Ctrl Pts',(-4.52297996781033,3.94047482528974,2.11420259970523));
#50468=CARTESIAN_POINT('Ctrl Pts',(-3.7625685915058,4.56695369006312,2.06781144723125));
#50469=CARTESIAN_POINT('Ctrl Pts',(-3.00215721520126,5.19343255483651,2.02142029475727));
#50470=CARTESIAN_POINT('Ctrl Pts',(-2.0818838832813,5.62587319151652,1.97502914228328));
#50471=CARTESIAN_POINT('Ctrl Pts',(-1.11426813628014,5.81140215018564,1.9286379898093));
#50472=CARTESIAN_POINT('Ctrl Pts',(-0.14665238927898,5.99693110885477,1.88224683733531));
#50473=CARTESIAN_POINT('Ctrl Pts',(0.868305772803379,5.93554838951301,1.83585568486133));
#50474=CARTESIAN_POINT('Ctrl Pts',(1.80650992910795,5.63475911385226,1.78946453238734));
#50475=CARTESIAN_POINT('Ctrl Pts',(2.74471408541252,5.33396983819152,1.74307337991336));
#50476=CARTESIAN_POINT('Ctrl Pts',(3.6061642359393,4.79377400621179,1.69668222743938));
#50477=CARTESIAN_POINT('Ctrl Pts',(4.28553300547993,4.08022000735929,1.65029107496539));
#50478=CARTESIAN_POINT('Ctrl Pts',(4.96490177502057,3.36666600850679,1.60389992249141));
#50479=CARTESIAN_POINT('Ctrl Pts',(5.46218916357505,2.47975384278151,1.55750877001742));
#50480=CARTESIAN_POINT('Ctrl Pts',(5.71659307223213,1.52792409666675,1.51111761754344));
#50481=CARTESIAN_POINT('Ctrl Pts',(5.97099698088921,0.57609435055201,1.46472646506946));
#50482=CARTESIAN_POINT('Ctrl Pts',(5.98251740964889,-0.440652975952207,
1.41833531259547));
#50483=CARTESIAN_POINT('Ctrl Pts',(5.74974578753971,-1.39800276984277,1.37194416012149));
#50484=CARTESIAN_POINT('Ctrl Pts',(5.51697416543054,-2.35535256373333,1.3255530076475));
#50485=CARTESIAN_POINT('Ctrl Pts',(5.03991049245251,-3.25330482501024,1.27916185517352));
#50486=CARTESIAN_POINT('Ctrl Pts',(4.37688415573885,-3.98206902990049,1.23277070269954));
#50487=CARTESIAN_POINT('Ctrl Pts',(3.71385781902519,-4.71083323479075,1.18637955022555));
#50488=CARTESIAN_POINT('Ctrl Pts',(2.86486881857591,-5.27040938329436,1.13998839775157));
#50489=CARTESIAN_POINT('Ctrl Pts',(1.93372094913206,-5.59237972963765,1.09359724527758));
#50490=CARTESIAN_POINT('Ctrl Pts',(1.0025730796882,-5.91435007598094,1.0472060928036));
#50491=CARTESIAN_POINT('Ctrl Pts',(-0.0107336587502209,-5.9987146201639,
1.00081494032962));
#50492=CARTESIAN_POINT('Ctrl Pts',(-0.982304785849564,-5.83515784283796,
0.954423787855632));
#50493=CARTESIAN_POINT('Ctrl Pts',(-1.95387591294891,-5.67160106551203,
0.908032635381648));
#50494=CARTESIAN_POINT('Ctrl Pts',(-2.88371142870917,-5.2601229666772,0.861641482907664));
#50495=CARTESIAN_POINT('Ctrl Pts',(-3.65812259986032,-4.65103488155748,
0.81525033043368));
#50496=CARTESIAN_POINT('Ctrl Pts',(-4.43253377101147,-4.04194679643775,
0.768859177959696));
#50497=CARTESIAN_POINT('Ctrl Pts',(-5.05152059755351,-3.23524872503314,
0.722468025485712));
#50498=CARTESIAN_POINT('Ctrl Pts',(-5.43940118700244,-2.32957183389829,
0.676076873011728));
#50499=CARTESIAN_POINT('Ctrl Pts',(-5.75350414307619,-1.59616109747218,
0.638509646076118));
#50500=CARTESIAN_POINT('Ctrl Pts',(-5.91605581529983,-0.797843557176284,
0.600942419140508));
#50501=CARTESIAN_POINT('Ctrl Pts',(-5.91687703775647,0.000148475150406543,
0.563375192204898));
#50502=CARTESIAN_POINT('Ctrl Pts',(-5.91673042899974,9.84771958866994E-5,
0.311624807795177));
#50503=CARTESIAN_POINT('Ctrl Pts',(-5.91596024431085,-0.749753351848488,
0.346923329285399));
#50504=CARTESIAN_POINT('Ctrl Pts',(-5.77290544891175,-1.49983745567011,
0.382221850775621));
#50505=CARTESIAN_POINT('Ctrl Pts',(-5.49469559885405,-2.1959450698255,0.417520372265843));
#50506=CARTESIAN_POINT('Ctrl Pts',(-5.12905774692967,-3.11080589411043,
0.463911524739827));
#50507=CARTESIAN_POINT('Ctrl Pts',(-4.5299722023385,-3.93243537752791,0.510302677213811));
#50508=CARTESIAN_POINT('Ctrl Pts',(-3.77067614149761,-4.56027540020292,
0.556693829687796));
#50509=CARTESIAN_POINT('Ctrl Pts',(-3.01138008065672,-5.18811542287793,
0.60308498216178));
#50510=CARTESIAN_POINT('Ctrl Pts',(-2.09187350356611,-5.62216598481048,
0.649476134635763));
#50511=CARTESIAN_POINT('Ctrl Pts',(-1.12458814094342,-5.80940752171066,
0.695867287109747));
#50512=CARTESIAN_POINT('Ctrl Pts',(-0.157302778320717,-5.99664905861084,
0.742258439583731));
#50513=CARTESIAN_POINT('Ctrl Pts',(0.857761369834063,-5.93708157047865,
0.788649592057716));
#50514=CARTESIAN_POINT('Ctrl Pts',(1.79649797196632,-5.63796225118424,0.8350407445317));
#50515=CARTESIAN_POINT('Ctrl Pts',(2.73523457409856,-5.33884293188984,0.881431897005684));
#50516=CARTESIAN_POINT('Ctrl Pts',(3.59764363020828,-4.80017178143322,0.927823049479668));
#50517=CARTESIAN_POINT('Ctrl Pts',(4.27827895860187,-4.08782410095791,0.974214201953652));
#50518=CARTESIAN_POINT('Ctrl Pts',(4.95891428699546,-3.37547642048261,1.02060535442764));
#50519=CARTESIAN_POINT('Ctrl Pts',(5.45777588767292,-2.48945220998862,1.06699650690162));
#50520=CARTESIAN_POINT('Ctrl Pts',(5.71386998951821,-1.53807662974237,1.1133876593756));
#50521=CARTESIAN_POINT('Ctrl Pts',(5.9699640913635,-0.586701049496119,1.15977881184959));
#50522=CARTESIAN_POINT('Ctrl Pts',(5.98329069437662,0.430025900502397,1.20616996432357));
#50523=CARTESIAN_POINT('Ctrl Pts',(5.75221997711583,1.38778803550136,1.25256111679756));
#50524=CARTESIAN_POINT('Ctrl Pts',(5.52114925985504,2.34555017050033,1.29895226927154));
#50525=CARTESIAN_POINT('Ctrl Pts',(5.04568122232034,3.24434749049973,1.34534342174553));
#50526=CARTESIAN_POINT('Ctrl Pts',(4.38395037427107,3.97428806732987,1.39173457421951));
#50527=CARTESIAN_POINT('Ctrl Pts',(3.7222195262218,4.70422864416001,1.43812572669349));
#50528=CARTESIAN_POINT('Ctrl Pts',(2.87422586765797,5.26531247782086,1.48451687916748));
#50529=CARTESIAN_POINT('Ctrl Pts',(1.94365137477809,5.58893631816464,1.53090803164146));
#50530=CARTESIAN_POINT('Ctrl Pts',(1.01307688189823,5.91256015850842,1.57729918411544));
#50531=CARTESIAN_POINT('Ctrl Pts',(-7.84452976816674E-5,5.99872400553511,
1.62369033658943));
#50532=CARTESIAN_POINT('Ctrl Pts',(-0.971938559216247,5.83689329055121,
1.67008148906341));
#50533=CARTESIAN_POINT('Ctrl Pts',(-1.94379867313481,5.67506257556731,1.7164726415374));
#50534=CARTESIAN_POINT('Ctrl Pts',(-2.87436357377604,5.26523729857281,1.76286379401138));
#50535=CARTESIAN_POINT('Ctrl Pts',(-3.64985542413063,4.65752553934663,1.80925494648536));
#50536=CARTESIAN_POINT('Ctrl Pts',(-4.42534727448522,4.04981378012046,1.85564609895935));
#50537=CARTESIAN_POINT('Ctrl Pts',(-5.04576607455317,3.2442155386626,1.90203725143333));
#50538=CARTESIAN_POINT('Ctrl Pts',(-5.43525473989259,2.33922944038597,1.94842840390732));
#50539=CARTESIAN_POINT('Ctrl Pts',(-5.75204442873269,1.603161128288,1.9861605385366));
#50540=CARTESIAN_POINT('Ctrl Pts',(-5.91606589125939,0.801344330739464,
2.02389267316589));
#50541=CARTESIAN_POINT('Ctrl Pts',(-5.91688804929001,-0.00014628683568293,
2.06162480779517));
#50542=CARTESIAN_POINT('Origin',(0.,0.,0.));
#50543=CARTESIAN_POINT('',(-5.91644339103703,0.000127799667652695,4.0633751922049));
#50544=CARTESIAN_POINT('',(-5.9163416407139,9.66719635090206E-5,3.81162480779517));
#50545=CARTESIAN_POINT('',(-5.91675,-7.2459289488551E-16,0.));
#50546=CARTESIAN_POINT('Ctrl Pts',(-5.91644339103703,0.000127799667652695,
4.0633751922049));
#50547=CARTESIAN_POINT('Ctrl Pts',(-5.91670480388819,0.333943128373217,
4.04766341184946));
#50548=CARTESIAN_POINT('Ctrl Pts',(-5.88892930320423,0.667715421417966,
4.03195163149402));
#50549=CARTESIAN_POINT('Ctrl Pts',(-5.83272798953327,0.996630632830126,
4.01623985113858));
#50550=CARTESIAN_POINT('Ctrl Pts',(-5.66678602415662,1.96779719565392,3.9698486986646));
#50551=CARTESIAN_POINT('Ctrl Pts',(-5.25302630322936,2.89661946143809,3.92345754619061));
#50552=CARTESIAN_POINT('Ctrl Pts',(-4.64203820294044,3.66953263245096,3.87706639371663));
#50553=CARTESIAN_POINT('Ctrl Pts',(-4.03105010265153,4.44244580346383,3.83067524124264));
#50554=CARTESIAN_POINT('Ctrl Pts',(-3.22283362300099,5.05944987970539,3.78428408876866));
#50555=CARTESIAN_POINT('Ctrl Pts',(-2.3162073909918,5.44510530110238,3.73789293629468));
#50556=CARTESIAN_POINT('Ctrl Pts',(-1.40958115898261,5.83076072249937,3.69150178382069));
#50557=CARTESIAN_POINT('Ctrl Pts',(-0.404545174614808,5.98506748905176,
3.64511063134671));
#50558=CARTESIAN_POINT('Ctrl Pts',(0.576017301791694,5.88915889463181,3.59871947887272));
#50559=CARTESIAN_POINT('Ctrl Pts',(1.55657977819819,5.79325030021187,3.55232832639874));
#50560=CARTESIAN_POINT('Ctrl Pts',(2.51266874664338,5.4471263448196,3.50593717392476));
#50561=CARTESIAN_POINT('Ctrl Pts',(3.32738557720147,4.89310674712962,3.45954602145077));
#50562=CARTESIAN_POINT('Ctrl Pts',(4.14210240775957,4.33908714943965,3.41315486897679));
#50563=CARTESIAN_POINT('Ctrl Pts',(4.81544710043059,3.57717190945197,3.36676371650281));
#50564=CARTESIAN_POINT('Ctrl Pts',(5.26509146752643,2.70051851627927,3.32037256402882));
#50565=CARTESIAN_POINT('Ctrl Pts',(5.71473583462227,1.82386512310658,3.27398141155484));
#50566=CARTESIAN_POINT('Ctrl Pts',(5.94067987614295,0.832473576748882,3.22759025908085));
#50567=CARTESIAN_POINT('Ctrl Pts',(5.91529797379783,-0.152441134100985,
3.18119910660687));
#50568=CARTESIAN_POINT('Ctrl Pts',(5.8899160714527,-1.13735584495085,3.13480795413288));
#50569=CARTESIAN_POINT('Ctrl Pts',(5.61320822524177,-2.11579372029289,3.0884168016589));
#50570=CARTESIAN_POINT('Ctrl Pts',(5.11900681811302,-2.96812358473493,3.04202564918492));
#50571=CARTESIAN_POINT('Ctrl Pts',(4.62480541098426,-3.82045344917698,2.99563449671093));
#50572=CARTESIAN_POINT('Ctrl Pts',(3.91311044293768,-4.54667530271904,2.94924334423695));
#50573=CARTESIAN_POINT('Ctrl Pts',(3.07093909483548,-5.05799579814922,2.90285219176296));
#50574=CARTESIAN_POINT('Ctrl Pts',(2.22876774673328,-5.5693162935794,2.85646103928898));
#50575=CARTESIAN_POINT('Ctrl Pts',(1.25612001857547,-5.86573543089771,2.81006988681499));
#50576=CARTESIAN_POINT('Ctrl Pts',(0.271919138825607,-5.91101077649929,
2.76367873434101));
#50577=CARTESIAN_POINT('Ctrl Pts',(-0.712281740924255,-5.95628612210086,
2.71728758186703));
#50578=CARTESIAN_POINT('Ctrl Pts',(-1.70803577226616,-5.7504176759857,2.67089642939304));
#50579=CARTESIAN_POINT('Ctrl Pts',(-2.59359457629318,-5.31857646296406,
2.62450527691906));
#50580=CARTESIAN_POINT('Ctrl Pts',(-3.4791533803202,-4.88673524994243,2.57811412444507));
#50581=CARTESIAN_POINT('Ctrl Pts',(-4.25451695703233,-4.22892127001432,
2.53172297197109));
#50582=CARTESIAN_POINT('Ctrl Pts',(-4.82488352247588,-3.42556380939725,
2.48533181949711));
#50583=CARTESIAN_POINT('Ctrl Pts',(-5.39525008791944,-2.62220634878019,
2.43894066702312));
#50584=CARTESIAN_POINT('Ctrl Pts',(-5.76061964209443,-1.67330540747417,
2.39254951454914));
#50585=CARTESIAN_POINT('Ctrl Pts',(-5.87631935466844,-0.694880752533762,
2.34615836207515));
#50586=CARTESIAN_POINT('Ctrl Pts',(-5.9035731385545,-0.464406765163384,
2.33523063878507));
#50587=CARTESIAN_POINT('Ctrl Pts',(-5.91697356177012,-0.2322946037521,2.32430291549498));
#50588=CARTESIAN_POINT('Ctrl Pts',(-5.91673471741553,-0.000155036278603748,
2.3133751922049));
#50589=CARTESIAN_POINT('Ctrl Pts',(-5.91688804929001,-0.00014628683568293,
2.06162480779517));
#50590=CARTESIAN_POINT('Ctrl Pts',(-5.9170767235097,-0.184077612962022,
2.07028382563987));
#50591=CARTESIAN_POINT('Ctrl Pts',(-5.90867065616891,-0.367991761119495,
2.07894284348457));
#50592=CARTESIAN_POINT('Ctrl Pts',(-5.89154378039528,-0.551090172782567,
2.08760186132927));
#50593=CARTESIAN_POINT('Ctrl Pts',(-5.7997856249477,-1.53204973257906,2.13399301380325));
#50594=CARTESIAN_POINT('Ctrl Pts',(-5.45771078344167,-2.48959489707664,
2.18038416627724));
#50595=CARTESIAN_POINT('Ctrl Pts',(-4.90714389560134,-3.30664895829955,
2.22677531875122));
#50596=CARTESIAN_POINT('Ctrl Pts',(-4.35657700776102,-4.12370301952246,
2.27316647122521));
#50597=CARTESIAN_POINT('Ctrl Pts',(-3.5975180735864,-4.8002659774707,2.31955762369919));
#50598=CARTESIAN_POINT('Ctrl Pts',(-2.72277535071871,-5.2536161718274,2.36594877617318));
#50599=CARTESIAN_POINT('Ctrl Pts',(-1.84803262785102,-5.7069663661841,2.41233992864716));
#50600=CARTESIAN_POINT('Ctrl Pts',(-0.857606116290267,-5.93710379694926,
2.45873108112114));
#50601=CARTESIAN_POINT('Ctrl Pts',(0.127407188700409,-5.91589012195794,
2.50512223359512));
#50602=CARTESIAN_POINT('Ctrl Pts',(1.11242049369109,-5.89467644696662,2.55151338606911));
#50603=CARTESIAN_POINT('Ctrl Pts',(2.09202059211168,-5.62211166621882,2.5979045385431));
#50604=CARTESIAN_POINT('Ctrl Pts',(2.94643420589685,-5.13152160469756,2.64429569101708));
#50605=CARTESIAN_POINT('Ctrl Pts',(3.80084781968202,-4.6409315431763,2.69068684349107));
#50606=CARTESIAN_POINT('Ctrl Pts',(4.53007494883177,-3.93231620088159,2.73707799596505));
#50607=CARTESIAN_POINT('Ctrl Pts',(5.04495479883511,-3.09231621821586,2.78346914843903));
#50608=CARTESIAN_POINT('Ctrl Pts',(5.55983464883846,-2.25231623555014,2.82986030091301));
#50609=CARTESIAN_POINT('Ctrl Pts',(5.8603672196954,-1.2809316125134,2.876251453387));
#50610=CARTESIAN_POINT('Ctrl Pts',(5.90980713825542,-0.296931141983866,
2.92264260586099));
#50611=CARTESIAN_POINT('Ctrl Pts',(5.95924705681544,0.687069328545672,2.96903375833497));
#50612=CARTESIAN_POINT('Ctrl Pts',(5.75759432307854,1.68368564656801,3.01542491080895));
#50613=CARTESIAN_POINT('Ctrl Pts',(5.32950451737138,2.57106400410279,3.06181606328293));
#50614=CARTESIAN_POINT('Ctrl Pts',(4.90141471166422,3.45844236163756,3.10820721575692));
#50615=CARTESIAN_POINT('Ctrl Pts',(4.24688783398681,4.23658275868477,3.1545983682309));
#50616=CARTESIAN_POINT('Ctrl Pts',(3.44595126436467,4.81034389605935,3.20098952070489));
#50617=CARTESIAN_POINT('Ctrl Pts',(2.64501469474253,5.38410503343392,3.24738067317887));
#50618=CARTESIAN_POINT('Ctrl Pts',(1.69766843317566,5.75348691113586,3.29377182565286));
#50619=CARTESIAN_POINT('Ctrl Pts',(0.719742160493715,5.87332612209818,3.34016297812684));
#50620=CARTESIAN_POINT('Ctrl Pts',(-0.258184112188229,5.9931653330605,3.38655413060082));
#50621=CARTESIAN_POINT('Ctrl Pts',(-1.26669039598524,5.8634618772832,3.43294528307481));
#50622=CARTESIAN_POINT('Ctrl Pts',(-2.18246912567144,5.50007427494718,3.47933643554879));
#50623=CARTESIAN_POINT('Ctrl Pts',(-3.09824785535763,5.13668667261115,3.52572758802278));
#50624=CARTESIAN_POINT('Ctrl Pts',(-3.92129903093301,4.5396149237164,3.57211874049676));
#50625=CARTESIAN_POINT('Ctrl Pts',(-4.55099022386481,3.78186151208579,3.61850989297074));
#50626=CARTESIAN_POINT('Ctrl Pts',(-5.1806814167966,3.02410810045518,3.66490104544473));
#50627=CARTESIAN_POINT('Ctrl Pts',(-5.61701262708482,2.10567302608871,3.71129219791871));
#50628=CARTESIAN_POINT('Ctrl Pts',(-5.80663471844869,1.1388510705313,3.7576833503927));
#50629=CARTESIAN_POINT('Ctrl Pts',(-5.88012927806763,0.764125987907549,
3.77566383619352));
#50630=CARTESIAN_POINT('Ctrl Pts',(-5.91656278747803,0.382132148291471,
3.79364432199434));
#50631=CARTESIAN_POINT('Ctrl Pts',(-5.9163416407139,9.66719635090206E-5,
3.81162480779517));
#50632=CARTESIAN_POINT('Origin',(0.,0.,0.));
#50633=CARTESIAN_POINT('',(-5.91715997915649,-8.5820353065702E-5,5.8133751922049));
#50634=CARTESIAN_POINT('',(-5.91724023967068,-3.97281055962929E-5,5.56162480779517));
#50635=CARTESIAN_POINT('',(-5.91675,-7.2459289488551E-16,0.));
#50636=CARTESIAN_POINT('Ctrl Pts',(-5.91715997915649,-8.5820353065702E-5,
5.8133751922049));
#50637=CARTESIAN_POINT('Ctrl Pts',(-5.91652656950878,0.899403380088141,
5.77102390820393));
#50638=CARTESIAN_POINT('Ctrl Pts',(-5.70841092001078,1.79917564355866,5.72867262420298));
#50639=CARTESIAN_POINT('Ctrl Pts',(-5.31219160137594,2.60664704332045,5.68632134020201));
#50640=CARTESIAN_POINT('Ctrl Pts',(-4.87817711379845,3.49114274890233,5.63993018772803));
#50641=CARTESIAN_POINT('Ctrl Pts',(-4.21846113592855,4.26488866108608,5.59353903525404));
#50642=CARTESIAN_POINT('Ctrl Pts',(-3.41370550625442,4.83328078376878,5.54714788278006));
#50643=CARTESIAN_POINT('Ctrl Pts',(-2.60894987658029,5.40167290645147,5.50075673030607));
#50644=CARTESIAN_POINT('Ctrl Pts',(-1.65915459510192,5.76471123963312,5.45436557783209));
#50645=CARTESIAN_POINT('Ctrl Pts',(-0.680448778229052,5.87800798556678,
5.40797442535811));
#50646=CARTESIAN_POINT('Ctrl Pts',(0.298257038643818,5.99130473150045,5.36158327288412));
#50647=CARTESIAN_POINT('Ctrl Pts',(1.30587339091119,5.85485989018613,5.31519212041014));
#50648=CARTESIAN_POINT('Ctrl Pts',(2.21920152306157,5.4853562343955,5.26880096793615));
#50649=CARTESIAN_POINT('Ctrl Pts',(3.13252965521195,5.11585257860486,5.22240981546217));
#50650=CARTESIAN_POINT('Ctrl Pts',(3.95156956724534,4.5132901083379,5.17601866298818));
#50651=CARTESIAN_POINT('Ctrl Pts',(4.5761792778911,3.75134264427823,5.1296275105142));
#50652=CARTESIAN_POINT('Ctrl Pts',(5.20078898853687,2.98939518021855,5.08323635804022));
#50653=CARTESIAN_POINT('Ctrl Pts',(5.630968497795,2.06806272236615,5.03684520556623));
#50654=CARTESIAN_POINT('Ctrl Pts',(5.81412082262937,1.09999430818887,4.99045405309225));
#50655=CARTESIAN_POINT('Ctrl Pts',(5.99727314746373,0.131925894011578,4.94406290061826));
#50656=CARTESIAN_POINT('Ctrl Pts',(5.93339828787432,-0.882878476490609,
4.89767174814428));
#50657=CARTESIAN_POINT('Ctrl Pts',(5.63030606472418,-1.82034118662145,4.85128059567029));
#50658=CARTESIAN_POINT('Ctrl Pts',(5.32721384157405,-2.75780389675229,4.80488944319631));
#50659=CARTESIAN_POINT('Ctrl Pts',(4.78490425486322,-3.61792494651176,4.75849829072233));
#50660=CARTESIAN_POINT('Ctrl Pts',(4.06968415445011,-4.29553946567809,4.71210713824835));
#50661=CARTESIAN_POINT('Ctrl Pts',(3.354464054037,-4.97315398484442,4.66571598577436));
#50662=CARTESIAN_POINT('Ctrl Pts',(2.4663334399216,-5.46826197341759,4.61932483330037));
#50663=CARTESIAN_POINT('Ctrl Pts',(1.51388184237951,-5.72032780402434,4.57293368082639));
#50664=CARTESIAN_POINT('Ctrl Pts',(0.561430244837424,-5.9723936346311,4.5265425283524));
#50665=CARTESIAN_POINT('Ctrl Pts',(-0.455342336131384,-5.98141730727146,
4.48015137587842));
#50666=CARTESIAN_POINT('Ctrl Pts',(-1.41211763561221,-5.74629551984348,
4.43376022340444));
#50667=CARTESIAN_POINT('Ctrl Pts',(-2.36889293509303,-5.5111737324155,4.38736907093045));
#50668=CARTESIAN_POINT('Ctrl Pts',(-3.26567095308587,-5.03190648491918,
4.34097791845647));
#50669=CARTESIAN_POINT('Ctrl Pts',(-3.99280486266284,-4.36709259655396,
4.29458676598249));
#50670=CARTESIAN_POINT('Ctrl Pts',(-4.7199387722398,-3.70227870818874,4.2481956135085));
#50671=CARTESIAN_POINT('Ctrl Pts',(-5.27742857340089,-2.85191817895462,
4.20180446103452));
#50672=CARTESIAN_POINT('Ctrl Pts',(-5.59711136906842,-1.91998248440585,
4.15541330856053));
#50673=CARTESIAN_POINT('Ctrl Pts',(-5.80852382435676,-1.30367526979957,
4.12473393644199));
#50674=CARTESIAN_POINT('Ctrl Pts',(-5.91593294715633,-0.651691692239068,
4.09405456432344));
#50675=CARTESIAN_POINT('Ctrl Pts',(-5.91644339103703,0.000127799667652695,
4.0633751922049));
#50676=CARTESIAN_POINT('Ctrl Pts',(-5.9163416407139,9.66719635090206E-5,
3.81162480779517));
#50677=CARTESIAN_POINT('Ctrl Pts',(-5.91599221038866,-0.603551232520732,
3.84003547446833));
#50678=CARTESIAN_POINT('Ctrl Pts',(-5.82412843901308,-1.20730308986252,
3.86844614114149));
#50679=CARTESIAN_POINT('Ctrl Pts',(-5.64235352522039,-1.78264836992076,
3.89685680781465));
#50680=CARTESIAN_POINT('Ctrl Pts',(-5.34553726818872,-2.72211701806704,
3.94324796028863));
#50681=CARTESIAN_POINT('Ctrl Pts',(-4.80899178168586,-3.58584547761124,
3.98963911276262));
#50682=CARTESIAN_POINT('Ctrl Pts',(-4.09831915331625,-4.26822780927827,
4.0360302652366));
#50683=CARTESIAN_POINT('Ctrl Pts',(-3.38764652494664,-4.95061014094529,
4.08242141771058));
#50684=CARTESIAN_POINT('Ctrl Pts',(-2.50284675471028,-5.45164634473513,
4.12881257018457));
#50685=CARTESIAN_POINT('Ctrl Pts',(-1.55210211885185,-5.71007596508149,
4.17520372265855));
#50686=CARTESIAN_POINT('Ctrl Pts',(-0.601357482993406,-5.96850558542785,
4.22159487513254));
#50687=CARTESIAN_POINT('Ctrl Pts',(0.415332018487122,-5.98432862233073,
4.26798602760652));
#50688=CARTESIAN_POINT('Ctrl Pts',(1.3736582785981,-5.75561043226334,4.31437718008051));
#50689=CARTESIAN_POINT('Ctrl Pts',(2.33198453870906,-5.52689224219595,4.36076833255449));
#50690=CARTESIAN_POINT('Ctrl Pts',(3.23194755745048,-5.0536328251583,4.40715948502848));
#50691=CARTESIAN_POINT('Ctrl Pts',(3.9635110857423,-4.39369643780044,4.45355063750246));
#50692=CARTESIAN_POINT('Ctrl Pts',(4.69507461403412,-3.73376005044257,4.49994178997644));
#50693=CARTESIAN_POINT('Ctrl Pts',(5.25823865187635,-2.88714669276451,4.54633294245043));
#50694=CARTESIAN_POINT('Ctrl Pts',(5.58414652732743,-1.95736968293639,4.59272409492441));
#50695=CARTESIAN_POINT('Ctrl Pts',(5.9100544027785,-1.02759267310829,4.63911524739839));
#50696=CARTESIAN_POINT('Ctrl Pts',(5.99870611583842,-0.0146520111301307,
4.68550639987238));
#50697=CARTESIAN_POINT('Ctrl Pts',(5.83926244114294,0.957602557326817,4.73189755234636));
#50698=CARTESIAN_POINT('Ctrl Pts',(5.67981876644747,1.92985712578377,4.77828870482035));
#50699=CARTESIAN_POINT('Ctrl Pts',(5.27227970399659,2.86142560071952,4.82467985729433));
#50700=CARTESIAN_POINT('Ctrl Pts',(4.66647404547604,3.63840741221214,4.87107100976832));
#50701=CARTESIAN_POINT('Ctrl Pts',(4.06066838695548,4.41538922370475,4.9174621622423));
#50702=CARTESIAN_POINT('Ctrl Pts',(3.25659613236525,5.03778437175423,4.96385331471628));
#50703=CARTESIAN_POINT('Ctrl Pts',(2.35256920457551,5.42949414329037,5.01024446719026));
#50704=CARTESIAN_POINT('Ctrl Pts',(1.44854227678578,5.82120391482652,5.05663561966425));
#50705=CARTESIAN_POINT('Ctrl Pts',(0.444560675796532,5.98222830984934,5.10302677213823));
#50706=CARTESIAN_POINT('Ctrl Pts',(-0.536621254916168,5.8928792744391,5.14941792461222));
#50707=CARTESIAN_POINT('Ctrl Pts',(-1.51780318562888,5.80353023902886,5.1958090770862));
#50708=CARTESIAN_POINT('Ctrl Pts',(-2.47618544606504,5.46380777318558,5.24220022956019));
#50709=CARTESIAN_POINT('Ctrl Pts',(-3.29458901116783,4.91524890131046,5.28859138203417));
#50710=CARTESIAN_POINT('Ctrl Pts',(-4.11299257627063,4.36669002943535,5.33498253450816));
#50711=CARTESIAN_POINT('Ctrl Pts',(-4.79141744604006,3.6092947515284,5.38137368698214));
#50712=CARTESIAN_POINT('Ctrl Pts',(-5.24691429211759,2.73566791214026,5.42776483945613));
#50713=CARTESIAN_POINT('Ctrl Pts',(-5.6850207710679,1.89539518178708,5.47238482890248));
#50714=CARTESIAN_POINT('Ctrl Pts',(-5.91689657222713,0.947596653160506,
5.51700481834882));
#50715=CARTESIAN_POINT('Ctrl Pts',(-5.91724023967068,-3.97281055962929E-5,
5.56162480779517));
#50716=CARTESIAN_POINT('Origin',(0.,0.,0.));
#50717=CARTESIAN_POINT('',(-5.9162413557982,1.18844204999302E-5,7.5633751922049));
#50718=CARTESIAN_POINT('',(-5.9162507091618,-3.31417769469161E-5,7.31162480779517));
#50719=CARTESIAN_POINT('',(-5.91675,-7.2459289488551E-16,0.));
#50720=CARTESIAN_POINT('Ctrl Pts',(-5.9162413557982,1.18844204999302E-5,
7.5633751922049));
#50721=CARTESIAN_POINT('Ctrl Pts',(-5.91627481843442,0.480214766201657,
7.5407755570324));
#50722=CARTESIAN_POINT('Ctrl Pts',(-5.8584953203415,0.960409734025278,7.51817592185989));
#50723=CARTESIAN_POINT('Ctrl Pts',(-5.74281060135014,1.42622397091085,7.49557628668739));
#50724=CARTESIAN_POINT('Ctrl Pts',(-5.5053400671281,2.38241902109478,7.4491851342134));
#50725=CARTESIAN_POINT('Ctrl Pts',(-5.02387213814794,3.27801744753458,7.40279398173942));
#50726=CARTESIAN_POINT('Ctrl Pts',(-4.35727470548306,4.00351664903967,7.35640282926544));
#50727=CARTESIAN_POINT('Ctrl Pts',(-3.69067727281818,4.72901585054476,7.31001167679145));
#50728=CARTESIAN_POINT('Ctrl Pts',(-2.83895033646859,5.28441582711515,7.26362052431747));
#50729=CARTESIAN_POINT('Ctrl Pts',(-1.90623243920183,5.60180919934935,7.21722937184349));
#50730=CARTESIAN_POINT('Ctrl Pts',(-0.973514541935027,5.91920257158355,
7.1708382193695));
#50731=CARTESIAN_POINT('Ctrl Pts',(0.0401943162489465,5.99858933948154,
7.12444706689551));
#50732=CARTESIAN_POINT('Ctrl Pts',(1.01095046423141,5.83026307957459,7.07805591442153));
#50733=CARTESIAN_POINT('Ctrl Pts',(1.98170661221383,5.66193681966765,7.03166476194754));
#50734=CARTESIAN_POINT('Ctrl Pts',(2.90951004999477,5.24589753195577,6.98527360947356));
#50735=CARTESIAN_POINT('Ctrl Pts',(3.68092054941919,4.6330133096122,6.93888245699958));
#50736=CARTESIAN_POINT('Ctrl Pts',(4.45233104884364,4.02012908726862,6.89249130452559));
#50737=CARTESIAN_POINT('Ctrl Pts',(5.06734860991157,3.21039993029335,6.84610015205162));
#50738=CARTESIAN_POINT('Ctrl Pts',(5.45077655883864,2.30282941699889,6.79970899957763));
#50739=CARTESIAN_POINT('Ctrl Pts',(5.83420450776571,1.39525890370445,6.75331784710365));
#50740=CARTESIAN_POINT('Ctrl Pts',(5.98604284455189,0.389847034090864,6.70692669462966));
#50741=CARTESIAN_POINT('Ctrl Pts',(5.88772667186408,-0.590476972963932,
6.66053554215567));
#50742=CARTESIAN_POINT('Ctrl Pts',(5.78941049917627,-1.57080098001873,6.61414438968169));
#50743=CARTESIAN_POINT('Ctrl Pts',(5.44093981701448,-2.52603712451473,6.56775323720771));
#50744=CARTESIAN_POINT('Ctrl Pts',(4.88492127251973,-3.33939104919812,6.52136208473372));
#50745=CARTESIAN_POINT('Ctrl Pts',(4.32890272802498,-4.15274497388151,6.47497093225974));
#50746=CARTESIAN_POINT('Ctrl Pts',(3.56533632119724,-4.82421667875231,6.42857977978575));
#50747=CARTESIAN_POINT('Ctrl Pts',(2.68758142523437,-5.27170698170104,6.38218862731177));
#50748=CARTESIAN_POINT('Ctrl Pts',(1.80982652927149,-5.71919728464978,6.33579747483778));
#50749=CARTESIAN_POINT('Ctrl Pts',(0.81788314417347,-5.94270618567646,6.2894063223638));
#50750=CARTESIAN_POINT('Ctrl Pts',(-0.166966269421853,-5.91490580508732,
6.24301516988982));
#50751=CARTESIAN_POINT('Ctrl Pts',(-1.15181568301718,-5.88710542449819,
6.19662401741583));
#50752=CARTESIAN_POINT('Ctrl Pts',(-2.12957112510979,-5.60799576229324,
6.15023286494185));
#50753=CARTESIAN_POINT('Ctrl Pts',(-2.98068485970938,-5.11170286551161,
6.10384171246786));
#50754=CARTESIAN_POINT('Ctrl Pts',(-3.83179859430896,-4.61540996872999,
6.05745055999388));
#50755=CARTESIAN_POINT('Ctrl Pts',(-4.55627062141552,-3.90193383737169,
6.0110594075199));
#50756=CARTESIAN_POINT('Ctrl Pts',(-5.06552154080239,-3.05850943072722,
5.96466825504591));
#50757=CARTESIAN_POINT('Ctrl Pts',(-5.57477246018926,-2.21508502408275,
5.91827710257193));
#50758=CARTESIAN_POINT('Ctrl Pts',(-5.86880227185644,-1.24171234215211,
5.87188595009794));
#50759=CARTESIAN_POINT('Ctrl Pts',(-5.91166067904749,-0.257403251696779,
5.82549479762396));
#50760=CARTESIAN_POINT('Ctrl Pts',(-5.91539290639649,-0.171686923255304,
5.82145492915094));
#50761=CARTESIAN_POINT('Ctrl Pts',(-5.91722039979607,-0.085887659622042,
5.81741506067792));
#50762=CARTESIAN_POINT('Ctrl Pts',(-5.91715997915649,-8.5820353065702E-5,
5.8133751922049));
#50763=CARTESIAN_POINT('Ctrl Pts',(-5.91724023967068,-3.97281055962929E-5,
5.56162480779517));
#50764=CARTESIAN_POINT('Ctrl Pts',(-5.9172538813384,-0.0376555712056591,
5.56339597082281));
#50765=CARTESIAN_POINT('Ctrl Pts',(-5.9169027107474,-0.0752711588191768,
5.56516713385044));
#50766=CARTESIAN_POINT('Ctrl Pts',(-5.9161851454377,-0.112879755686916,
5.56693829687808));
#50767=CARTESIAN_POINT('Ctrl Pts',(-5.89739033029467,-1.09794218325665,
5.61332944935206));
#50768=CARTESIAN_POINT('Ctrl Pts',(-5.62723187762299,-2.07820863752684,
5.65972060182604));
#50769=CARTESIAN_POINT('Ctrl Pts',(-5.13874139224443,-2.93382436726798,
5.70611175430003));
#50770=CARTESIAN_POINT('Ctrl Pts',(-4.65025090686588,-3.78944009700913,
5.75250290677401));
#50771=CARTESIAN_POINT('Ctrl Pts',(-3.94342838878045,-4.52040510222124,
5.798894059248));
#50772=CARTESIAN_POINT('Ctrl Pts',(-3.10469527646488,-5.03734610232792,
5.84528521172198));
#50773=CARTESIAN_POINT('Ctrl Pts',(-2.26596216414931,-5.55428710243459,
5.89167636419597));
#50774=CARTESIAN_POINT('Ctrl Pts',(-1.2953184576036,-5.85720409743582,5.93806751666994));
#50775=CARTESIAN_POINT('Ctrl Pts',(-0.311442358528609,-5.90906017668256,
5.98445866914393));
#50776=CARTESIAN_POINT('Ctrl Pts',(0.672433740546371,-5.96091625592931,
6.03084982161791));
#50777=CARTESIAN_POINT('Ctrl Pts',(1.66954223215063,-5.76171141942157,6.0772409740919));
#50778=CARTESIAN_POINT('Ctrl Pts',(2.55796913086782,-5.3358019490859,6.12363212656589));
#50779=CARTESIAN_POINT('Ctrl Pts',(3.44639602958501,-4.90989247875023,6.17002327903987));
#50780=CARTESIAN_POINT('Ctrl Pts',(4.22614133541513,-4.25727837458664,6.21641443151385));
#50781=CARTESIAN_POINT('Ctrl Pts',(4.80186752125472,-3.45775314657664,6.26280558398784));
#50782=CARTESIAN_POINT('Ctrl Pts',(5.37759370709432,-2.65822791856663,6.30919673646182));
#50783=CARTESIAN_POINT('Ctrl Pts',(5.74930077294337,-1.71179156671023,6.35558788893581));
#50784=CARTESIAN_POINT('Ctrl Pts',(5.87154101658429,-0.734162519412394,
6.40197904140979));
#50785=CARTESIAN_POINT('Ctrl Pts',(5.99378126022521,0.243466527885433,6.44837019388378));
#50786=CARTESIAN_POINT('Ctrl Pts',(5.86655468165799,1.25228827062469,6.49476134635776));
#50787=CARTESIAN_POINT('Ctrl Pts',(5.50541695950198,2.16895657318664,6.54115249883174));
#50788=CARTESIAN_POINT('Ctrl Pts',(5.14427923734597,3.08562487574861,6.58754365130572));
#50789=CARTESIAN_POINT('Ctrl Pts',(4.54923037160118,3.91013973813327,6.63393480377971));
#50790=CARTESIAN_POINT('Ctrl Pts',(3.79302551313757,4.54168977045208,6.6803259562537));
#50791=CARTESIAN_POINT('Ctrl Pts',(3.03682065467397,5.17323980277089,6.72671710872768));
#50792=CARTESIAN_POINT('Ctrl Pts',(2.11945980349156,5.61182500502386,6.77310826120166));
#50793=CARTESIAN_POINT('Ctrl Pts',(1.15310639854836,5.80382065091337,6.81949941367564));
#50794=CARTESIAN_POINT('Ctrl Pts',(0.186752993605153,5.99581629680288,6.86589056614963));
#50795=CARTESIAN_POINT('Ctrl Pts',(-0.82859296509884,5.94122238632894,6.91228171862361));
#50796=CARTESIAN_POINT('Ctrl Pts',(-1.76878764221949,5.6467139816953,6.9586728710976));
#50797=CARTESIAN_POINT('Ctrl Pts',(-2.70898231934014,5.35220557706166,7.00506402357158));
#50798=CARTESIAN_POINT('Ctrl Pts',(-3.57402571487744,4.81778267826832,7.05145517604557));
#50799=CARTESIAN_POINT('Ctrl Pts',(-4.25815111558402,4.10878784937751,7.09784632851955));
#50800=CARTESIAN_POINT('Ctrl Pts',(-4.94227651629061,3.39979302048667,7.14423748099354));
#50801=CARTESIAN_POINT('Ctrl Pts',(-5.44548392216648,2.51622626149834,7.19062863346752));
#50802=CARTESIAN_POINT('Ctrl Pts',(-5.70624741014717,1.56611909142644,7.23701978594151));
#50803=CARTESIAN_POINT('Ctrl Pts',(-5.84603172017157,1.05680670169657,7.2618881265594));
#50804=CARTESIAN_POINT('Ctrl Pts',(-5.9161478310269,0.528373392570541,7.28675646717728));
#50805=CARTESIAN_POINT('Ctrl Pts',(-5.9162507091618,-3.31417769469161E-5,
7.31162480779517));
#50806=CARTESIAN_POINT('Origin',(0.,0.,0.));
#50807=CARTESIAN_POINT('',(-5.9172084520385,6.25597485048868E-5,9.3133751922049));
#50808=CARTESIAN_POINT('',(-5.91710638445669,0.000104510447198684,9.06162480779517));
#50809=CARTESIAN_POINT('',(-5.91675,-7.2459289488551E-16,0.));
#50810=CARTESIAN_POINT('Ctrl Pts',(-5.9172084520385,6.25597485048868E-5,
9.3133751922049));
#50811=CARTESIAN_POINT('Ctrl Pts',(-5.91724119307767,0.0605488496737315,
9.31052720586085));
#50812=CARTESIAN_POINT('Ctrl Pts',(-5.91633311693352,0.121034154618972,
9.30767921951681));
#50813=CARTESIAN_POINT('Ctrl Pts',(-5.91447796966348,0.181490397943491,
9.30483123317277));
#50814=CARTESIAN_POINT('Ctrl Pts',(-5.88425927846571,1.16626857566792,9.25844008069878));
#50815=CARTESIAN_POINT('Ctrl Pts',(-5.60274948328953,2.14333568866362,9.2120489282248));
#50816=CARTESIAN_POINT('Ctrl Pts',(-5.10436808948731,2.99322816123395,9.16565777575082));
#50817=CARTESIAN_POINT('Ctrl Pts',(-4.60598669568509,3.84312063380428,9.11926662327683));
#50818=CARTESIAN_POINT('Ctrl Pts',(-3.89073370325683,4.56583846594923,9.07287547080284));
#50819=CARTESIAN_POINT('Ctrl Pts',(-3.04606132389475,5.07301673851495,9.02648431832886));
#50820=CARTESIAN_POINT('Ctrl Pts',(-2.20138894453265,5.58019501108068,8.98009316585487));
#50821=CARTESIAN_POINT('Ctrl Pts',(-1.22729717823674,5.87183372406716,8.9337020133809));
#50822=CARTESIAN_POINT('Ctrl Pts',(-0.242885812432634,5.91227493443085,
8.88731086090691));
#50823=CARTESIAN_POINT('Ctrl Pts',(0.74152555337144,5.95271614479453,8.84091970843293));
#50824=CARTESIAN_POINT('Ctrl Pts',(1.7362565186837,5.74195985253542,8.79452855595894));
#50825=CARTESIAN_POINT('Ctrl Pts',(2.61968379233836,5.30577470746167,8.74813740348495));
#50826=CARTESIAN_POINT('Ctrl Pts',(3.50311106599304,4.86958956238792,8.70174625101097));
#50827=CARTESIAN_POINT('Ctrl Pts',(4.27523464799013,4.20797556449952,8.655355098537));
#50828=CARTESIAN_POINT('Ctrl Pts',(4.84164890052009,3.40182661849086,8.60896394606301));
#50829=CARTESIAN_POINT('Ctrl Pts',(5.40806315305005,2.5956776724822,8.56257279358903));
#50830=CARTESIAN_POINT('Ctrl Pts',(5.76876807611289,1.64499377835328,8.51618164111504));
#50831=CARTESIAN_POINT('Ctrl Pts',(5.87966117223702,0.666012700981533,8.46979048864105));
#50832=CARTESIAN_POINT('Ctrl Pts',(5.99055426836114,-0.312968376390219,
8.42339933616706));
#50833=CARTESIAN_POINT('Ctrl Pts',(5.85163553754656,-1.32024663700481,8.37700818369309));
#50834=CARTESIAN_POINT('Ctrl Pts',(5.47989022890625,-2.23266466297967,8.3306170312191));
#50835=CARTESIAN_POINT('Ctrl Pts',(5.10814492026594,-3.14508268895454,8.28422587874512));
#50836=CARTESIAN_POINT('Ctrl Pts',(4.50357303379992,-3.96264048028968,8.23783472627113));
#50837=CARTESIAN_POINT('Ctrl Pts',(3.74009407653309,-4.58537727094101,8.19144357379715));
#50838=CARTESIAN_POINT('Ctrl Pts',(2.97661511926626,-5.20811406159233,8.14505242132316));
#50839=CARTESIAN_POINT('Ctrl Pts',(2.05422909119864,-5.63602985155983,8.09866126884918));
#50840=CARTESIAN_POINT('Ctrl Pts',(1.08571384721853,-5.81680443715776,8.0522701163752));
#50841=CARTESIAN_POINT('Ctrl Pts',(0.117198603238411,-5.9975790227557,8.00587896390121));
#50842=CARTESIAN_POINT('Ctrl Pts',(-0.897445856654189,-5.93121240398407,
7.95948781142723));
#50843=CARTESIAN_POINT('Ctrl Pts',(-1.83416146763716,-5.62581906292901,
7.91309665895325));
#50844=CARTESIAN_POINT('Ctrl Pts',(-2.77087707862012,-5.32042572187395,
7.86670550647926));
#50845=CARTESIAN_POINT('Ctrl Pts',(-3.62966384069345,-4.77600565853546,
7.82031435400528));
#50846=CARTESIAN_POINT('Ctrl Pts',(-4.30552002368566,-4.05912376552159,
7.77392320153129));
#50847=CARTESIAN_POINT('Ctrl Pts',(-4.98137620667786,-3.34224187250773,
7.72753204905731));
#50848=CARTESIAN_POINT('Ctrl Pts',(-5.47430181058894,-2.45289814981848,
7.68114089658332));
#50849=CARTESIAN_POINT('Ctrl Pts',(-5.72402804281252,-1.49983045150984,
7.63474974410934));
#50850=CARTESIAN_POINT('Ctrl Pts',(-5.852099143825,-1.01105348813285,7.61095822680786));
#50851=CARTESIAN_POINT('Ctrl Pts',(-5.91620612837604,-0.505516416497265,
7.58716670950638));
#50852=CARTESIAN_POINT('Ctrl Pts',(-5.9162413557982,1.18844204999302E-5,
7.5633751922049));
#50853=CARTESIAN_POINT('Ctrl Pts',(-5.9162507091618,-3.31417769469161E-5,
7.31162480779517));
#50854=CARTESIAN_POINT('Ctrl Pts',(-5.91633974713885,-0.457353338449392,
7.33314761965127));
#50855=CARTESIAN_POINT('Ctrl Pts',(-5.86398614648453,-0.914653479769718,
7.35467043150736));
#50856=CARTESIAN_POINT('Ctrl Pts',(-5.75896623194724,-1.35952067054277,
7.37619324336345));
#50857=CARTESIAN_POINT('Ctrl Pts',(-5.53260199568109,-2.31840568128467,
7.42258439583744));
#50858=CARTESIAN_POINT('Ctrl Pts',(-5.06155395306328,-3.21952812161301,
7.46897554831142));
#50859=CARTESIAN_POINT('Ctrl Pts',(-4.40341598147186,-3.95270998284213,
7.51536670078541));
#50860=CARTESIAN_POINT('Ctrl Pts',(-3.74527800988045,-4.68589184407125,
7.56175785325939));
#50861=CARTESIAN_POINT('Ctrl Pts',(-2.90005010931545,-5.25113312620114,
7.60814900573337));
#50862=CARTESIAN_POINT('Ctrl Pts',(-1.97107620153722,-5.57932317777661,
7.65454015820736));
#50863=CARTESIAN_POINT('Ctrl Pts',(-1.042102293759,-5.90751322935207,7.70093131068134));
#50864=CARTESIAN_POINT('Ctrl Pts',(-0.0293823787675436,-5.9986520503731,
7.74732246315532));
#50865=CARTESIAN_POINT('Ctrl Pts',(0.943260787952951,-5.84159632294564,
7.79371361562931));
#50866=CARTESIAN_POINT('Ctrl Pts',(1.91590395467344,-5.68454059551817,7.84010476810329));
#50867=CARTESIAN_POINT('Ctrl Pts',(2.84847037312298,-5.27929031964222,7.88649592057728));
#50868=CARTESIAN_POINT('Ctrl Pts',(3.62693745729823,-4.67539444273835,7.93288707305126));
#50869=CARTESIAN_POINT('Ctrl Pts',(4.4054045414735,-4.07149856583446,7.97927822552525));
#50870=CARTESIAN_POINT('Ctrl Pts',(5.02977229137448,-3.26895708790266,8.02566937799923));
#50871=CARTESIAN_POINT('Ctrl Pts',(5.4237008087887,-2.36589476754282,8.07206053047321));
#50872=CARTESIAN_POINT('Ctrl Pts',(5.81762932620292,-1.46283244718296,8.1184516829472));
#50873=CARTESIAN_POINT('Ctrl Pts',(5.98111861113038,-0.45924928439506,8.16484283542118));
#50874=CARTESIAN_POINT('Ctrl Pts',(5.89417923366829,0.522149093396754,8.21123398789517));
#50875=CARTESIAN_POINT('Ctrl Pts',(5.80723985620622,1.50354747118852,8.25762514036915));
#50876=CARTESIAN_POINT('Ctrl Pts',(5.46987181635464,2.46276106398421,8.30401629284313));
#50877=CARTESIAN_POINT('Ctrl Pts',(4.9233242686807,3.28250920177862,8.35040744531711));
#50878=CARTESIAN_POINT('Ctrl Pts',(4.37677672100673,4.10225733957307,8.3967985977911));
#50879=CARTESIAN_POINT('Ctrl Pts',(3.62104966551037,4.78254002236623,8.44318975026509));
#50880=CARTESIAN_POINT('Ctrl Pts',(2.74854397732036,5.24018077160298,8.48958090273907));
#50881=CARTESIAN_POINT('Ctrl Pts',(1.87603828913037,5.69782152083972,8.53597205521306));
#50882=CARTESIAN_POINT('Ctrl Pts',(0.886753968246731,5.93282033652007,8.58236320768704));
#50883=CARTESIAN_POINT('Ctrl Pts',(-0.0983516418876641,5.91644449554626,
8.62875436016102));
#50884=CARTESIAN_POINT('Ctrl Pts',(-1.08345725202206,5.90006865457244,8.67514551263501));
#50885=CARTESIAN_POINT('Ctrl Pts',(-2.0643841514072,5.63231815694446,8.72153666510899));
#50886=CARTESIAN_POINT('Ctrl Pts',(-2.92119683782535,5.14593019278544,8.76792781758298));
#50887=CARTESIAN_POINT('Ctrl Pts',(-3.7780095242435,4.65954222862642,8.81431897005696));
#50888=CARTESIAN_POINT('Ctrl Pts',(-4.51070799769467,3.95451679793635,8.86071012253094));
#50889=CARTESIAN_POINT('Ctrl Pts',(-5.02970703073467,3.11705561376756,8.90710127500493));
#50890=CARTESIAN_POINT('Ctrl Pts',(-5.54870606377467,2.27959442959876,8.95349242747891));
#50891=CARTESIAN_POINT('Ctrl Pts',(-5.8540056564035,1.30969749195124,8.9998835799529));
#50892=CARTESIAN_POINT('Ctrl Pts',(-5.90827758366193,0.325951696942433,
9.04627473242688));
#50893=CARTESIAN_POINT('Ctrl Pts',(-5.91426348204536,0.217449886494213,
9.05139142421631));
#50894=CARTESIAN_POINT('Ctrl Pts',(-5.91719565645419,0.108779606217447,
9.05650811600574));
#50895=CARTESIAN_POINT('Ctrl Pts',(-5.91710638445669,0.000104510447198684,
9.06162480779517));
#50896=CARTESIAN_POINT('Origin',(0.,0.,0.));
#50897=CARTESIAN_POINT('',(-5.91638614209071,-0.000112643280536506,11.0633751922049));
#50898=CARTESIAN_POINT('',(-5.91650151471712,-0.000138897455152014,10.8116248077952));
#50899=CARTESIAN_POINT('',(-5.91675,-7.2459289488551E-16,0.));
#50900=CARTESIAN_POINT('Ctrl Pts',(-5.91638614209071,-0.000112643280536506,
11.0633751922049));
#50901=CARTESIAN_POINT('Ctrl Pts',(-5.91595937575435,0.6264012739477,11.0338877022153));
#50902=CARTESIAN_POINT('Ctrl Pts',(-5.81687601168185,1.25304699970507,11.0044002122258));
#50903=CARTESIAN_POINT('Ctrl Pts',(-5.62129813760519,1.84797068871148,10.9749127222362));
#50904=CARTESIAN_POINT('Ctrl Pts',(-5.31360552015834,2.78393355217811,10.9285215697622));
#50905=CARTESIAN_POINT('Ctrl Pts',(-4.76707826302969,3.64138084810558,10.8821304172882));
#50906=CARTESIAN_POINT('Ctrl Pts',(-4.04853890019245,4.31547461953014,10.8357392648142));
#50907=CARTESIAN_POINT('Ctrl Pts',(-3.32999953735522,4.9895683909547,10.7893481123403));
#50908=CARTESIAN_POINT('Ctrl Pts',(-2.4394480688094,5.48030863787637,10.7429569598663));
#50909=CARTESIAN_POINT('Ctrl Pts',(-1.48577001670525,5.72769376587471,10.6965658073923));
#50910=CARTESIAN_POINT('Ctrl Pts',(-0.53209196460107,5.97507889387305,10.6501746549183));
#50911=CARTESIAN_POINT('Ctrl Pts',(0.484712671061443,5.97910890294806,10.6037835024443));
#50912=CARTESIAN_POINT('Ctrl Pts',(1.44032170611958,5.73929105387252,10.5573923499703));
#50913=CARTESIAN_POINT('Ctrl Pts',(2.39593074117771,5.49947320479697,10.5110011974964));
#50914=CARTESIAN_POINT('Ctrl Pts',(3.29034417563147,5.01580749757088,10.4646100450224));
#50915=CARTESIAN_POINT('Ctrl Pts',(4.01420429432519,4.34743054016985,10.4182188925484));
#50916=CARTESIAN_POINT('Ctrl Pts',(4.7380644130189,3.67905358276882,10.3718277400744));
#50917=CARTESIAN_POINT('Ctrl Pts',(5.29137121595257,2.82596537519285,10.3254365876004));
#50918=CARTESIAN_POINT('Ctrl Pts',(5.60647325088044,1.89247089947045,10.2790454351264));
#50919=CARTESIAN_POINT('Ctrl Pts',(5.92157528580831,0.958976423748022,10.2326542826525));
#50920=CARTESIAN_POINT('Ctrl Pts',(5.99847255273037,-0.0549243201208414,
10.1862631301785));
#50921=CARTESIAN_POINT('Ctrl Pts',(5.82776301329569,-1.02526419963007,10.1398719777045));
#50922=CARTESIAN_POINT('Ctrl Pts',(5.65705347386101,-1.99560407913926,10.0934808252305));
#50923=CARTESIAN_POINT('Ctrl Pts',(5.23873712806962,-2.92238309428882,10.0470896727565));
#50924=CARTESIAN_POINT('Ctrl Pts',(4.62396047934579,-3.69228627054141,10.0006985202825));
#50925=CARTESIAN_POINT('Ctrl Pts',(4.00918383062193,-4.46218944679403,9.95430736780855));
#50926=CARTESIAN_POINT('Ctrl Pts',(3.19794687896562,-5.07521678414965,9.90791621533456));
#50927=CARTESIAN_POINT('Ctrl Pts',(2.28943755701025,-5.45641494854737,9.86152506286057));
#50928=CARTESIAN_POINT('Ctrl Pts',(1.3809282350549,-5.83761311294508,9.81513391038659));
#50929=CARTESIAN_POINT('Ctrl Pts',(0.375146542800495,-5.9869821043849,9.76874275791261));
#50930=CARTESIAN_POINT('Ctrl Pts',(-0.604933083576789,-5.88625894627263,
9.72235160543862));
#50931=CARTESIAN_POINT('Ctrl Pts',(-1.58501270995407,-5.78553578816036,
9.67596045296464));
#50932=CARTESIAN_POINT('Ctrl Pts',(-2.53939027045424,-5.434720480496,9.62956930049065));
#50933=CARTESIAN_POINT('Ctrl Pts',(-3.35137638476191,-4.87670634197308,
9.58317814801667));
#50934=CARTESIAN_POINT('Ctrl Pts',(-4.16336249906959,-4.31869220345017,
9.53678699554269));
#50935=CARTESIAN_POINT('Ctrl Pts',(-4.83295716718478,-3.55347923406871,
9.4903958430687));
#50936=CARTESIAN_POINT('Ctrl Pts',(-5.2782907076327,-2.6746281281514,9.44400469059472));
#50937=CARTESIAN_POINT('Ctrl Pts',(-5.69628490050886,-1.84973032614273,
9.40046152446478));
#50938=CARTESIAN_POINT('Ctrl Pts',(-5.91670787080818,-0.924718760325417,
9.35691835833484));
#50939=CARTESIAN_POINT('Ctrl Pts',(-5.9172084520385,6.25597485048868E-5,
9.3133751922049));
#50940=CARTESIAN_POINT('Ctrl Pts',(-5.91710638445669,0.000104510447198684,
9.06162480779517));
#50941=CARTESIAN_POINT('Ctrl Pts',(-5.9163862602626,-0.876537302731103,
9.10289926847972));
#50942=CARTESIAN_POINT('Ctrl Pts',(-5.71905903720832,-1.75349246259044,
9.14417372916428));
#50943=CARTESIAN_POINT('Ctrl Pts',(-5.34206720605816,-2.54485883307889,
9.18544818984883));
#50944=CARTESIAN_POINT('Ctrl Pts',(-4.91834063930793,-3.43432891572131,
9.23183934232282));
#50945=CARTESIAN_POINT('Ctrl Pts',(-4.26764324391943,-4.2156744286361,9.27823049479681));
#50946=CARTESIAN_POINT('Ctrl Pts',(-3.46953417864001,-4.79336219136322,
9.32462164727079));
#50947=CARTESIAN_POINT('Ctrl Pts',(-2.6714251133606,-5.37104995409033,9.37101279974477));
#50948=CARTESIAN_POINT('Ctrl Pts',(-1.72590437819026,-5.74507996662981,
9.41740395221876));
#50949=CARTESIAN_POINT('Ctrl Pts',(-0.748578451349749,-5.86972050582619,
9.46379510469274));
#50950=CARTESIAN_POINT('Ctrl Pts',(0.228747475490778,-5.99436104502257,
9.51018625716672));
#50951=CARTESIAN_POINT('Ctrl Pts',(1.23787859400146,-5.86961211087585,9.55657740964071));
#50952=CARTESIAN_POINT('Ctrl Pts',(2.15543094195436,-5.51072644655923,9.60296856211469));
#50953=CARTESIAN_POINT('Ctrl Pts',(3.07298328990726,-5.15184078224262,9.64935971458867));
#50954=CARTESIAN_POINT('Ctrl Pts',(3.89895686730239,-4.55881838775608,9.69575086706266));
#50955=CARTESIAN_POINT('Ctrl Pts',(4.53236193078007,-3.80416664234851,9.74214201953664));
#50956=CARTESIAN_POINT('Ctrl Pts',(5.16576699425776,-3.04951489694093,9.78853317201063));
#50957=CARTESIAN_POINT('Ctrl Pts',(5.60660354381802,-2.13323380061229,9.83492432448461));
#50958=CARTESIAN_POINT('Ctrl Pts',(5.80097158650461,-1.1673547733692,9.8813154769586));
#50959=CARTESIAN_POINT('Ctrl Pts',(5.99533962919119,-0.201475746126127,
9.92770662943258));
#50960=CARTESIAN_POINT('Ctrl Pts',(5.94323916500412,0.814001212031379,9.97409778190656));
#50961=CARTESIAN_POINT('Ctrl Pts',(5.65104038864595,1.75491624878051,10.0204889343805));
#50962=CARTESIAN_POINT('Ctrl Pts',(5.35884161228778,2.69583128552964,10.0668800868545));
#50963=CARTESIAN_POINT('Ctrl Pts',(4.82654452375848,3.56218440087041,10.1132712393285));
#50964=CARTESIAN_POINT('Ctrl Pts',(4.119231769565,4.24804874535922,10.1596623918025));
#50965=CARTESIAN_POINT('Ctrl Pts',(3.41191901537151,4.93391308984804,10.2060535442765));
#50966=CARTESIAN_POINT('Ctrl Pts',(2.52959059551382,5.43928866348491,10.2524446967505));
#50967=CARTESIAN_POINT('Ctrl Pts',(1.58012662034769,5.70238444670387,10.2988358492245));
#50968=CARTESIAN_POINT('Ctrl Pts',(0.630662645181565,5.96548022992282,10.3452270016984));
#50969=CARTESIAN_POINT('Ctrl Pts',(-0.38593688529298,5.98629622272385,10.3916181541724));
#50970=CARTESIAN_POINT('Ctrl Pts',(-1.34537486461655,5.76228730522868,10.4380093066464));
#50971=CARTESIAN_POINT('Ctrl Pts',(-2.30481284394012,5.53827838773352,10.4844004591204));
#50972=CARTESIAN_POINT('Ctrl Pts',(-3.20708927211268,5.06944455994216,10.5307916115944));
#50973=CARTESIAN_POINT('Ctrl Pts',(-3.94188504521335,4.41310897267051,10.5771827640684));
#50974=CARTESIAN_POINT('Ctrl Pts',(-4.67668081831403,3.75677338539885,10.6235739165423));
#50975=CARTESIAN_POINT('Ctrl Pts',(-5.2439959363428,2.91293603864686,10.6699650690163));
#50976=CARTESIAN_POINT('Ctrl Pts',(-5.574466185066,1.98477083460466,10.7163562214903));
#50977=CARTESIAN_POINT('Ctrl Pts',(-5.80068341064102,1.3494127104016,10.7481124169253));
#50978=CARTESIAN_POINT('Ctrl Pts',(-5.91591913630772,0.674539978541786,
10.7798686123602));
#50979=CARTESIAN_POINT('Ctrl Pts',(-5.91650151471712,-0.000138897455152014,
10.8116248077952));
#50980=CARTESIAN_POINT('Origin',(0.,0.,0.));
#50981=CARTESIAN_POINT('',(-5.91681535977711,0.000152256150380351,12.8133751922049));
#50982=CARTESIAN_POINT('',(-5.91666319015572,0.00015412212114384,12.5616248077952));
#50983=CARTESIAN_POINT('',(-5.91675,-7.2459289488551E-16,0.));
#50984=CARTESIAN_POINT('Ctrl Pts',(-5.91681535977711,0.00015225615038035,
12.8133751922049));
#50985=CARTESIAN_POINT('Ctrl Pts',(-5.91703012865227,0.206964346823776,
12.8036393510438));
#50986=CARTESIAN_POINT('Ctrl Pts',(-5.90639892222455,0.413754466608288,
12.7939035098827));
#50987=CARTESIAN_POINT('Ctrl Pts',(-5.88475572670746,0.619385546460389,
12.7841676687216));
#50988=CARTESIAN_POINT('Ctrl Pts',(-5.7816261905285,1.59921488230794,12.7377765162476));
#50989=CARTESIAN_POINT('Ctrl Pts',(-5.42846837276787,2.55272810394278,12.6913853637736));
#50990=CARTESIAN_POINT('Ctrl Pts',(-4.86846200502615,3.3633415116216,12.6449942112996));
#50991=CARTESIAN_POINT('Ctrl Pts',(-4.30845563728443,4.17395491930043,12.5986030588256));
#50992=CARTESIAN_POINT('Ctrl Pts',(-3.54160071956163,4.84166851302325,12.5522119063517));
#50993=CARTESIAN_POINT('Ctrl Pts',(-2.66165870313702,5.28484260562179,12.5058207538777));
#50994=CARTESIAN_POINT('Ctrl Pts',(-1.78171668671241,5.72801669822032,12.4594296014037));
#50995=CARTESIAN_POINT('Ctrl Pts',(-0.78868757158598,5.94665128969457,12.4130384489297));
#50996=CARTESIAN_POINT('Ctrl Pts',(0.196013432083201,5.91401447010601,12.3666472964557));
#50997=CARTESIAN_POINT('Ctrl Pts',(1.18071443575238,5.88137765051745,12.3202561439817));
#50998=CARTESIAN_POINT('Ctrl Pts',(2.15708732796432,5.59746941986609,12.2738649915078));
#50999=CARTESIAN_POINT('Ctrl Pts',(3.005753413678,5.09700253426888,12.2274738390338));
#51000=CARTESIAN_POINT('Ctrl Pts',(3.85441949939168,4.59653564867167,12.1810826865598));
#51001=CARTESIAN_POINT('Ctrl Pts',(4.5753787786071,3.87951010812861,12.1346915340858));
#51002=CARTESIAN_POINT('Ctrl Pts',(5.08048134608114,3.03359484939929,12.0883003816118));
#51003=CARTESIAN_POINT('Ctrl Pts',(5.58558391355517,2.18767959066998,12.0419092291378));
#51004=CARTESIAN_POINT('Ctrl Pts',(5.87482976928782,1.2128746137544,11.9955180766638));
#51005=CARTESIAN_POINT('Ctrl Pts',(5.91285353896481,0.228366908574042,11.9491269241899));
#51006=CARTESIAN_POINT('Ctrl Pts',(5.95087730864179,-0.756140796606319,
11.9027357717159));
#51007=CARTESIAN_POINT('Ctrl Pts',(5.73767899226313,-1.75035123005147,11.8563446192419));
#51008=CARTESIAN_POINT('Ctrl Pts',(5.29932581987711,-2.63270474473765,11.8099534667679));
#51009=CARTESIAN_POINT('Ctrl Pts',(4.86097264749109,-3.51505825942384,11.7635623142939));
#51010=CARTESIAN_POINT('Ctrl Pts',(4.19746461909773,-4.28555485535106,11.7171711618199));
#51011=CARTESIAN_POINT('Ctrl Pts',(3.38992721780971,-4.84998782226649,11.670780009346));
#51012=CARTESIAN_POINT('Ctrl Pts',(2.5823898165217,-5.41442078918191,11.624388856872));
#51013=CARTESIAN_POINT('Ctrl Pts',(1.63082304233903,-5.77279012708554,11.577997704398));
#51014=CARTESIAN_POINT('Ctrl Pts',(0.651572607696405,-5.88127890471792,
11.531606551924));
#51015=CARTESIAN_POINT('Ctrl Pts',(-0.327677826946226,-5.9897676823503,
11.48521539945));
#51016=CARTESIAN_POINT('Ctrl Pts',(-1.33461192204882,-5.84837589971142,
11.438824246976));
#51017=CARTESIAN_POINT('Ctrl Pts',(-2.24611433999348,-5.47439117983507,
11.3924330945021));
#51018=CARTESIAN_POINT('Ctrl Pts',(-3.15761675793815,-5.1004064599587,11.3460419420281));
#51019=CARTESIAN_POINT('Ctrl Pts',(-3.97368749872487,-4.49382880284485,
11.2996507895541));
#51020=CARTESIAN_POINT('Ctrl Pts',(-4.59454761429665,-3.72882295612721,
11.2532596370801));
#51021=CARTESIAN_POINT('Ctrl Pts',(-5.21540772986842,-2.96381710940959,
11.2068684846061));
#51022=CARTESIAN_POINT('Ctrl Pts',(-5.64105722022526,-2.04038307308817,
11.1604773321321));
#51023=CARTESIAN_POINT('Ctrl Pts',(-5.81945297652116,-1.07142683942457,
11.1140861796581));
#51024=CARTESIAN_POINT('Ctrl Pts',(-5.88445549299818,-0.718365786560998,
11.0971825171737));
#51025=CARTESIAN_POINT('Ctrl Pts',(-5.91663078529745,-0.359260871982291,
11.0802788546893));
#51026=CARTESIAN_POINT('Ctrl Pts',(-5.91638614209071,-0.000112643280536506,
11.0633751922049));
#51027=CARTESIAN_POINT('Ctrl Pts',(-5.91650151471712,-0.000138897455152014,
10.8116248077952));
#51028=CARTESIAN_POINT('Ctrl Pts',(-5.91676990590458,-0.31106708737575,
10.8262597648342));
#51029=CARTESIAN_POINT('Ctrl Pts',(-5.89268752645461,-0.621954105016895,
10.8408947218732));
#51030=CARTESIAN_POINT('Ctrl Pts',(-5.84389498008895,-0.928913330743386,
10.8555296789123));
#51031=CARTESIAN_POINT('Ctrl Pts',(-5.68922814697106,-1.90193923071684,
10.9019208313862));
#51032=CARTESIAN_POINT('Ctrl Pts',(-5.28626910131762,-2.83549796933134,
10.9483119838602));
#51033=CARTESIAN_POINT('Ctrl Pts',(-4.68428664750531,-3.61544563205493,
10.9947031363342));
#51034=CARTESIAN_POINT('Ctrl Pts',(-4.08230419369302,-4.39539329477851,
11.0410942888082));
#51035=CARTESIAN_POINT('Ctrl Pts',(-3.28129833172186,-5.0217298816112,11.0874854412822));
#51036=CARTESIAN_POINT('Ctrl Pts',(-2.37920606423197,-5.41787476952573,
11.1338765937562));
#51037=CARTESIAN_POINT('Ctrl Pts',(-1.47711379674208,-5.81401965744026,
11.1802677462301));
#51038=CARTESIAN_POINT('Ctrl Pts',(-0.473935123733492,-5.97997284643662,
11.2266588987041));
#51039=CARTESIAN_POINT('Ctrl Pts',(0.507673783333144,-5.89544365116467,
11.2730500511781));
#51040=CARTESIAN_POINT('Ctrl Pts',(1.48928269039977,-5.81091445589273,11.3194412036521));
#51041=CARTESIAN_POINT('Ctrl Pts',(2.44932183152441,-5.47590287635248,11.3658323561261));
#51042=CARTESIAN_POINT('Ctrl Pts',(3.27040959895255,-4.9313699485458,11.4122235086001));
#51043=CARTESIAN_POINT('Ctrl Pts',(4.09149736638069,-4.38683702073912,11.4586146610741));
#51044=CARTESIAN_POINT('Ctrl Pts',(4.77363376011235,-3.63278274466601,11.505005813548));
#51045=CARTESIAN_POINT('Ctrl Pts',(5.23341565294764,-2.7614034688586,11.551396966022));
#51046=CARTESIAN_POINT('Ctrl Pts',(5.69319754578292,-1.89002419305118,11.597788118496));
#51047=CARTESIAN_POINT('Ctrl Pts',(5.93062493772184,-0.901319917509466,
11.64417927097));
#51048=CARTESIAN_POINT('Ctrl Pts',(5.91666816966309,0.0838229350308153,
11.690570423444));
#51049=CARTESIAN_POINT('Ctrl Pts',(5.90271140160435,1.0689657875711,11.736961575918));
#51050=CARTESIAN_POINT('Ctrl Pts',(5.63737047354794,2.05054721710995,11.7833527283919));
#51051=CARTESIAN_POINT('Ctrl Pts',(5.15308796351401,2.90855169364903,11.8297438808659));
#51052=CARTESIAN_POINT('Ctrl Pts',(4.66880545348009,3.7665561701881,11.8761350333399));
#51053=CARTESIAN_POINT('Ctrl Pts',(3.96558136146864,4.5009836937274,11.9225261858139));
#51054=CARTESIAN_POINT('Ctrl Pts',(3.12939715531371,5.02203763015134,11.9689173382879));
#51055=CARTESIAN_POINT('Ctrl Pts',(2.29321294915875,5.54309156657529,12.0153084907619));
#51056=CARTESIAN_POINT('Ctrl Pts',(1.32406862886034,5.85077191588387,12.0616996432359));
#51057=CARTESIAN_POINT('Ctrl Pts',(0.340459069876811,5.90745936389581,12.1080907957098));
#51058=CARTESIAN_POINT('Ctrl Pts',(-0.643150489106702,5.96414681190774,
12.1544819481838));
#51059=CARTESIAN_POINT('Ctrl Pts',(-1.6412252867753,5.76984135862302,12.2008731006578));
#51060=CARTESIAN_POINT('Ctrl Pts',(-2.5317331898637,5.34830025051737,12.2472642531318));
#51061=CARTESIAN_POINT('Ctrl Pts',(-3.42224109295211,4.92675914241172,12.2936554056058));
#51062=CARTESIAN_POINT('Ctrl Pts',(-4.20518210146036,4.27798237948509,12.3400465580798));
#51063=CARTESIAN_POINT('Ctrl Pts',(-4.78482795763426,3.48129428951119,12.3864377105537));
#51064=CARTESIAN_POINT('Ctrl Pts',(-5.36447381380816,2.68460619953728,12.4328288630277));
#51065=CARTESIAN_POINT('Ctrl Pts',(-5.74082451764775,1.7400067825161,12.4792200155017));
#51066=CARTESIAN_POINT('Ctrl Pts',(-5.86786460082069,0.762989869380371,
12.5256111679757));
#51067=CARTESIAN_POINT('Ctrl Pts',(-5.90073851142677,0.510169138624673,
12.5376157145822));
#51068=CARTESIAN_POINT('Ctrl Pts',(-5.91691836162161,0.25517770356015,12.5496202611887));
#51069=CARTESIAN_POINT('Ctrl Pts',(-5.91666319015572,0.00015412212114384,
12.5616248077952));
#51070=CARTESIAN_POINT('Origin',(0.,0.,0.));
#51071=CARTESIAN_POINT('',(-5.91679636992553,-0.000153270388958127,14.5633751922049));
#51072=CARTESIAN_POINT('',(-5.91694833112707,-0.000138697138948813,14.3116248077952));
#51073=CARTESIAN_POINT('',(-5.91675,-7.2459289488551E-16,0.));
#51074=CARTESIAN_POINT('Ctrl Pts',(-5.91679636992553,-0.000153270388958127,
14.5633751922049));
#51075=CARTESIAN_POINT('Ctrl Pts',(-5.91599400906461,0.77255147152922,14.5269998473983));
#51076=CARTESIAN_POINT('Ctrl Pts',(-5.76385503515043,1.54556283765356,14.4906245025916));
#51077=CARTESIAN_POINT('Ctrl Pts',(-5.46885912034106,2.25955047300182,14.454249157785));
#51078=CARTESIAN_POINT('Ctrl Pts',(-5.09263724434586,3.17013178658265,14.407858005311));
#51079=CARTESIAN_POINT('Ctrl Pts',(-4.48405747423019,3.98471055593761,14.361466852837));
#51080=CARTESIAN_POINT('Ctrl Pts',(-3.71752935102522,4.60369025266104,14.315075700363));
#51081=CARTESIAN_POINT('Ctrl Pts',(-2.95100122782026,5.22266994938447,14.2686845478891));
#51082=CARTESIAN_POINT('Ctrl Pts',(-2.026524751526,5.64605057347636,14.2222933954151));
#51083=CARTESIAN_POINT('Ctrl Pts',(-1.05713337095738,5.82206642474891,14.1759022429411));
#51084=CARTESIAN_POINT('Ctrl Pts',(-0.0877419903887519,5.99808227602147,
14.1295110904671));
#51085=CARTESIAN_POINT('Ctrl Pts',(0.926564294454247,5.92673335447469,14.0831199379931));
#51086=CARTESIAN_POINT('Ctrl Pts',(1.86176876657516,5.61674331601378,14.0367287855192));
#51087=CARTESIAN_POINT('Ctrl Pts',(2.7969732386961,5.30675327755287,13.9903376330452));
#51088=CARTESIAN_POINT('Ctrl Pts',(3.65307589809495,4.75812212217783,13.9439464805712));
#51089=CARTESIAN_POINT('Ctrl Pts',(4.32540319318566,4.03792962228907,13.8975553280972));
#51090=CARTESIAN_POINT('Ctrl Pts',(4.99773048827635,3.31773712240034,13.8511641756232));
#51091=CARTESIAN_POINT('Ctrl Pts',(5.48628241905891,2.4259832779979,13.8047730231492));
#51092=CARTESIAN_POINT('Ctrl Pts',(5.73132495110672,1.47170062274971,13.7583818706752));
#51093=CARTESIAN_POINT('Ctrl Pts',(5.97636748315454,0.517417967501514,13.7119907182013));
#51094=CARTESIAN_POINT('Ctrl Pts',(5.97790061646761,-0.499393498592441,
13.6655995657273));
#51095=CARTESIAN_POINT('Ctrl Pts',(5.73573689863335,-1.45441075622952,13.6192084132533));
#51096=CARTESIAN_POINT('Ctrl Pts',(5.4935731807991,-2.40942801386659,13.5728172607793));
#51097=CARTESIAN_POINT('Ctrl Pts',(5.00771261181753,-3.30265106304676,13.5264261083053));
#51098=CARTESIAN_POINT('Ctrl Pts',(4.33756015997436,-4.0248677340732,13.4800349558313));
#51099=CARTESIAN_POINT('Ctrl Pts',(3.66740770813118,-4.74708440509965,13.4336438033574));
#51100=CARTESIAN_POINT('Ctrl Pts',(2.8129633734264,-5.29829469797234,13.3872526508834));
#51101=CARTESIAN_POINT('Ctrl Pts',(1.87869794819343,-5.61110349553759,13.3408614984094));
#51102=CARTESIAN_POINT('Ctrl Pts',(0.944432522960453,-5.92391229310283,
13.2944703459354));
#51103=CARTESIAN_POINT('Ctrl Pts',(-0.069653992800721,-5.99831959536062,
13.2480791934614));
#51104=CARTESIAN_POINT('Ctrl Pts',(-1.0395717527149,-5.82522780577186,13.2016880409874));
#51105=CARTESIAN_POINT('Ctrl Pts',(-2.00948951262906,-5.65213601618309,
13.1552968885134));
#51106=CARTESIAN_POINT('Ctrl Pts',(-2.93523851669623,-5.23154513474778,
13.1089057360395));
#51107=CARTESIAN_POINT('Ctrl Pts',(-3.70362972728275,-4.61487976672933,
13.0625145835655));
#51108=CARTESIAN_POINT('Ctrl Pts',(-4.47202093786928,-3.99821439871089,
13.0161234310915));
#51109=CARTESIAN_POINT('Ctrl Pts',(-5.08305435497515,-3.1854745441093,12.9697322786175));
#51110=CARTESIAN_POINT('Ctrl Pts',(-5.46202043622944,-2.27603189177837,
12.9233411261435));
#51111=CARTESIAN_POINT('Ctrl Pts',(-5.7614551116923,-1.55744867569876,12.8866858148307));
#51112=CARTESIAN_POINT('Ctrl Pts',(-5.91600675784442,-0.778492489737632,
12.8500305035178));
#51113=CARTESIAN_POINT('Ctrl Pts',(-5.91681535977711,0.00015225615038035,
12.8133751922049));
#51114=CARTESIAN_POINT('Ctrl Pts',(-5.91666319015572,0.00015412212114384,
12.5616248077952));
#51115=CARTESIAN_POINT('Ctrl Pts',(-5.91593226037439,-0.730352049358422,
12.5960114136627));
#51116=CARTESIAN_POINT('Ctrl Pts',(-5.78034933477605,-1.46112198701044,
12.6303980195302));
#51117=CARTESIAN_POINT('Ctrl Pts',(-5.51600270409303,-2.14189231353492,
12.6647846253976));
#51118=CARTESIAN_POINT('Ctrl Pts',(-5.15937126168614,-3.06032317406425,
12.7111757778716));
#51119=CARTESIAN_POINT('Ctrl Pts',(-4.56837891436605,-3.88775048587267,
12.7575669303456));
#51120=CARTESIAN_POINT('Ctrl Pts',(-3.81528483254303,-4.52300676109474,
12.8039580828196));
#51121=CARTESIAN_POINT('Ctrl Pts',(-3.06219075072002,-5.1582630363168,12.8503492352936));
#51122=CARTESIAN_POINT('Ctrl Pts',(-2.14699493439408,-5.60134827495253,
12.8967403877676));
#51123=CARTESIAN_POINT('Ctrl Pts',(-1.18159610907414,-5.79808754240245,
12.9431315402415));
#51124=CARTESIAN_POINT('Ctrl Pts',(-0.216197283754185,-5.99482680985238,
12.9895226927155));
#51125=CARTESIAN_POINT('Ctrl Pts',(0.79940455055973,-5.9452201061165,13.0359138451895));
#51126=CARTESIAN_POINT('Ctrl Pts',(1.74103427324652,-5.65533271998409,13.0823049976635));
#51127=CARTESIAN_POINT('Ctrl Pts',(2.68266399593328,-5.36544533385168,13.1286961501375));
#51128=CARTESIAN_POINT('Ctrl Pts',(3.55032160699291,-4.83527726532272,13.1750873026115));
#51129=CARTESIAN_POINT('Ctrl Pts',(4.2379207595215,-4.12965085090232,13.2214784550854));
#51130=CARTESIAN_POINT('Ctrl Pts',(4.92551991205011,-3.42402443648192,13.2678696075594));
#51131=CARTESIAN_POINT('Ctrl Pts',(5.43306060604772,-2.54293967617006,13.3142607600334));
#51132=CARTESIAN_POINT('Ctrl Pts',(5.69848709804486,-1.59412462115041,13.3606519125074));
#51133=CARTESIAN_POINT('Ctrl Pts',(5.963913590042,-0.645309566130763,13.4070430649814));
#51134=CARTESIAN_POINT('Ctrl Pts',(5.98722588003867,0.371235783596643,13.4534342174554));
#51135=CARTESIAN_POINT('Ctrl Pts',(5.76557363208187,1.3312209461182,13.4998253699294));
#51136=CARTESIAN_POINT('Ctrl Pts',(5.54392138412507,2.29120610863978,13.5462165224033));
#51137=CARTESIAN_POINT('Ctrl Pts',(5.07730459821478,3.19463108395547,13.5926076748773));
#51138=CARTESIAN_POINT('Ctrl Pts',(4.42277535294775,3.93103633813013,13.6389988273513));
#51139=CARTESIAN_POINT('Ctrl Pts',(3.76824610768071,4.66744159230479,13.6853899798253));
#51140=CARTESIAN_POINT('Ctrl Pts',(2.92580440305693,5.23682712533842,13.7317811322993));
#51141=CARTESIAN_POINT('Ctrl Pts',(1.99845349956049,5.56957557848316,13.7781722847733));
#51142=CARTESIAN_POINT('Ctrl Pts',(1.07110259606408,5.9023240316279,13.8245634372472));
#51143=CARTESIAN_POINT('Ctrl Pts',(0.0588424936950185,5.99843540488377,
13.8709545897212));
#51144=CARTESIAN_POINT('Ctrl Pts',(-0.914560272212906,5.84615839871205,
13.9173457421952));
#51145=CARTESIAN_POINT('Ctrl Pts',(-1.88796303812086,5.69388139254032,13.9637368946692));
#51146=CARTESIAN_POINT('Ctrl Pts',(-2.82250846756768,5.29321600694098,14.0101280471432));
#51147=CARTESIAN_POINT('Ctrl Pts',(-3.60393200577741,4.69315060615732,14.0565191996172));
#51148=CARTESIAN_POINT('Ctrl Pts',(-4.38535554398713,4.09308520537367,14.1029103520911));
#51149=CARTESIAN_POINT('Ctrl Pts',(-5.01365719095976,3.29361978940572,14.1493015045651));
#51150=CARTESIAN_POINT('Ctrl Pts',(-5.41201606063222,2.39250301437647,14.1956926570391));
#51151=CARTESIAN_POINT('Ctrl Pts',(-5.7438508902712,1.64186846274086,14.2343367072911));
#51152=CARTESIAN_POINT('Ctrl Pts',(-5.91612913741916,0.82069834722353,14.2729807575432));
#51153=CARTESIAN_POINT('Ctrl Pts',(-5.91694833112707,-0.000138697138948813,
14.3116248077952));
#51154=CARTESIAN_POINT('Origin',(0.,0.,0.));
#51155=CARTESIAN_POINT('',(-5.91639886804204,0.000116455658438486,16.3133751922049));
#51156=CARTESIAN_POINT('',(-5.91630979238255,8.1702894319434E-5,16.0616248077952));
#51157=CARTESIAN_POINT('',(-5.91675,-7.2459289488551E-16,0.));
#51158=CARTESIAN_POINT('Ctrl Pts',(-5.91639886804204,0.000116455658438486,
16.3133751922049));
#51159=CARTESIAN_POINT('Ctrl Pts',(-5.91664831842101,0.35331412429619,16.2967514962267));
#51160=CARTESIAN_POINT('Ctrl Pts',(-5.88553605112261,0.706468355663527,
16.2801278002486));
#51161=CARTESIAN_POINT('Ctrl Pts',(-5.82265747229035,1.05387303721164,16.2635041042704));
#51162=CARTESIAN_POINT('Ctrl Pts',(-5.64718447628607,2.02336282895428,16.2171129517964));
#51163=CARTESIAN_POINT('Ctrl Pts',(-5.22432159535791,2.9480762396989,16.1707217993224));
#51164=CARTESIAN_POINT('Ctrl Pts',(-4.60577122651949,3.71495085124224,16.1243306468484));
#51165=CARTESIAN_POINT('Ctrl Pts',(-3.98722085768104,4.48182546278563,16.0779394943744));
#51166=CARTESIAN_POINT('Ctrl Pts',(-3.1729830009323,5.09086127512771,16.0315483419005));
#51167=CARTESIAN_POINT('Ctrl Pts',(-2.26261250213904,5.46759298808392,15.9851571894265));
#51168=CARTESIAN_POINT('Ctrl Pts',(-1.35224200334581,5.84432470104011,15.9387660369525));
#51169=CARTESIAN_POINT('Ctrl Pts',(-0.345738862508056,5.98875231461044,
15.8923748844785));
#51170=CARTESIAN_POINT('Ctrl Pts',(0.633834274466793,5.88321702223295,15.8459837320045));
#51171=CARTESIAN_POINT('Ctrl Pts',(1.61340741144164,5.77768172985545,15.7995925795305));
#51172=CARTESIAN_POINT('Ctrl Pts',(2.56605054455358,5.42218353153013,15.7532014270566));
#51173=CARTESIAN_POINT('Ctrl Pts',(3.37528635762781,4.86018831139205,15.7068102745826));
#51174=CARTESIAN_POINT('Ctrl Pts',(4.18452217070204,4.29819309125397,15.6604191221086));
#51175=CARTESIAN_POINT('Ctrl Pts',(4.85035066373854,3.52970084930314,15.6140279696346));
#51176=CARTESIAN_POINT('Ctrl Pts',(5.29136263616055,2.64867322839651,15.5676368171606));
#51177=CARTESIAN_POINT('Ctrl Pts',(5.73237460858256,1.76764560748987,15.5212456646866));
#51178=CARTESIAN_POINT('Ctrl Pts',(5.94857006039006,0.774082607627441,15.4748545122126));
#51179=CARTESIAN_POINT('Ctrl Pts',(5.91351530920981,-0.2105352842675,15.4284633597387));
#51180=CARTESIAN_POINT('Ctrl Pts',(5.87846055802955,-1.19515317616244,15.3820722072647));
#51181=CARTESIAN_POINT('Ctrl Pts',(5.59215560386154,-2.17082596008989,15.3356810547907));
#51182=CARTESIAN_POINT('Ctrl Pts',(5.0896062442704,-3.01826054151461,15.2892899023167));
#51183=CARTESIAN_POINT('Ctrl Pts',(4.58705688467926,-3.86569512293933,15.2428987498427));
#51184=CARTESIAN_POINT('Ctrl Pts',(3.86826311966498,-4.58489150186131,15.1965075973688));
#51185=CARTESIAN_POINT('Ctrl Pts',(3.02111008241334,-5.08791531848957,15.1501164448948));
#51186=CARTESIAN_POINT('Ctrl Pts',(2.1739570451617,-5.59093913511783,15.1037252924208));
#51187=CARTESIAN_POINT('Ctrl Pts',(1.19844473567268,-5.87779038945237,15.0573341399468));
#51188=CARTESIAN_POINT('Ctrl Pts',(0.213846627669457,-5.91339648916041,
15.0109429874728));
#51189=CARTESIAN_POINT('Ctrl Pts',(-0.770751480333769,-5.94900258886845,
14.9645518349988));
#51190=CARTESIAN_POINT('Ctrl Pts',(-1.7644353868512,-5.73336353394999,14.9181606825248));
#51191=CARTESIAN_POINT('Ctrl Pts',(-2.64570982200234,-5.29284497750885,
14.8717695300509));
#51192=CARTESIAN_POINT('Ctrl Pts',(-3.52698425715349,-4.85232642106771,
14.8253783775769));
#51193=CARTESIAN_POINT('Ctrl Pts',(-4.29584922093833,-4.18692836310389,
14.7789872251029));
#51194=CARTESIAN_POINT('Ctrl Pts',(-4.85829749872451,-3.37800737596404,
14.7325960726289));
#51195=CARTESIAN_POINT('Ctrl Pts',(-5.4207457765107,-2.56908638882419,14.6862049201549));
#51196=CARTESIAN_POINT('Ctrl Pts',(-5.77677736829822,-1.61664247250831,
14.6398137676809));
#51197=CARTESIAN_POINT('Ctrl Pts',(-5.88286117325461,-0.637128585447021,
14.593422615207));
#51198=CARTESIAN_POINT('Ctrl Pts',(-5.90576457035516,-0.425652427233307,
14.5834068075396));
#51199=CARTESIAN_POINT('Ctrl Pts',(-5.91701729682273,-0.212914472237162,
14.5733909998723));
#51200=CARTESIAN_POINT('Ctrl Pts',(-5.91679636992553,-0.000153270388958127,
14.5633751922049));
#51201=CARTESIAN_POINT('Ctrl Pts',(-5.91694833112707,-0.000138697138948813,
14.3116248077952));
#51202=CARTESIAN_POINT('Ctrl Pts',(-5.91711255763421,-0.164694649446748,
14.3193719100171));
#51203=CARTESIAN_POINT('Ctrl Pts',(-5.91038591951096,-0.329237215769999,
14.3271190122391));
#51204=CARTESIAN_POINT('Ctrl Pts',(-5.89667251930381,-0.493195412011086,
14.3348661144611));
#51205=CARTESIAN_POINT('Ctrl Pts',(-5.81455401593065,-1.4750089292788,14.3812572669351));
#51206=CARTESIAN_POINT('Ctrl Pts',(-5.48190091681204,-2.43586782972369,
14.427648419409));
#51207=CARTESIAN_POINT('Ctrl Pts',(-4.93938589239068,-3.25829027564972,
14.474039571883));
#51208=CARTESIAN_POINT('Ctrl Pts',(-4.39687086796933,-4.08071272157575,
14.520430724357));
#51209=CARTESIAN_POINT('Ctrl Pts',(-3.64449391824523,-4.76469871298291,
14.566821876831));
#51210=CARTESIAN_POINT('Ctrl Pts',(-2.7742463092126,-5.22661897694503,14.613213029305));
#51211=CARTESIAN_POINT('Ctrl Pts',(-1.90399870017996,-5.68853924090715,
14.659604181779));
#51212=CARTESIAN_POINT('Ctrl Pts',(-0.91588043183879,-5.92839377742422,
14.7059953342529));
#51213=CARTESIAN_POINT('Ctrl Pts',(0.0692937227240556,-5.91685616643946,
14.7523864867269));
#51214=CARTESIAN_POINT('Ctrl Pts',(1.0544678772869,-5.90531855545469,14.7987776392009));
#51215=CARTESIAN_POINT('Ctrl Pts',(2.03669791807142,-5.64238879696809,14.8451687916749));
#51216=CARTESIAN_POINT('Ctrl Pts',(2.89588901098887,-5.160214661269,14.8915599441489));
#51217=CARTESIAN_POINT('Ctrl Pts',(3.75508010390632,-4.67804052556991,14.9379510966229));
#51218=CARTESIAN_POINT('Ctrl Pts',(4.49123224895671,-3.97662201265833,14.9843422490968));
#51219=CARTESIAN_POINT('Ctrl Pts',(5.01433794682421,-3.14171982668418,15.0307334015708));
#51220=CARTESIAN_POINT('Ctrl Pts',(5.5374436446917,-2.30681764071002,15.0771245540448));
#51221=CARTESIAN_POINT('Ctrl Pts',(5.84750289537631,-1.33843178167331,15.1235157065188));
#51222=CARTESIAN_POINT('Ctrl Pts',(5.90660552231805,-0.354964389852698,
15.1699068589928));
#51223=CARTESIAN_POINT('Ctrl Pts',(5.9657081492598,0.628503001967902,15.2162980114668));
#51224=CARTESIAN_POINT('Ctrl Pts',(5.77385415245868,1.62705192657243,15.2626891639407));
#51225=CARTESIAN_POINT('Ctrl Pts',(5.35450104487847,2.51859228036953,15.3090803164147));
#51226=CARTESIAN_POINT('Ctrl Pts',(4.93514793729825,3.41013263416665,15.3554714688887));
#51227=CARTESIAN_POINT('Ctrl Pts',(4.28829571893895,4.19466441715633,15.4018626213627));
#51228=CARTESIAN_POINT('Ctrl Pts',(3.49303340827702,4.77626487152903,15.4482537738367));
#51229=CARTESIAN_POINT('Ctrl Pts',(2.69777109761512,5.35786532590172,15.4946449263107));
#51230=CARTESIAN_POINT('Ctrl Pts',(1.75409869465059,5.73653445165742,15.5410360787846));
#51231=CARTESIAN_POINT('Ctrl Pts',(0.777396686603823,5.86597331275885,15.5874272312586));
#51232=CARTESIAN_POINT('Ctrl Pts',(-0.199305321442962,5.99541217386027,
15.6338183837326));
#51233=CARTESIAN_POINT('Ctrl Pts',(-1.20903693457202,5.87562077030744,15.6802095362066));
#51234=CARTESIAN_POINT('Ctrl Pts',(-2.12834076956585,5.52124570028771,15.7266006886806));
#51235=CARTESIAN_POINT('Ctrl Pts',(-3.04764460455968,5.16687063026797,15.7729918411546));
#51236=CARTESIAN_POINT('Ctrl Pts',(-3.87652066141828,4.57791189378134,15.8193829936286));
#51237=CARTESIAN_POINT('Ctrl Pts',(-4.51362431780749,3.82638001667875,15.8657741461025));
#51238=CARTESIAN_POINT('Ctrl Pts',(-5.15072797419671,3.07484813957616,15.9121652985765));
#51239=CARTESIAN_POINT('Ctrl Pts',(-5.59605923011654,2.1607431218576,15.9585564510505));
#51240=CARTESIAN_POINT('Ctrl Pts',(-5.79516853599763,1.19583031978821,16.0049476035245));
#51241=CARTESIAN_POINT('Ctrl Pts',(-5.87625410368171,0.802877805714503,
16.0238400049481));
#51242=CARTESIAN_POINT('Ctrl Pts',(-5.91650483938724,0.401499043140845,
16.0427324063716));
#51243=CARTESIAN_POINT('Ctrl Pts',(-5.91630979238255,8.1702894319434E-5,
16.0616248077952));
#51244=CARTESIAN_POINT('Origin',(0.,0.,0.));
#51245=CARTESIAN_POINT('',(-5.91719822611734,-6.82369026905327E-5,18.0633751922049));
#51246=CARTESIAN_POINT('',(-5.91725660741841,-1.9475412519191E-5,17.8116248077952));
#51247=CARTESIAN_POINT('',(-5.91675,-7.2459289488551E-16,0.));
#51248=CARTESIAN_POINT('Ctrl Pts',(-5.91719822611734,-6.82369026905327E-5,
18.0633751922049));
#51249=CARTESIAN_POINT('Ctrl Pts',(-5.91666274279714,0.918771692973182,
18.0201119925812));
#51250=CARTESIAN_POINT('Ctrl Pts',(-5.69916543753697,1.83785627542067,17.9768487929575));
#51251=CARTESIAN_POINT('Ctrl Pts',(-5.28633221943619,2.65869894571221,17.9335855933338));
#51252=CARTESIAN_POINT('Ctrl Pts',(-4.84365093525427,3.53888898726857,17.8871944408598));
#51253=CARTESIAN_POINT('Ctrl Pts',(-4.17636686005132,4.3061176826772,17.8408032883858));
#51254=CARTESIAN_POINT('Ctrl Pts',(-3.36606716483014,4.86657787978705,17.7944121359119));
#51255=CARTESIAN_POINT('Ctrl Pts',(-2.55576746960896,5.4270380768969,17.7480209834379));
#51256=CARTESIAN_POINT('Ctrl Pts',(-1.60245215436954,5.78072977570796,17.7016298309639));
#51257=CARTESIAN_POINT('Ctrl Pts',(-0.622680721330418,5.88440796830605,
17.6552386784899));
#51258=CARTESIAN_POINT('Ctrl Pts',(0.35709071170871,5.98808616090414,17.6088475260159));
#51259=CARTESIAN_POINT('Ctrl Pts',(1.36331826254754,5.84175084728925,17.5624563735419));
#51260=CARTESIAN_POINT('Ctrl Pts',(2.27297298098518,5.46329408378239,17.516065221068));
#51261=CARTESIAN_POINT('Ctrl Pts',(3.18262769942285,5.08483732027552,17.469674068594));
#51262=CARTESIAN_POINT('Ctrl Pts',(3.99570958545932,4.47425910687667,17.42328291612));
#51263=CARTESIAN_POINT('Ctrl Pts',(4.61280513090447,3.70621332932708,17.376891763646));
#51264=CARTESIAN_POINT('Ctrl Pts',(5.2299006763496,2.93816755177751,17.330500611172));
#51265=CARTESIAN_POINT('Ctrl Pts',(5.65100988120343,2.01265421007721,17.284109458698));
#51266=CARTESIAN_POINT('Ctrl Pts',(5.82464476608204,1.04283352800596,17.237718306224));
#51267=CARTESIAN_POINT('Ctrl Pts',(5.99827965096066,0.0730128459347218,
17.1913271537501));
#51268=CARTESIAN_POINT('Ctrl Pts',(5.92444021586407,-0.941115176507489,
17.1449360012761));
#51269=CARTESIAN_POINT('Ctrl Pts',(5.61215462562019,-1.87555561802635,17.0985448488021));
#51270=CARTESIAN_POINT('Ctrl Pts',(5.29986903537631,-2.80999605954522,17.0521536963281));
#51271=CARTESIAN_POINT('Ctrl Pts',(4.74913728998514,-3.66474892014077,17.0057625438541));
#51272=CARTESIAN_POINT('Ctrl Pts',(4.02729599578517,-4.33530568478315,16.9593713913801));
#51273=CARTESIAN_POINT('Ctrl Pts',(3.30545470158519,-5.00586244942553,16.9129802389062));
#51274=CARTESIAN_POINT('Ctrl Pts',(2.41250385857643,-5.49222311811475,16.8665890864322));
#51275=CARTESIAN_POINT('Ctrl Pts',(1.45762235448143,-5.73492157661256,16.8201979339582));
#51276=CARTESIAN_POINT('Ctrl Pts',(0.502740850386421,-5.97762003511037,
16.7738067814842));
#51277=CARTESIAN_POINT('Ctrl Pts',(-0.514071314794815,-5.97665628341679,
16.7274156290102));
#51278=CARTESIAN_POINT('Ctrl Pts',(-1.46849103628399,-5.73214815706415,
16.6810244765362));
#51279=CARTESIAN_POINT('Ctrl Pts',(-2.42291075777316,-5.4876400307115,16.6346333240623));
#51280=CARTESIAN_POINT('Ctrl Pts',(-3.31493803557027,-4.99958752969981,
16.5882421715883));
#51281=CARTESIAN_POINT('Ctrl Pts',(-4.03550690398349,-4.32766362441467,
16.5418510191143));
#51282=CARTESIAN_POINT('Ctrl Pts',(-4.7560757723967,-3.65573971912954,16.4954598666403));
#51283=CARTESIAN_POINT('Ctrl Pts',(-5.30518623142603,-2.799944409571,16.4490687141663));
#51284=CARTESIAN_POINT('Ctrl Pts',(-5.61569990540051,-1.8649136684214,16.4026775616923));
#51285=CARTESIAN_POINT('Ctrl Pts',(-5.81494484303325,-1.26493963404005,
16.3729101051965));
#51286=CARTESIAN_POINT('Ctrl Pts',(-5.9159521861902,-0.632341948862379,
16.3431426487007));
#51287=CARTESIAN_POINT('Ctrl Pts',(-5.91639886804204,0.000116455658438486,
16.3133751922049));
#51288=CARTESIAN_POINT('Ctrl Pts',(-5.91630979238255,8.1702894319434E-5,
16.0616248077952));
#51289=CARTESIAN_POINT('Ctrl Pts',(-5.91602589258047,-0.584199525271585,
16.0891235588456));
#51290=CARTESIAN_POINT('Ctrl Pts',(-5.83005303644549,-1.16856248459223,
16.116622309896));
#51291=CARTESIAN_POINT('Ctrl Pts',(-5.65959094982708,-1.72714179932542,
16.1441210609464));
#51292=CARTESIAN_POINT('Ctrl Pts',(-5.37201670193311,-2.66948052994944,
16.1905122134204));
#51293=CARTESIAN_POINT('Ctrl Pts',(-4.84398085030286,-3.53843740477723,
16.2369033658944));
#51294=CARTESIAN_POINT('Ctrl Pts',(-4.14004503056272,-4.22776721914234,
16.2832945183684));
#51295=CARTESIAN_POINT('Ctrl Pts',(-3.43610921082259,-4.91709703350743,
16.3296856708424));
#51296=CARTESIAN_POINT('Ctrl Pts',(-2.55627342297255,-5.42679978740986,
16.3760768233164));
#51297=CARTESIAN_POINT('Ctrl Pts',(-1.60811300942713,-5.694555387671,16.4224679757903));
#51298=CARTESIAN_POINT('Ctrl Pts',(-0.659952595881694,-5.96231098793215,
16.4688591282643));
#51299=CARTESIAN_POINT('Ctrl Pts',(0.356532443359141,-5.98811943455204,
16.5152502807383));
#51300=CARTESIAN_POINT('Ctrl Pts',(1.31705900039552,-5.76882519269035,16.5616414332123));
#51301=CARTESIAN_POINT('Ctrl Pts',(2.2775855574319,-5.54953095082865,16.6080325856863));
#51302=CARTESIAN_POINT('Ctrl Pts',(3.18215363226381,-5.08513402048537,16.6544237381603));
#51303=CARTESIAN_POINT('Ctrl Pts',(3.92016392700974,-4.43241506401568,16.7008148906342));
#51304=CARTESIAN_POINT('Ctrl Pts',(4.65817422175568,-3.77969610754599,16.7472060431082));
#51305=CARTESIAN_POINT('Ctrl Pts',(5.22962673641563,-2.93865512494991,16.7935971955822));
#51306=CARTESIAN_POINT('Ctrl Pts',(5.56465138751824,-2.01212411389878,16.8399883480562));
#51307=CARTESIAN_POINT('Ctrl Pts',(5.89967603862086,-1.08559310284766,16.8863795005302));
#51308=CARTESIAN_POINT('Ctrl Pts',(5.99827282616614,-0.0735720633414831,
16.9327706530042));
#51309=CARTESIAN_POINT('Ctrl Pts',(5.8483865651666,0.900201698910001,16.9791618054781));
#51310=CARTESIAN_POINT('Ctrl Pts',(5.69850030416705,1.8739754611615,17.0255529579521));
#51311=CARTESIAN_POINT('Ctrl Pts',(5.30013099462269,2.80950194615832,17.0719441104261));
#51312=CARTESIAN_POINT('Ctrl Pts',(4.70198626524495,3.59239664789253,17.1183352629001));
#51313=CARTESIAN_POINT('Ctrl Pts',(4.1038415358672,4.37529134962675,17.1647264153741));
#51314=CARTESIAN_POINT('Ctrl Pts',(3.30592138665607,5.00555426809834,17.2111175678481));
#51315=CARTESIAN_POINT('Ctrl Pts',(2.40578553779589,5.40612471743612,17.2575087203221));
#51316=CARTESIAN_POINT('Ctrl Pts',(1.50564968893573,5.80669516677389,17.303899872796));
#51317=CARTESIAN_POINT('Ctrl Pts',(0.50329814042653,5.97757314697785,17.35029102527));
#51318=CARTESIAN_POINT('Ctrl Pts',(-0.478714066734747,5.8978658306757,17.396682177744));
#51319=CARTESIAN_POINT('Ctrl Pts',(-1.46072627389601,5.81815851437354,17.443073330218));
#51320=CARTESIAN_POINT('Ctrl Pts',(-2.42239913970938,5.48786590156526,17.489464482692));
#51321=CARTESIAN_POINT('Ctrl Pts',(-3.24615130494937,4.94737205187937,17.535855635166));
#51322=CARTESIAN_POINT('Ctrl Pts',(-4.06990347018936,4.40687820219348,17.5822467876399));
#51323=CARTESIAN_POINT('Ctrl Pts',(-4.755734934856,3.65618311562998,17.6286379401139));
#51324=CARTESIAN_POINT('Ctrl Pts',(-5.21979078457892,2.7870724209404,17.6750290925879));
#51325=CARTESIAN_POINT('Ctrl Pts',(-5.67525148709518,1.93405921616332,17.720560997657));
#51326=CARTESIAN_POINT('Ctrl Pts',(-5.91707585786333,0.966976319151631,
17.7660929027261));
#51327=CARTESIAN_POINT('Ctrl Pts',(-5.91725660741841,-1.9475412519191E-5,
17.8116248077952));
#51328=CARTESIAN_POINT('Origin',(0.,0.,0.));
#51329=CARTESIAN_POINT('',(-5.9162403766418,-6.30554099573244E-6,19.8133751922049));
#51330=CARTESIAN_POINT('',(-5.91626547054495,-5.06783466652393E-5,19.5616248077952));
#51331=CARTESIAN_POINT('',(-5.91675,-7.2459289488551E-16,0.));
#51332=CARTESIAN_POINT('Ctrl Pts',(-5.9162403766418,-6.30554099573244E-6,
19.8133751922049));
#51333=CARTESIAN_POINT('Ctrl Pts',(-5.91622190953983,0.499573431236169,
19.7898636414097));
#51334=CARTESIAN_POINT('Ctrl Pts',(-5.85363170713743,0.999157711713498,
19.7663520906144));
#51335=CARTESIAN_POINT('Ctrl Pts',(-5.72852485080488,1.48256246137935,19.7428405398192));
#51336=CARTESIAN_POINT('Ctrl Pts',(-5.48167379031089,2.4363788915969,19.6964493873452));
#51337=CARTESIAN_POINT('Ctrl Pts',(-4.99143230021176,3.32720501911184,19.6500582348712));
#51338=CARTESIAN_POINT('Ctrl Pts',(-4.31774099316667,4.04612173990211,19.6036670823972));
#51339=CARTESIAN_POINT('Ctrl Pts',(-3.64404968612158,4.76503846069237,19.5572759299233));
#51340=CARTESIAN_POINT('Ctrl Pts',(-2.78690856213052,5.31204577475796,19.5108847774493));
#51341=CARTESIAN_POINT('Ctrl Pts',(-1.85111814327297,5.62026245275307,19.4644936249753));
#51342=CARTESIAN_POINT('Ctrl Pts',(-0.915327724415407,5.92847913074819,
19.4181024725013));
#51343=CARTESIAN_POINT('Ctrl Pts',(0.0991119893086599,5.99790517267283,
19.3717113200273));
#51344=CARTESIAN_POINT('Ctrl Pts',(1.068167966884,5.82005202835019,19.3253201675533));
#51345=CARTESIAN_POINT('Ctrl Pts',(2.03722394445934,5.64219888402755,19.2789290150793));
#51346=CARTESIAN_POINT('Ctrl Pts',(2.96089618588596,5.21706655345763,19.2325378626054));
#51347=CARTESIAN_POINT('Ctrl Pts',(3.72624957415409,4.59663491364028,19.1861467101314));
#51348=CARTESIAN_POINT('Ctrl Pts',(4.49160296242219,3.97620327382295,19.1397555576574));
#51349=CARTESIAN_POINT('Ctrl Pts',(5.09863749753183,3.16047232475821,19.0933644051834));
#51350=CARTESIAN_POINT('Ctrl Pts',(5.47313257050844,2.24917946901088,19.0469732527094));
#51351=CARTESIAN_POINT('Ctrl Pts',(5.84762764348506,1.33788661326349,19.0005821002354));
#51352=CARTESIAN_POINT('Ctrl Pts',(5.98958325432864,0.331031850833484,18.9541909477615));
#51353=CARTESIAN_POINT('Ctrl Pts',(5.88164284212742,-0.648279180470583,
18.9077997952875));
#51354=CARTESIAN_POINT('Ctrl Pts',(5.7737024299262,-1.62759021177459,18.8614086428135));
#51355=CARTESIAN_POINT('Ctrl Pts',(5.41586599468022,-2.57935751195267,18.8150174903395));
#51356=CARTESIAN_POINT('Ctrl Pts',(4.85188531096097,-3.38721085075339,18.7686263378655));
#51357=CARTESIAN_POINT('Ctrl Pts',(4.28790462724169,-4.19506418955415,18.7222351853915));
#51358=CARTESIAN_POINT('Ctrl Pts',(3.51777969504913,-4.85900356697753,18.6758440329176));
#51359=CARTESIAN_POINT('Ctrl Pts',(2.6356717822319,-5.29785075993339,18.6294528804436));
#51360=CARTESIAN_POINT('Ctrl Pts',(1.7535638694147,-5.73669795288924,18.5830617279696));
#51361=CARTESIAN_POINT('Ctrl Pts',(0.759472975972835,-5.95045296137758,
18.5366705754956));
#51362=CARTESIAN_POINT('Ctrl Pts',(-0.225055866930035,-5.91298048998478,
18.4902794230216));
#51363=CARTESIAN_POINT('Ctrl Pts',(-1.20958470983288,-5.87550801859199,
18.4438882705476));
#51364=CARTESIAN_POINT('Ctrl Pts',(-2.18455150219673,-5.58680806731807,
18.3974971180736));
#51365=CARTESIAN_POINT('Ctrl Pts',(-3.03074946932609,-5.08217926409134,
18.3511059655997));
#51366=CARTESIAN_POINT('Ctrl Pts',(-3.87694743645549,-4.57755046086458,
18.3047148131257));
#51367=CARTESIAN_POINT('Ctrl Pts',(-4.59437657835038,-3.85699280568499,
18.2583236606517));
#51368=CARTESIAN_POINT('Ctrl Pts',(-5.0953186109136,-3.00860709821967,18.2119325081777));
#51369=CARTESIAN_POINT('Ctrl Pts',(-5.59626064347681,-2.16022139075437,
18.1655413557037));
#51370=CARTESIAN_POINT('Ctrl Pts',(-5.88071556670836,-1.18400763100336,
18.1191502032297));
#51371=CARTESIAN_POINT('Ctrl Pts',(-5.91390378174369,-0.199325057275803,
18.0727590507558));
#51372=CARTESIAN_POINT('Ctrl Pts',(-5.91614151817142,-0.132932210819952,
18.0696310979055));
#51373=CARTESIAN_POINT('Ctrl Pts',(-5.91723694185247,-0.0665008633059073,
18.0665031450552));
#51374=CARTESIAN_POINT('Ctrl Pts',(-5.91719822611734,-6.82369026905327E-5,
18.0633751922049));
#51375=CARTESIAN_POINT('Ctrl Pts',(-5.91725660741841,-1.9475412519191E-5,
17.8116248077952));
#51376=CARTESIAN_POINT('Ctrl Pts',(-5.91726001840211,-0.0182679678874798,
17.8124840552001));
#51377=CARTESIAN_POINT('Ctrl Pts',(-5.91717737358503,-0.0365164293429135,
17.813343302605));
#51378=CARTESIAN_POINT('Ctrl Pts',(-5.91700848474174,-0.0547640925781233,
17.8142025500099));
#51379=CARTESIAN_POINT('Ctrl Pts',(-5.90789010040242,-1.03996360859147,
17.8605937024839));
#51380=CARTESIAN_POINT('Ctrl Pts',(-5.64737309694456,-2.02283633780253,
17.9069848549578));
#51381=CARTESIAN_POINT('Ctrl Pts',(-5.16731024307657,-2.88320886620057,
17.9533760074318));
#51382=CARTESIAN_POINT('Ctrl Pts',(-4.6872473892086,-3.74358139459857,17.9997671599058));
#51383=CARTESIAN_POINT('Ctrl Pts',(-3.98763868493051,-4.48145372218359,
18.0461583123798));
#51384=CARTESIAN_POINT('Ctrl Pts',(-3.15402355357354,-5.00660802718217,
18.0925494648538));
#51385=CARTESIAN_POINT('Ctrl Pts',(-2.32040842221657,-5.53176233218075,
18.1389406173278));
#51386=CARTESIAN_POINT('Ctrl Pts',(-1.35278686378078,-5.84419861459291,
18.1853317698017));
#51387=CARTESIAN_POINT('Ctrl Pts',(-0.369467569403431,-5.90571606407731,
18.2317229222757));
#51388=CARTESIAN_POINT('Ctrl Pts',(0.613851724973923,-5.96723351356171,
18.2781140747497));
#51389=CARTESIAN_POINT('Ctrl Pts',(1.6128687552928,-5.77783213011833,18.3245052272237));
#51390=CARTESIAN_POINT('Ctrl Pts',(2.50543618383567,-5.36066955175085,18.3708963796977));
#51391=CARTESIAN_POINT('Ctrl Pts',(3.39800361237853,-4.94350697338336,18.4172875321717));
#51392=CARTESIAN_POINT('Ctrl Pts',(4.18412143914543,-4.29858320009175,18.4636786846456));
#51393=CARTESIAN_POINT('Ctrl Pts',(4.76767298468275,-3.5047514641509,18.5100698371196));
#51394=CARTESIAN_POINT('Ctrl Pts',(5.35122453022008,-2.71091972821004,18.5564609895936));
#51395=CARTESIAN_POINT('Ctrl Pts',(5.73220979452784,-1.7681800296199,18.6028521420676));
#51396=CARTESIAN_POINT('Ctrl Pts',(5.86404665304509,-0.791798816147322,
18.6492432945416));
#51397=CARTESIAN_POINT('Ctrl Pts',(5.99588351156234,0.184582397325205,18.6956344470156));
#51398=CARTESIAN_POINT('Ctrl Pts',(5.87857196428913,1.19460512568014,18.7420255994895));
#51399=CARTESIAN_POINT('Ctrl Pts',(5.52645540352815,2.11477639176251,18.7884167519635));
#51400=CARTESIAN_POINT('Ctrl Pts',(5.17433884276716,3.03494765784494,18.8348079044375));
#51401=CARTESIAN_POINT('Ctrl Pts',(4.58741726851836,3.86526746165476,18.8811990569115));
#51402=CARTESIAN_POINT('Ctrl Pts',(3.83745212785197,4.50421465749424,18.9275902093855));
#51403=CARTESIAN_POINT('Ctrl Pts',(3.08748698718558,5.14316185333373,18.9739813618595));
#51404=CARTESIAN_POINT('Ctrl Pts',(2.17447828010157,5.5907364412029,19.0203725143335));
#51405=CARTESIAN_POINT('Ctrl Pts',(1.2100573196794,5.79221458489168,19.0667636668074));
#51406=CARTESIAN_POINT('Ctrl Pts',(0.245636359257291,5.99369272858046,19.1131548192814));
#51407=CARTESIAN_POINT('Ctrl Pts',(-0.77019685450301,5.94907442808888,19.1595459717554));
#51408=CARTESIAN_POINT('Ctrl Pts',(-1.71323891078853,5.6638150524979,19.2059371242294));
#51409=CARTESIAN_POINT('Ctrl Pts',(-2.65628096707413,5.37855567690688,19.2523282767034));
#51410=CARTESIAN_POINT('Ctrl Pts',(-3.52653186588491,4.85265522621645,19.2987194291774));
#51411=CARTESIAN_POINT('Ctrl Pts',(-4.21758818544739,4.15041424586946,19.3451105816513));
#51412=CARTESIAN_POINT('Ctrl Pts',(-4.90864450500983,3.44817326552251,19.3915017341253));
#51413=CARTESIAN_POINT('Ctrl Pts',(-5.42050624532396,2.56959175551903,19.4378928865993));
#51414=CARTESIAN_POINT('Ctrl Pts',(-5.69058933929046,1.6220917008281,19.4842840390733));
#51415=CARTESIAN_POINT('Ctrl Pts',(-5.84067854805978,1.09555177036103,19.5100642953139));
#51416=CARTESIAN_POINT('Ctrl Pts',(-5.91610189576638,0.547728477777345,
19.5358445515546));
#51417=CARTESIAN_POINT('Ctrl Pts',(-5.91626547054495,-5.06783466652393E-5,
19.5616248077952));
#51418=CARTESIAN_POINT('Origin',(0.,0.,0.));
#51419=CARTESIAN_POINT('',(-5.917172481729,8.05799595049797E-5,21.5633751922049));
#51420=CARTESIAN_POINT('',(-5.91705519232424,0.000118322035579633,21.3116248077952));
#51421=CARTESIAN_POINT('',(-5.91675,-7.2459289488551E-16,0.));
#51422=CARTESIAN_POINT('Ctrl Pts',(-5.917172481729,8.05799595049797E-5,
21.5633751922049));
#51423=CARTESIAN_POINT('Ctrl Pts',(-5.91722591425258,0.0799357853801551,
21.5596152902381));
#51424=CARTESIAN_POINT('Ctrl Pts',(-5.91564301057614,0.159788870386215,
21.5558553882713));
#51425=CARTESIAN_POINT('Ctrl Pts',(-5.9124100156559,0.239575092512105,21.5520954863046));
#51426=CARTESIAN_POINT('Ctrl Pts',(-5.87252005000849,1.22400894974203,21.5057043338306));
#51427=CARTESIAN_POINT('Ctrl Pts',(-5.5814268424811,2.19826387152037,21.4593131813566));
#51428=CARTESIAN_POINT('Ctrl Pts',(-5.07472163851603,3.04322012180477,21.4129220288826));
#51429=CARTESIAN_POINT('Ctrl Pts',(-4.56801643455097,3.88817637208916,21.3665308764086));
#51430=CARTESIAN_POINT('Ctrl Pts',(-3.84569923414823,4.60383395087964,21.3201397239346));
#51431=CARTESIAN_POINT('Ctrl Pts',(-2.99608597221093,5.10269117871161,21.2737485714607));
#51432=CARTESIAN_POINT('Ctrl Pts',(-2.14647271027362,5.60154840654358,21.2273574189867));
#51433=CARTESIAN_POINT('Ctrl Pts',(-1.16956338680175,5.88360528341705,21.1809662665127));
#51434=CARTESIAN_POINT('Ctrl Pts',(-0.18480228495773,5.91437541365567,21.1345751140387));
#51435=CARTESIAN_POINT('Ctrl Pts',(0.799958816886288,5.94514554389429,21.0881839615647));
#51436=CARTESIAN_POINT('Ctrl Pts',(1.79257169710246,5.72462892749805,21.0417928090907));
#51437=CARTESIAN_POINT('Ctrl Pts',(2.67167203754318,5.27978758493088,20.9954016566168));
#51438=CARTESIAN_POINT('Ctrl Pts',(3.55077237798389,4.83494624236371,20.9490105041428));
#51439=CARTESIAN_POINT('Ctrl Pts',(4.31636017864916,4.16578017362559,20.9026193516688));
#51440=CARTESIAN_POINT('Ctrl Pts',(4.87482891552365,3.35410665640716,20.8562281991948));
#51441=CARTESIAN_POINT('Ctrl Pts',(5.43329765239815,2.54243313918872,20.8098370467208));
#51442=CARTESIAN_POINT('Ctrl Pts',(5.78464732548189,1.58825217348994,20.7634458942468));
#51443=CARTESIAN_POINT('Ctrl Pts',(5.88591928054512,0.60822910246681,20.7170547417728));
#51444=CARTESIAN_POINT('Ctrl Pts',(5.98719123560835,-0.37179396855635,20.6706635892989));
#51445=CARTESIAN_POINT('Ctrl Pts',(5.83838547265108,-1.37765914490381,20.6242724368249));
#51446=CARTESIAN_POINT('Ctrl Pts',(5.45769610371606,-2.28638178300624,20.5778812843509));
#51447=CARTESIAN_POINT('Ctrl Pts',(5.07700673478105,-3.19510442110866,20.5314901318769));
#51448=CARTESIAN_POINT('Ctrl Pts',(4.4644337598683,-4.00668452096599,20.4850989794029));
#51449=CARTESIAN_POINT('Ctrl Pts',(3.6948749592683,-4.62189219406429,20.438707826929));
#51450=CARTESIAN_POINT('Ctrl Pts',(2.92531615866827,-5.23709986716261,20.392316674455));
#51451=CARTESIAN_POINT('Ctrl Pts',(1.99877153238097,-5.6559351135019,20.345925521981));
#51452=CARTESIAN_POINT('Ctrl Pts',(1.02852739679816,-5.82718798497319,20.299534369507));
#51453=CARTESIAN_POINT('Ctrl Pts',(0.0582832612154045,-5.99844085644447,
20.253143217033));
#51454=CARTESIAN_POINT('Ctrl Pts',(-0.955660383662874,-5.92211135304779,
20.206752064559));
#51455=CARTESIAN_POINT('Ctrl Pts',(-1.88933115993044,-5.60753209409417,
20.160360912085));
#51456=CARTESIAN_POINT('Ctrl Pts',(-2.82300193619803,-5.29295283514055,
20.1139697596111));
#51457=CARTESIAN_POINT('Ctrl Pts',(-3.67639984385493,-4.74012382062998,
20.0675786071371));
#51458=CARTESIAN_POINT('Ctrl Pts',(-4.34518203461083,-4.01663808480122,
20.0211874546631));
#51459=CARTESIAN_POINT('Ctrl Pts',(-5.01396422536674,-3.29315234897246,
19.9747963021891));
#51460=CARTESIAN_POINT('Ctrl Pts',(-5.49813069922166,-2.39900989182551,
19.9284051497151));
#51461=CARTESIAN_POINT('Ctrl Pts',(-5.7384836207047,-1.44353529679196,19.8820139972411));
#51462=CARTESIAN_POINT('Ctrl Pts',(-5.85702301480442,-0.972305827750752,
19.8591343955624));
#51463=CARTESIAN_POINT('Ctrl Pts',(-5.91625834738056,-0.486158218010563,
19.8362547938837));
#51464=CARTESIAN_POINT('Ctrl Pts',(-5.9162403766418,-6.30554099573244E-6,
19.8133751922049));
#51465=CARTESIAN_POINT('Ctrl Pts',(-5.91626547054495,-5.06783466652393E-5,
19.5616248077952));
#51466=CARTESIAN_POINT('Ctrl Pts',(-5.91639624592421,-0.437991218591476,
19.5822357040285));
#51467=CARTESIAN_POINT('Ctrl Pts',(-5.86842290975251,-0.875903547946226,
19.6028466002619));
#51468=CARTESIAN_POINT('Ctrl Pts',(-5.77204196744726,-1.30288911284467,
19.6234574964952));
#51469=CARTESIAN_POINT('Ctrl Pts',(-5.55510705401869,-2.26395127244807,
19.6698486489692));
#51470=CARTESIAN_POINT('Ctrl Pts',(-5.09293277954264,-3.16965699227654,
19.7162398014432));
#51471=CARTESIAN_POINT('Ctrl Pts',(-4.442028047747,-3.90926787741268,19.7626309539172));
#51472=CARTESIAN_POINT('Ctrl Pts',(-3.79112331595134,-4.64887876254883,
19.8090221063912));
#51473=CARTESIAN_POINT('Ctrl Pts',(-2.95148812683609,-5.2223948129927,19.8554132588652));
#51474=CARTESIAN_POINT('Ctrl Pts',(-2.02578259518584,-5.55969364186407,
19.9018044113391));
#51475=CARTESIAN_POINT('Ctrl Pts',(-1.10007706353559,-5.89699247073543,
19.9481955638131));
#51476=CARTESIAN_POINT('Ctrl Pts',(-0.0883011893503864,-5.99807407803428,
19.9945867162871));
#51477=CARTESIAN_POINT('Ctrl Pts',(0.885837697416628,-5.85057946601678,
20.0409778687611));
#51478=CARTESIAN_POINT('Ctrl Pts',(1.85997658418364,-5.70308485399929,20.0873690212351));
#51479=CARTESIAN_POINT('Ctrl Pts',(2.79647848353242,-5.30701402266545,20.1337601737091));
#51480=CARTESIAN_POINT('Ctrl Pts',(3.58083962795835,-4.71079357148928,20.1801513261831));
#51481=CARTESIAN_POINT('Ctrl Pts',(4.36520077238426,-4.11457312031313,20.2265424786571));
#51482=CARTESIAN_POINT('Ctrl Pts',(4.99742116188733,-3.31820304929461,20.272933631131));
#51483=CARTESIAN_POINT('Ctrl Pts',(5.400200775462,-2.4190535543971,20.319324783605));
#51484=CARTESIAN_POINT('Ctrl Pts',(5.80298038903667,-1.51990405949956,20.365715936079));
#51485=CARTESIAN_POINT('Ctrl Pts',(5.97631922668297,-0.517975140722991,
20.412107088553));
#51486=CARTESIAN_POINT('Ctrl Pts',(5.89902357808467,0.464229834826226,20.458498241027));
#51487=CARTESIAN_POINT('Ctrl Pts',(5.82172792948637,1.44643481037541,20.5048893935009));
#51488=CARTESIAN_POINT('Ctrl Pts',(5.49379779464347,2.40891584269728,20.5512805459749));
#51489=CARTESIAN_POINT('Ctrl Pts',(4.95532837885557,3.23399276004914,20.5976716984489));
#51490=CARTESIAN_POINT('Ctrl Pts',(4.41685896306763,4.05906967740105,20.6440628509229));
#51491=CARTESIAN_POINT('Ctrl Pts',(3.66785026633468,4.74674247978297,20.6904540033969));
#51492=CARTESIAN_POINT('Ctrl Pts',(2.79988172670085,5.21293111702315,20.7368451558709));
#51493=CARTESIAN_POINT('Ctrl Pts',(1.93191318706708,5.67911975426331,20.7832363083449));
#51494=CARTESIAN_POINT('Ctrl Pts',(0.944984804532506,5.92382422636172,20.8296274608188));
#51495=CARTESIAN_POINT('Ctrl Pts',(-0.0402341322062733,5.91712512365145,
20.8760186132928));
#51496=CARTESIAN_POINT('Ctrl Pts',(-1.02545306894505,5.91042602094118,20.9224097657668));
#51497=CARTESIAN_POINT('Ctrl Pts',(-2.00896255988798,5.65232334342222,20.9688009182408));
#51498=CARTESIAN_POINT('Ctrl Pts',(-2.87051133574473,5.17437466615075,21.0151920707148));
#51499=CARTESIAN_POINT('Ctrl Pts',(-3.7320601116015,4.69642598887926,21.0615832231888));
#51500=CARTESIAN_POINT('Ctrl Pts',(-4.4716481723721,3.99863131185519,21.1079743756627));
#51501=CARTESIAN_POINT('Ctrl Pts',(-4.99884791783631,3.16630826179089,21.1543655281367));
#51502=CARTESIAN_POINT('Ctrl Pts',(-5.52604766330052,2.33398521172659,21.2007566806107));
#51503=CARTESIAN_POINT('Ctrl Pts',(-5.84085909345838,1.36713378862203,21.2471478330847));
#51504=CARTESIAN_POINT('Ctrl Pts',(-5.90479099453697,0.383968521075246,
21.2935389855587));
#51505=CARTESIAN_POINT('Ctrl Pts',(-5.91309905140046,0.256204559560241,
21.2995675929709));
#51506=CARTESIAN_POINT('Ctrl Pts',(-5.91717039659536,0.128165099062277,
21.305596200383));
#51507=CARTESIAN_POINT('Ctrl Pts',(-5.91705519232424,0.000118322035579633,
21.3116248077952));
#51508=CARTESIAN_POINT('Origin',(0.,0.,0.));
#51509=CARTESIAN_POINT('',(-5.91642923825227,-0.000124498022167352,23.3133751922049));
#51510=CARTESIAN_POINT('',(-5.91655481024517,-0.00014617215624503,23.0616248077952));
#51511=CARTESIAN_POINT('',(-5.91675,-7.2459289488551E-16,0.));
#51512=CARTESIAN_POINT('Ctrl Pts',(-5.91642923825227,-0.000124498022167352,
23.3133751922049));
#51513=CARTESIAN_POINT('Ctrl Pts',(-5.9159381515581,0.645751202424775,23.2829757865926));
#51514=CARTESIAN_POINT('Ctrl Pts',(-5.81051644106084,1.29178331094863,23.2525763809803));
#51515=CARTESIAN_POINT('Ctrl Pts',(-5.60287574930939,1.90309530922156,23.222176975368));
#51516=CARTESIAN_POINT('Ctrl Pts',(-5.28600471854996,2.83599079022973,23.175785822894));
#51517=CARTESIAN_POINT('Ctrl Pts',(-4.73108176846316,3.6880285989829,23.12939467042));
#51518=CARTESIAN_POINT('Ctrl Pts',(-4.00595595360395,4.35503218311477,23.0830035179461));
#51519=CARTESIAN_POINT('Ctrl Pts',(-3.28083013874475,5.02203576724663,23.0366123654721));
#51520=CARTESIAN_POINT('Ctrl Pts',(-2.38550145911315,5.50400512675718,22.9902212129981));
#51521=CARTESIAN_POINT('Ctrl Pts',(-1.42943953462563,5.74201106190414,22.9438300605241));
#51522=CARTESIAN_POINT('Ctrl Pts',(-0.473377610138116,5.98001699705111,
22.8974389080501));
#51523=CARTESIAN_POINT('Ctrl Pts',(0.543417559205304,5.97405950783449,22.8510477555761));
#51524=CARTESIAN_POINT('Ctrl Pts',(1.49662494666533,5.724867001704,22.8046566031021));
#51525=CARTESIAN_POINT('Ctrl Pts',(2.44983233412535,5.47567449557351,22.7582654506282));
#51526=CARTESIAN_POINT('Ctrl Pts',(3.33945193970195,4.98324697252917,22.7118742981541));
#51527=CARTESIAN_POINT('Ctrl Pts',(4.05671217782192,4.30779232606351,22.6654831456802));
#51528=CARTESIAN_POINT('Ctrl Pts',(4.77397241594188,3.63233767959784,22.6190919932062));
#51529=CARTESIAN_POINT('Ctrl Pts',(5.31887328660519,2.77385590971089,22.5727008407322));
#51530=CARTESIAN_POINT('Ctrl Pts',(5.62479111008316,1.83731145593495,22.5263096882582));
#51531=CARTESIAN_POINT('Ctrl Pts',(5.93070893356112,0.900767002159047,22.4799185357843));
#51532=CARTESIAN_POINT('Ctrl Pts',(5.99764370985374,-0.11384013550589,22.4335273833102));
#51533=CARTESIAN_POINT('Ctrl Pts',(5.81741148966215,-1.08245645553395,22.3871362308363));
#51534=CARTESIAN_POINT('Ctrl Pts',(5.63717926947054,-2.05107277556205,22.3407450783623));
#51535=CARTESIAN_POINT('Ctrl Pts',(5.20978005279472,-2.97369827795332,22.2943539258883));
#51536=CARTESIAN_POINT('Ctrl Pts',(4.58747088318358,-3.73752582788711,22.2479627734143));
#51537=CARTESIAN_POINT('Ctrl Pts',(3.96516171357244,-4.5013533778209,22.2015716209404));
#51538=CARTESIAN_POINT('Ctrl Pts',(3.147942591026,-5.10638297529717,22.1551804684663));
#51539=CARTESIAN_POINT('Ctrl Pts',(2.23573287339444,-5.47863915009957,22.1087893159924));
#51540=CARTESIAN_POINT('Ctrl Pts',(1.32352315576289,-5.85089532490197,22.0623981635184));
#51541=CARTESIAN_POINT('Ctrl Pts',(0.316322843046232,-5.99037807703048,
22.0160070110444));
#51542=CARTESIAN_POINT('Ctrl Pts',(-0.662720177369385,-5.88003319588315,
21.9696158585704));
#51543=CARTESIAN_POINT('Ctrl Pts',(-1.641763197785,-5.76968831473581,21.9232247060964));
#51544=CARTESIAN_POINT('Ctrl Pts',(-2.59264892589957,-5.40951580031264,
21.8768335536224));
#51545=CARTESIAN_POINT('Ctrl Pts',(-3.39911491909419,-4.84355305379962,
21.8304424011485));
#51546=CARTESIAN_POINT('Ctrl Pts',(-4.20558091228882,-4.2775903072866,21.7840512486745));
#51547=CARTESIAN_POINT('Ctrl Pts',(-4.86762717056349,-3.50583732868374,
21.7376600962005));
#51548=CARTESIAN_POINT('Ctrl Pts',(-5.30430693781711,-2.62265444304155,
21.6912689437265));
#51549=CARTESIAN_POINT('Ctrl Pts',(-5.70559476009434,-1.81105160858726,
21.6486376932193));
#51550=CARTESIAN_POINT('Ctrl Pts',(-5.91656664271564,-0.905349214931068,
21.6060064427121));
#51551=CARTESIAN_POINT('Ctrl Pts',(-5.917172481729,8.05799595049797E-5,
21.5633751922049));
#51552=CARTESIAN_POINT('Ctrl Pts',(-5.91705519232424,0.000118322035579633,
21.3116248077952));
#51553=CARTESIAN_POINT('Ctrl Pts',(-5.91628388026723,-0.857176481624185,
21.351987352857));
#51554=CARTESIAN_POINT('Ctrl Pts',(-5.72784928662205,-1.71479925078451,
21.3923498979188));
#51555=CARTESIAN_POINT('Ctrl Pts',(-5.36680573393853,-2.49226497959308,
21.4327124429806));
#51556=CARTESIAN_POINT('Ctrl Pts',(-4.95183620026223,-3.38585410072555,
21.4791035954546));
#51557=CARTESIAN_POINT('Ctrl Pts',(-4.30884476091035,-4.17355323100148,
21.5254947479286));
#51558=CARTESIAN_POINT('Ctrl Pts',(-3.51644838647332,-4.75905234890422,
21.5718859004026));
#51559=CARTESIAN_POINT('Ctrl Pts',(-2.7240520120363,-5.34455146680696,21.6182770528766));
#51560=CARTESIAN_POINT('Ctrl Pts',(-1.78225070251412,-5.72785057233648,
21.6646682053505));
#51561=CARTESIAN_POINT('Ctrl Pts',(-0.806196171166689,-5.86208463329708,
21.7110593578245));
#51562=CARTESIAN_POINT('Ctrl Pts',(0.169858360180775,-5.99631869425769,
21.7574505102985));
#51563=CARTESIAN_POINT('Ctrl Pts',(1.18016611335355,-5.88148771064937,21.8038416627725));
#51564=CARTESIAN_POINT('Ctrl Pts',(2.10119926191803,-5.53163178239991,21.8502328152465));
#51565=CARTESIAN_POINT('Ctrl Pts',(3.02223241048248,-5.18177585415046,21.8966239677205));
#51566=CARTESIAN_POINT('Ctrl Pts',(3.85399095443862,-4.59689498125992,21.9430151201944));
#51567=CARTESIAN_POINT('Ctrl Pts',(4.49477783689496,-3.8485010992982,21.9894062726684));
#51568=CARTESIAN_POINT('Ctrl Pts',(5.13556471935129,-3.10010721733648,22.0357974251424));
#51569=CARTESIAN_POINT('Ctrl Pts',(5.58537994030777,-2.18820032630358,22.0821885776164));
#51570=CARTESIAN_POINT('Ctrl Pts',(5.78922570689681,-1.22427702295961,22.1285797300904));
#51571=CARTESIAN_POINT('Ctrl Pts',(5.99307147348585,-0.260353719615633,
22.1749708825644));
#51572=CARTESIAN_POINT('Ctrl Pts',(5.95094778570745,0.755585996039466,22.2213620350384));
#51573=CARTESIAN_POINT('Ctrl Pts',(5.66800500252533,1.69932569146983,22.2677531875123));
#51574=CARTESIAN_POINT('Ctrl Pts',(5.3850622193432,2.64306538690021,22.3141443399863));
#51575=CARTESIAN_POINT('Ctrl Pts',(4.8613003407573,3.51460506210591,22.3605354924603));
#51576=CARTESIAN_POINT('Ctrl Pts',(4.16075843429663,4.20738371981581,22.4069266449343));
#51577=CARTESIAN_POINT('Ctrl Pts',(3.46021652783598,4.90016237752569,22.4533177974083));
#51578=CARTESIAN_POINT('Ctrl Pts',(2.58289459350059,5.41418001773979,22.4997089498823));
#51579=CARTESIAN_POINT('Ctrl Pts',(1.63606061106249,5.6865889768183,22.5461001023563));
#51580=CARTESIAN_POINT('Ctrl Pts',(0.689226628624362,5.95899793589682,22.5924912548302));
#51581=CARTESIAN_POINT('Ctrl Pts',(-0.327119401916475,5.98979821383971,
22.6388824073042));
#51582=CARTESIAN_POINT('Ctrl Pts',(-1.28871136890952,5.77522393695561,22.6852735597782));
#51583=CARTESIAN_POINT('Ctrl Pts',(-2.25030333590257,5.5606496600715,22.7316647122522));
#51584=CARTESIAN_POINT('Ctrl Pts',(-3.1571412393478,5.10070082836044,22.7780558647262));
#51585=CARTESIAN_POINT('Ctrl Pts',(-3.89834825504163,4.45161424617581,22.8244470172002));
#51586=CARTESIAN_POINT('Ctrl Pts',(-4.63955527073545,3.8025276639912,22.8708381696741));
#51587=CARTESIAN_POINT('Ctrl Pts',(-5.21513139867784,2.96430333133301,22.9172293221481));
#51588=CARTESIAN_POINT('Ctrl Pts',(-5.55470237141563,2.03942886106165,22.9636204746221));
#51589=CARTESIAN_POINT('Ctrl Pts',(-5.79382430863389,1.3881429951588,22.9962885856798));
#51590=CARTESIAN_POINT('Ctrl Pts',(-5.91591570474866,0.693888947129682,
23.0289566967375));
#51591=CARTESIAN_POINT('Ctrl Pts',(-5.91655481024517,-0.00014617215624503,
23.0616248077952));
#51592=CARTESIAN_POINT('Origin',(0.,0.,0.));
#51593=CARTESIAN_POINT('',(-5.91675358287475,0.000154743843751581,25.0633751922049));
#51594=CARTESIAN_POINT('',(-5.91660456592006,0.00015087079125364,24.8116248077952));
#51595=CARTESIAN_POINT('',(-5.91675,-7.2459289488551E-16,0.));
#51596=CARTESIAN_POINT('Ctrl Pts',(-5.91675358287475,0.000154743843751581,
25.0633751922049));
#51597=CARTESIAN_POINT('Ctrl Pts',(-5.91698729620724,0.226344858207055,
25.0527274354211));
#51598=CARTESIAN_POINT('Ctrl Pts',(-5.90426631585309,0.452508838225063,
25.0420796786372));
#51599=CARTESIAN_POINT('Ctrl Pts',(-5.87838809320626,0.677157178084404,
25.0314319218534));
#51600=CARTESIAN_POINT('Ctrl Pts',(-5.7656394084893,1.65592628401005,24.9850407693794));
#51601=CARTESIAN_POINT('Ctrl Pts',(-5.40313298671896,2.60592470624721,24.9386496169054));
#51602=CARTESIAN_POINT('Ctrl Pts',(-4.83519159015146,3.41099849086875,24.8922584644314));
#51603=CARTESIAN_POINT('Ctrl Pts',(-4.26725019358391,4.21607227549036,24.8458673119574));
#51604=CARTESIAN_POINT('Ctrl Pts',(-3.49387382221916,4.87622142249632,24.7994761594835));
#51605=CARTESIAN_POINT('Ctrl Pts',(-2.60962128931955,5.31073113088118,24.7530850070095));
#51606=CARTESIAN_POINT('Ctrl Pts',(-1.72536875642002,5.74524083926599,24.7066938545355));
#51607=CARTESIAN_POINT('Ctrl Pts',(-0.730240061985659,5.95411110902974,
24.6603027020615));
#51608=CARTESIAN_POINT('Ctrl Pts',(0.254092873463193,5.91180388966308,24.6139115495875));
#51609=CARTESIAN_POINT('Ctrl Pts',(1.23842580891207,5.86949667029642,24.5675203971135));
#51610=CARTESIAN_POINT('Ctrl Pts',(2.21196298537544,5.57601196179933,24.5211292446396));
#51611=CARTESIAN_POINT('Ctrl Pts',(3.05567242375276,5.0672334125139,24.4747380921656));
#51612=CARTESIAN_POINT('Ctrl Pts',(3.89938186213007,4.55845486322847,24.4283469396916));
#51613=CARTESIAN_POINT('Ctrl Pts',(4.61326356242133,3.8343824731547,24.3819557872176));
#51614=CARTESIAN_POINT('Ctrl Pts',(5.1100329774272,2.98354677988914,24.3355646347436));
#51615=CARTESIAN_POINT('Ctrl Pts',(5.60680239243305,2.13271108662361,24.2891734822696));
#51616=CARTESIAN_POINT('Ctrl Pts',(5.88645952215352,1.1551120901663,24.2427823297956));
#51617=CARTESIAN_POINT('Ctrl Pts',(5.91481138205244,0.17027839828723,24.1963911773217));
#51618=CARTESIAN_POINT('Ctrl Pts',(5.94316324195136,-0.8145552935919,24.1500000248477));
#51619=CARTESIAN_POINT('Ctrl Pts',(5.72020983202869,-1.8066236808928,24.1036088723737));
#51620=CARTESIAN_POINT('Ctrl Pts',(5.27321111345687,-2.68462901926789,24.0572177198997));
#51621=CARTESIAN_POINT('Ctrl Pts',(4.82621239488508,-3.56263435764293,24.0108265674257));
#51622=CARTESIAN_POINT('Ctrl Pts',(4.15516836766416,-4.32657664709217,23.9644354149517));
#51623=CARTESIAN_POINT('Ctrl Pts',(3.34212592281667,-4.88305055618075,23.9180442624778));
#51624=CARTESIAN_POINT('Ctrl Pts',(2.52908347796912,-5.43952446526937,23.8716531100038));
#51625=CARTESIAN_POINT('Ctrl Pts',(1.57404261549497,-5.78852999399728,23.8252619575298));
#51626=CARTESIAN_POINT('Ctrl Pts',(0.593773815998961,-5.88739510085864,
23.7788708050558));
#51627=CARTESIAN_POINT('Ctrl Pts',(-0.386494983496995,-5.98626020772,23.7324796525818));
#51628=CARTESIAN_POINT('Ctrl Pts',(-1.39199172001481,-5.83498489271484,
23.6860885001078));
#51629=CARTESIAN_POINT('Ctrl Pts',(-2.29977679821038,-5.45206521389771,
23.6396973476339));
#51630=CARTESIAN_POINT('Ctrl Pts',(-3.20756187640595,-5.06914553508058,
23.5933061951599));
#51631=CARTESIAN_POINT('Ctrl Pts',(-4.01763529627927,-4.45458149245148,
23.5469150426859));
#51632=CARTESIAN_POINT('Ctrl Pts',(-4.63095138734598,-3.68351430921866,
23.5005238902119));
#51633=CARTESIAN_POINT('Ctrl Pts',(-5.2442674784127,-2.91244712598584,23.4541327377379));
#51634=CARTESIAN_POINT('Ctrl Pts',(-5.66082624067281,-1.9848768021493,23.4077415852639));
#51635=CARTESIAN_POINT('Ctrl Pts',(-5.82969606608683,-1.01421506359947,
23.36135043279));
#51636=CARTESIAN_POINT('Ctrl Pts',(-5.88790810343836,-0.679612968514472,
23.3453586859283));
#51637=CARTESIAN_POINT('Ctrl Pts',(-5.91668757666193,-0.339890374940268,
23.3293669390666));
#51638=CARTESIAN_POINT('Ctrl Pts',(-5.91642923825227,-0.000124498022167352,
23.3133751922049));
#51639=CARTESIAN_POINT('Ctrl Pts',(-5.91655481024517,-0.00014617215624503,
23.0616248077952));
#51640=CARTESIAN_POINT('Ctrl Pts',(-5.91682328218658,-0.291692649070739,
23.0753478492115));
#51641=CARTESIAN_POINT('Ctrl Pts',(-5.89565996578793,-0.583200493247537,
23.0890708906278));
#51642=CARTESIAN_POINT('Ctrl Pts',(-5.85273708803951,-0.871468354347098,
23.102793932044));
#51643=CARTESIAN_POINT('Ctrl Pts',(-5.70763501439238,-1.84596649159989,
23.149185084518));
#51644=CARTESIAN_POINT('Ctrl Pts',(-5.3138650495649,-2.78343815822088,23.195576236992));
#51645=CARTESIAN_POINT('Ctrl Pts',(-4.71957247178265,-3.56926101566318,
23.241967389466));
#51646=CARTESIAN_POINT('Ctrl Pts',(-4.1252798940004,-4.35508387310549,23.28835854194));
#51647=CARTESIAN_POINT('Ctrl Pts',(-3.33046470326339,-4.98925792136908,
23.334749694414));
#51648=CARTESIAN_POINT('Ctrl Pts',(-2.43230698417431,-5.39424427043108,
23.381140846888));
#51649=CARTESIAN_POINT('Ctrl Pts',(-1.53414926508527,-5.79923061949304,
23.4275319993619));
#51650=CARTESIAN_POINT('Ctrl Pts',(-0.53264901764413,-5.97502926935343,
23.4739231518359));
#51651=CARTESIAN_POINT('Ctrl Pts',(0.449742803624946,-5.90014575454956,
23.5203143043099));
#51652=CARTESIAN_POINT('Ctrl Pts',(1.43213462489411,-5.82526223974569,23.5667054567839));
#51653=CARTESIAN_POINT('Ctrl Pts',(2.39541801999124,-5.49969656027755,23.6130966092579));
#51654=CARTESIAN_POINT('Ctrl Pts',(3.22181471426473,-4.96325482534283,23.6594877617319));
#51655=CARTESIAN_POINT('Ctrl Pts',(4.04821140853817,-4.42681309040814,23.7058789142058));
#51656=CARTESIAN_POINT('Ctrl Pts',(4.73772140198794,-3.6794953000069,23.7522700666798));
#51657=CARTESIAN_POINT('Ctrl Pts',(5.20604001564117,-2.8126741492545,23.7986612191538));
#51658=CARTESIAN_POINT('Ctrl Pts',(5.67435862929443,-1.94585299850204,23.8450523716278));
#51659=CARTESIAN_POINT('Ctrl Pts',(5.92148586315112,-0.959528487398357,
23.8914435241018));
#51660=CARTESIAN_POINT('Ctrl Pts',(5.91720608246528,0.0257039292238365,
23.9378346765758));
#51661=CARTESIAN_POINT('Ctrl Pts',(5.91292630177943,1.010936345846,23.9842258290497));
#51662=CARTESIAN_POINT('Ctrl Pts',(5.6572395065511,1.99507666798671,24.0306169815237));
#51663=CARTESIAN_POINT('Ctrl Pts',(5.18140788789295,2.85779649618763,24.0770081339977));
#51664=CARTESIAN_POINT('Ctrl Pts',(4.70557626923483,3.72051632438851,24.1233992864717));
#51665=CARTESIAN_POINT('Ctrl Pts',(4.00959982714694,4.46181565864958,24.1697904389457));
#51666=CARTESIAN_POINT('Ctrl Pts',(3.17857387725964,4.99105766557993,24.2161815914197));
#51667=CARTESIAN_POINT('Ctrl Pts',(2.34754792737227,5.52029967251033,24.2625727438937));
#51668=CARTESIAN_POINT('Ctrl Pts',(1.38147246968551,5.83748435210995,24.3089638963677));
#51669=CARTESIAN_POINT('Ctrl Pts',(0.398467157427821,5.90383031927519,24.3553550488416));
#51670=CARTESIAN_POINT('Ctrl Pts',(-0.584538154829837,5.97017628644043,
24.4017462013156));
#51671=CARTESIAN_POINT('Ctrl Pts',(-1.58447332165837,5.78568354117129,24.4481373537896));
#51672=CARTESIAN_POINT('Ctrl Pts',(-2.47907874706353,5.37290955444064,24.4945285062636));
#51673=CARTESIAN_POINT('Ctrl Pts',(-3.37368417246867,4.96013556771,24.5409196587376));
#51674=CARTESIAN_POINT('Ctrl Pts',(-4.16295985645046,4.31908033951782,24.5873108112116));
#51675=CARTESIAN_POINT('Ctrl Pts',(-4.75040301617563,3.52812410471217,24.6337019636855));
#51676=CARTESIAN_POINT('Ctrl Pts',(-5.33784617590082,2.73716786990651,24.6800931161595));
#51677=CARTESIAN_POINT('Ctrl Pts',(-5.72345681136941,1.79631062848735,24.7264842686335));
#51678=CARTESIAN_POINT('Ctrl Pts',(-5.86008726534579,0.820588664846031,
24.7728754211075));
#51679=CARTESIAN_POINT('Ctrl Pts',(-5.8981286159921,0.548923159302109,24.7857918833367));
#51680=CARTESIAN_POINT('Ctrl Pts',(-5.91686888656188,0.27455492139041,24.798708345566));
#51681=CARTESIAN_POINT('Ctrl Pts',(-5.91660456592006,0.00015087079125364,
24.8116248077952));
#51682=CARTESIAN_POINT('Origin',(0.,0.,0.));
#51683=CARTESIAN_POINT('',(-5.91685813319025,-0.000149150696060474,26.8133751922049));
#51684=CARTESIAN_POINT('',(-5.91700643196177,-0.000128843304525861,26.5616248077952));
#51685=CARTESIAN_POINT('',(-5.91675,-7.2459289488551E-16,0.));
#51686=CARTESIAN_POINT('Ctrl Pts',(-5.91685813319025,-0.000149150696060474,
26.8133751922049));
#51687=CARTESIAN_POINT('Ctrl Pts',(-5.91603947382885,0.791903180632938,
26.7760879317755));
#51688=CARTESIAN_POINT('Ctrl Pts',(-5.7559669811698,1.5842763881686,26.7388006713462));
#51689=CARTESIAN_POINT('Ctrl Pts',(-5.44640144828155,2.3131579458258,26.7015134109168));
#51690=CARTESIAN_POINT('Ctrl Pts',(-5.06125376857705,3.21999999019643,26.6551222584428));
#51691=CARTESIAN_POINT('Ctrl Pts',(-4.44470236403523,4.02856184536616,26.6087311059688));
#51692=CARTESIAN_POINT('Ctrl Pts',(-3.67213144768269,4.63998265612277,26.5623399534948));
#51693=CARTESIAN_POINT('Ctrl Pts',(-2.89956053133025,5.2514034668793,26.5159488010208));
#51694=CARTESIAN_POINT('Ctrl Pts',(-1.97097010316713,5.66568323322276,26.4695576485469));
#51695=CARTESIAN_POINT('Ctrl Pts',(-0.999896614712929,5.83216899429929,
26.4231664960729));
#51696=CARTESIAN_POINT('Ctrl Pts',(-0.0288231262586201,5.99865475537583,
26.3767753435989));
#51697=CARTESIAN_POINT('Ctrl Pts',(0.984733422486779,5.91734651118538,26.3303841911249));
#51698=CARTESIAN_POINT('Ctrl Pts',(1.91684798290235,5.59818561934342,26.2839930386509));
#51699=CARTESIAN_POINT('Ctrl Pts',(2.84896254331783,5.27902472750149,26.2376018861769));
#51700=CARTESIAN_POINT('Ctrl Pts',(3.6996351154035,4.72201118800808,26.191210733703));
#51701=CARTESIAN_POINT('Ctrl Pts',(4.36485607089869,3.99524966660648,26.144819581229));
#51702=CARTESIAN_POINT('Ctrl Pts',(5.0300770263939,3.26848814520484,26.098428428755));
#51703=CARTESIAN_POINT('Ctrl Pts',(5.50984636529861,2.37197864189498,26.052037276281));
#51704=CARTESIAN_POINT('Ctrl Pts',(5.74550387894051,1.41533515297964,26.005646123807));
#51705=CARTESIAN_POINT('Ctrl Pts',(5.9811613925824,0.458691664064318,25.9592549713331));
#51706=CARTESIAN_POINT('Ctrl Pts',(5.97270708096148,-0.558085810456485,
25.9128638188591));
#51707=CARTESIAN_POINT('Ctrl Pts',(5.7211746318182,-1.51067840734559,25.8664726663851));
#51708=CARTESIAN_POINT('Ctrl Pts',(5.46964218267493,-2.46327100423464,25.8200815139111));
#51709=CARTESIAN_POINT('Ctrl Pts',(4.97503159600933,-3.35167872349201,25.7736903614371));
#51710=CARTESIAN_POINT('Ctrl Pts',(4.29781768309543,-4.06727815388284,25.7272992089631));
#51711=CARTESIAN_POINT('Ctrl Pts',(3.62060377018146,-4.78287758427373,25.6809080564892));
#51712=CARTESIAN_POINT('Ctrl Pts',(2.76078653101917,-5.32566872579805,25.6345169040152));
#51713=CARTESIAN_POINT('Ctrl Pts',(1.82349368966122,-5.62928585008312,25.5881257515412));
#51714=CARTESIAN_POINT('Ctrl Pts',(0.886200848303285,-5.93290297436818,
25.5417345990672));
#51715=CARTESIAN_POINT('Ctrl Pts',(-0.128567595250301,-5.997346081414,25.4953434465932));
#51716=CARTESIAN_POINT('Ctrl Pts',(-1.09673841700233,-5.81473587214859,
25.4489522941192));
#51717=CARTESIAN_POINT('Ctrl Pts',(-2.06490923875435,-5.63212566288317,
25.4025611416452));
#51718=CARTESIAN_POINT('Ctrl Pts',(-2.98648243870481,-5.20246213730653,
25.3561699891713));
#51719=CARTESIAN_POINT('Ctrl Pts',(-3.74877954444589,-4.57827919040816,
25.3097788366973));
#51720=CARTESIAN_POINT('Ctrl Pts',(-4.51107665018696,-3.95409624350979,
25.2633876842233));
#51721=CARTESIAN_POINT('Ctrl Pts',(-5.11409766171865,-3.1353938752897,25.2169965317493));
#51722=CARTESIAN_POINT('Ctrl Pts',(-5.48411269365271,-2.22227279637257,
25.1706053792753));
#51723=CARTESIAN_POINT('Ctrl Pts',(-5.76920140114136,-1.5187324380027,25.1348619835852));
#51724=CARTESIAN_POINT('Ctrl Pts',(-5.91596903188523,-0.759141596503511,
25.0991185878951));
#51725=CARTESIAN_POINT('Ctrl Pts',(-5.91675358287475,0.000154743843751581,
25.0633751922049));
#51726=CARTESIAN_POINT('Ctrl Pts',(-5.91660456592006,0.00015087079125364,
24.8116248077952));
#51727=CARTESIAN_POINT('Ctrl Pts',(-5.91591954463069,-0.711002882665989,
24.8450994980399));
#51728=CARTESIAN_POINT('Ctrl Pts',(-5.7875893169904,-1.42239717367699,24.8785741882847));
#51729=CARTESIAN_POINT('Ctrl Pts',(-5.53677480568972,-2.08760946190163,
24.9120488785294));
#51730=CARTESIAN_POINT('Ctrl Pts',(-5.18918161957311,-3.00949893914454,
24.9584400310034));
#51731=CARTESIAN_POINT('Ctrl Pts',(-4.60634497485573,-3.84269120776689,
25.0048311834774));
#51732=CARTESIAN_POINT('Ctrl Pts',(-3.85952686439241,-4.48531391291345,
25.0512223359514));
#51733=CARTESIAN_POINT('Ctrl Pts',(-3.11270875392911,-5.12793661806,25.0976134884254));
#51734=CARTESIAN_POINT('Ctrl Pts',(-2.20190917771993,-5.57998975973076,
25.1440046408994));
#51735=CARTESIAN_POINT('Ctrl Pts',(-1.23848934388416,-5.78620192003589,
25.1903957933733));
#51736=CARTESIAN_POINT('Ctrl Pts',(-0.275069510048367,-5.99241408034102,
25.2367869458473));
#51737=CARTESIAN_POINT('Ctrl Pts',(0.740970581413977,-5.95278525928045,
25.2831780983213));
#51738=CARTESIAN_POINT('Ctrl Pts',(1.6854022252657,-5.67216077464409,25.3295692507953));
#51739=CARTESIAN_POINT('Ctrl Pts',(2.6298338691174,-5.39153629000774,25.3759604032693));
#51740=CARTESIAN_POINT('Ctrl Pts',(3.50265706535853,-4.86991614179561,25.4223515557433));
#51741=CARTESIAN_POINT('Ctrl Pts',(4.19715388378028,-4.17107753346899,25.4687427082172));
#51742=CARTESIAN_POINT('Ctrl Pts',(4.89165070220204,-3.47223892514236,25.5151338606912));
#51743=CARTESIAN_POINT('Ctrl Pts',(5.40782114280446,-2.59618185670121,25.5615250131652));
#51744=CARTESIAN_POINT('Ctrl Pts',(5.6825543243767,-1.65001965589786,25.6079161656392));
#51745=CARTESIAN_POINT('Ctrl Pts',(5.95728750594894,-0.703857455094489,
25.6543073181132));
#51746=CARTESIAN_POINT('Ctrl Pts',(5.99058342849101,0.31240987807104,25.7006984705872));
#51747=CARTESIAN_POINT('Ctrl Pts',(5.77837108202817,1.27452585408153,25.7470896230612));
#51748=CARTESIAN_POINT('Ctrl Pts',(5.56615873556533,2.236641830092,25.7934807755351));
#51749=CARTESIAN_POINT('Ctrl Pts',(5.10843812009756,3.14460644894739,25.8398719280091));
#51750=CARTESIAN_POINT('Ctrl Pts',(4.46117360149757,3.88740512574169,25.8862630804831));
#51751=CARTESIAN_POINT('Ctrl Pts',(3.81390908289758,4.63020380253599,25.9326542329571));
#51752=CARTESIAN_POINT('Ctrl Pts',(2.97710066116534,5.20783653726923,25.9790453854311));
#51753=CARTESIAN_POINT('Ctrl Pts',(2.05306282923954,5.54967760627017,26.0254365379051));
#51754=CARTESIAN_POINT('Ctrl Pts',(1.12902499731371,5.89151867527112,26.071827690379));
#51755=CARTESIAN_POINT('Ctrl Pts',(0.117757755194285,5.99756807853976,26.118218842853));
#51756=CARTESIAN_POINT('Ctrl Pts',(-0.857093756348307,5.85485941822435,
26.164609995327));
#51757=CARTESIAN_POINT('Ctrl Pts',(-1.83194526789087,5.71215075790894,26.211001147801));
#51758=CARTESIAN_POINT('Ctrl Pts',(-2.77038104885656,5.32068403400952,26.257392300275));
#51759=CARTESIAN_POINT('Ctrl Pts',(-3.5576608808258,4.72832291318851,26.303783452749));
#51760=CARTESIAN_POINT('Ctrl Pts',(-4.34494071279503,4.13596179236749,26.350174605223));
#51761=CARTESIAN_POINT('Ctrl Pts',(-4.98106459576776,3.34270627462487,26.3965657576969));
#51762=CARTESIAN_POINT('Ctrl Pts',(-5.38825523826091,2.44554574720971,26.4429569101709));
#51763=CARTESIAN_POINT('Ctrl Pts',(-5.7354511646396,1.6805711924923,26.4825128760457));
#51764=CARTESIAN_POINT('Ctrl Pts',(-5.91620524671528,0.840054346904411,
26.5220688419204));
#51765=CARTESIAN_POINT('Ctrl Pts',(-5.91700643196177,-0.000128843304525861,
26.5616248077952));
#51766=CARTESIAN_POINT('Origin',(0.,0.,0.));
#51767=CARTESIAN_POINT('',(-5.91635914490505,0.000103511046959798,28.5633751922049));
#51768=CARTESIAN_POINT('',(-5.9162836429884,6.56326992744338E-5,28.3116248077952));
#51769=CARTESIAN_POINT('',(-5.91675,-7.2459289488551E-16,0.));
#51770=CARTESIAN_POINT('Ctrl Pts',(-5.91635914490505,0.000103511046959798,
28.5633751922049));
#51771=CARTESIAN_POINT('Ctrl Pts',(-5.91659096314501,0.372683485960868,
28.545839580604));
#51772=CARTESIAN_POINT('Ctrl Pts',(-5.88194934158775,0.745220890230166,
28.5283039690031));
#51773=CARTESIAN_POINT('Ctrl Pts',(-5.8120251919434,1.11101376516929,28.5107683574022));
#51774=CARTESIAN_POINT('Ctrl Pts',(-5.62703809473853,2.07873325060279,28.4643772049282));
#51775=CARTESIAN_POINT('Ctrl Pts',(-5.1951128511199,2.9992485910523,28.4179860524542));
#51776=CARTESIAN_POINT('Ctrl Pts',(-4.56905989073968,3.76001065597083,28.3715948999802));
#51777=CARTESIAN_POINT('Ctrl Pts',(-3.94300693035947,4.52077272088937,28.3252037475062));
#51778=CARTESIAN_POINT('Ctrl Pts',(-3.12282625321767,5.12178151027694,28.2788125950323));
#51779=CARTESIAN_POINT('Ctrl Pts',(-2.20879931910905,5.48955316816257,28.2324214425583));
#51780=CARTESIAN_POINT('Ctrl Pts',(-1.2947723850004,5.85732482604821,28.1860302900843));
#51781=CARTESIAN_POINT('Ctrl Pts',(-0.286899193924923,5.99185935243189,
28.1396391376103));
#51782=CARTESIAN_POINT('Ctrl Pts',(0.691590095561016,5.87670754401665,28.0932479851363));
#51783=CARTESIAN_POINT('Ctrl Pts',(1.6700793850469,5.76155573560141,28.0468568326623));
#51784=CARTESIAN_POINT('Ctrl Pts',(2.61918477294326,5.39671759238728,28.0004656801884));
#51785=CARTESIAN_POINT('Ctrl Pts',(3.42286149441974,4.8268009704357,27.9540745277144));
#51786=CARTESIAN_POINT('Ctrl Pts',(4.22653821589624,4.2568843484841,27.9076833752404));
#51787=CARTESIAN_POINT('Ctrl Pts',(4.88478627095287,3.48188924779502,27.8612922227664));
#51788=CARTESIAN_POINT('Ctrl Pts',(5.31712330038777,2.5965723996557,27.8149010702924));
#51789=CARTESIAN_POINT('Ctrl Pts',(5.74946032982268,1.71125555151635,27.7685099178184));
#51790=CARTESIAN_POINT('Ctrl Pts',(5.95588633363586,0.715616955926808,27.7221187653445));
#51791=CARTESIAN_POINT('Ctrl Pts',(5.91116211566127,-0.268609122241495,
27.6757276128705));
#51792=CARTESIAN_POINT('Ctrl Pts',(5.86643789768668,-1.25283520040977,27.6293364603965));
#51793=CARTESIAN_POINT('Ctrl Pts',(5.57056345792431,-2.22564876115675,27.5829453079225));
#51794=CARTESIAN_POINT('Ctrl Pts',(5.05971463123867,-3.0681063000831,27.5365541554485));
#51795=CARTESIAN_POINT('Ctrl Pts',(4.54886580455303,-3.91056383900945,27.4901630029745));
#51796=CARTESIAN_POINT('Ctrl Pts',(3.8230425909441,-4.6226653561152,27.4437718505005));
#51797=CARTESIAN_POINT('Ctrl Pts',(2.97098959686529,-5.11734396278954,27.3973806980266));
#51798=CARTESIAN_POINT('Ctrl Pts',(2.11893660278645,-5.61202256946389,27.3509895455526));
#51799=CARTESIAN_POINT('Ctrl Pts',(1.1406538282377,-5.88927826570684,27.3045983930786));
#51800=CARTESIAN_POINT('Ctrl Pts',(0.155753484842588,-5.91521168430511,
27.2582072406046));
#51801=CARTESIAN_POINT('Ctrl Pts',(-0.829146858552467,-5.94114510290338,
27.2118160881306));
#51802=CARTESIAN_POINT('Ctrl Pts',(-1.8206647707939,-5.71575624385699,27.1654249356566));
#51803=CARTESIAN_POINT('Ctrl Pts',(-2.69756981275611,-5.26660284467011,
27.1190337831827));
#51804=CARTESIAN_POINT('Ctrl Pts',(-3.57447485471833,-4.81744944548322,
27.0726426307087));
#51805=CARTESIAN_POINT('Ctrl Pts',(-4.33676702640134,-4.14453150615582,
27.0262514782347));
#51806=CARTESIAN_POINT('Ctrl Pts',(-4.89124275218217,-3.33012503630204,
26.9798603257607));
#51807=CARTESIAN_POINT('Ctrl Pts',(-5.44571847796304,-2.51571856644821,
26.9334691732867));
#51808=CARTESIAN_POINT('Ctrl Pts',(-5.79237775784171,-1.55982356606796,
26.8870780208127));
#51809=CARTESIAN_POINT('Ctrl Pts',(-5.88883542034745,-0.579314949092088,
26.8406868683387));
#51810=CARTESIAN_POINT('Ctrl Pts',(-5.90776446391498,-0.386897987630189,
26.8315829762941));
#51811=CARTESIAN_POINT('Ctrl Pts',(-5.91705801342714,-0.193533133189506,
26.8224790842495));
#51812=CARTESIAN_POINT('Ctrl Pts',(-5.91685813319025,-0.000149150696060474,
26.8133751922049));
#51813=CARTESIAN_POINT('Ctrl Pts',(-5.91700643196177,-0.000128843304525861,
26.5616248077952));
#51814=CARTESIAN_POINT('Ctrl Pts',(-5.91714487506483,-0.145310707926279,
26.5684599943944));
#51815=CARTESIAN_POINT('Ctrl Pts',(-5.91191008600676,-0.290482609897553,
26.5752951809936));
#51816=CARTESIAN_POINT('Ctrl Pts',(-5.90123235330366,-0.435253060487541,
26.5821303675929));
#51817=CARTESIAN_POINT('Ctrl Pts',(-5.82876142383966,-1.41782580368188,
26.6285215200669));
#51818=CARTESIAN_POINT('Ctrl Pts',(-5.50556216289807,-2.38190575298281,
26.6749126725408));
#51819=CARTESIAN_POINT('Ctrl Pts',(-4.97115134354497,-3.20961724102932,
26.7213038250148));
#51820=CARTESIAN_POINT('Ctrl Pts',(-4.43674052419186,-4.03732872907586,
26.7676949774888));
#51821=CARTESIAN_POINT('Ctrl Pts',(-3.69111814642719,-4.72867175586796,
26.8140861299628));
#51822=CARTESIAN_POINT('Ctrl Pts',(-2.82544961146294,-5.19911752198635,
26.8604772824368));
#51823=CARTESIAN_POINT('Ctrl Pts',(-1.95978107649869,-5.66956328810475,
26.9068684349107));
#51824=CARTESIAN_POINT('Ctrl Pts',(-0.974066384334856,-5.91911179354946,
26.9532595873847));
#51825=CARTESIAN_POINT('Ctrl Pts',(0.0111735712472701,-5.91725136069503,
26.9996507398587));
#51826=CARTESIAN_POINT('Ctrl Pts',(0.996413526829369,-5.9153909278406,27.0460418923327));
#51827=CARTESIAN_POINT('Ctrl Pts',(1.98117874582977,-5.66212155668702,27.0924330448067));
#51828=CARTESIAN_POINT('Ctrl Pts',(2.84506442419887,-5.18840986589336,27.1388241972807));
#51829=CARTESIAN_POINT('Ctrl Pts',(3.70895010256799,-4.7146981750997,27.1852153497547));
#51830=CARTESIAN_POINT('Ctrl Pts',(4.45195624030583,-4.02054416466596,27.2316065022287));
#51831=CARTESIAN_POINT('Ctrl Pts',(4.98323731738814,-3.19082032601835,27.2779976547026));
#51832=CARTESIAN_POINT('Ctrl Pts',(5.51451839447044,-2.36109648737076,27.3243888071766));
#51833=CARTESIAN_POINT('Ctrl Pts',(5.83407441089722,-1.39580282050927,27.3707799596506));
#51834=CARTESIAN_POINT('Ctrl Pts',(5.90283404408481,-0.412963391034791,
27.4171711121246));
#51835=CARTESIAN_POINT('Ctrl Pts',(5.9715936772724,0.569876038439717,27.4635622645986));
#51836=CARTESIAN_POINT('Ctrl Pts',(5.78955692722082,1.57026123052724,27.5099534170725));
#51837=CARTESIAN_POINT('Ctrl Pts',(5.3789809764512,2.46587756575986,27.5563445695465));
#51838=CARTESIAN_POINT('Ctrl Pts',(4.96840502568157,3.36149390099247,27.6027357220205));
#51839=CARTESIAN_POINT('Ctrl Pts',(4.32928987419394,4.15234137937011,27.6491268744945));
#51840=CARTESIAN_POINT('Ctrl Pts',(3.5397785484632,4.74172503865222,27.6955180269685));
#51841=CARTESIAN_POINT('Ctrl Pts',(2.75026722273249,5.3311086979343,27.7419091794425));
#51842=CARTESIAN_POINT('Ctrl Pts',(1.81035972275864,5.71902853812085,27.7883003319165));
#51843=CARTESIAN_POINT('Ctrl Pts',(0.834976210399108,5.85805456123526,27.8346914843904));
#51844=CARTESIAN_POINT('Ctrl Pts',(-0.140407301960424,5.99708058434966,
27.8810826368644));
#51845=CARTESIAN_POINT('Ctrl Pts',(-1.15126682670565,5.88721279039195,27.9274737893384));
#51846=CARTESIAN_POINT('Ctrl Pts',(-2.07400707365966,5.54188444238522,27.9738649418124));
#51847=CARTESIAN_POINT('Ctrl Pts',(-2.99674732061373,5.19655609437846,28.0202560942864));
#51848=CARTESIAN_POINT('Ctrl Pts',(-3.83136828977652,4.61576719232268,28.0666472467603));
#51849=CARTESIAN_POINT('Ctrl Pts',(-4.47582294261673,3.87052935664972,28.1130383992343));
#51850=CARTESIAN_POINT('Ctrl Pts',(-5.12027759545691,3.12529152097679,28.1594295517083));
#51851=CARTESIAN_POINT('Ctrl Pts',(-5.57456593197452,2.21560475168666,28.2058207041823));
#51852=CARTESIAN_POINT('Ctrl Pts',(-5.78314324254227,1.25269419675327,28.2522118566563));
#51853=CARTESIAN_POINT('Ctrl Pts',(-5.87218459993183,0.841629049625724,
28.2720161737026));
#51854=CARTESIAN_POINT('Ctrl Pts',(-5.9164469911479,0.420864272260875,28.2918204907489));
#51855=CARTESIAN_POINT('Ctrl Pts',(-5.9162836429884,6.56326992744338E-5,
28.3116248077952));
#51856=CARTESIAN_POINT('Origin',(0.,0.,0.));
#51857=CARTESIAN_POINT('',(-5.91722862746563,-4.93335032009101E-5,30.3133751922049));
#51858=CARTESIAN_POINT('',(-5.91726189923285,1.1977277558789E-6,30.0616248077952));
#51859=CARTESIAN_POINT('',(-5.91675,-7.2459289488551E-16,0.));
#51860=CARTESIAN_POINT('Ctrl Pts',(-5.91722862746563,-4.93335032009101E-5,
30.3133751922049));
#51861=CARTESIAN_POINT('Ctrl Pts',(-5.91681565401081,0.938144190620326,
30.2692000769585));
#51862=CARTESIAN_POINT('Ctrl Pts',(-5.68970999499436,1.87653053611386,30.225024961712));
#51863=CARTESIAN_POINT('Ctrl Pts',(-5.25996281841822,2.7104943399753,30.1808498464656));
#51864=CARTESIAN_POINT('Ctrl Pts',(-4.80865744699841,3.5862937978123,30.1344586939916));
#51865=CARTESIAN_POINT('Ctrl Pts',(-4.13386965324051,4.34693125512901,30.0880675415176));
#51866=CARTESIAN_POINT('Ctrl Pts',(-3.31810406922818,4.89940545412927,30.0416763890437));
#51867=CARTESIAN_POINT('Ctrl Pts',(-2.50233848521586,5.45187965312954,29.9952852365697));
#51868=CARTESIAN_POINT('Ctrl Pts',(-1.54559511094913,5.79619059381336,29.9488940840957));
#51869=CARTESIAN_POINT('Ctrl Pts',(-0.564852588932413,5.89024023032649,
29.9025029316217));
#51870=CARTESIAN_POINT('Ctrl Pts',(0.4158899330843,5.98428986683962,29.8561117791477));
#51871=CARTESIAN_POINT('Ctrl Pts',(1.42063160285098,5.82807819918207,29.8097206266737));
#51872=CARTESIAN_POINT('Ctrl Pts',(2.32652514516487,5.44070484101977,29.7633294741997));
#51873=CARTESIAN_POINT('Ctrl Pts',(3.23241868747876,5.05333148285746,29.7169383217258));
#51874=CARTESIAN_POINT('Ctrl Pts',(4.03946410233985,4.43479643419041,29.6705471692518));
#51875=CARTESIAN_POINT('Ctrl Pts',(4.64898594593624,3.66072644329887,29.6241560167778));
#51876=CARTESIAN_POINT('Ctrl Pts',(5.25850778953263,2.88665645240734,29.5777648643038));
#51877=CARTESIAN_POINT('Ctrl Pts',(5.6705060618643,1.95705151929134,29.5313737118298));
#51878=CARTESIAN_POINT('Ctrl Pts',(5.83460675469892,0.985572136478123,29.4849825593558));
#51879=CARTESIAN_POINT('Ctrl Pts',(5.99870744753355,0.0140927536648758,
29.4385914068819));
#51880=CARTESIAN_POINT('Ctrl Pts',(5.91491056087111,-0.999261078845656,
29.3922002544079));
#51881=CARTESIAN_POINT('Ctrl Pts',(5.59346173247772,-1.93058909804433,29.3458091019339));
#51882=CARTESIAN_POINT('Ctrl Pts',(5.27201290408436,-2.86191711724293,29.2994179494599));
#51883=CARTESIAN_POINT('Ctrl Pts',(4.71291213396012,-3.71121932312976,29.2530267969859));
#51884=CARTESIAN_POINT('Ctrl Pts',(3.98451928836737,-4.37465363872486,29.2066356445119));
#51885=CARTESIAN_POINT('Ctrl Pts',(3.25612644277459,-5.03808795432001,29.160244492038));
#51886=CARTESIAN_POINT('Ctrl Pts',(2.3584415217133,-5.51565437962341,29.113853339564));
#51887=CARTESIAN_POINT('Ctrl Pts',(1.40122223690316,-5.74896205075215,29.06746218709));
#51888=CARTESIAN_POINT('Ctrl Pts',(0.444002952092992,-5.9822697218809,29.021071034616));
#51889=CARTESIAN_POINT('Ctrl Pts',(-0.572750696465934,-5.97131863883498,
28.974679882142));
#51890=CARTESIAN_POINT('Ctrl Pts',(-1.52472275867795,-5.71744776341243,
28.928288729668));
#51891=CARTESIAN_POINT('Ctrl Pts',(-2.4766948208899,-5.46357688798989,28.8818975771941));
#51892=CARTESIAN_POINT('Ctrl Pts',(-3.36388529675494,-4.96678622019069,
28.8355064247201));
#51893=CARTESIAN_POINT('Ctrl Pts',(-4.0778196043725,-4.28781712440906,28.7891152722461));
#51894=CARTESIAN_POINT('Ctrl Pts',(-4.79175391199009,-3.60884802862741,
28.7427241197721));
#51895=CARTESIAN_POINT('Ctrl Pts',(-5.33243205136026,-2.74770050486329,
28.6963329672981));
#51896=CARTESIAN_POINT('Ctrl Pts',(-5.63374664564981,-1.80966492777249,
28.6499418148241));
#51897=CARTESIAN_POINT('Ctrl Pts',(-5.82116590832173,-1.22620186441537,
28.6210862739511));
#51898=CARTESIAN_POINT('Ctrl Pts',(-5.91597767884327,-0.612991540285919,
28.592230733078));
#51899=CARTESIAN_POINT('Ctrl Pts',(-5.91635914490505,0.000103511046959798,
28.5633751922049));
#51900=CARTESIAN_POINT('Ctrl Pts',(-5.9162836429884,6.56326992744338E-5,
28.3116248077952));
#51901=CARTESIAN_POINT('Ctrl Pts',(-5.9160643518801,-0.564846762515274,
28.3382116432229));
#51902=CARTESIAN_POINT('Ctrl Pts',(-5.83577904487672,-1.1298201856659,28.3647984786505));
#51903=CARTESIAN_POINT('Ctrl Pts',(-5.67628234379502,-1.67146859613411,
28.3913853140782));
#51904=CARTESIAN_POINT('Ctrl Pts',(-5.3979778498621,-2.61658649351127,28.4377764665522));
#51905=CARTESIAN_POINT('Ctrl Pts',(-4.87850257737835,-3.49068794768887,
28.4841676190262));
#51906=CARTESIAN_POINT('Ctrl Pts',(-4.18137148116261,-4.18689873902649,
28.5305587715002));
#51907=CARTESIAN_POINT('Ctrl Pts',(-3.48424038494692,-4.88310953036406,
28.5769499239742));
#51908=CARTESIAN_POINT('Ctrl Pts',(-2.60945346499925,-5.4014296588617,28.6233410764482));
#51909=CARTESIAN_POINT('Ctrl Pts',(-1.6639687511618,-5.67848540629442,28.6697322289221));
#51910=CARTESIAN_POINT('Ctrl Pts',(-0.718484037324299,-5.95554115372715,
28.7161233813961));
#51911=CARTESIAN_POINT('Ctrl Pts',(0.297698470402942,-5.99133252009495,
28.7625145338701));
#51912=CARTESIAN_POINT('Ctrl Pts',(1.26033265389896,-5.78148338368776,28.8089056863441));
#51913=CARTESIAN_POINT('Ctrl Pts',(2.22296683739498,-5.57163424728057,28.8552968388181));
#51914=CARTESIAN_POINT('Ctrl Pts',(3.13205269665974,-5.11614460809836,28.9016879912921));
#51915=CARTESIAN_POINT('Ctrl Pts',(3.87643855549968,-4.47070605606958,28.9480791437661));
#51916=CARTESIAN_POINT('Ctrl Pts',(4.62082441433958,-3.82526750404082,28.99447029624));
#51917=CARTESIAN_POINT('Ctrl Pts',(5.20051027275471,-2.98988003916548,29.040861448714));
#51918=CARTESIAN_POINT('Ctrl Pts',(5.54461937672687,-2.06668441750707,29.087252601188));
#51919=CARTESIAN_POINT('Ctrl Pts',(5.88872848069905,-1.14348879584861,29.133643753662));
#51920=CARTESIAN_POINT('Ctrl Pts',(5.99726083022826,-0.132485017407117,
29.180034906136));
#51921=CARTESIAN_POINT('Ctrl Pts',(5.85694644377375,0.842713990098421,29.22642605861));
#51922=CARTESIAN_POINT('Ctrl Pts',(5.71663205731926,1.8179129976039,29.2728172110839));
#51923=CARTESIAN_POINT('Ctrl Pts',(5.32747093488102,2.75730723417347,29.3192083635579));
#51924=CARTESIAN_POINT('Ctrl Pts',(4.73704484294192,3.54603929339467,29.3655995160319));
#51925=CARTESIAN_POINT('Ctrl Pts',(4.1466187510028,4.33477135261589,29.4119906685059));
#51926=CARTESIAN_POINT('Ctrl Pts',(3.35492768956284,4.97284123448879,29.4583818209799));
#51927=CARTESIAN_POINT('Ctrl Pts',(2.45876976367401,5.38223371506516,29.5047729734539));
#51928=CARTESIAN_POINT('Ctrl Pts',(1.56261183778516,5.79162619564153,29.5511641259278));
#51929=CARTESIAN_POINT('Ctrl Pts',(0.561987047447457,5.97234127492132,29.5975552784018));
#51930=CARTESIAN_POINT('Ctrl Pts',(-0.420760692786501,5.90228336779483,
29.6439464308758));
#51931=CARTESIAN_POINT('Ctrl Pts',(-1.40350843302046,5.83222546066834,29.6903375833498));
#51932=CARTESIAN_POINT('Ctrl Pts',(-2.36837912315064,5.51139456713559,29.7367287358238));
#51933=CARTESIAN_POINT('Ctrl Pts',(-3.19740041389354,4.97901788584606,29.7831198882978));
#51934=CARTESIAN_POINT('Ctrl Pts',(-4.02642170463643,4.44664120455655,29.8295110407718));
#51935=CARTESIAN_POINT('Ctrl Pts',(-4.71959359599201,3.70271873551026,29.8759021932458));
#51936=CARTESIAN_POINT('Ctrl Pts',(-5.19216367780099,2.83820803629081,29.9222933457197));
#51937=CARTESIAN_POINT('Ctrl Pts',(-5.66527027191213,1.97271585169314,29.9687371664116));
#51938=CARTESIAN_POINT('Ctrl Pts',(-5.91727379117156,0.986361472032727,
30.0151809871034));
#51939=CARTESIAN_POINT('Ctrl Pts',(-5.91726188962992,1.19770528722231E-6,
30.0616248077952));
#51940=CARTESIAN_POINT('Origin',(0.,0.,0.));
#51941=CARTESIAN_POINT('',(-5.91624577020395,-2.44117356945628E-5,32.0633751922049));
#51942=CARTESIAN_POINT('',(-5.91628636364003,-6.75382191168991E-5,31.8116248077952));
#51943=CARTESIAN_POINT('',(-5.91675,-7.2459289488551E-16,0.));
#51944=CARTESIAN_POINT('Ctrl Pts',(-5.91624577020395,-2.44117356945628E-5,
32.0633751922049));
#51945=CARTESIAN_POINT('Ctrl Pts',(-5.91617142152926,0.518930599746724,
32.038951725787));
#51946=CARTESIAN_POINT('Ctrl Pts',(-5.84857166224644,1.03790461430612,32.014528259369));
#51947=CARTESIAN_POINT('Ctrl Pts',(-5.71368641895957,1.53875791597551,31.990104792951));
#51948=CARTESIAN_POINT('Ctrl Pts',(-5.4574786480919,2.49010370314597,31.943713640477));
#51949=CARTESIAN_POINT('Ctrl Pts',(-4.95851089479277,3.37607158588524,31.897322488003));
#51950=CARTESIAN_POINT('Ctrl Pts',(-4.27779071030773,4.08833646572602,31.850931335529));
#51951=CARTESIAN_POINT('Ctrl Pts',(-3.59707052582268,4.80060134556683,31.804540183055));
#51952=CARTESIAN_POINT('Ctrl Pts',(-2.73459791015171,5.33916322250914,31.7581490305811));
#51953=CARTESIAN_POINT('Ctrl Pts',(-1.79582525365581,5.63817346988476,31.7117578781071));
#51954=CARTESIAN_POINT('Ctrl Pts',(-0.857052597159934,5.93718371726037,
31.6653667256331));
#51955=CARTESIAN_POINT('Ctrl Pts',(0.158020100160874,5.9966423350693,31.6189755731591));
#51956=CARTESIAN_POINT('Ctrl Pts',(1.12528241395491,5.80927946539191,31.5725844206851));
#51957=CARTESIAN_POINT('Ctrl Pts',(2.09254472774896,5.62191659571452,31.5261932682111));
#51958=CARTESIAN_POINT('Ctrl Pts',(3.01199665801623,5.1877322385508,31.4798021157372));
#51959=CARTESIAN_POINT('Ctrl Pts',(3.77121909473866,4.55981303977025,31.4334109632632));
#51960=CARTESIAN_POINT('Ctrl Pts',(4.53044153146111,3.93189384098969,31.3870198107892));
#51961=CARTESIAN_POINT('Ctrl Pts',(5.12943447463871,3.11023980059227,31.3406286583152));
#51962=CARTESIAN_POINT('Ctrl Pts',(5.49496054082328,2.1953125228485,31.2942375058412));
#51963=CARTESIAN_POINT('Ctrl Pts',(5.86048660700783,1.28038524510478,31.2478463533672));
#51964=CARTESIAN_POINT('Ctrl Pts',(5.99254579619939,0.272184730014703,31.2014552008933));
#51965=CARTESIAN_POINT('Ctrl Pts',(5.87499155844803,-0.706018842768892,
31.1550640484193));
#51966=CARTESIAN_POINT('Ctrl Pts',(5.75743732069666,-1.68422241555252,31.1086728959453));
#51967=CARTESIAN_POINT('Ctrl Pts',(5.39026965600235,-2.63242904602966,31.0622817434713));
#51968=CARTESIAN_POINT('Ctrl Pts',(4.81838124524767,-3.43470385821338,31.0158905909973));
#51969=CARTESIAN_POINT('Ctrl Pts',(4.246492834493,-4.23697867039708,30.9694994385233));
#51970=CARTESIAN_POINT('Ctrl Pts',(3.46988367767797,-4.89332166428738,30.9231082860494));
#51971=CARTESIAN_POINT('Ctrl Pts',(2.58350785273426,-5.32348340779237,30.8767171335754));
#51972=CARTESIAN_POINT('Ctrl Pts',(1.6971320277905,-5.75364515129739,30.8303259811014));
#51973=CARTESIAN_POINT('Ctrl Pts',(0.700989534718055,-5.95762564441709,
30.7839348286274));
#51974=CARTESIAN_POINT('Ctrl Pts',(-0.283123751314443,-5.91048469752033,
30.7375436761534));
#51975=CARTESIAN_POINT('Ctrl Pts',(-1.26723703734694,-5.86334375062357,
30.6911525236794));
#51976=CARTESIAN_POINT('Ctrl Pts',(-2.23932111633949,-5.56508136371036,
30.6447613712054));
#51977=CARTESIAN_POINT('Ctrl Pts',(-3.08052167581995,-5.05216534002835,
30.5983702187315));
#51978=CARTESIAN_POINT('Ctrl Pts',(-3.92172223530036,-4.53924931634636,
30.5519790662575));
#51979=CARTESIAN_POINT('Ctrl Pts',(-4.6320392752687,-3.8116796558956,30.5055879137835));
#51980=CARTESIAN_POINT('Ctrl Pts',(-5.1246240907136,-2.95841449885882,30.4591967613095));
#51981=CARTESIAN_POINT('Ctrl Pts',(-5.61720890615852,-2.10514934182202,
30.4128056088355));
#51982=CARTESIAN_POINT('Ctrl Pts',(-5.89206149707999,-1.12618868819918,
30.3664144563616));
#51983=CARTESIAN_POINT('Ctrl Pts',(-5.91557631799987,-0.141227632209123,
30.3200233038876));
#51984=CARTESIAN_POINT('Ctrl Pts',(-5.91669958646333,-0.0941774889952961,
30.31780726666));
#51985=CARTESIAN_POINT('Ctrl Pts',(-5.91724934420955,-0.047113653867736,
30.3155912294325));
#51986=CARTESIAN_POINT('Ctrl Pts',(-5.91722862746563,-4.93335032009101E-5,
30.3133751922049));
#51987=CARTESIAN_POINT('Ctrl Pts',(-5.91726188962992,1.19770528722231E-6,
30.0616248077952));
#51988=CARTESIAN_POINT('Ctrl Pts',(-5.91725001508146,-0.984121972222739,
30.1079632920513));
#51989=CARTESIAN_POINT('Ctrl Pts',(-5.66643406602473,-1.96825097069318,
30.1543017763075));
#51990=CARTESIAN_POINT('Ctrl Pts',(-5.19538055793008,-2.83231519655277,
30.2006402605636));
#51991=CARTESIAN_POINT('Ctrl Pts',(-4.72379165146888,-3.69736151588404,
30.2470314130376));
#51992=CARTESIAN_POINT('Ctrl Pts',(-4.03146425841823,-4.44206997679278,
30.2934225655116));
#51993=CARTESIAN_POINT('Ctrl Pts',(-3.20304753422148,-4.97538692041728,
30.3398137179856));
#51994=CARTESIAN_POINT('Ctrl Pts',(-2.3746308100247,-5.50870386404179,30.3862048704596));
#51995=CARTESIAN_POINT('Ctrl Pts',(-1.41012475468182,-5.83062929038205,
30.4325960229335));
#51996=CARTESIAN_POINT('Ctrl Pts',(-0.427457134484195,-5.90180217497335,
30.4789871754075));
#51997=CARTESIAN_POINT('Ctrl Pts',(0.555210485713345,-5.97297505956465,
30.5253783278815));
#51998=CARTESIAN_POINT('Ctrl Pts',(1.55603967076562,-5.79339540240703,30.5717694803555));
#51999=CARTESIAN_POINT('Ctrl Pts',(2.45266151528465,-5.38501996335977,30.6181606328295));
#52000=CARTESIAN_POINT('Ctrl Pts',(3.34928335980375,-4.97664452431247,30.6645517853035));
#52001=CARTESIAN_POINT('Ctrl Pts',(4.14169786378957,-4.33947330337547,30.7109429377774));
#52002=CARTESIAN_POINT('Ctrl Pts',(4.73301846866193,-3.55141164745045,30.7573340902514));
#52003=CARTESIAN_POINT('Ctrl Pts',(5.32433907353427,-2.76334999152544,30.8037252427254));
#52004=CARTESIAN_POINT('Ctrl Pts',(5.71456577929316,-1.82439790061242,30.8501163951994));
#52005=CARTESIAN_POINT('Ctrl Pts',(5.85598653322264,-0.849358721069426,
30.8965075476734));
#52006=CARTESIAN_POINT('Ctrl Pts',(5.99740728715212,0.125680458473537,30.9428987001474));
#52007=CARTESIAN_POINT('Ctrl Pts',(5.89002208925218,1.13680672664654,30.9892898526213));
#52008=CARTESIAN_POINT('Ctrl Pts',(5.54696066167538,2.06039217921429,31.0356810050953));
#52009=CARTESIAN_POINT('Ctrl Pts',(5.20389923409858,2.98397763178207,31.0820721575693));
#52010=CARTESIAN_POINT('Ctrl Pts',(4.62516157684496,3.82002226874459,31.1284633100433));
#52011=CARTESIAN_POINT('Ctrl Pts',(3.8815085097253,4.46630498323522,31.1748544625173));
#52012=CARTESIAN_POINT('Ctrl Pts',(3.13785544260559,5.11258769772589,31.2212456149913));
#52013=CARTESIAN_POINT('Ctrl Pts',(2.2292869656198,5.56910848974459,31.2676367674653));
#52014=CARTESIAN_POINT('Ctrl Pts',(1.26689149591189,5.78004969285972,31.3140279199392));
#52015=CARTESIAN_POINT('Ctrl Pts',(0.304496026204034,5.99099089597484,31.3604190724132));
#52016=CARTESIAN_POINT('Ctrl Pts',(-0.711726436225908,5.95635251018647,
31.4068102248872));
#52017=CARTESIAN_POINT('Ctrl Pts',(-1.6575248880945,5.68036968512516,31.4532013773612));
#52018=CARTESIAN_POINT('Ctrl Pts',(-2.6033233399631,5.40438686006385,31.4995925298352));
#52019=CARTESIAN_POINT('Ctrl Pts',(-3.47869778127026,4.88705959572961,31.5459836823092));
#52020=CARTESIAN_POINT('Ctrl Pts',(-4.17661834739248,4.19164021530547,31.5923748347831));
#52021=CARTESIAN_POINT('Ctrl Pts',(-4.87453891351471,3.49622083488134,31.6387659872571));
#52022=CARTESIAN_POINT('Ctrl Pts',(-5.39500560445199,2.62270933836731,31.6851571397311));
#52023=CARTESIAN_POINT('Ctrl Pts',(-5.67438224710694,1.67790781274158,31.7315482922051));
#52024=CARTESIAN_POINT('Ctrl Pts',(-5.83512775487457,1.13429543508152,31.7582404640685));
#52025=CARTESIAN_POINT('Ctrl Pts',(-5.9160596836837,0.567082280831977,31.7849326359318));
#52026=CARTESIAN_POINT('Ctrl Pts',(-5.91628636364003,-6.75382191168991E-5,
31.8116248077952));
#52027=CARTESIAN_POINT('Origin',(0.,0.,0.));
#52028=CARTESIAN_POINT('',(-5.91712951644955,9.70841563171718E-5,33.8133751922049));
#52029=CARTESIAN_POINT('',(-5.91699986415359,0.000130094215637797,33.5616248077952));
#52030=CARTESIAN_POINT('',(-5.91675,-7.2459289488551E-16,0.));
#52031=CARTESIAN_POINT('Ctrl Pts',(-5.91712951644955,9.70841563171718E-5,
33.8133751922049));
#52032=CARTESIAN_POINT('Ctrl Pts',(-5.91720654989048,0.0993222265836009,
33.8087033746154));
#52033=CARTESIAN_POINT('Ctrl Pts',(-5.91476231278835,0.198543573571387,
33.8040315570259));
#52034=CARTESIAN_POINT('Ctrl Pts',(-5.90977163932508,0.297636673159239,
33.7993597394364));
#52035=CARTESIAN_POINT('Ctrl Pts',(-5.86021424776472,1.28163123288083,33.7529685869624));
#52036=CARTESIAN_POINT('Ctrl Pts',(-5.55956571221439,2.2529799684796,33.7065774344884));
#52037=CARTESIAN_POINT('Ctrl Pts',(-5.04458558440507,3.09291847609872,33.6601862820144));
#52038=CARTESIAN_POINT('Ctrl Pts',(-4.52960545659575,3.93285698371785,33.6137951295404));
#52039=CARTESIAN_POINT('Ctrl Pts',(-3.80029373652743,4.64138526335733,33.5674039770665));
#52040=CARTESIAN_POINT('Ctrl Pts',(-2.94582156169723,5.13187331730042,33.5210128245925));
#52041=CARTESIAN_POINT('Ctrl Pts',(-2.09134938686702,5.62236137124351,33.4746216721185));
#52042=CARTESIAN_POINT('Ctrl Pts',(-1.11171675727491,5.89480919949021,33.4282305196445));
#52043=CARTESIAN_POINT('Ctrl Pts',(-0.126700927976976,5.915905280938,33.3818393671705));
#52044=CARTESIAN_POINT('Ctrl Pts',(0.858314901320957,5.93700136238578,33.3354482146965));
#52045=CARTESIAN_POINT('Ctrl Pts',(1.84871393032473,5.70674569703466,33.2890570622226));
#52046=CARTESIAN_POINT('Ctrl Pts',(2.72340252299071,5.25329107474049,33.2426659097486));
#52047=CARTESIAN_POINT('Ctrl Pts',(3.5980911156567,4.79983645244633,33.1962747572746));
#52048=CARTESIAN_POINT('Ctrl Pts',(4.35706927198491,4.12318287320913,33.1498836048006));
#52049=CARTESIAN_POINT('Ctrl Pts',(4.90753861280094,3.30606309408155,33.1034924523266));
#52050=CARTESIAN_POINT('Ctrl Pts',(5.45800795361698,2.48894331495397,33.0571012998526));
#52051=CARTESIAN_POINT('Ctrl Pts',(5.79996847892084,1.53135733593599,33.0107101473786));
#52052=CARTESIAN_POINT('Ctrl Pts',(5.89160952232476,0.550386822727887,32.9643189949047));
#52053=CARTESIAN_POINT('Ctrl Pts',(5.98325056572869,-0.430583690480249,
32.9179278424307));
#52054=CARTESIAN_POINT('Ctrl Pts',(5.8245721272327,-1.43493873787846,32.8715366899567));
#52055=CARTESIAN_POINT('Ctrl Pts',(5.43497542646289,-2.33987831562345,32.8251455374827));
#52056=CARTESIAN_POINT('Ctrl Pts',(5.04537872569309,-3.24481789336841,32.7787543850087));
#52057=CARTESIAN_POINT('Ctrl Pts',(4.42486376264948,-4.05034200146009,32.7323632325347));
#52058=CARTESIAN_POINT('Ctrl Pts',(3.6492993648389,-4.65796120249694,32.6859720800608));
#52059=CARTESIAN_POINT('Ctrl Pts',(2.87373496702833,-5.26558040353378,32.6395809275868));
#52060=CARTESIAN_POINT('Ctrl Pts',(1.94312113445076,-5.67529469751581,32.5931897751128));
#52061=CARTESIAN_POINT('Ctrl Pts',(0.971241715271586,-5.83700933258605,
32.5467986226388));
#52062=CARTESIAN_POINT('Ctrl Pts',(-0.000637703907585968,-5.99872396765628,
32.5004074701648));
#52063=CARTESIAN_POINT('Ctrl Pts',(-1.01378270968838,-5.91243894381474,
32.4540163176908));
#52064=CARTESIAN_POINT('Ctrl Pts',(-1.94431857178876,-5.58870411719726,
32.4076251652168));
#52065=CARTESIAN_POINT('Ctrl Pts',(-2.87485443388914,-5.26496929057979,
32.3612340127429));
#52066=CARTESIAN_POINT('Ctrl Pts',(-3.72278115230912,-4.70378466118638,
32.3148428602689));
#52067=CARTESIAN_POINT('Ctrl Pts',(-4.38442482751419,-3.97376488359055,
32.2684517077949));
#52068=CARTESIAN_POINT('Ctrl Pts',(-5.04606850271927,-3.24374510599472,
32.2220605553209));
#52069=CARTESIAN_POINT('Ctrl Pts',(-5.52142913470946,-2.34489018019647,
32.1756694028469));
#52070=CARTESIAN_POINT('Ctrl Pts',(-5.75238555648645,-1.38710087149652,
32.1292782503729));
#52071=CARTESIAN_POINT('Ctrl Pts',(-5.86175076721409,-0.93355717363047,
32.1073105643169));
#52072=CARTESIAN_POINT('Ctrl Pts',(-5.91631264311692,-0.466798479525038,
32.0853428782609));
#52073=CARTESIAN_POINT('Ctrl Pts',(-5.91624577020395,-2.44117356945628E-5,
32.0633751922049));
#52074=CARTESIAN_POINT('Ctrl Pts',(-5.91628636364003,-6.75382191168991E-5,
31.8116248077952));
#52075=CARTESIAN_POINT('Ctrl Pts',(-5.91645365478769,-0.418627457059442,
31.8313237884058));
#52076=CARTESIAN_POINT('Ctrl Pts',(-5.87266461226124,-0.837152880211372,
31.8510227690164));
#52077=CARTESIAN_POINT('Ctrl Pts',(-5.78456082316728,-1.2461318539464,31.870721749627));
#52078=CARTESIAN_POINT('Ctrl Pts',(-5.57707616220006,-2.20927844027123,
31.917112902101));
#52079=CARTESIAN_POINT('Ctrl Pts',(-5.12382024589301,-3.11948005818347,
31.963504054575));
#52080=CARTESIAN_POINT('Ctrl Pts',(-4.48021155241156,-3.86544861044351,
32.009895207049));
#52081=CARTESIAN_POINT('Ctrl Pts',(-3.83660285893011,-4.61141716270354,
32.056286359523));
#52082=CARTESIAN_POINT('Ctrl Pts',(-3.00264138827423,-5.1931526493114,32.102677511997));
#52083=CARTESIAN_POINT('Ctrl Pts',(-2.08029354372645,-5.53952771328672,
32.1490686644709));
#52084=CARTESIAN_POINT('Ctrl Pts',(-1.15794569917867,-5.88590277726204,
32.1954598169449));
#52085=CARTESIAN_POINT('Ctrl Pts',(-0.147211480738965,-5.99691741860484,
32.2418509694189));
#52086=CARTESIAN_POINT('Ctrl Pts',(0.828329142307269,-5.85899815210298,
32.2882421218929));
#52087=CARTESIAN_POINT('Ctrl Pts',(1.8038697653535,-5.72107888560113,32.3346332743669));
#52088=CARTESIAN_POINT('Ctrl Pts',(2.74421679300629,-5.33422571125461,32.3810244268409));
#52089=CARTESIAN_POINT('Ctrl Pts',(3.53439632344765,-4.74573820844991,32.4274155793149));
#52090=CARTESIAN_POINT('Ctrl Pts',(4.32457585388903,-4.15725070564519,32.4738067317888));
#52091=CARTESIAN_POINT('Ctrl Pts',(4.96458788711896,-3.36712887438234,32.5201978842628));
#52092=CARTESIAN_POINT('Ctrl Pts',(5.37617973715353,-2.47197895382655,32.5665890367368));
#52093=CARTESIAN_POINT('Ctrl Pts',(5.78777158718809,-1.57682903327079,32.6129801892108));
#52094=CARTESIAN_POINT('Ctrl Pts',(5.97094325402726,-0.576651023422171,
32.6593713416848));
#52095=CARTESIAN_POINT('Ctrl Pts',(5.90329879168547,0.406265787910474,32.7057624941588));
#52096=CARTESIAN_POINT('Ctrl Pts',(5.83565432934368,1.38918259924312,32.7521536466327));
#52097=CARTESIAN_POINT('Ctrl Pts',(5.51719373782093,2.3548382120598,32.7985447991067));
#52098=CARTESIAN_POINT('Ctrl Pts',(4.98685440481123,3.18516430652431,32.8449359515807));
#52099=CARTESIAN_POINT('Ctrl Pts',(4.45651507180153,4.01549040098881,32.8913271040547));
#52100=CARTESIAN_POINT('Ctrl Pts',(3.71429699730487,4.71048697710115,32.9377182565287));
#52101=CARTESIAN_POINT('Ctrl Pts',(2.8509493468051,5.18517852501659,32.9841094090027));
#52102=CARTESIAN_POINT('Ctrl Pts',(1.98760169630535,5.65987007293202,33.0305005614767));
#52103=CARTESIAN_POINT('Ctrl Pts',(1.00312446980238,5.9142565926506,33.0768917139506));
#52104=CARTESIAN_POINT('Ctrl Pts',(0.0178872592165909,5.91723487452538,
33.1232828664246));
#52105=CARTESIAN_POINT('Ctrl Pts',(-0.967349951369257,5.92021315640015,
33.1696740188986));
#52106=CARTESIAN_POINT('Ctrl Pts',(-1.95334714603794,5.67178320043115,33.2160651713726));
#52107=CARTESIAN_POINT('Ctrl Pts',(-2.81954889012674,5.20231992197007,33.2624563238466));
#52108=CARTESIAN_POINT('Ctrl Pts',(-3.68575063421552,4.73285664350901,33.3088474763206));
#52109=CARTESIAN_POINT('Ctrl Pts',(-4.43215692772435,4.0423600425559,33.3552386287945));
#52110=CARTESIAN_POINT('Ctrl Pts',(-4.96750652200506,3.21525542813924,33.4016297812685));
#52111=CARTESIAN_POINT('Ctrl Pts',(-5.50285611628576,2.38815081372258,33.4480209337425));
#52112=CARTESIAN_POINT('Ctrl Pts',(-5.82714901133836,1.42443818584236,33.4944120862165));
#52113=CARTESIAN_POINT('Ctrl Pts',(-5.90073471816293,0.441948300379427,
33.5408032386905));
#52114=CARTESIAN_POINT('Ctrl Pts',(-5.91174378489267,0.294959201855924,
33.5477437617254));
#52115=CARTESIAN_POINT('Ctrl Pts',(-5.91714132713061,0.147549816058014,
33.5546842847603));
#52116=CARTESIAN_POINT('Ctrl Pts',(-5.91699986415359,0.000130094215637797,
33.5616248077952));
#52117=CARTESIAN_POINT('Origin',(0.,0.,0.));
#52118=CARTESIAN_POINT('',(-5.91647681799755,-0.000134629570711919,35.5633751922049));
#52119=CARTESIAN_POINT('',(-5.91661122068025,-0.000151359735457047,35.3116248077952));
#52120=CARTESIAN_POINT('',(-5.91675,-7.2459289488551E-16,0.));
#52121=CARTESIAN_POINT('Ctrl Pts',(-5.91647681799755,-0.000134629570711919,
35.5633751922049));
#52122=CARTESIAN_POINT('Ctrl Pts',(-5.91592360889482,0.665100593798877,
35.5320638709699));
#52123=CARTESIAN_POINT('Ctrl Pts',(-5.80395651976011,1.33051735339803,35.5007525497348));
#52124=CARTESIAN_POINT('Ctrl Pts',(-5.58391280219011,1.95803632134791,35.4694412284998));
#52125=CARTESIAN_POINT('Ctrl Pts',(-5.25789392946026,2.88777441524527,35.4230500760258));
#52126=CARTESIAN_POINT('Ctrl Pts',(-4.69462882472502,3.73432053322438,35.3766589235518));
#52127=CARTESIAN_POINT('Ctrl Pts',(-3.96298651712459,4.39416957834686,35.3302677710778));
#52128=CARTESIAN_POINT('Ctrl Pts',(-3.23134420952415,5.05401862346935,35.2838766186039));
#52129=CARTESIAN_POINT('Ctrl Pts',(-2.33132469905851,5.52717059573522,35.2374854661299));
#52130=CARTESIAN_POINT('Ctrl Pts',(-1.37297114191099,5.75577437549979,35.1910943136559));
#52131=CARTESIAN_POINT('Ctrl Pts',(-0.414617584763474,5.98437815526435,
35.1447031611819));
#52132=CARTESIAN_POINT('Ctrl Pts',(0.602070019065926,5.96843374252761,35.0983120087079));
#52133=CARTESIAN_POINT('Ctrl Pts',(1.55278379460685,5.70989062114036,35.0519208562339));
#52134=CARTESIAN_POINT('Ctrl Pts',(2.50349757014778,5.4513474997531,35.0055297037599));
#52135=CARTESIAN_POINT('Ctrl Pts',(3.38823751740023,4.95020566971533,34.959138551286));
#52136=CARTESIAN_POINT('Ctrl Pts',(4.09882867452727,4.2677385012502,34.912747398812));
#52137=CARTESIAN_POINT('Ctrl Pts',(4.80941983165431,3.58527133278508,34.866356246338));
#52138=CARTESIAN_POINT('Ctrl Pts',(5.34586219865593,2.72147882589261,34.819965093864));
#52139=CARTESIAN_POINT('Ctrl Pts',(5.64256629609434,1.78197475076402,34.77357394139));
#52140=CARTESIAN_POINT('Ctrl Pts',(5.93927039353275,0.842470675635441,34.7271827889161));
#52141=CARTESIAN_POINT('Ctrl Pts',(5.99623622140793,-0.172744967729249,
34.6807916364421));
#52142=CARTESIAN_POINT('Ctrl Pts',(5.80649870905078,-1.13954427731964,34.6344004839681));
#52143=CARTESIAN_POINT('Ctrl Pts',(5.61676119669363,-2.10634358691004,34.5880093314941));
#52144=CARTESIAN_POINT('Ctrl Pts',(5.18032034410413,-3.02472656272614,34.5416181790201));
#52145=CARTESIAN_POINT('Ctrl Pts',(4.55053869325812,-3.7824047931628,34.4952270265461));
#52146=CARTESIAN_POINT('Ctrl Pts',(3.92075704241212,-4.54008302359946,34.4488358740721));
#52147=CARTESIAN_POINT('Ctrl Pts',(3.0976345933096,-5.13705650865668,34.4024447215982));
#52148=CARTESIAN_POINT('Ctrl Pts',(2.18181248891615,-5.50033477902844,34.3560535691242));
#52149=CARTESIAN_POINT('Ctrl Pts',(1.2659903845227,-5.86361304940021,34.3096624166502));
#52150=CARTESIAN_POINT('Ctrl Pts',(0.257468624838311,-5.99319610508651,
34.2632712641762));
#52151=CARTESIAN_POINT('Ctrl Pts',(-0.720443332703347,-5.8732401468477,
34.2168801117022));
#52152=CARTESIAN_POINT('Ctrl Pts',(-1.69835529024501,-5.75328418860889,
34.1704889592282));
#52153=CARTESIAN_POINT('Ctrl Pts',(-2.64565744564394,-5.38378921644496,
34.1240978067543));
#52154=CARTESIAN_POINT('Ctrl Pts',(-3.44652551084063,-4.80993246535802,
34.0777066542803));
#52155=CARTESIAN_POINT('Ctrl Pts',(-4.24739357603731,-4.23607571427107,
34.0313155018063));
#52156=CARTESIAN_POINT('Ctrl Pts',(-4.90182755103176,-3.45785718426112,
33.9849243493323));
#52157=CARTESIAN_POINT('Ctrl Pts',(-5.32981141474379,-2.57042772733394,
33.9385331968583));
#52158=CARTESIAN_POINT('Ctrl Pts',(-5.71469519501551,-1.77236678843735,
33.8968138619738));
#52159=CARTESIAN_POINT('Ctrl Pts',(-5.91644160775919,-0.88598351864123,
33.8550945270894));
#52160=CARTESIAN_POINT('Ctrl Pts',(-5.91712951644955,9.70841563171718E-5,
33.8133751922049));
#52161=CARTESIAN_POINT('Ctrl Pts',(-5.91699986415359,0.000130094215637797,
33.5616248077952));
#52162=CARTESIAN_POINT('Ctrl Pts',(-5.91619577439583,-0.837818398883012,
33.6010754372343));
#52163=CARTESIAN_POINT('Ctrl Pts',(-5.73643198268786,-1.67610083920967,
33.6405260666734));
#52164=CARTESIAN_POINT('Ctrl Pts',(-5.39102647875133,-2.43943067533054,
33.6799766961124));
#52165=CARTESIAN_POINT('Ctrl Pts',(-4.98485401391861,-3.33705262253189,
33.7263678485864));
#52166=CARTESIAN_POINT('Ctrl Pts',(-4.34963056565659,-4.13102937388896,
33.7727590010604));
#52167=CARTESIAN_POINT('Ctrl Pts',(-3.56302333152666,-4.72428335870514,
33.8191501535344));
#52168=CARTESIAN_POINT('Ctrl Pts',(-2.77641609739674,-5.31753734352131,
33.8655413060084));
#52169=CARTESIAN_POINT('Ctrl Pts',(-1.83842507739896,-5.71006856179661,
33.9119324584823));
#52170=CARTESIAN_POINT('Ctrl Pts',(-0.863736110131024,-5.85388319377807,
33.9583236109563));
#52171=CARTESIAN_POINT('Ctrl Pts',(0.110952857136989,-5.99769782575954,
34.0047147634303));
#52172=CARTESIAN_POINT('Ctrl Pts',(1.12233977167512,-5.89279587144709,34.0511059159043));
#52173=CARTESIAN_POINT('Ctrl Pts',(2.04676486066272,-5.55200343295085,34.0974970683783));
#52174=CARTESIAN_POINT('Ctrl Pts',(2.97118994965026,-5.21121099445462,34.1438882208523));
#52175=CARTESIAN_POINT('Ctrl Pts',(3.80865321308733,-4.63452807177462,34.1902793733263));
#52176=CARTESIAN_POINT('Ctrl Pts',(4.45676009216202,-3.89246425741503,34.2366705258002));
#52177=CARTESIAN_POINT('Ctrl Pts',(5.10486697123672,-3.15040044305545,34.2830616782742));
#52178=CARTESIAN_POINT('Ctrl Pts',(5.56361746594906,-2.24295573701623,34.3294528307482));
#52179=CARTESIAN_POINT('Ctrl Pts',(5.77692128964215,-1.28108115575122,34.3758439832222));
#52180=CARTESIAN_POINT('Ctrl Pts',(5.99022511333525,-0.319206574486185,
34.4222351356962));
#52181=CARTESIAN_POINT('Ctrl Pts',(5.9580822660091,0.697097882004619,34.4686262881702));
#52182=CARTESIAN_POINT('Ctrl Pts',(5.68442277398798,1.64357118522697,34.5150174406441));
#52183=CARTESIAN_POINT('Ctrl Pts',(5.41076328196687,2.5900444884493,34.5614085931181));
#52184=CARTESIAN_POINT('Ctrl Pts',(4.89558714525077,3.46668663840314,34.6077997455921));
#52185=CARTESIAN_POINT('Ctrl Pts',(4.20188367397727,4.16631277086886,34.6541908980661));
#52186=CARTESIAN_POINT('Ctrl Pts',(3.50818020270377,4.86593890333457,34.7005820505401));
#52187=CARTESIAN_POINT('Ctrl Pts',(2.63594939687283,5.38854901831218,34.7469732030141));
#52188=CARTESIAN_POINT('Ctrl Pts',(1.69183675658515,5.67024487155617,34.793364355488));
#52189=CARTESIAN_POINT('Ctrl Pts',(0.747724116297463,5.95194072480015,34.839755507962));
#52190=CARTESIAN_POINT('Ctrl Pts',(-0.268270358447003,5.99272231631053,
34.886146660436));
#52191=CARTESIAN_POINT('Ctrl Pts',(-1.23192353985419,5.78760338190989,34.93253781291));
#52192=CARTESIAN_POINT('Ctrl Pts',(-2.19557672126134,5.58248444750926,34.978928965384));
#52193=CARTESIAN_POINT('Ctrl Pts',(-3.10688860933118,5.13146498719767,35.025320117858));
#52194=CARTESIAN_POINT('Ctrl Pts',(-3.85443535684222,4.48969003320565,35.0717112703319));
#52195=CARTESIAN_POINT('Ctrl Pts',(-4.60198210435332,3.84791507921359,35.1181024228059));
#52196=CARTESIAN_POINT('Ctrl Pts',(-5.18576371130555,3.01538463154107,35.1644935752799));
#52197=CARTESIAN_POINT('Ctrl Pts',(-5.53440264665228,2.09389012583512,35.2108847277539));
#52198=CARTESIAN_POINT('Ctrl Pts',(-5.78676336904098,1.42687048012088,35.2444647544343));
#52199=CARTESIAN_POINT('Ctrl Pts',(-5.91592054800081,0.713237911653397,
35.2780447811148));
#52200=CARTESIAN_POINT('Ctrl Pts',(-5.91661122068025,-0.000151359735457047,
35.3116248077952));
#52201=CARTESIAN_POINT('Origin',(0.,0.,0.));
#52202=CARTESIAN_POINT('',(-5.91669249471401,0.000154889389280682,37.3133751922049));
#52203=CARTESIAN_POINT('',(-5.91654848309511,0.000145436179947218,37.0616248077952));
#52204=CARTESIAN_POINT('',(-5.91675,-7.2459289488551E-16,0.));
#52205=CARTESIAN_POINT('Ctrl Pts',(-5.91669249471401,0.000154889389280682,
37.3133751922049));
#52206=CARTESIAN_POINT('Ctrl Pts',(-5.91694160613561,0.245724103443592,
37.3018155197983));
#52207=CARTESIAN_POINT('Ctrl Pts',(-5.9019420281964,0.491263090650058,37.2902558473917));
#52208=CARTESIAN_POINT('Ctrl Pts',(-5.87145331977663,0.734863478385117,
37.2786961749852));
#52209=CARTESIAN_POINT('Ctrl Pts',(-5.74909636438138,1.71247792390357,37.2323050225112));
#52210=CARTESIAN_POINT('Ctrl Pts',(-5.37727631279197,2.65886989201929,37.1859138700372));
#52211=CARTESIAN_POINT('Ctrl Pts',(-4.80145468171261,3.45832638101732,37.1395227175632));
#52212=CARTESIAN_POINT('Ctrl Pts',(-4.22563305063326,4.25778287001535,37.0931315650893));
#52213=CARTESIAN_POINT('Ctrl Pts',(-3.44580984006395,4.91030387989569,37.0467404126153));
#52214=CARTESIAN_POINT('Ctrl Pts',(-2.55733210232766,5.33610728308424,37.0003492601413));
#52215=CARTESIAN_POINT('Ctrl Pts',(-1.66885436459137,5.76191068627279,36.9539581076673));
#52216=CARTESIAN_POINT('Ctrl Pts',(-0.671722099688089,5.96099648276954,
36.9075669551933));
#52217=CARTESIAN_POINT('Ctrl Pts',(0.31214780026346,5.90902294537523,36.8611758027193));
#52218=CARTESIAN_POINT('Ctrl Pts',(1.29601770021501,5.85704940798092,36.8147846502453));
#52219=CARTESIAN_POINT('Ctrl Pts',(2.26662523521483,5.55401653669555,36.7683934977713));
#52220=CARTESIAN_POINT('Ctrl Pts',(3.10529662616736,5.03697541007437,36.7220023452974));
#52221=CARTESIAN_POINT('Ctrl Pts',(3.9439680171199,4.5199342834532,36.6756111928234));
#52222=CARTESIAN_POINT('Ctrl Pts',(4.65070326402515,3.78888490149623,36.6292200403494));
#52223=CARTESIAN_POINT('Ctrl Pts',(5.13909159883741,2.93321086131548,36.5828288878754));
#52224=CARTESIAN_POINT('Ctrl Pts',(5.62747993364967,2.07753682113472,36.5364377354014));
#52225=CARTESIAN_POINT('Ctrl Pts',(5.89752135636894,1.09723812273018,36.4900465829274));
#52226=CARTESIAN_POINT('Ctrl Pts',(5.91619857113585,0.112173459741759,36.4436554304535));
#52227=CARTESIAN_POINT('Ctrl Pts',(5.93487578590275,-0.872891203246667,
36.3972642779795));
#52228=CARTESIAN_POINT('Ctrl Pts',(5.70218879271729,-1.86272183081898,36.3508731255055));
#52229=CARTESIAN_POINT('Ctrl Pts',(5.2465876538672,-2.73629428396665,36.3044819730315));
#52230=CARTESIAN_POINT('Ctrl Pts',(4.79098651501711,-3.60986673711433,36.2580908205575));
#52231=CARTESIAN_POINT('Ctrl Pts',(4.1124712305024,-4.36718101583737,36.2116996680835));
#52232=CARTESIAN_POINT('Ctrl Pts',(3.29400218346852,-4.91564217915472,36.1653085156096));
#52233=CARTESIAN_POINT('Ctrl Pts',(2.47553313643465,-5.46410334247206,36.1189173631356));
#52234=CARTESIAN_POINT('Ctrl Pts',(1.51711032688161,-5.8037113903837,36.0725262106616));
#52235=CARTESIAN_POINT('Ctrl Pts',(0.535917737706336,-5.89294328808551,
36.0261350581876));
#52236=CARTESIAN_POINT('Ctrl Pts',(-0.44527485146894,-5.98217518578732,
35.9797439057136));
#52237=CARTESIAN_POINT('Ctrl Pts',(-1.44923722026646,-5.82103093327931,
35.9333527532396));
#52238=CARTESIAN_POINT('Ctrl Pts',(-2.35321737668262,-5.42921323915899,
35.8869616007656));
#52239=CARTESIAN_POINT('Ctrl Pts',(-3.25719753309878,-5.03739554503867,
35.8405704482917));
#52240=CARTESIAN_POINT('Ctrl Pts',(-4.06119547713358,-4.41490440930605,
35.7941792958177));
#52241=CARTESIAN_POINT('Ctrl Pts',(-4.66690837168441,-3.63785028120762,
35.7477881433437));
#52242=CARTESIAN_POINT('Ctrl Pts',(-5.27262126623519,-2.86079615310923,
35.7013969908697));
#52243=CARTESIAN_POINT('Ctrl Pts',(-5.68004911130202,-1.92917903264505,
35.6550058383957));
#52244=CARTESIAN_POINT('Ctrl Pts',(-5.83937671347322,-0.956905437505181,
35.6086146859218));
#52245=CARTESIAN_POINT('Ctrl Pts',(-5.89116748012414,-0.640859791926311,
35.5935348546828));
#52246=CARTESIAN_POINT('Ctrl Pts',(-5.91674324878296,-0.320518264209038,
35.5784550234439));
#52247=CARTESIAN_POINT('Ctrl Pts',(-5.91647681799755,-0.000134629570711919,
35.5633751922049));
#52248=CARTESIAN_POINT('Ctrl Pts',(-5.91661122068025,-0.000151359735457047,
35.3116248077952));
#52249=CARTESIAN_POINT('Ctrl Pts',(-5.91687471941605,-0.272316709171056,
35.3244359335887));
#52250=CARTESIAN_POINT('Ctrl Pts',(-5.89843990491604,-0.544446646691766,
35.3372470593823));
#52251=CARTESIAN_POINT('Ctrl Pts',(-5.86101453084031,-0.81393929971491,
35.3500581851759));
#52252=CARTESIAN_POINT('Ctrl Pts',(-5.72549121594036,-1.78981565581969,
35.3964493376498));
#52253=CARTESIAN_POINT('Ctrl Pts',(-5.34094832239917,-2.73110980428999,
35.4428404901238));
#52254=CARTESIAN_POINT('Ctrl Pts',(-4.75440295729178,-3.52273204119144,
35.4892316425978));
#52255=CARTESIAN_POINT('Ctrl Pts',(-4.16785759218437,-4.31435427809291,
35.5356227950718));
#52256=CARTESIAN_POINT('Ctrl Pts',(-3.37930975551075,-4.95630460342556,
35.5820139475458));
#52257=CARTESIAN_POINT('Ctrl Pts',(-2.48517323801659,-5.37009334103121,
35.6284051000198));
#52258=CARTESIAN_POINT('Ctrl Pts',(-1.59103672052242,-5.78388207863687,
35.6747962524937));
#52259=CARTESIAN_POINT('Ctrl Pts',(-0.591311522207775,-5.96950922851551,
35.7211874049677));
#52260=CARTESIAN_POINT('Ctrl Pts',(0.391768433263235,-5.90427861885261,
35.7675785574417));
#52261=CARTESIAN_POINT('Ctrl Pts',(1.37484838873424,-5.83904800918971,35.8139697099157));
#52262=CARTESIAN_POINT('Ctrl Pts',(2.34128310136155,-5.52295963998528,35.8603608623897));
#52263=CARTESIAN_POINT('Ctrl Pts',(3.17290899270499,-4.99466085318647,35.9067520148637));
#52264=CARTESIAN_POINT('Ctrl Pts',(4.00453488404839,-4.46636206638769,35.9531431673376));
#52265=CARTESIAN_POINT('Ctrl Pts',(4.701351954108,-3.72585286199446,35.9995343198116));
#52266=CARTESIAN_POINT('Ctrl Pts',(5.17816210575339,-2.86367346617613,36.0459254722856));
#52267=CARTESIAN_POINT('Ctrl Pts',(5.65497225739884,-2.00149407035771,36.0923166247596));
#52268=CARTESIAN_POINT('Ctrl Pts',(5.91177549063012,-1.01764448311409,36.1387077772336));
#52269=CARTESIAN_POINT('Ctrl Pts',(5.91717311022538,-0.0324175564679062,
36.1850989297076));
#52270=CARTESIAN_POINT('Ctrl Pts',(5.92257072982063,0.952809370178166,36.2314900821816));
#52271=CARTESIAN_POINT('Ctrl Pts',(5.67656273577991,1.93941363622675,36.2778812346556));
#52272=CARTESIAN_POINT('Ctrl Pts',(5.20922791616921,2.80676558190117,36.3242723871295));
#52273=CARTESIAN_POINT('Ctrl Pts',(4.74189309655848,3.67411752757564,36.3706635396035));
#52274=CARTESIAN_POINT('Ctrl Pts',(4.05323145137778,4.42221715287586,36.4170546920775));
#52275=CARTESIAN_POINT('Ctrl Pts',(3.22744393415846,4.95959616967,36.4634458445515));
#52276=CARTESIAN_POINT('Ctrl Pts',(2.40165641693915,5.49697518646414,36.5098369970254));
#52277=CARTESIAN_POINT('Ctrl Pts',(1.43874302768128,5.82363359475216,36.5562281494994));
#52278=CARTESIAN_POINT('Ctrl Pts',(0.456436801339,5.8996316800903,36.6026193019734));
#52279=CARTESIAN_POINT('Ctrl Pts',(-0.525869425003222,5.97562976542843,
36.6490104544474));
#52280=CARTESIAN_POINT('Ctrl Pts',(-1.52756848842996,5.80096752781665,36.6954016069214));
#52281=CARTESIAN_POINT('Ctrl Pts',(-2.42618512567881,5.39700048640691,36.7417927593954));
#52282=CARTESIAN_POINT('Ctrl Pts',(-3.32480176292772,4.99303344499716,36.7881839118694));
#52283=CARTESIAN_POINT('Ctrl Pts',(-4.12033597399883,4.35976159978945,36.8345750643434));
#52284=CARTESIAN_POINT('Ctrl Pts',(-4.71551976145427,3.57461353067377,36.8809662168173));
#52285=CARTESIAN_POINT('Ctrl Pts',(-5.3107035489097,2.78946546155808,36.9273573692913));
#52286=CARTESIAN_POINT('Ctrl Pts',(-5.70553691274941,1.8524411685345,36.9737485217653));
#52287=CARTESIAN_POINT('Ctrl Pts',(-5.85174455558468,0.878108290888243,
37.0201396742393));
#52288=CARTESIAN_POINT('Ctrl Pts',(-5.89532645476485,0.587676980882504,
37.0339680520913));
#52289=CARTESIAN_POINT('Ctrl Pts',(-5.91681720987146,0.293930690774358,
37.0477964299432));
#52290=CARTESIAN_POINT('Ctrl Pts',(-5.91654848309511,0.000145436179947218,
37.0616248077952));
#52291=CARTESIAN_POINT('Origin',(0.,0.,0.));
#52292=CARTESIAN_POINT('',(-5.91691912648428,-0.000142687999947211,39.0633751922049));
#52293=CARTESIAN_POINT('',(-5.91706133753908,-0.000116827836684568,38.8116248077952));
#52294=CARTESIAN_POINT('',(-5.91675,-7.2459289488551E-16,0.));
#52295=CARTESIAN_POINT('Ctrl Pts',(-5.91691912648428,-0.000142687999947211,
39.0633751922049));
#52296=CARTESIAN_POINT('Ctrl Pts',(-5.9160967133036,0.811256349217919,39.0251760161528));
#52297=CARTESIAN_POINT('Ctrl Pts',(-5.74787377874497,1.62298581578632,38.9869768401007));
#52298=CARTESIAN_POINT('Ctrl Pts',(-5.42341831385396,2.36654224790806,38.9487776640486));
#52299=CARTESIAN_POINT('Ctrl Pts',(-5.02938198903266,3.26955753202083,38.9023865115746));
#52300=CARTESIAN_POINT('Ctrl Pts',(-4.40491843421483,4.07202446391407,38.8559953591006));
#52301=CARTESIAN_POINT('Ctrl Pts',(-3.62637926144279,4.67582739954737,38.8096042066266));
#52302=CARTESIAN_POINT('Ctrl Pts',(-2.84784008867076,5.27963033518068,38.7632130541527));
#52303=CARTESIAN_POINT('Ctrl Pts',(-1.91522529794454,5.68476927455403,38.7168219016787));
#52304=CARTESIAN_POINT('Ctrl Pts',(-0.942563389625921,5.84170888308526,
38.6704307492047));
#52305=CARTESIAN_POINT('Ctrl Pts',(0.0300985186927029,5.99864849161649,
38.6240395967307));
#52306=CARTESIAN_POINT('Ctrl Pts',(1.0428075446037,5.90738876930559,38.5776484442567));
#52307=CARTESIAN_POINT('Ctrl Pts',(1.97174226400384,5.57908781634788,38.5312572917827));
#52308=CARTESIAN_POINT('Ctrl Pts',(2.90067698340398,5.25078686339016,38.4848661393088));
#52309=CARTESIAN_POINT('Ctrl Pts',(3.74583739629323,4.68544467978563,38.4384749868348));
#52310=CARTESIAN_POINT('Ctrl Pts',(4.40388783246218,3.95218425396285,38.3920838343608));
#52311=CARTESIAN_POINT('Ctrl Pts',(5.06193826863114,3.21892382814006,38.3456926818868));
#52312=CARTESIAN_POINT('Ctrl Pts',(5.53287872807978,2.31774516009906,38.2993015294128));
#52313=CARTESIAN_POINT('Ctrl Pts',(5.75912848735764,1.3588331333486,38.2529103769389));
#52314=CARTESIAN_POINT('Ctrl Pts',(5.9853782466355,0.399921106598193,38.2065192244649));
#52315=CARTESIAN_POINT('Ctrl Pts',(5.96693730574259,-0.616724278861779,
38.1601280719908));
#52316=CARTESIAN_POINT('Ctrl Pts',(5.70606039284341,-1.56680030999616,38.1137369195169));
#52317=CARTESIAN_POINT('Ctrl Pts',(5.44518347994422,-2.51687634113059,38.0673457670429));
#52318=CARTESIAN_POINT('Ctrl Pts',(4.94187059503875,-3.40038301793954,38.0209546145689));
#52319=CARTESIAN_POINT('Ctrl Pts',(4.25766055785111,-4.10929616750841,37.9745634620949));
#52320=CARTESIAN_POINT('Ctrl Pts',(3.57345052066347,-4.81820931707727,37.928172309621));
#52321=CARTESIAN_POINT('Ctrl Pts',(2.70834333119368,-5.35252893940602,37.8817811571469));
#52322=CARTESIAN_POINT('Ctrl Pts',(1.76811350261519,-5.64692509778996,37.835390004673));
#52323=CARTESIAN_POINT('Ctrl Pts',(0.827883674036693,-5.9413212561739,37.788998852199));
#52324=CARTESIAN_POINT('Ctrl Pts',(-0.187468793650468,-5.99579395061301,
37.742607699725));
#52325=CARTESIAN_POINT('Ctrl Pts',(-1.15379926926493,-5.80368293968787,
37.696216547251));
#52326=CARTESIAN_POINT('Ctrl Pts',(-2.1201297448794,-5.61157192876273,37.6498253947771));
#52327=CARTESIAN_POINT('Ctrl Pts',(-3.03743822842114,-5.17287721247336,
37.6034342423031));
#52328=CARTESIAN_POINT('Ctrl Pts',(-3.79356768379389,-4.54123690712729,
37.5570430898291));
#52329=CARTESIAN_POINT('Ctrl Pts',(-4.54969713916663,-3.90959660178122,
37.5106519373551));
#52330=CARTESIAN_POINT('Ctrl Pts',(-5.14464756637036,-3.08501070737847,
37.4642607848811));
#52331=CARTESIAN_POINT('Ctrl Pts',(-5.50567585037168,-2.1682992987165,37.4178696324071));
#52332=CARTESIAN_POINT('Ctrl Pts',(-5.77674368997775,-1.48001255748339,
37.3830381523397));
#52333=CARTESIAN_POINT('Ctrl Pts',(-5.91594187486849,-0.739791614598744,
37.3482066722723));
#52334=CARTESIAN_POINT('Ctrl Pts',(-5.91669249471401,0.000154889389280682,
37.3133751922049));
#52335=CARTESIAN_POINT('Ctrl Pts',(-5.91654848309511,0.000145436179947218,
37.0616248077952));
#52336=CARTESIAN_POINT('Ctrl Pts',(-5.91591569090887,-0.691653929951799,
37.0941875824172));
#52337=CARTESIAN_POINT('Ctrl Pts',(-5.79462691049747,-1.38366935355313,
37.1267503570392));
#52338=CARTESIAN_POINT('Ctrl Pts',(-5.55701272580384,-2.03312520017727,
37.1593131316612));
#52339=CARTESIAN_POINT('Ctrl Pts',(-5.2184913313569,-2.95838435132766,37.2057042841352));
#52340=CARTESIAN_POINT('Ctrl Pts',(-4.64386662063219,-3.79726119135959,
37.2520954366092));
#52341=CARTESIAN_POINT('Ctrl Pts',(-3.90339653365634,-4.44718832695235,
37.2984865890832));
#52342=CARTESIAN_POINT('Ctrl Pts',(-3.16292644668049,-5.09711546254512,
37.3448777415572));
#52343=CARTESIAN_POINT('Ctrl Pts',(-2.25661098345347,-5.55809289369875,
37.3912688940312));
#52344=CARTESIAN_POINT('Ctrl Pts',(-1.29526309070761,-5.77375805175383,
37.4376600465051));
#52345=CARTESIAN_POINT('Ctrl Pts',(-0.333915197961686,-5.98942320980892,
37.4840511989791));
#52346=CARTESIAN_POINT('Ctrl Pts',(0.682465124303125,-5.95977609476543,
37.5304423514531));
#52347=CARTESIAN_POINT('Ctrl Pts',(1.62960757167219,-5.6884415859434,37.5768335039271));
#52348=CARTESIAN_POINT('Ctrl Pts',(2.57675001904114,-5.41710707712141,37.6232246564011));
#52349=CARTESIAN_POINT('Ctrl Pts',(3.45465459151441,-4.90408517452091,37.6696158088751));
#52350=CARTESIAN_POINT('Ctrl Pts',(4.15598207159793,-4.21210179541024,37.7160069613491));
#52351=CARTESIAN_POINT('Ctrl Pts',(4.85730955168154,-3.5201184162995,37.762398113823));
#52352=CARTESIAN_POINT('Ctrl Pts',(5.3820599393754,-2.6491735606785,37.808789266297));
#52353=CARTESIAN_POINT('Ctrl Pts',(5.66607330459045,-1.70575549870112,37.855180418771));
#52354=CARTESIAN_POINT('Ctrl Pts',(5.95008666980548,-0.762337436723782,
37.901571571245));
#52355=CARTESIAN_POINT('Ctrl Pts',(5.99336301254174,0.253553831609811,37.947962723719));
#52356=CARTESIAN_POINT('Ctrl Pts',(5.79061104156902,1.21770779729813,37.994353876193));
#52357=CARTESIAN_POINT('Ctrl Pts',(5.5878590705963,2.18186176298639,38.0407450286669));
#52358=CARTESIAN_POINT('Ctrl Pts',(5.13907878591457,3.09427842602926,38.0871361811409));
#52359=CARTESIAN_POINT('Ctrl Pts',(4.49914144129667,3.8433988611057,38.1335273336149));
#52360=CARTESIAN_POINT('Ctrl Pts',(3.85920409667869,4.59251929618222,38.1799184860889));
#52361=CARTESIAN_POINT('Ctrl Pts',(3.02810969212445,5.1783435032923,38.2263096385629));
#52362=CARTESIAN_POINT('Ctrl Pts',(2.107474081846,5.52924420772758,38.2727007910369));
#52363=CARTESIAN_POINT('Ctrl Pts',(1.1868384715676,5.88014491216284,38.3190919435108));
#52364=CARTESIAN_POINT('Ctrl Pts',(0.176661655564968,5.99612211392334,38.3654830959848));
#52365=CARTESIAN_POINT('Ctrl Pts',(-0.799544549091766,5.86299556782702,
38.4118742484588));
#52366=CARTESIAN_POINT('Ctrl Pts',(-1.7757507537485,5.7298690217307,38.4582654009328));
#52367=CARTESIAN_POINT('Ctrl Pts',(-2.71798634705937,5.34763872777755,38.5046565534068));
#52368=CARTESIAN_POINT('Ctrl Pts',(-3.5110465169614,4.76303903721929,38.5510477058807));
#52369=CARTESIAN_POINT('Ctrl Pts',(-4.30410668686342,4.17843934666103,38.5974388583547));
#52370=CARTESIAN_POINT('Ctrl Pts',(-4.94799143335662,3.39147025949764,38.6438300108287));
#52371=CARTESIAN_POINT('Ctrl Pts',(-5.36397456339906,2.49835253668281,38.6902211633027));
#52372=CARTESIAN_POINT('Ctrl Pts',(-5.72684453135159,1.71926902091001,38.7306890448002));
#52373=CARTESIAN_POINT('Ctrl Pts',(-5.91629496269227,0.859412724788655,
38.7711569262977));
#52374=CARTESIAN_POINT('Ctrl Pts',(-5.91706133753908,-0.000116827836684568,
38.8116248077952));
#52375=CARTESIAN_POINT('Origin',(0.,0.,0.));
#52376=CARTESIAN_POINT('',(-5.9163246276023,8.91563840094145E-5,40.8133751922049));
#52377=CARTESIAN_POINT('',(-5.91626344896283,4.86828180632854E-5,40.5616248077952));
#52378=CARTESIAN_POINT('',(-5.91675,-7.2459289488551E-16,0.));
#52379=CARTESIAN_POINT('Ctrl Pts',(-5.9163246276023,8.91563840094145E-5,
40.8133751922049));
#52380=CARTESIAN_POINT('Ctrl Pts',(-5.91653311395868,0.392051192521081,
40.7949276649813));
#52381=CARTESIAN_POINT('Ctrl Pts',(-5.87816883703071,0.783972960225323,
40.7764801377576));
#52382=CARTESIAN_POINT('Ctrl Pts',(-5.8008321742822,1.16804730383351,40.758032610534));
#52383=CARTESIAN_POINT('Ctrl Pts',(-5.60634882321301,2.1339031185268,40.71164145806));
#52384=CARTESIAN_POINT('Ctrl Pts',(-5.16540288854038,3.05013157845018,40.665250305586));
#52385=CARTESIAN_POINT('Ctrl Pts',(-4.5319077374673,3.80470769931993,40.618859153112));
#52386=CARTESIAN_POINT('Ctrl Pts',(-3.89841258639425,4.55928382018964,40.572468000638));
#52387=CARTESIAN_POINT('Ctrl Pts',(-3.07236821892077,5.15220760200574,40.5260768481641));
#52388=CARTESIAN_POINT('Ctrl Pts',(-2.15477303373402,5.51098372264635,40.4796856956901));
#52389=CARTESIAN_POINT('Ctrl Pts',(-1.23717784854716,5.869759843287,40.4332945432161));
#52390=CARTESIAN_POINT('Ctrl Pts',(-0.228031845647002,5.9943883027521,40.3869033907421));
#52391=CARTESIAN_POINT('Ctrl Pts',(0.749279192861052,5.86963108800935,40.3405122382681));
#52392=CARTESIAN_POINT('Ctrl Pts',(1.72659023136905,5.7448738732666,40.2941210857941));
#52393=CARTESIAN_POINT('Ctrl Pts',(2.67206630548495,5.37073098431603,40.2477299333201));
#52394=CARTESIAN_POINT('Ctrl Pts',(3.47010639758447,4.79294794543229,40.2013387808462));
#52395=CARTESIAN_POINT('Ctrl Pts',(4.268146489684,4.21516490654855,40.1549476283722));
#52396=CARTESIAN_POINT('Ctrl Pts',(4.91875059976714,3.43374171773163,40.1085564758982));
#52397=CARTESIAN_POINT('Ctrl Pts',(5.34237097484983,2.54422105668167,40.0621653234242));
#52398=CARTESIAN_POINT('Ctrl Pts',(5.76599134993251,1.65470039563171,40.0157741709502));
#52399=CARTESIAN_POINT('Ctrl Pts',(5.96262799001472,0.657082262348707,39.9693830184762));
#52400=CARTESIAN_POINT('Ctrl Pts',(5.9082386201854,-0.32665704512534,39.9229918660023));
#52401=CARTESIAN_POINT('Ctrl Pts',(5.85384925035609,-1.31039635259939,39.8766007135283));
#52402=CARTESIAN_POINT('Ctrl Pts',(5.54843387061524,-2.28025683426448,39.8302095610543));
#52403=CARTESIAN_POINT('Ctrl Pts',(5.02933486292548,-3.11765605138583,39.7838184085803));
#52404=CARTESIAN_POINT('Ctrl Pts',(4.51023585523571,-3.95505526850718,39.7374272561063));
#52405=CARTESIAN_POINT('Ctrl Pts',(3.77745321959704,-4.6599932210848,39.6910361036323));
#52406=CARTESIAN_POINT('Ctrl Pts',(2.92058247375582,-5.14627889179849,39.6446449511583));
#52407=CARTESIAN_POINT('Ctrl Pts',(2.0637117279146,-5.63256456251218,39.5982537986844));
#52408=CARTESIAN_POINT('Ctrl Pts',(1.08275287187084,-5.90019795136195,39.5518626462104));
#52409=CARTESIAN_POINT('Ctrl Pts',(0.0976453151037753,-5.9164561868249,
39.5054714937364));
#52410=CARTESIAN_POINT('Ctrl Pts',(-0.887462241663293,-5.93271442228785,
39.4590803412624));
#52411=CARTESIAN_POINT('Ctrl Pts',(-1.87671849915367,-5.69759750436398,
39.4126891887884));
#52412=CARTESIAN_POINT('Ctrl Pts',(-2.74916954516603,-5.23985259621985,
39.3662980363144));
#52413=CARTESIAN_POINT('Ctrl Pts',(-3.6216205911784,-4.78210768807572,39.3199068838405));
#52414=CARTESIAN_POINT('Ctrl Pts',(-4.37726642571275,-4.10173478971132,
39.2735157313665));
#52415=CARTESIAN_POINT('Ctrl Pts',(-4.92371610432621,-3.28192141011619,
39.2271245788925));
#52416=CARTESIAN_POINT('Ctrl Pts',(-5.47016578293967,-2.46210803052105,
39.1807334264185));
#52417=CARTESIAN_POINT('Ctrl Pts',(-5.80741930563224,-1.50285416969518,
39.1343422739445));
#52418=CARTESIAN_POINT('Ctrl Pts',(-5.89424151956614,-0.521445421116098,
39.0879511214705));
#52419=CARTESIAN_POINT('Ctrl Pts',(-5.90957301041108,-0.348143468053205,
39.0797591450487));
#52420=CARTESIAN_POINT('Ctrl Pts',(-5.91709549650274,-0.174150676354238,
39.0715671686268));
#52421=CARTESIAN_POINT('Ctrl Pts',(-5.91691912648428,-0.000142687999947211,
39.0633751922049));
#52422=CARTESIAN_POINT('Ctrl Pts',(-5.91706133753908,-0.000116827836684568,
38.8116248077952));
#52423=CARTESIAN_POINT('Ctrl Pts',(-5.91717351158228,-0.125925895771626,
38.8175480787717));
#52424=CARTESIAN_POINT('Ctrl Pts',(-5.91324330254416,-0.251727963526452,
38.8234713497482));
#52425=CARTESIAN_POINT('Ctrl Pts',(-5.90522284338791,-0.377268716263677,
38.8293946207247));
#52426=CARTESIAN_POINT('Ctrl Pts',(-5.84240647974259,-1.3605058879289,38.8757857731986));
#52427=CARTESIAN_POINT('Ctrl Pts',(-5.5286922388603,-2.32771387279308,38.9221769256726));
#52428=CARTESIAN_POINT('Ctrl Pts',(-5.002437183899,-3.160634546335,38.9685680781466));
#52429=CARTESIAN_POINT('Ctrl Pts',(-4.47618212893773,-3.99355521987688,
39.0149592306206));
#52430=CARTESIAN_POINT('Ctrl Pts',(-3.73738625989748,-4.69218858209652,
39.0613503830946));
#52431=CARTESIAN_POINT('Ctrl Pts',(-2.87638031767776,-5.17111446232025,
39.1077415355686));
#52432=CARTESIAN_POINT('Ctrl Pts',(-2.01537437545794,-5.65004034254403,
39.1541326880426));
#52433=CARTESIAN_POINT('Ctrl Pts',(-1.03215836005863,-5.90925874077186,
39.2005238405165));
#52434=CARTESIAN_POINT('Ctrl Pts',(-0.0469476582424495,-5.91707566554013,
39.2469149929905));
#52435=CARTESIAN_POINT('Ctrl Pts',(0.938263043573675,-5.92489259030839,
39.2933061454645));
#52436=CARTESIAN_POINT('Ctrl Pts',(1.92546843180667,-5.68130804161713,39.3396972979385));
#52437=CARTESIAN_POINT('Ctrl Pts',(2.79396534895927,-5.21610449887237,39.3860884504125));
#52438=CARTESIAN_POINT('Ctrl Pts',(3.66246226611187,-4.7509009561276,39.4324796028865));
#52439=CARTESIAN_POINT('Ctrl Pts',(4.41225071218408,-4.06407841932935,39.4788707553604));
#52440=CARTESIAN_POINT('Ctrl Pts',(4.95165591111146,-3.23961297878258,39.5252619078344));
#52441=CARTESIAN_POINT('Ctrl Pts',(5.49106111003884,-2.41514753823582,39.5716530603084));
#52442=CARTESIAN_POINT('Ctrl Pts',(5.82008306182138,-1.45303919394055,39.6180442127824));
#52443=CARTESIAN_POINT('Ctrl Pts',(5.89849306740675,-0.4709225499975,39.6644353652564));
#52444=CARTESIAN_POINT('Ctrl Pts',(5.97690307299213,0.511194093945548,39.7108265177304));
#52445=CARTESIAN_POINT('Ctrl Pts',(5.80470113238033,1.51331903753637,39.7572176702043));
#52446=CARTESIAN_POINT('Ctrl Pts',(5.40294195030329,2.41292494620007,39.8036088226783));
#52447=CARTESIAN_POINT('Ctrl Pts',(5.00118276822624,3.31253085486376,39.8499999751523));
#52448=CARTESIAN_POINT('Ctrl Pts',(4.36986634468393,4.10961772860033,39.8963911276263));
#52449=CARTESIAN_POINT('Ctrl Pts',(3.586182175003,4.70672772975369,39.9427822801003));
#52450=CARTESIAN_POINT('Ctrl Pts',(2.80249800532207,5.30383773090705,39.9891734325743));
#52451=CARTESIAN_POINT('Ctrl Pts',(1.86644608950252,5.7009708594772,40.0355645850482));
#52452=CARTESIAN_POINT('Ctrl Pts',(0.892475176677488,5.84957063153836,40.0819557375222));
#52453=CARTESIAN_POINT('Ctrl Pts',(-0.0814957361475431,5.99817040359952,
40.1283468899962));
#52454=CARTESIAN_POINT('Ctrl Pts',(-1.09338564597805,5.89823681915169,40.1747380424702));
#52455=CARTESIAN_POINT('Ctrl Pts',(-2.01947328000496,5.56198851002837,40.2211291949442));
#52456=CARTESIAN_POINT('Ctrl Pts',(-2.94556091403187,5.22574020090506,40.2675203474182));
#52457=CARTESIAN_POINT('Ctrl Pts',(-3.78584627225519,4.65317716710625,40.3139114998921));
#52458=CARTESIAN_POINT('Ctrl Pts',(-4.4375897453239,3.91430527252765,40.3603026523661));
#52459=CARTESIAN_POINT('Ctrl Pts',(-5.08933321839262,3.17543337794904,40.4066938048401));
#52460=CARTESIAN_POINT('Ctrl Pts',(-5.55253480630674,2.27025262259063,40.4530849573141));
#52461=CARTESIAN_POINT('Ctrl Pts',(-5.77055999826902,1.3094372152643,40.4994761097881));
#52462=CARTESIAN_POINT('Ctrl Pts',(-5.86792038626399,0.880379637069279,
40.5201923424572));
#52463=CARTESIAN_POINT('Ctrl Pts',(-5.91638966469366,0.440227842995804,
40.5409085751262));
#52464=CARTESIAN_POINT('Ctrl Pts',(-5.91626344896283,4.86828180632854E-5,
40.5616248077952));
#52465=CARTESIAN_POINT('Origin',(0.,0.,0.));
#52466=CARTESIAN_POINT('',(-5.9172499153618,-2.94340949030803E-5,42.5633751922049));
#52467=CARTESIAN_POINT('',(-5.91725525726564,2.18443538467081E-5,42.3116248077952));
#52468=CARTESIAN_POINT('',(-5.91675,-7.2459289488551E-16,0.));
#52469=CARTESIAN_POINT('Ctrl Pts',(-5.9172499153618,-2.94340949030803E-5,
42.5633751922049));
#52470=CARTESIAN_POINT('Ctrl Pts',(-5.91698609659766,0.957521378018406,
42.5182881613357));
#52471=CARTESIAN_POINT('Ctrl Pts',(-5.68004380919251,1.91519802461481,42.4732011304666));
#52472=CARTESIAN_POINT('Ctrl Pts',(-5.23308594241081,2.7620282289511,42.4281140995974));
#52473=CARTESIAN_POINT('Ctrl Pts',(-4.77320002516144,3.63335260697322,42.3817229471234));
#52474=CARTESIAN_POINT('Ctrl Pts',(-4.09097361557659,4.38732544079608,42.3353317946494));
#52475=CARTESIAN_POINT('Ctrl Pts',(-3.26982084687155,4.93176033962971,42.2889406421755));
#52476=CARTESIAN_POINT('Ctrl Pts',(-2.44866807816651,5.47619523846334,42.2425494897015));
#52477=CARTESIAN_POINT('Ctrl Pts',(-1.48858895034126,5.81109220230777,42.1961583372275));
#52478=CARTESIAN_POINT('Ctrl Pts',(-0.506969960225164,5.89550420893833,
42.1497671847535));
#52479=CARTESIAN_POINT('Ctrl Pts',(0.474649029890985,5.9799162155689,42.1033760322795));
#52480=CARTESIAN_POINT('Ctrl Pts',(1.47780788229784,5.81384326498563,42.0569848798055));
#52481=CARTESIAN_POINT('Ctrl Pts',(2.37985284895086,5.41759068549118,42.0105937273315));
#52482=CARTESIAN_POINT('Ctrl Pts',(3.28189781560384,5.02133810599675,41.9642025748575));
#52483=CARTESIAN_POINT('Ctrl Pts',(4.08282889650282,4.39490589759118,41.9178114223836));
#52484=CARTESIAN_POINT('Ctrl Pts',(4.68471823230415,3.61488637471462,41.8714202699096));
#52485=CARTESIAN_POINT('Ctrl Pts',(5.28660756810544,2.83486685183809,41.8250291174356));
#52486=CARTESIAN_POINT('Ctrl Pts',(5.68945515880915,1.90126001449041,41.7786379649616));
#52487=CARTESIAN_POINT('Ctrl Pts',(5.8440058273591,0.928215658116778,41.7322468124877));
#52488=CARTESIAN_POINT('Ctrl Pts',(5.99855649590908,-0.0448286982570238,
41.6858556600137));
#52489=CARTESIAN_POINT('Ctrl Pts',(5.90481024230533,-1.05731057365682,41.6394645075397));
#52490=CARTESIAN_POINT('Ctrl Pts',(5.57422918876514,-1.98543631710994,41.5930733550657));
#52491=CARTESIAN_POINT('Ctrl Pts',(5.24364813522496,-2.91356206056301,41.5466822025917));
#52492=CARTESIAN_POINT('Ctrl Pts',(4.67623228174835,-3.75733167206929,41.5002910501177));
#52493=CARTESIAN_POINT('Ctrl Pts',(3.94135815924267,-4.41357953125936,41.4538998976437));
#52494=CARTESIAN_POINT('Ctrl Pts',(3.20648403673703,-5.06982739044939,41.4075087451697));
#52495=CARTESIAN_POINT('Ctrl Pts',(2.30415164520231,-5.53855349732326,41.3611175926957));
#52496=CARTESIAN_POINT('Ctrl Pts',(1.34468693106113,-5.76244787183483,41.3147264402218));
#52497=CARTESIAN_POINT('Ctrl Pts',(0.385222216919947,-5.98634224634639,
41.2683352877478));
#52498=CARTESIAN_POINT('Ctrl Pts',(-0.63137481982772,-5.96540488849565,
41.2219441352738));
#52499=CARTESIAN_POINT('Ctrl Pts',(-1.58080737762424,-5.70219575716487,
41.1755529827998));
#52500=CARTESIAN_POINT('Ctrl Pts',(-2.5302399354207,-5.43898662583412,41.1291618303258));
#52501=CARTESIAN_POINT('Ctrl Pts',(-3.41250801426605,-4.93350572102335,
41.0827706778519));
#52502=CARTESIAN_POINT('Ctrl Pts',(-4.11973888155062,-4.24755694088029,
41.0363795253779));
#52503=CARTESIAN_POINT('Ctrl Pts',(-4.82696974883531,-3.56160816073712,
40.9899883729039));
#52504=CARTESIAN_POINT('Ctrl Pts',(-5.35916340455918,-2.69519150526158,
40.9435972204299));
#52505=CARTESIAN_POINT('Ctrl Pts',(-5.6512498486882,-1.75424159279215,40.8972060679559));
#52506=CARTESIAN_POINT('Ctrl Pts',(-5.82718758034986,-1.18746214604047,
40.8692624427056));
#52507=CARTESIAN_POINT('Ctrl Pts',(-5.91600882025632,-0.593640296750067,
40.8413188174552));
#52508=CARTESIAN_POINT('Ctrl Pts',(-5.9163246276023,8.91563840094145E-5,
40.8133751922049));
#52509=CARTESIAN_POINT('Ctrl Pts',(-5.91626344896283,4.86828180632854E-5,
40.5616248077952));
#52510=CARTESIAN_POINT('Ctrl Pts',(-5.91610702193196,-0.545492816832468,
40.5872997276001));
#52511=CARTESIAN_POINT('Ctrl Pts',(-5.84130698505393,-1.09107635134332,
40.6129746474051));
#52512=CARTESIAN_POINT('Ctrl Pts',(-5.69242609675824,-1.61563413162986,
40.63864956721));
#52513=CARTESIAN_POINT('Ctrl Pts',(-5.42341820727474,-2.56344001190361,
40.685040719684));
#52514=CARTESIAN_POINT('Ctrl Pts',(-4.91255363229728,-3.44260171315683,
40.731431872158));
#52515=CARTESIAN_POINT('Ctrl Pts',(-4.22229451798941,-4.14562631187354,
40.777823024632));
#52516=CARTESIAN_POINT('Ctrl Pts',(-3.53203540368151,-4.84865091059029,
40.824214177106));
#52517=CARTESIAN_POINT('Ctrl Pts',(-2.66238175004321,-5.37553840677047,
40.8706053295799));
#52518=CARTESIAN_POINT('Ctrl Pts',(-1.71966395516019,-5.6618675713641,40.9169964820539));
#52519=CARTESIAN_POINT('Ctrl Pts',(-0.776946160277282,-5.94819673595769,
40.9633876345279));
#52520=CARTESIAN_POINT('Ctrl Pts',(0.238835775850449,-5.99396756896476,
41.0097787870019));
#52521=CARTESIAN_POINT('Ctrl Pts',(1.20348471199892,-5.79358378400852,41.0561699394759));
#52522=CARTESIAN_POINT('Ctrl Pts',(2.16813364814744,-5.59319999905228,41.1025610919499));
#52523=CARTESIAN_POINT('Ctrl Pts',(3.08164958431682,-5.14666159613273,41.1489522444239));
#52524=CARTESIAN_POINT('Ctrl Pts',(3.83233918978381,-4.50856571969277,41.1953433968978));
#52525=CARTESIAN_POINT('Ctrl Pts',(4.58302879525085,-3.87046984325278,41.2417345493718));
#52526=CARTESIAN_POINT('Ctrl Pts',(5.17089207001545,-3.04081649329238,41.2881257018459));
#52527=CARTESIAN_POINT('Ctrl Pts',(5.52405242761798,-2.12104532984789,41.3345168543198));
#52528=CARTESIAN_POINT('Ctrl Pts',(5.87721278522047,-1.20127416640351,41.3809080067938));
#52529=CARTESIAN_POINT('Ctrl Pts',(5.99567022566093,-0.191385189475094,
41.4272991592678));
#52530=CARTESIAN_POINT('Ctrl Pts',(5.8649412511175,0.785144977237938,41.4736903117417));
#52531=CARTESIAN_POINT('Ctrl Pts',(5.73421227657406,1.76167514395103,41.5200814642157));
#52532=CARTESIAN_POINT('Ctrl Pts',(5.3542968870467,2.70484650044868,41.5664726166897));
#52533=CARTESIAN_POINT('Ctrl Pts',(4.77164639615703,3.49933982122104,41.6128637691637));
#52534=CARTESIAN_POINT('Ctrl Pts',(4.18899590526738,4.29383314199335,41.6592549216377));
#52535=CARTESIAN_POINT('Ctrl Pts',(3.40361031301533,4.93964842704044,41.7056460741117));
#52536=CARTESIAN_POINT('Ctrl Pts',(2.51151677035428,5.35782344115321,41.7520372265857));
#52537=CARTESIAN_POINT('Ctrl Pts',(1.61942322769312,5.77599845526603,41.7984283790596));
#52538=CARTESIAN_POINT('Ctrl Pts',(0.620621734623047,5.96653319844456,41.8448195315337));
#52539=CARTESIAN_POINT('Ctrl Pts',(-0.362766724344341,5.90613145959774,
41.8912106840076));
#52540=CARTESIAN_POINT('Ctrl Pts',(-1.34615518331167,5.84572972075092,41.9376018364816));
#52541=CARTESIAN_POINT('Ctrl Pts',(-2.31413060817627,5.53439149987867,41.9839929889556));
#52542=CARTESIAN_POINT('Ctrl Pts',(-3.14834104142876,5.01018335005785,42.0303841414296));
#52543=CARTESIAN_POINT('Ctrl Pts',(-3.9825514746812,4.48597520023706,42.0767752939036));
#52544=CARTESIAN_POINT('Ctrl Pts',(-4.68299691632168,3.74889712146773,42.1231664463775));
#52545=CARTESIAN_POINT('Ctrl Pts',(-5.16403563721432,2.88906982468789,42.1695575988515));
#52546=CARTESIAN_POINT('Ctrl Pts',(-5.64507435810699,2.029242527908,42.2159487513255));
#52547=CARTESIAN_POINT('Ctrl Pts',(-5.90670635825177,1.04666601311763,42.2623399037995));
#52548=CARTESIAN_POINT('Ctrl Pts',(-5.91694254105722,0.0614774769239503,
42.3087310562735));
#52549=CARTESIAN_POINT('Ctrl Pts',(-5.91715537596208,0.0409930334200531,
42.3096956401141));
#52550=CARTESIAN_POINT('Ctrl Pts',(-5.91725952634774,0.0205074606758483,
42.3106602239546));
#52551=CARTESIAN_POINT('Ctrl Pts',(-5.91725525726564,2.18443538467081E-5,
42.3116248077952));
#52552=CARTESIAN_POINT('Origin',(0.,0.,0.));
#52553=CARTESIAN_POINT('',(-5.91625748489978,-4.2193274442659E-5,44.3133751922049));
#52554=CARTESIAN_POINT('',(-5.91631318557293,-8.34923490093236E-5,44.0616248077952));
#52555=CARTESIAN_POINT('',(-5.91675,-7.2459289488551E-16,0.));
#52556=CARTESIAN_POINT('Ctrl Pts',(-5.91625748489978,-4.2193274442659E-5,
44.3133751922049));
#52557=CARTESIAN_POINT('Ctrl Pts',(-5.91612386542984,0.538286346723986,
44.2880398101642));
#52558=CARTESIAN_POINT('Ctrl Pts',(-5.84331471980756,1.07665031667677,44.2627044281235));
#52559=CARTESIAN_POINT('Ctrl Pts',(-5.69829673740849,1.59480491302855,44.2373690460828));
#52560=CARTESIAN_POINT('Ctrl Pts',(-5.43275697478975,2.54358827243592,44.1909778936088));
#52561=CARTESIAN_POINT('Ctrl Pts',(-4.92511109810911,3.42461243326639,44.1445867411348));
#52562=CARTESIAN_POINT('Ctrl Pts',(-4.23742771126215,4.13015675368477,44.0981955886608));
#52563=CARTESIAN_POINT('Ctrl Pts',(-3.54974432441519,4.83570107410316,44.0518044361868));
#52564=CARTESIAN_POINT('Ctrl Pts',(-2.68202342740191,5.36576555410946,44.0054132837129));
#52565=CARTESIAN_POINT('Ctrl Pts',(-1.74035910494293,5.65554052271067,43.9590221312389));
#52566=CARTESIAN_POINT('Ctrl Pts',(-0.798694782483963,5.94531549131189,
43.9126309787649));
#52567=CARTESIAN_POINT('Ctrl Pts',(0.216912965420696,5.99480094850802,43.8662398262909));
#52568=CARTESIAN_POINT('Ctrl Pts',(1.18228829510979,5.79794643002389,43.8198486738169));
#52569=CARTESIAN_POINT('Ctrl Pts',(2.14766362479889,5.60109191153975,43.7734575213429));
#52570=CARTESIAN_POINT('Ctrl Pts',(3.06280653627241,5.15789741737534,43.727066368869));
#52571=CARTESIAN_POINT('Ctrl Pts',(3.8158247725667,4.522551240533,43.680675216395));
#52572=CARTESIAN_POINT('Ctrl Pts',(4.568843008861,3.88720506369065,43.634284063921));
#52573=CARTESIAN_POINT('Ctrl Pts',(5.15973656997605,3.05970720417037,43.587892911447));
#52574=CARTESIAN_POINT('Ctrl Pts',(5.51625836384621,2.14123377553155,43.541501758973));
#52575=CARTESIAN_POINT('Ctrl Pts',(5.87278015771636,1.22276034689272,43.495110606499));
#52576=CARTESIAN_POINT('Ctrl Pts',(5.99493018434163,0.213311349135362,43.448719454025));
#52577=CARTESIAN_POINT('Ctrl Pts',(5.8677734625339,-0.763690389204473,43.4023283015511));
#52578=CARTESIAN_POINT('Ctrl Pts',(5.74061674072617,-1.74069212754431,43.3559371490771));
#52579=CARTESIAN_POINT('Ctrl Pts',(5.36415327048545,-2.68524660646662,43.3095459966031));
#52580=CARTESIAN_POINT('Ctrl Pts',(4.78441230781263,-3.48186548950865,43.2631548441291));
#52581=CARTESIAN_POINT('Ctrl Pts',(4.20467134513981,-4.27848437255069,43.2167636916552));
#52582=CARTESIAN_POINT('Ctrl Pts',(3.42165289003488,-4.92716765971245,43.1703725391812));
#52583=CARTESIAN_POINT('Ctrl Pts',(2.53109466945551,-5.34860245227052,43.1239813867072));
#52584=CARTESIAN_POINT('Ctrl Pts',(1.64053644887615,-5.77003724482859,43.0775902342332));
#52585=CARTESIAN_POINT('Ctrl Pts',(0.642438462822346,-5.96422354278298,
43.0311990817592));
#52586=CARTESIAN_POINT('Ctrl Pts',(-0.34116432025421,-5.90741866848506,
42.9848079292852));
#52587=CARTESIAN_POINT('Ctrl Pts',(-1.32476710333077,-5.85061379418714,
42.9384167768112));
#52588=CARTESIAN_POINT('Ctrl Pts',(-2.29387468343007,-5.54281774763692,
42.8920256243373));
#52589=CARTESIAN_POINT('Ctrl Pts',(-3.12999667722686,-5.02166398903084,
42.8456344718633));
#52590=CARTESIAN_POINT('Ctrl Pts',(-3.96611867102364,-4.50051023042476,
42.7992433193893));
#52591=CARTESIAN_POINT('Ctrl Pts',(-4.6692550785179,-3.76599875976282,42.7528521669153));
#52592=CARTESIAN_POINT('Ctrl Pts',(-5.15343515284433,-2.90793647516735,
42.7064610144413));
#52593=CARTESIAN_POINT('Ctrl Pts',(-5.63761522717078,-2.04987419057183,
42.6600698619673));
#52594=CARTESIAN_POINT('Ctrl Pts',(-5.90283896832939,-1.06826109204276,
42.6136787094933));
#52595=CARTESIAN_POINT('Ctrl Pts',(-5.91667812645172,-0.0831165816674949,
42.5672875570194));
#52596=CARTESIAN_POINT('Ctrl Pts',(-5.91706716496741,-0.0554227613734876,
42.5659834354146));
#52597=CARTESIAN_POINT('Ctrl Pts',(-5.91725754619806,-0.0277261503725831,
42.5646793138097));
#52598=CARTESIAN_POINT('Ctrl Pts',(-5.9172499153618,-2.94340949030803E-5,
42.5633751922049));
#52599=CARTESIAN_POINT('Ctrl Pts',(-5.91725525726564,2.18443538467081E-5,
42.3116248077952));
#52600=CARTESIAN_POINT('Ctrl Pts',(-5.9170542070895,-0.96473748158776,42.3570513764286));
#52601=CARTESIAN_POINT('Ctrl Pts',(-5.67639075946303,-1.92959345826523,
42.402477945062));
#52602=CARTESIAN_POINT('Ctrl Pts',(-5.22294962861403,-2.78114826848592,
42.4479045136954));
#52603=CARTESIAN_POINT('Ctrl Pts',(-4.75988016789937,-3.65078492010495,
42.4942956661694));
#52604=CARTESIAN_POINT('Ctrl Pts',(-4.07490088100393,-4.40225766574615,
42.5406868186434));
#52605=CARTESIAN_POINT('Ctrl Pts',(-3.25176248863289,-4.94368579420877,
42.5870779711174));
#52606=CARTESIAN_POINT('Ctrl Pts',(-2.42862409626176,-5.48511392267146,
42.6334691235913));
#52607=CARTESIAN_POINT('Ctrl Pts',(-1.46732659841493,-5.81649743395556,
42.6798602760653));
#52608=CARTESIAN_POINT('Ctrl Pts',(-0.485405459006441,-5.89731888697808,
42.7262514285393));
#52609=CARTESIAN_POINT('Ctrl Pts',(0.496515680401994,-5.97814034000059,
42.7726425810133));
#52610=CARTESIAN_POINT('Ctrl Pts',(1.49906046137198,-5.8083997347616,42.8190337334873));
#52611=CARTESIAN_POINT('Ctrl Pts',(2.3996502168525,-5.40885083461371,42.8654248859613));
#52612=CARTESIAN_POINT('Ctrl Pts',(3.30023997233296,-5.00930193446583,42.9118160384352));
#52613=CARTESIAN_POINT('Ctrl Pts',(4.09887470232382,-4.37994473940907,42.9582071909092));
#52614=CARTESIAN_POINT('Ctrl Pts',(4.69790731661882,-3.59772919475618,43.0045983433832));
#52615=CARTESIAN_POINT('Ctrl Pts',(5.2969399309139,-2.81551365010321,43.0509894958572));
#52616=CARTESIAN_POINT('Ctrl Pts',(5.69637042951309,-1.88043975585402,43.0973806483312));
#52617=CARTESIAN_POINT('Ctrl Pts',(5.84736143474778,-0.906836680867013,
43.1437718008052));
#52618=CARTESIAN_POINT('Ctrl Pts',(5.99835243998247,0.0667663941199431,
43.1901629532792));
#52619=CARTESIAN_POINT('Ctrl Pts',(5.90090395185268,1.07889864984477,43.2365541057531));
#52620=CARTESIAN_POINT('Ctrl Pts',(5.56693075562074,2.00580918246615,43.2829452582271));
#52621=CARTESIAN_POINT('Ctrl Pts',(5.2329575593888,2.93271971508754,43.3293364107011));
#52622=CARTESIAN_POINT('Ctrl Pts',(4.66245965505468,3.77440852460552,43.3757275631751));
#52623=CARTESIAN_POINT('Ctrl Pts',(3.92519040824982,4.42796440515563,43.4221187156491));
#52624=CARTESIAN_POINT('Ctrl Pts',(3.18792116144496,5.08152028570573,43.4685098681231));
#52625=CARTESIAN_POINT('Ctrl Pts',(2.28388057216931,5.546943237288,43.5149010205971));
#52626=CARTESIAN_POINT('Ctrl Pts',(1.32360344395206,5.7673271484718,43.561292173071));
#52627=CARTESIAN_POINT('Ctrl Pts',(0.363326315734754,5.98771105965562,43.607683325545));
#52628=CARTESIAN_POINT('Ctrl Pts',(-0.653187351424031,5.96305593044097,
43.654074478019));
#52629=CARTESIAN_POINT('Ctrl Pts',(-1.60165094936008,5.69637628240582,43.700465630493));
#52630=CARTESIAN_POINT('Ctrl Pts',(-2.55011454729602,5.4296966343707,43.746856782967));
#52631=CARTESIAN_POINT('Ctrl Pts',(-3.43052807600912,4.92099246751511,43.793247935441));
#52632=CARTESIAN_POINT('Ctrl Pts',(-4.13524555414061,4.23246178025295,43.839639087915));
#52633=CARTESIAN_POINT('Ctrl Pts',(-4.83996303227218,3.5439310929907,43.8860302403889));
#52634=CARTESIAN_POINT('Ctrl Pts',(-5.36898445982214,2.67557388532179,43.9324213928629));
#52635=CARTESIAN_POINT('Ctrl Pts',(-5.65762769723763,1.73356204209462,43.9788125453369));
#52636=CARTESIAN_POINT('Ctrl Pts',(-5.82937883410267,1.17303754665422,44.006416632823));
#52637=CARTESIAN_POINT('Ctrl Pts',(-5.91602174695989,0.58643491484543,44.0340207203091));
#52638=CARTESIAN_POINT('Ctrl Pts',(-5.91631318557293,-8.34923490093236E-5,
44.0616248077952));
#52639=CARTESIAN_POINT('Origin',(0.,0.,0.));
#52640=CARTESIAN_POINT('',(-5.91708074246689,0.000111828887577881,46.0633751922049));
#52641=CARTESIAN_POINT('',(-5.9169414605903,0.000139691133403882,45.8116248077952));
#52642=CARTESIAN_POINT('',(-5.91675,-7.2459289488551E-16,0.));
#52643=CARTESIAN_POINT('Ctrl Pts',(-5.91708074246689,0.000111828887577881,
46.0633751922049));
#52644=CARTESIAN_POINT('Ctrl Pts',(-5.91718319560474,0.118708057921104,
46.0577914589927));
#52645=CARTESIAN_POINT('Ctrl Pts',(-5.91369093890245,0.237298258279482,
46.0522077257804));
#52646=CARTESIAN_POINT('Ctrl Pts',(-5.90656309521846,0.355669538172284,
46.0466239925682));
#52647=CARTESIAN_POINT('Ctrl Pts',(-5.84734305898366,1.33912986575459,46.0002328400942));
#52648=CARTESIAN_POINT('Ctrl Pts',(-5.53716820162539,2.307478700597,45.9538416876202));
#52649=CARTESIAN_POINT('Ctrl Pts',(-5.01396283464526,3.14231842927739,45.9074505351462));
#52650=CARTESIAN_POINT('Ctrl Pts',(-4.49075746766513,3.97715815795778,45.8610593826722));
#52651=CARTESIAN_POINT('Ctrl Pts',(-3.75452159106314,4.67848878047613,45.8146682301982));
#52652=CARTESIAN_POINT('Ctrl Pts',(-2.89527294180451,5.1605603388232,45.7682770777242));
#52653=CARTESIAN_POINT('Ctrl Pts',(-2.03602429254593,5.64263189717024,45.7218859252502));
#52654=CARTESIAN_POINT('Ctrl Pts',(-1.05376287063074,5.90544439134602,45.6754947727763));
#52655=CARTESIAN_POINT('Ctrl Pts',(-0.06858734704076,5.91686438867803,45.6291036203023));
#52656=CARTESIAN_POINT('Ctrl Pts',(0.916588176549275,5.92828438601003,45.5827124678283));
#52657=CARTESIAN_POINT('Ctrl Pts',(1.90467780181407,5.68831188649823,45.5363213153544));
#52658=CARTESIAN_POINT('Ctrl Pts',(2.77487025778479,5.22628773324257,45.4899301628804));
#52659=CARTESIAN_POINT('Ctrl Pts',(3.64506271375556,4.76426357998688,45.4435390104064));
#52660=CARTESIAN_POINT('Ctrl Pts',(4.3973580004322,4.08018777298733,45.3971478579324));
#52661=CARTESIAN_POINT('Ctrl Pts',(4.93977483655907,3.25770056670009,45.3507567054584));
#52662=CARTESIAN_POINT('Ctrl Pts',(5.48219167268588,2.43521336041294,45.3043655529844));
#52663=CARTESIAN_POINT('Ctrl Pts',(5.81473005826294,1.47431475483818,45.2579744005104));
#52664=CARTESIAN_POINT('Ctrl Pts',(5.89673134858815,0.492491442319647,45.2115832480365));
#52665=CARTESIAN_POINT('Ctrl Pts',(5.97873263891336,-0.489331870198937,
45.1651920955625));
#52666=CARTESIAN_POINT('Ctrl Pts',(5.81019683398663,-1.4920798896614,45.1188009430885));
#52667=CARTESIAN_POINT('Ctrl Pts',(5.41173038921079,-2.39314909954912,45.0724097906145));
#52668=CARTESIAN_POINT('Ctrl Pts',(5.01326394443495,-3.29421830943683,45.0260186381405));
#52669=CARTESIAN_POINT('Ctrl Pts',(4.38486685980999,-4.09360870974991,44.9796274856665));
#52670=CARTESIAN_POINT('Ctrl Pts',(3.60337169032434,-4.69358081634368,44.9332363331926));
#52671=CARTESIAN_POINT('Ctrl Pts',(2.8218765208387,-5.29355292293745,44.8868451807186));
#52672=CARTESIAN_POINT('Ctrl Pts',(1.88728326649239,-5.69410673581187,44.8404540282446));
#52673=CARTESIAN_POINT('Ctrl Pts',(0.913862329493332,-5.84626753244438,
44.7940628757706));
#52674=CARTESIAN_POINT('Ctrl Pts',(-0.0595586075057249,-5.9984283290769,
44.7476717232966));
#52675=CARTESIAN_POINT('Ctrl Pts',(-1.07180722715749,-5.9021961094675,44.7012805708226));
#52676=CARTESIAN_POINT('Ctrl Pts',(-1.99911839809162,-5.56933694873922,
44.6548894183486));
#52677=CARTESIAN_POINT('Ctrl Pts',(-2.92642956902575,-5.23647778801094,
44.6084982658746));
#52678=CARTESIAN_POINT('Ctrl Pts',(-3.76880329124222,-4.66699168616381,
44.5621071134007));
#52679=CARTESIAN_POINT('Ctrl Pts',(-4.42324461629749,-3.93050829824535,
44.5157159609267));
#52680=CARTESIAN_POINT('Ctrl Pts',(-5.07768594135277,-3.19402491032689,
44.4693248084527));
#52681=CARTESIAN_POINT('Ctrl Pts',(-5.54419486924684,-2.29054423633713,
44.4229336559787));
#52682=CARTESIAN_POINT('Ctrl Pts',(-5.76573250891546,-1.33053262035011,
44.3765425035047));
#52683=CARTESIAN_POINT('Ctrl Pts',(-5.8662828387614,-0.8948076357027,44.3554867330715));
#52684=CARTESIAN_POINT('Ctrl Pts',(-5.91636853358576,-0.447437150164224,
44.3344309626382));
#52685=CARTESIAN_POINT('Ctrl Pts',(-5.91625748489978,-4.2193274442659E-5,
44.3133751922049));
#52686=CARTESIAN_POINT('Ctrl Pts',(-5.91631318557293,-8.34923490093236E-5,
44.0616248077952));
#52687=CARTESIAN_POINT('Ctrl Pts',(-5.91651153576893,-0.399262035675468,
44.0804118727831));
#52688=CARTESIAN_POINT('Ctrl Pts',(-5.87671164968556,-0.798401565932907,
44.099198937771));
#52689=CARTESIAN_POINT('Ctrl Pts',(-5.79652159130293,-1.18925436972102,
44.1179860027589));
#52690=CARTESIAN_POINT('Ctrl Pts',(-5.59850720067171,-2.15439245952413,
44.1643771552329));
#52691=CARTESIAN_POINT('Ctrl Pts',(-5.15421337212823,-3.06900216034495,
44.2107683077068));
#52692=CARTESIAN_POINT('Ctrl Pts',(-4.51796281156627,-3.82125640956555,
44.2571594601808));
#52693=CARTESIAN_POINT('Ctrl Pts',(-3.88171225100428,-4.57351065878619,
44.3035506126548));
#52694=CARTESIAN_POINT('Ctrl Pts',(-3.05350495842378,-5.16340945640659,
44.3499417651288));
#52695=CARTESIAN_POINT('Ctrl Pts',(-2.1346037880072,-5.51882733762952,44.3963329176028));
#52696=CARTESIAN_POINT('Ctrl Pts',(-1.21570261759073,-5.87424521885241,
44.4427240700767));
#52697=CARTESIAN_POINT('Ctrl Pts',(-0.206107569338182,-5.99518218367789,
44.4891152225507));
#52698=CARTESIAN_POINT('Ctrl Pts',(0.770740670982104,-5.86685156897937,
44.5355063750247));
#52699=CARTESIAN_POINT('Ctrl Pts',(1.7475889113025,-5.73852095428082,44.5818975274987));
#52700=CARTESIAN_POINT('Ctrl Pts',(2.69169034369063,-5.36092276005821,44.6282886799727));
#52701=CARTESIAN_POINT('Ctrl Pts',(3.48761202456127,-4.78022498220296,44.6746798324467));
#52702=CARTESIAN_POINT('Ctrl Pts',(4.2835337054319,-4.1995272043477,44.7210709849206));
#52703=CARTESIAN_POINT('Ctrl Pts',(4.93127563478503,-3.41572984285981,44.7674621373946));
#52704=CARTESIAN_POINT('Ctrl Pts',(5.35164001138475,-2.52466585965103,44.8138532898686));
#52705=CARTESIAN_POINT('Ctrl Pts',(5.77200438798442,-1.63360187644235,44.8602444423426));
#52706=CARTESIAN_POINT('Ctrl Pts',(5.96499121183073,-0.635271271512821,
44.9066355948166));
#52707=CARTESIAN_POINT('Ctrl Pts',(5.90700446200314,0.348262544952162,44.9530267472906));
#52708=CARTESIAN_POINT('Ctrl Pts',(5.84901771217555,1.3317963614172,44.9994178997646));
#52709=CARTESIAN_POINT('Ctrl Pts',(5.54005738867404,2.30053338941769,45.0458090522385));
#52710=CARTESIAN_POINT('Ctrl Pts',(5.01789930495395,3.1360285521156,45.0922002047125));
#52711=CARTESIAN_POINT('Ctrl Pts',(4.49574122123386,3.97152371481352,45.1385913571865));
#52712=CARTESIAN_POINT('Ctrl Pts',(3.76038537729519,4.67377701220886,45.1849825096605));
#52713=CARTESIAN_POINT('Ctrl Pts',(2.90174191068929,5.15692567312065,45.2313736621345));
#52714=CARTESIAN_POINT('Ctrl Pts',(2.04309844408339,5.64007433403244,45.2777648146084));
#52715=CARTESIAN_POINT('Ctrl Pts',(1.06116735481026,5.90411835846068,45.3241559670825));
#52716=CARTESIAN_POINT('Ctrl Pts',(0.0760069248978496,5.91677373757939,
45.3705471195564));
#52717=CARTESIAN_POINT('Ctrl Pts',(-0.909153505014565,5.9294291166981,45.4169382720304));
#52718=CARTESIAN_POINT('Ctrl Pts',(-1.89754327556627,5.69069585050728,45.4633294245044));
#52719=CARTESIAN_POINT('Ctrl Pts',(-2.76831441776762,5.22976326411833,45.5097205769784));
#52720=CARTESIAN_POINT('Ctrl Pts',(-3.63908555996897,4.76883067772938,45.5561117294523));
#52721=CARTESIAN_POINT('Ctrl Pts',(-4.39223807381997,4.0856987711423,45.6025028819263));
#52722=CARTESIAN_POINT('Ctrl Pts',(-4.93568586702171,3.26389239044791,45.6488940344003));
#52723=CARTESIAN_POINT('Ctrl Pts',(-5.47913366022345,2.44208600975352,45.6952851868743));
#52724=CARTESIAN_POINT('Ctrl Pts',(-5.81287673277592,1.48160515495182,45.7416763393483));
#52725=CARTESIAN_POINT('Ctrl Pts',(-5.89610914588454,0.499885441034465,
45.7880674918223));
#52726=CARTESIAN_POINT('Ctrl Pts',(-5.91019755247519,0.333713802232241,
45.7959199304799));
#52727=CARTESIAN_POINT('Ctrl Pts',(-5.91710859473939,0.166933650282954,
45.8037723691375));
#52728=CARTESIAN_POINT('Ctrl Pts',(-5.9169414605903,0.000139691133403882,
45.8116248077952));
#52729=CARTESIAN_POINT('Origin',(0.,0.,0.));
#52730=CARTESIAN_POINT('',(-5.9165283748373,-0.000142876380609669,47.8133751922049));
#52731=CARTESIAN_POINT('',(-5.91667009430184,-0.00015435290976692,47.5616248077952));
#52732=CARTESIAN_POINT('',(-5.91675,-7.2459289488551E-16,0.));
#52733=CARTESIAN_POINT('Ctrl Pts',(-5.9165283748373,-0.000142876380609669,
47.8133751922049));
#52734=CARTESIAN_POINT('Ctrl Pts',(-5.91591637761327,0.684449648370852,
47.7811519553471));
#52735=CARTESIAN_POINT('Ctrl Pts',(-5.79719566143619,1.36924892251219,47.7489287184894));
#52736=CARTESIAN_POINT('Ctrl Pts',(-5.56441112577014,2.01278842444649,47.7167054816317));
#52737=CARTESIAN_POINT('Ctrl Pts',(-5.22927586498499,2.93927943120176,47.6703143291577));
#52738=CARTESIAN_POINT('Ctrl Pts',(-4.65772294875219,3.78025218463893,47.6239231766836));
#52739=CARTESIAN_POINT('Ctrl Pts',(-3.91963473639474,4.43288302929686,47.5775320242096));
#52740=CARTESIAN_POINT('Ctrl Pts',(-3.18154652403728,5.08551387395478,47.5311408717356));
#52741=CARTESIAN_POINT('Ctrl Pts',(-2.27692301555514,5.54980280983347,47.4847497192617));
#52742=CARTESIAN_POINT('Ctrl Pts',(-1.31637028656497,5.76898237879343,47.4383585667877));
#52743=CARTESIAN_POINT('Ctrl Pts',(-0.355817557574798,5.98816194775339,
47.3919674143137));
#52744=CARTESIAN_POINT('Ctrl Pts',(0.660664391923433,5.96223214979463,47.3455762618397));
#52745=CARTESIAN_POINT('Ctrl Pts',(1.608792831805,5.69436335708507,47.2991851093657));
#52746=CARTESIAN_POINT('Ctrl Pts',(2.55692127168663,5.4264945643755,47.2527939568917));
#52747=CARTESIAN_POINT('Ctrl Pts',(3.43669620195162,4.91668677691509,47.2064028044177));
#52748=CARTESIAN_POINT('Ctrl Pts',(4.14054972109162,4.22727293007542,47.1600116519438));
#52749=CARTESIAN_POINT('Ctrl Pts',(4.84440324023159,3.53785908323578,47.1136204994698));
#52750=CARTESIAN_POINT('Ctrl Pts',(5.37233534824662,2.66883917701688,47.0672293469958));
#52751=CARTESIAN_POINT('Ctrl Pts',(5.65979709398515,1.72646612277727,47.0208381945218));
#52752=CARTESIAN_POINT('Ctrl Pts',(5.94725883972366,0.784093068537711,46.9744470420478));
#52753=CARTESIAN_POINT('Ctrl Pts',(5.99425022318572,-0.231633133722414,
46.9280558895739));
#52754=CARTESIAN_POINT('Ctrl Pts',(5.79502572431377,-1.19652215722151,46.8816647370999));
#52755=CARTESIAN_POINT('Ctrl Pts',(5.59580122544179,-2.16141118072072,46.8352735846259));
#52756=CARTESIAN_POINT('Ctrl Pts',(5.15036084423571,-3.07546302545876,46.7888824321519));
#52757=CARTESIAN_POINT('Ctrl Pts',(4.51316747274337,-3.82691883649908,46.7424912796779));
#52758=CARTESIAN_POINT('Ctrl Pts',(3.87597410125107,-4.57837464753936,46.6961001272039));
#52759=CARTESIAN_POINT('Ctrl Pts',(3.0470277394725,-5.16723442488198,46.64970897473));
#52760=CARTESIAN_POINT('Ctrl Pts',(2.12768160575026,-5.52149974216538,46.603317822256));
#52761=CARTESIAN_POINT('Ctrl Pts',(1.20833547202802,-5.87576505944878,46.556926669782));
#52762=CARTESIAN_POINT('Ctrl Pts',(0.19858956636208,-5.99543591667298,46.510535517308));
#52763=CARTESIAN_POINT('Ctrl Pts',(-0.778096980516938,-5.86588045455162,
46.464144364834));
#52764=CARTESIAN_POINT('Ctrl Pts',(-1.75478352739596,-5.73632499243026,
46.41775321236));
#52765=CARTESIAN_POINT('Ctrl Pts',(-2.69841071548808,-5.35754321096334,
46.3713620598861));
#52766=CARTESIAN_POINT('Ctrl Pts',(-3.49360358588342,-4.77584782032288,
46.3249709074121));
#52767=CARTESIAN_POINT('Ctrl Pts',(-4.28879645627876,-4.19415242968242,
46.2785797549381));
#52768=CARTESIAN_POINT('Ctrl Pts',(-4.93555500897735,-3.40954342986841,
46.2321886024641));
#52769=CARTESIAN_POINT('Ctrl Pts',(-5.35480167777096,-2.51795301980031,
46.1857974499901));
#52770=CARTESIAN_POINT('Ctrl Pts',(-5.72358696710265,-1.73367624000276,
46.1449900307284));
#52771=CARTESIAN_POINT('Ctrl Pts',(-5.91633198746874,-0.866621207429096,
46.1041826114666));
#52772=CARTESIAN_POINT('Ctrl Pts',(-5.91708074246689,0.000111828887577881,
46.0633751922049));
#52773=CARTESIAN_POINT('Ctrl Pts',(-5.9169414605903,0.000139691133403882,
45.8116248077952));
#52774=CARTESIAN_POINT('Ctrl Pts',(-5.91612118864406,-0.818462648626552,
45.8501635216115));
#52775=CARTESIAN_POINT('Ctrl Pts',(-5.74480785464818,-1.63739756442216,
45.8887022354279));
#52776=CARTESIAN_POINT('Ctrl Pts',(-5.41472710370765,-2.38636101768265,
45.9272409492443));
#52777=CARTESIAN_POINT('Ctrl Pts',(-5.01739089475736,-3.2879291894494,45.9736321017182));
#52778=CARTESIAN_POINT('Ctrl Pts',(-4.38999672319199,-4.08810695994993,
46.0200232541922));
#52779=CARTESIAN_POINT('Ctrl Pts',(-3.60925452030443,-4.689058575237,46.0664144066662));
#52780=CARTESIAN_POINT('Ctrl Pts',(-2.82851231741688,-5.29001019052406,
46.1128055591401));
#52781=CARTESIAN_POINT('Ctrl Pts',(-1.89442208320712,-5.69173565059769,
46.1591967116142));
#52782=CARTESIAN_POINT('Ctrl Pts',(-0.921192716857027,-5.84511697853441,
46.2055878640882));
#52783=CARTESIAN_POINT('Ctrl Pts',(0.0520366494930682,-5.99849830647113,
46.2519790165621));
#52784=CARTESIAN_POINT('Ctrl Pts',(1.06440514798353,-5.90353550227096,46.2983701690361));
#52785=CARTESIAN_POINT('Ctrl Pts',(1.99213298995529,-5.57183943277922,46.3447613215101));
#52786=CARTESIAN_POINT('Ctrl Pts',(2.91986083192704,-5.24014336328747,46.3911524739841));
#52787=CARTESIAN_POINT('Ctrl Pts',(3.76294801738013,-4.67171402850415,46.4375436264581));
#52788=CARTESIAN_POINT('Ctrl Pts',(4.41831236448827,-3.93605187518555,46.4839347789321));
#52789=CARTESIAN_POINT('Ctrl Pts',(5.07367671159642,-3.20038972186696,46.530325931406));
#52790=CARTESIAN_POINT('Ctrl Pts',(5.54131822035965,-2.29749475001306,46.57671708388));
#52791=CARTESIAN_POINT('Ctrl Pts',(5.76405952185625,-1.3377616913486,46.623108236354));
#52792=CARTESIAN_POINT('Ctrl Pts',(5.98680082335285,-0.378028632684144,
46.6694993888279));
#52793=CARTESIAN_POINT('Ctrl Pts',(5.96464191758284,0.638542512790754,46.715890541302));
#52794=CARTESIAN_POINT('Ctrl Pts',(5.70029211906678,1.58765810918055,46.762281693776));
#52795=CARTESIAN_POINT('Ctrl Pts',(5.43594232055071,2.53677370557039,46.8086728462499));
#52796=CARTESIAN_POINT('Ctrl Pts',(4.92940162928853,3.418433752875,46.8550639987239));
#52797=CARTESIAN_POINT('Ctrl Pts',(4.24260352089231,4.12483986099506,46.9014551511979));
#52798=CARTESIAN_POINT('Ctrl Pts',(3.55580541249617,4.83124596911503,46.9478463036719));
#52799=CARTESIAN_POINT('Ctrl Pts',(2.68874988696585,5.3623981380506,46.9942374561459));
#52800=CARTESIAN_POINT('Ctrl Pts',(1.74744967569917,5.6533537077774,47.0406286086199));
#52801=CARTESIAN_POINT('Ctrl Pts',(0.806149464432386,5.94430927750424,47.0870197610938));
#52802=CARTESIAN_POINT('Ctrl Pts',(-0.20939543257075,5.99506824802238,47.1334109135677));
#52803=CARTESIAN_POINT('Ctrl Pts',(-1.17501685627332,5.79942444573728,47.1798020660417));
#52804=CARTESIAN_POINT('Ctrl Pts',(-2.14063827997589,5.60378064345219,47.2261932185157));
#52805=CARTESIAN_POINT('Ctrl Pts',(-3.05633623037776,5.16173406836383,47.2725843709898));
#52806=CARTESIAN_POINT('Ctrl Pts',(-3.81015058728028,4.52733266025254,47.3189755234638));
#52807=CARTESIAN_POINT('Ctrl Pts',(-4.56396494418272,3.89293125214132,47.3653666759378));
#52808=CARTESIAN_POINT('Ctrl Pts',(-5.15589570758587,3.06617501100719,47.4117578284117));
#52809=CARTESIAN_POINT('Ctrl Pts',(-5.51356896926947,2.14814937456649,47.4581489808856));
#52810=CARTESIAN_POINT('Ctrl Pts',(-5.77949996790739,1.46559493053359,47.4926409231888));
#52811=CARTESIAN_POINT('Ctrl Pts',(-5.91593433074091,0.732587119768138,
47.527132865492));
#52812=CARTESIAN_POINT('Ctrl Pts',(-5.91667009430184,-0.00015435290976692,
47.5616248077952));
#52813=CARTESIAN_POINT('Origin',(0.,0.,0.));
#52814=CARTESIAN_POINT('',(-5.91663288208029,0.000152735557782668,49.5633751922049));
#52815=CARTESIAN_POINT('',(-5.91649558673351,0.000137928394543142,49.3116248077952));
#52816=CARTESIAN_POINT('',(-5.91675,-7.2459289488551E-16,0.));
#52817=CARTESIAN_POINT('Ctrl Pts',(-5.91663288208029,0.000152735557782668,
49.5633751922049));
#52818=CARTESIAN_POINT('Ctrl Pts',(-5.91689330738711,0.265102003771003,
49.5509036041756));
#52819=CARTESIAN_POINT('Ctrl Pts',(-5.89942583762255,0.530017195188502,
49.5384320161463));
#52820=CARTESIAN_POINT('Ctrl Pts',(-5.86395207547737,0.792498879926616,
49.525960428117));
#52821=CARTESIAN_POINT('Ctrl Pts',(-5.73199865425815,1.76886434595278,49.479569275643));
#52822=CARTESIAN_POINT('Ctrl Pts',(-5.35090084560841,2.71155855316966,49.433178123169));
#52823=CARTESIAN_POINT('Ctrl Pts',(-4.76725453460696,3.50532061592798,49.386786970695));
#52824=CARTESIAN_POINT('Ctrl Pts',(-4.18360822360548,4.29908267868635,49.340395818221));
#52825=CARTESIAN_POINT('Ctrl Pts',(-3.39741341025227,4.94391259698615,49.294004665747));
#52826=CARTESIAN_POINT('Ctrl Pts',(-2.50479618696016,5.36096861396988,49.2476135132731));
#52827=CARTESIAN_POINT('Ctrl Pts',(-1.61217896366814,5.77802463095356,49.2012223607991));
#52828=CARTESIAN_POINT('Ctrl Pts',(-0.613139330437237,5.96730674662122,
49.1548312083251));
#52829=CARTESIAN_POINT('Ctrl Pts',(0.370172611413013,5.9056719055447,49.1084400558511));
#52830=CARTESIAN_POINT('Ctrl Pts',(1.35348455326337,5.84403706446818,49.0620489033771));
#52831=CARTESIAN_POINT('Ctrl Pts',(2.32106880373308,5.53148526664742,49.0156577509031));
#52832=CARTESIAN_POINT('Ctrl Pts',(3.15462123323734,5.00623144620666,48.9692665984291));
#52833=CARTESIAN_POINT('Ctrl Pts',(3.98817366274155,4.48097762576594,48.9228754459552));
#52834=CARTESIAN_POINT('Ctrl Pts',(4.68769427128033,3.74302178270524,48.8764842934812));
#52835=CARTESIAN_POINT('Ctrl Pts',(5.16765440677028,2.88259195002832,48.8300931410072));
#52836=CARTESIAN_POINT('Ctrl Pts',(5.64761454226022,2.02216211735141,48.7837019885332));
#52837=CARTESIAN_POINT('Ctrl Pts',(5.90801420470134,1.03925829505829,48.7373108360592));
#52838=CARTESIAN_POINT('Ctrl Pts',(5.91701497238067,0.054057698833775,48.6909196835852));
#52839=CARTESIAN_POINT('Ctrl Pts',(5.92601574006001,-0.931142897390738,
48.6445285311112));
#52840=CARTESIAN_POINT('Ctrl Pts',(5.68361761297757,-1.91864026754664,48.5981373786373));
#52841=CARTESIAN_POINT('Ctrl Pts',(5.21945800970806,-2.78769555423019,48.5517462261633));
#52842=CARTESIAN_POINT('Ctrl Pts',(4.75529840643854,-3.65675084091374,48.5053550736894));
#52843=CARTESIAN_POINT('Ctrl Pts',(4.06937732698195,-4.40736404412495,48.4589639212153));
#52844=CARTESIAN_POINT('Ctrl Pts',(3.24556064268704,-4.94775954678693,48.4125727687413));
#52845=CARTESIAN_POINT('Ctrl Pts',(2.42174395839217,-5.48815504944887,48.3661816162673));
#52846=CARTESIAN_POINT('Ctrl Pts',(1.460031669259,-5.8183328515616,48.3197904637934));
#52847=CARTESIAN_POINT('Ctrl Pts',(0.4780099547046,-5.89792293111597,48.2733993113195));
#52848=CARTESIAN_POINT('Ctrl Pts',(-0.504011759849913,-5.97751301067036,
48.2270081588455));
#52849=CARTESIAN_POINT('Ctrl Pts',(-1.50634289982566,-5.80651536766633,
48.1806170063714));
#52850=CARTESIAN_POINT('Ctrl Pts',(-2.40643091952649,-5.40583746035036,
48.1342258538974));
#52851=CARTESIAN_POINT('Ctrl Pts',(-3.30651893922726,-5.00515955303441,
48.0878347014234));
#52852=CARTESIAN_POINT('Ctrl Pts',(-4.10436383865314,-4.37480138140656,
48.0414435489495));
#52853=CARTESIAN_POINT('Ctrl Pts',(-4.70241509822463,-3.59183527770545,
47.9950523964756));
#52854=CARTESIAN_POINT('Ctrl Pts',(-5.30046635779612,-2.80886917400434,
47.9486612440016));
#52855=CARTESIAN_POINT('Ctrl Pts',(-5.69872397751323,-1.87329513822997,
47.9022700915275));
#52856=CARTESIAN_POINT('Ctrl Pts',(-5.84849398470302,-0.89950349030608,
47.8558789390535));
#52857=CARTESIAN_POINT('Ctrl Pts',(-5.89423393101919,-0.602106310891314,
47.8417110234373));
#52858=CARTESIAN_POINT('Ctrl Pts',(-5.91679745783059,-0.301144577885169,
47.8275431078211));
#52859=CARTESIAN_POINT('Ctrl Pts',(-5.9165283748373,-0.000142876380609669,
47.8133751922049));
#52860=CARTESIAN_POINT('Ctrl Pts',(-5.91667009430184,-0.00015435290976692,
47.5616248077952));
#52861=CARTESIAN_POINT('Ctrl Pts',(-5.91692392185294,-0.252939328242564,
47.573524017966));
#52862=CARTESIAN_POINT('Ctrl Pts',(-5.90102760783804,-0.505692605401303,
47.5854232281369));
#52863=CARTESIAN_POINT('Ctrl Pts',(-5.86872650989343,-0.756331717182153,
47.5973224383077));
#52864=CARTESIAN_POINT('Ctrl Pts',(-5.74279502886973,-1.73349214074265,
47.6437135907817));
#52865=CARTESIAN_POINT('Ctrl Pts',(-5.3675163068583,-2.67851795611633,47.6901047432556));
#52866=CARTESIAN_POINT('Ctrl Pts',(-4.78877474362866,-3.4758631977001,47.7364958957296));
#52867=CARTESIAN_POINT('Ctrl Pts',(-4.21003318039895,-4.27320843928395,
47.7828870482035));
#52868=CARTESIAN_POINT('Ctrl Pts',(-3.427828775951,-4.92287310707781,47.8292782006776));
#52869=CARTESIAN_POINT('Ctrl Pts',(-2.53779972528504,-5.34542431137929,
47.8756693531516));
#52870=CARTESIAN_POINT('Ctrl Pts',(-1.64777067461913,-5.76797551568076,
47.9220605056256));
#52871=CARTESIAN_POINT('Ctrl Pts',(-0.649916977735285,-5.96341325648985,
47.9684516580995));
#52872=CARTESIAN_POINT('Ctrl Pts',(0.333756265546592,-5.90784184533997,
48.0148428105735));
#52873=CARTESIAN_POINT('Ctrl Pts',(1.31742950882841,-5.85227043419009,48.0612339630475));
#52874=CARTESIAN_POINT('Ctrl Pts',(2.28692229850836,-5.5456898710812,48.1076251155215));
#52875=CARTESIAN_POINT('Ctrl Pts',(3.12369715263964,-5.02558500206023,48.1540162679955));
#52876=CARTESIAN_POINT('Ctrl Pts',(3.96047200677097,-4.50548013303922,48.2004074204695));
#52877=CARTESIAN_POINT('Ctrl Pts',(4.66452892535374,-3.77185095810608,48.2467985729434));
#52878=CARTESIAN_POINT('Ctrl Pts',(5.14978461291203,-2.91439649926981,48.2931897254174));
#52879=CARTESIAN_POINT('Ctrl Pts',(5.63504030047034,-2.05694204043349,48.3395808778914));
#52880=CARTESIAN_POINT('Ctrl Pts',(5.90149475700412,-1.07566229769406,48.3859720303654));
#52881=CARTESIAN_POINT('Ctrl Pts',(5.91656925612452,-0.0905359145521563,
48.4323631828394));
#52882=CARTESIAN_POINT('Ctrl Pts',(5.93164375524491,0.894590468589636,48.4787543353134));
#52883=CARTESIAN_POINT('Ctrl Pts',(5.69533829695198,1.88356349213385,48.5251454877873));
#52884=CARTESIAN_POINT('Ctrl Pts',(5.23654536429916,2.75546387419225,48.5715366402613));
#52885=CARTESIAN_POINT('Ctrl Pts',(4.77775243164632,3.6273642562507,48.6179277927353));
#52886=CARTESIAN_POINT('Ctrl Pts',(4.09647202463357,4.38219199682328,48.6643189452093));
#52887=CARTESIAN_POINT('Ctrl Pts',(3.27600261108496,4.92765617778941,48.7107100976833));
#52888=CARTESIAN_POINT('Ctrl Pts',(2.45553319753639,5.47312035875552,48.7571012501573));
#52889=CARTESIAN_POINT('Ctrl Pts',(1.49587477745183,5.80922098011522,48.8034924026312));
#52890=CARTESIAN_POINT('Ctrl Pts',(0.514362408767521,5.89486385142087,48.8498835551052));
#52891=CARTESIAN_POINT('Ctrl Pts',(-0.467149959916903,5.98050672272653,
48.8962747075792));
#52892=CARTESIAN_POINT('Ctrl Pts',(-1.47051627720118,5.81569184397815,48.9426658600532));
#52893=CARTESIAN_POINT('Ctrl Pts',(-2.37305742882386,5.42057072215145,48.9890570125272));
#52894=CARTESIAN_POINT('Ctrl Pts',(-3.27559858044644,5.0254496003248,49.0354481650012));
#52895=CARTESIAN_POINT('Ctrl Pts',(-4.07731456640738,4.4000222354199,49.0818393174752));
#52896=CARTESIAN_POINT('Ctrl Pts',(-4.68018155896538,3.62075808215104,49.1282304699491));
#52897=CARTESIAN_POINT('Ctrl Pts',(-5.2830485515234,2.84149392888212,49.1746216224231));
#52898=CARTESIAN_POINT('Ctrl Pts',(-5.68706655067842,1.90839298724927,49.2210127748971));
#52899=CARTESIAN_POINT('Ctrl Pts',(-5.84283727643217,0.935543198081372,
49.2674039273711));
#52900=CARTESIAN_POINT('Ctrl Pts',(-5.89233176169344,0.626430562710378,
49.2821442208458));
#52901=CARTESIAN_POINT('Ctrl Pts',(-5.91676362954661,0.313304952112986,
49.2968845143205));
#52902=CARTESIAN_POINT('Ctrl Pts',(-5.91649558673351,0.000137928394543142,
49.3116248077952));
#52903=CARTESIAN_POINT('Origin',(0.,0.,0.));
#52904=CARTESIAN_POINT('',(-5.91697841467406,-0.000133927646978338,51.3133751922049));
#52905=CARTESIAN_POINT('',(-5.91711198123886,-0.000102791298586485,51.0616248077951));
#52906=CARTESIAN_POINT('',(-5.91675,-7.2459289488551E-16,0.));
#52907=CARTESIAN_POINT('Ctrl Pts',(-5.91697841467406,-0.000133927646978338,
51.3133751922049));
#52908=CARTESIAN_POINT('Ctrl Pts',(-5.9161664555486,0.830611330087965,51.27426410053));
#52909=CARTESIAN_POINT('Ctrl Pts',(-5.73957473098069,1.66169081825054,51.2351530088552));
#52910=CARTESIAN_POINT('Ctrl Pts',(-5.39991193444408,2.41969822879398,51.1960419171804));
#52911=CARTESIAN_POINT('Ctrl Pts',(-4.99702498066439,3.31879963080272,51.1496507647064));
#52912=CARTESIAN_POINT('Ctrl Pts',(-4.36470952307547,4.11509421835936,51.1032596122324));
#52913=CARTESIAN_POINT('Ctrl Pts',(-3.58027720642218,4.71122102467653,51.0568684597585));
#52914=CARTESIAN_POINT('Ctrl Pts',(-2.79584488976889,5.30734783099369,51.0104773072845));
#52915=CARTESIAN_POINT('Ctrl Pts',(-1.85929571405124,5.70330685607139,50.9640861548105));
#52916=CARTESIAN_POINT('Ctrl Pts',(-0.885139227138412,5.85068517070959,
50.9176950023365));
#52917=CARTESIAN_POINT('Ctrl Pts',(0.0890172597743667,5.99806348534778,
50.8713038498625));
#52918=CARTESIAN_POINT('Ctrl Pts',(1.10078105788233,5.89686108954651,50.8249126973885));
#52919=CARTESIAN_POINT('Ctrl Pts',(2.02644631374435,5.55945174956059,50.7785215449145));
#52920=CARTESIAN_POINT('Ctrl Pts',(2.95211156960648,5.22204240957463,50.7321303924405));
#52921=CARTESIAN_POINT('Ctrl Pts',(3.79167828322265,4.64842612540397,50.6857392399666));
#52922=CARTESIAN_POINT('Ctrl Pts',(4.44249471213787,3.90873753925835,50.6393480874926));
#52923=CARTESIAN_POINT('Ctrl Pts',(5.09331114105305,3.16904895311277,50.5929569350186));
#52924=CARTESIAN_POINT('Ctrl Pts',(5.5553772852673,2.26328806499226,50.5465657825446));
#52925=CARTESIAN_POINT('Ctrl Pts',(5.77219746187205,1.30220001510451,50.5001746300706));
#52926=CARTESIAN_POINT('Ctrl Pts',(5.9890176384768,0.341111965216764,50.4537834775966));
#52927=CARTESIAN_POINT('Ctrl Pts',(5.96059184747205,-0.675303246438216,
50.4073923251226));
#52928=CARTESIAN_POINT('Ctrl Pts',(5.69039563991286,-1.62277104960652,50.3610011726487));
#52929=CARTESIAN_POINT('Ctrl Pts',(5.42019943235367,-2.57023885277483,50.3146100201747));
#52930=CARTESIAN_POINT('Ctrl Pts',(4.90823280824003,-3.44875924745646,50.2682188677007));
#52931=CARTESIAN_POINT('Ctrl Pts',(4.2170926585536,-4.1509177211014,50.2218277152267));
#52932=CARTESIAN_POINT('Ctrl Pts',(3.52595250886718,-4.85307619474633,50.1754365627528));
#52933=CARTESIAN_POINT('Ctrl Pts',(2.65563883360783,-5.37887274735463,50.1290454102787));
#52934=CARTESIAN_POINT('Ctrl Pts',(1.71256273007023,-5.66401953684437,50.0826542578048));
#52935=CARTESIAN_POINT('Ctrl Pts',(0.769486626532637,-5.94916632633411,
50.0362631053308));
#52936=CARTESIAN_POINT('Ctrl Pts',(-0.246351905283146,-5.99366335270539,
49.9898719528568));
#52937=CARTESIAN_POINT('Ctrl Pts',(-1.21074880433904,-5.79207007476359,
49.9434808003828));
#52938=CARTESIAN_POINT('Ctrl Pts',(-2.17514570339494,-5.59047679682179,
49.8970896479088));
#52939=CARTESIAN_POINT('Ctrl Pts',(-3.08810096969077,-5.14279321456688,
49.8506984954348));
#52940=CARTESIAN_POINT('Ctrl Pts',(-3.83798982421993,-4.50375649068248,
49.8043073429609));
#52941=CARTESIAN_POINT('Ctrl Pts',(-4.58787867874904,-3.86471976679812,
49.7579161904869));
#52942=CARTESIAN_POINT('Ctrl Pts',(-5.17470112151149,-3.03432990128429,
49.7115250380129));
#52943=CARTESIAN_POINT('Ctrl Pts',(-5.52670782599837,-2.11411660610968,
49.6651338855389));
#52944=CARTESIAN_POINT('Ctrl Pts',(-5.78408263694966,-1.4412892995228,49.6312143210943));
#52945=CARTESIAN_POINT('Ctrl Pts',(-5.91592459112672,-0.720442248546615,
49.5972947566496));
#52946=CARTESIAN_POINT('Ctrl Pts',(-5.91663288208029,0.000152735557782668,
49.5633751922049));
#52947=CARTESIAN_POINT('Ctrl Pts',(-5.91649558673351,0.000137928394543142,
49.3116248077952));
#52948=CARTESIAN_POINT('Ctrl Pts',(-5.91592003609756,-0.672304945823302,
49.3432756667945));
#52949=CARTESIAN_POINT('Ctrl Pts',(-5.80146273753077,-1.34493875994679,
49.3749265257938));
#52950=CARTESIAN_POINT('Ctrl Pts',(-5.57671451190474,-1.9784447849391,49.406577384793));
#52951=CARTESIAN_POINT('Ctrl Pts',(-5.24729756927107,-2.90698434208879,
49.452968537267));
#52952=CARTESIAN_POINT('Ctrl Pts',(-4.68094023165125,-3.75146481968527,
49.499359689741));
#52953=CARTESIAN_POINT('Ctrl Pts',(-3.94688960784076,-4.40863368152314,
49.545750842215));
#52954=CARTESIAN_POINT('Ctrl Pts',(-3.21283898403027,-5.065802543361,49.592141994689));
#52955=CARTESIAN_POINT('Ctrl Pts',(-2.3110950740291,-5.53565978944027,49.638533147163));
#52956=CARTESIAN_POINT('Ctrl Pts',(-1.35191187208043,-5.76075713812599,
49.684924299637));
#52957=CARTESIAN_POINT('Ctrl Pts',(-0.392728670131761,-5.98585448681172,
49.7313154521109));
#52958=CARTESIAN_POINT('Ctrl Pts',(0.623893823764432,-5.96619193810391,
49.7777066045849));
#52959=CARTESIAN_POINT('Ctrl Pts',(1.57365569546802,-5.70417358312865,49.8240977570589));
#52960=CARTESIAN_POINT('Ctrl Pts',(2.5234175671716,-5.44215522815339,49.8704889095328));
#52961=CARTESIAN_POINT('Ctrl Pts',(3.40631881668261,-4.93778106691066,49.9168800620069));
#52962=CARTESIAN_POINT('Ctrl Pts',(4.11440929518245,-4.25271967875358,49.9632712144809));
#52963=CARTESIAN_POINT('Ctrl Pts',(4.82249977368232,-3.56765829059645,50.0096623669548));
#52964=CARTESIAN_POINT('Ctrl Pts',(5.35577948117102,-2.7019096755249,50.0560535194288));
#52965=CARTESIAN_POINT('Ctrl Pts',(5.6490456287554,-1.76132677223197,50.1024446719028));
#52966=CARTESIAN_POINT('Ctrl Pts',(5.94231177633977,-0.820743868939092,
50.1488358243768));
#52967=CARTESIAN_POINT('Ctrl Pts',(5.99556436401987,0.194673322575037,50.1952269768508));
#52968=CARTESIAN_POINT('Ctrl Pts',(5.8022923298075,1.1607722575073,50.2416181293248));
#52969=CARTESIAN_POINT('Ctrl Pts',(5.60902029559514,2.12687119243956,50.2880092817987));
#52970=CARTESIAN_POINT('Ctrl Pts',(5.16922363949027,3.04365187078983,50.3344004342727));
#52971=CARTESIAN_POINT('Ctrl Pts',(4.5366752092522,3.79902178989515,50.3807915867467));
#52972=CARTESIAN_POINT('Ctrl Pts',(3.90412677901412,4.55439170900048,50.4271827392207));
#52973=CARTESIAN_POINT('Ctrl Pts',(3.07882657464281,5.14835086886089,50.4735738916947));
#52974=CARTESIAN_POINT('Ctrl Pts',(2.16168200784626,5.50827735424564,50.5199650441686));
#52975=CARTESIAN_POINT('Ctrl Pts',(1.24453744104967,5.86820383963041,50.5663561966426));
#52976=CARTESIAN_POINT('Ctrl Pts',(0.235548511827793,5.99409765053951,50.6127473491166));
#52977=CARTESIAN_POINT('Ctrl Pts',(-0.741918202723497,5.87056606255386,
50.6591385015906));
#52978=CARTESIAN_POINT('Ctrl Pts',(-1.71938491727473,5.74703447456822,50.7055296540646));
#52979=CARTESIAN_POINT('Ctrl Pts',(-2.66532941715542,5.37407748768786,50.7519208065386));
#52980=CARTESIAN_POINT('Ctrl Pts',(-3.46409341148329,4.7972956288788,50.7983119590126));
#52981=CARTESIAN_POINT('Ctrl Pts',(-4.26285740581116,4.22051377006975,50.8447031114865));
#52982=CARTESIAN_POINT('Ctrl Pts',(-4.91444089458624,3.43990703933199,50.8910942639605));
#52983=CARTESIAN_POINT('Ctrl Pts',(-5.33917637861769,2.55091828805872,50.9374854164345));
#52984=CARTESIAN_POINT('Ctrl Pts',(-5.71803025962081,1.75796160972512,50.9788652135547));
#52985=CARTESIAN_POINT('Ctrl Pts',(-5.91639904055335,0.878773889402353,
51.0202450106749));
#52986=CARTESIAN_POINT('Ctrl Pts',(-5.91711198123886,-0.000102791298586485,
51.0616248077951));
#52987=CARTESIAN_POINT('Origin',(0.,0.,0.));
#52988=CARTESIAN_POINT('',(-5.91629566222658,7.35963193231049E-5,53.0633751922049));
#52989=CARTESIAN_POINT('',(-5.91624940617419,3.10831558172524E-5,52.8116248077951));
#52990=CARTESIAN_POINT('',(-5.91675,-7.2459289488551E-16,0.));
#52991=CARTESIAN_POINT('Ctrl Pts',(-5.91629566222658,7.35963193231049E-5,
53.0633751922049));
#52992=CARTESIAN_POINT('Ctrl Pts',(-5.91647516542744,0.411417234058072,
53.0440157493585));
#52993=CARTESIAN_POINT('Ctrl Pts',(-5.87419418252669,0.822724493908837,
53.0246563065121));
#52994=CARTESIAN_POINT('Ctrl Pts',(-5.78907949919593,1.22496815067562,53.0052968636658));
#52995=CARTESIAN_POINT('Ctrl Pts',(-5.58511865778604,2.18886711000249,52.9589057111918));
#52996=CARTESIAN_POINT('Ctrl Pts',(-5.13519457400149,3.100720292762,52.9125145587178));
#52997=CARTESIAN_POINT('Ctrl Pts',(-4.49431835109818,3.84903766897162,52.8661234062438));
#52998=CARTESIAN_POINT('Ctrl Pts',(-3.8534421281949,4.59735504518119,52.8197322537698));
#52999=CARTESIAN_POINT('Ctrl Pts',(-3.0216137661729,5.1821366148409,52.7733411012958));
#53000=CARTESIAN_POINT('Ctrl Pts',(-2.10053885840573,5.53188258394083,52.7269499488218));
#53001=CARTESIAN_POINT('Ctrl Pts',(-1.17946395063866,5.88162855304072,52.6805587963479));
#53002=CARTESIAN_POINT('Ctrl Pts',(-0.169142497126457,5.99633892158089,
52.6341676438739));
#53003=CARTESIAN_POINT('Ctrl Pts',(0.806896000590799,5.86198833693917,52.5877764913999));
#53004=CARTESIAN_POINT('Ctrl Pts',(1.78293449830828,5.72763775229742,52.5413853389259));
#53005=CARTESIAN_POINT('Ctrl Pts',(2.72469004023079,5.34422621447368,52.4949941864519));
#53006=CARTESIAN_POINT('Ctrl Pts',(3.51701650898951,4.75863250248173,52.4486030339779));
#53007=CARTESIAN_POINT('Ctrl Pts',(4.3093429777481,4.17303879048989,52.4022118815039));
#53008=CARTESIAN_POINT('Ctrl Pts',(4.95224037334295,3.38526290432992,52.35582072903));
#53009=CARTESIAN_POINT('Ctrl Pts',(5.36710322368081,2.49162425027036,52.309429576556));
#53010=CARTESIAN_POINT('Ctrl Pts',(5.78196607401873,1.5979855962107,52.2630384240821));
#53011=CARTESIAN_POINT('Ctrl Pts',(5.9687943790996,0.598484174251422,52.216647271608));
#53012=CARTESIAN_POINT('Ctrl Pts',(5.9047451048376,-0.384673452523944,52.170256119134));
#53013=CARTESIAN_POINT('Ctrl Pts',(5.84069583057561,-1.3678310792992,52.12386496666));
#53014=CARTESIAN_POINT('Ctrl Pts',(5.52576897697081,-2.33464491089054,52.0774738141861));
#53015=CARTESIAN_POINT('Ctrl Pts',(4.99846987033509,-3.16690501492114,52.0310826617121));
#53016=CARTESIAN_POINT('Ctrl Pts',(4.47117076369931,-3.99916511895182,51.9846915092381));
#53017=CARTESIAN_POINT('Ctrl Pts',(3.73149940403256,-4.69687149542172,51.9383003567641));
#53018=CARTESIAN_POINT('Ctrl Pts',(2.86989357630467,-5.17471731390861,51.8919092042902));
#53019=CARTESIAN_POINT('Ctrl Pts',(2.00828774857684,-5.65256313239547,51.8455180518162));
#53020=CARTESIAN_POINT('Ctrl Pts',(1.02474745278804,-5.91054839289931,51.7991268993422));
#53021=CARTESIAN_POINT('Ctrl Pts',(0.0395277246605722,-5.91712987665164,
51.7527357468682));
#53022=CARTESIAN_POINT('Ctrl Pts',(-0.945692003466838,-5.92371136040397,
51.7063445943942));
#53023=CARTESIAN_POINT('Ctrl Pts',(-1.93259116393294,-5.67888906740469,
51.6599534419202));
#53024=CARTESIAN_POINT('Ctrl Pts',(-2.80050404095068,-5.21259681299055,
51.6135622894462));
#53025=CARTESIAN_POINT('Ctrl Pts',(-3.66841691796848,-4.74630455857639,
51.5671711369723));
#53026=CARTESIAN_POINT('Ctrl Pts',(-4.41734351153807,-4.0585423427473,51.5207799844983));
#53027=CARTESIAN_POINT('Ctrl Pts',(-4.9557144221657,-3.2334011480358,51.4743888320243));
#53028=CARTESIAN_POINT('Ctrl Pts',(-5.4940853327933,-2.40825995332434,51.4279976795503));
#53029=CARTESIAN_POINT('Ctrl Pts',(-5.82190056047894,-1.44573977973047,
51.3816065270763));
#53030=CARTESIAN_POINT('Ctrl Pts',(-5.89907894933658,-0.463525584703147,
51.3352153746023));
#53031=CARTESIAN_POINT('Ctrl Pts',(-5.91119038294624,-0.309388886728128,
51.3279353138032));
#53032=CARTESIAN_POINT('Ctrl Pts',(-5.91712955113041,-0.154767197288363,
51.320655253004));
#53033=CARTESIAN_POINT('Ctrl Pts',(-5.91697841467406,-0.000133927646978338,
51.3133751922049));
#53034=CARTESIAN_POINT('Ctrl Pts',(-5.91711198123886,-0.000102791298586485,
51.0616248077951));
#53035=CARTESIAN_POINT('Ctrl Pts',(-5.91719832286859,-0.106540320374477,
51.0666361631489));
#53036=CARTESIAN_POINT('Ctrl Pts',(-5.91438569706757,-0.212973287512141,
51.0716475185027));
#53037=CARTESIAN_POINT('Ctrl Pts',(-5.9086436045588,-0.319247973600419,
51.0766588738565));
#53038=CARTESIAN_POINT('Ctrl Pts',(-5.85548786718063,-1.30305471217748,
51.1230500263304));
#53039=CARTESIAN_POINT('Ctrl Pts',(-5.55128891313645,-2.2732974175228,51.1694411788044));
#53040=CARTESIAN_POINT('Ctrl Pts',(-5.03324039503204,-3.11134691735899,
51.2158323312784));
#53041=CARTESIAN_POINT('Ctrl Pts',(-4.51519187692764,-3.94939641719518,
51.2622234837524));
#53042=CARTESIAN_POINT('Ctrl Pts',(-3.78329379476302,-4.65525271152223,
51.3086146362264));
#53043=CARTESIAN_POINT('Ctrl Pts',(-2.92703351412233,-5.14261249964901,
51.3550057887004));
#53044=CARTESIAN_POINT('Ctrl Pts',(-2.07077323348164,-5.62997228777579,
51.4013969411744));
#53045=CARTESIAN_POINT('Ctrl Pts',(-1.09015075436489,-5.89883556970231,
51.4477880936484));
#53046=CARTESIAN_POINT('Ctrl Pts',(-0.105064358277646,-5.91632909792562,
51.4941792461223));
#53047=CARTESIAN_POINT('Ctrl Pts',(0.880022037809597,-5.93382262614893,
51.5405703985963));
#53048=CARTESIAN_POINT('Ctrl Pts',(1.86957235086733,-5.69994640066903,51.5869615510703));
#53049=CARTESIAN_POINT('Ctrl Pts',(2.74259671524839,-5.24329588826058,51.6333527035443));
#53050=CARTESIAN_POINT('Ctrl Pts',(3.61562107962945,-4.78664537585214,51.6797438560182));
#53051=CARTESIAN_POINT('Ctrl Pts',(4.37211949533384,-4.10722057651513,51.7261350084922));
#53052=CARTESIAN_POINT('Ctrl Pts',(4.91959677493087,-3.28809307751947,51.7725261609662));
#53053=CARTESIAN_POINT('Ctrl Pts',(5.4670740545279,-2.46896557852381,51.8189173134402));
#53054=CARTESIAN_POINT('Ctrl Pts',(5.80553019801757,-1.51013537986949,51.8653084659142));
#53055=CARTESIAN_POINT('Ctrl Pts',(5.89358301109615,-0.528836274909741,
51.9116996183882));
#53056=CARTESIAN_POINT('Ctrl Pts',(5.98163582417474,0.452462830050005,51.9580907708622));
#53057=CARTESIAN_POINT('Ctrl Pts',(5.81928530684224,1.45623084131518,52.0044819233362));
#53058=CARTESIAN_POINT('Ctrl Pts',(5.42638165470832,2.35973953049624,52.0508730758101));
#53059=CARTESIAN_POINT('Ctrl Pts',(5.0334780025744,3.2632482196773,52.0972642282841));
#53060=CARTESIAN_POINT('Ctrl Pts',(4.41002121563907,4.06649758677425,52.1436553807581));
#53061=CARTESIAN_POINT('Ctrl Pts',(3.63223981092944,4.67127632133242,52.1900465332321));
#53062=CARTESIAN_POINT('Ctrl Pts',(2.85445840621981,5.27605505589058,52.2364376857061));
#53063=CARTESIAN_POINT('Ctrl Pts',(1.92235238373589,5.68236315790995,52.2828288381801));
#53064=CARTESIAN_POINT('Ctrl Pts',(0.949888038006726,5.84052234218767,52.3292199906541));
#53065=CARTESIAN_POINT('Ctrl Pts',(-0.0225763077224432,5.99868152646538,
52.375611143128));
#53066=CARTESIAN_POINT('Ctrl Pts',(-1.03539897669686,5.90869179300144,52.422002295602));
#53067=CARTESIAN_POINT('Ctrl Pts',(-1.9647446499574,5.5815559636006,52.468393448076));
#53068=CARTESIAN_POINT('Ctrl Pts',(-2.89409032321793,5.25442013419976,52.5147846005499));
#53069=CARTESIAN_POINT('Ctrl Pts',(-3.73995900076458,4.69013820886202,52.561175753024));
#53070=CARTESIAN_POINT('Ctrl Pts',(-4.39892841462264,3.95770354086397,52.6075669054979));
#53071=CARTESIAN_POINT('Ctrl Pts',(-5.0578978284807,3.22526887286591,52.6539580579719));
#53072=CARTESIAN_POINT('Ctrl Pts',(-5.52996797865016,2.32468146220754,52.7003492104459));
#53073=CARTESIAN_POINT('Ctrl Pts',(-5.75742001719438,1.36605390082203,52.7467403629199));
#53074=CARTESIAN_POINT('Ctrl Pts',(-5.86346106503545,0.919129477768853,
52.7683685112116));
#53075=CARTESIAN_POINT('Ctrl Pts',(-5.91633330006424,0.459589774967568,
52.7899966595034));
#53076=CARTESIAN_POINT('Ctrl Pts',(-5.91624940617419,3.10831558172524E-5,
52.8116248077951));
#53077=CARTESIAN_POINT('Origin',(0.,0.,0.));
#53078=CARTESIAN_POINT('',(-5.91726077539081,-8.91287485260684E-6,54.8133751922049));
#53079=CARTESIAN_POINT('',(-5.91723769598478,4.20217595612923E-5,54.5616248077952));
#53080=CARTESIAN_POINT('',(-5.91675,-7.2459289488551E-16,0.));
#53081=CARTESIAN_POINT('Ctrl Pts',(-5.91726077539081,-8.91287485260684E-6,
54.8133751922049));
#53082=CARTESIAN_POINT('Ctrl Pts',(-5.9171748721973,0.976903784862937,54.767376245713));
#53083=CARTESIAN_POINT('Ctrl Pts',(-5.67016608464484,1.95385832373982,54.7213772992211));
#53084=CARTESIAN_POINT('Ctrl Pts',(-5.20570418446295,2.81329564071131,54.6753783527292));
#53085=CARTESIAN_POINT('Ctrl Pts',(-4.73728209063319,3.68006087457345,54.6289872002552));
#53086=CARTESIAN_POINT('Ctrl Pts',(-4.04768288561822,4.42729634249545,54.5825960477812));
#53087=CARTESIAN_POINT('Ctrl Pts',(-3.22122215606804,4.96363941472753,54.5362048953072));
#53088=CARTESIAN_POINT('Ctrl Pts',(-2.39476142651782,5.49998248695964,54.4898137428333));
#53089=CARTESIAN_POINT('Ctrl Pts',(-1.43143917243238,5.82543316350179,54.4434225903593));
#53090=CARTESIAN_POINT('Ctrl Pts',(-0.449038419655624,5.9001993962792,54.3970314378853));
#53091=CARTESIAN_POINT('Ctrl Pts',(0.533362333121136,5.97496562905662,54.3506402854113));
#53092=CARTESIAN_POINT('Ctrl Pts',(1.53484158458918,5.79904741806929,54.3042491329373));
#53093=CARTESIAN_POINT('Ctrl Pts',(2.43295094735011,5.39395384722269,54.2578579804633));
#53094=CARTESIAN_POINT('Ctrl Pts',(3.33106031011092,4.98886027637614,54.2114668279893));
#53095=CARTESIAN_POINT('Ctrl Pts',(4.12579978416473,4.35459134567027,54.1650756755154));
#53096=CARTESIAN_POINT('Ctrl Pts',(4.71999854259989,3.56869754616937,54.1186845230414));
#53097=CARTESIAN_POINT('Ctrl Pts',(5.3141973010351,2.78280374666838,54.0722933705674));
#53098=CARTESIAN_POINT('Ctrl Pts',(5.7078553438517,1.84528507837241,54.0259022180934));
#53099=CARTESIAN_POINT('Ctrl Pts',(5.85284107725128,0.870769626606426,53.9795110656194));
#53100=CARTESIAN_POINT('Ctrl Pts',(5.99782681065085,-0.103745825159506,
53.9331199131455));
#53101=CARTESIAN_POINT('Ctrl Pts',(5.89414023463332,-1.11525806039542,53.8867287606715));
#53102=CARTESIAN_POINT('Ctrl Pts',(5.55445885001522,-2.04009198362915,53.8403376081975));
#53103=CARTESIAN_POINT('Ctrl Pts',(5.21477746539714,-2.96492590686283,53.7939464557235));
#53104=CARTESIAN_POINT('Ctrl Pts',(4.63910127217853,-3.80308151809446,53.7475553032495));
#53105=CARTESIAN_POINT('Ctrl Pts',(3.89781677254598,-4.45207960686234,53.7011641507755));
#53106=CARTESIAN_POINT('Ctrl Pts',(3.15653227291338,-5.10107769563026,53.6547729983015));
#53107=CARTESIAN_POINT('Ctrl Pts',(2.24963946686684,-5.56091826193439,53.6083818458276));
#53108=CARTESIAN_POINT('Ctrl Pts',(1.28802189141507,-5.77537773876444,53.5619906933536));
#53109=CARTESIAN_POINT('Ctrl Pts',(0.326404315963302,-5.9898372155945,53.5155995408796));
#53110=CARTESIAN_POINT('Ctrl Pts',(-0.689938028893665,-5.95891560295047,
53.4692083884056));
#53111=CARTESIAN_POINT('Ctrl Pts',(-1.63673948214485,-5.68639360981707,
53.4228172359316));
#53112=CARTESIAN_POINT('Ctrl Pts',(-2.5835409353961,-5.41387161668366,53.3764260834576));
#53113=CARTESIAN_POINT('Ctrl Pts',(-3.46080149704152,-4.89974924306087,
53.3300349309837));
#53114=CARTESIAN_POINT('Ctrl Pts',(-4.16126069119583,-4.20688695808299,
53.2836437785097));
#53115=CARTESIAN_POINT('Ctrl Pts',(-4.86171988535005,-3.51402467310519,
53.2372526260357));
#53116=CARTESIAN_POINT('Ctrl Pts',(-5.38537771201318,-2.64242247677237,
53.1908614735617));
#53117=CARTESIAN_POINT('Ctrl Pts',(-5.66820782582712,-1.69864901065889,
53.1444703210877));
#53118=CARTESIAN_POINT('Ctrl Pts',(-5.83301040353528,-1.14872065299335,
53.1174386114601));
#53119=CARTESIAN_POINT('Ctrl Pts',(-5.91604502079844,-0.574288065881491,
53.0904069018325));
#53120=CARTESIAN_POINT('Ctrl Pts',(-5.91629566222658,7.35963193231049E-5,
53.0633751922049));
#53121=CARTESIAN_POINT('Ctrl Pts',(-5.91624940617419,3.10831558172524E-5,
52.8116248077951));
#53122=CARTESIAN_POINT('Ctrl Pts',(-5.91615335242415,-0.526137576953405,
52.8363878119774));
#53123=CARTESIAN_POINT('Ctrl Pts',(-5.84663736162251,-1.05233112966596,
52.8611508161596));
#53124=CARTESIAN_POINT('Ctrl Pts',(-5.70802065118634,-1.55964379265648,
52.8859138203418));
#53125=CARTESIAN_POINT('Ctrl Pts',(-5.44833531971509,-2.51004621263684,
52.9323049728158));
#53126=CARTESIAN_POINT('Ctrl Pts',(-4.9461307298536,-3.39418334048491,52.9786961252898));
#53127=CARTESIAN_POINT('Ctrl Pts',(-4.26281019283623,-4.10395391959914,
53.0250872777638));
#53128=CARTESIAN_POINT('Ctrl Pts',(-3.57948965581886,-4.81372449871337,
53.0714784302378));
#53129=CARTESIAN_POINT('Ctrl Pts',(-2.7150531716456,-5.34912852909375,53.1178695827118));
#53130=CARTESIAN_POINT('Ctrl Pts',(-1.77519324801468,-5.64470348614918,
53.1642607351857));
#53131=CARTESIAN_POINT('Ctrl Pts',(-0.835333324383751,-5.94027844320462,
53.2106518876597));
#53132=CARTESIAN_POINT('Ctrl Pts',(0.179950038704843,-5.99602432693511,
53.2570430401337));
#53133=CARTESIAN_POINT('Ctrl Pts',(1.1465206593178,-5.80512522622028,53.3034341926077));
#53134=CARTESIAN_POINT('Ctrl Pts',(2.11309127993076,-5.61422612550546,53.3498253450817));
#53135=CARTESIAN_POINT('Ctrl Pts',(3.03094915806809,-5.17668204034532,53.3962164975557));
#53136=CARTESIAN_POINT('Ctrl Pts',(3.78787008451714,-4.54599040222939,53.4426076500296));
#53137=CARTESIAN_POINT('Ctrl Pts',(4.54479101096619,-3.91529876411345,53.4889988025036));
#53138=CARTESIAN_POINT('Ctrl Pts',(5.14077498572698,-3.09145957304172,53.5353899549776));
#53139=CARTESIAN_POINT('Ctrl Pts',(5.50295252446638,-2.17520160624497,53.5817811074516));
#53140=CARTESIAN_POINT('Ctrl Pts',(5.86513006320579,-1.25894363944822,53.6281722599256));
#53141=CARTESIAN_POINT('Ctrl Pts',(5.99350116592383,-0.250266896926448,
53.6745634123995));
#53142=CARTESIAN_POINT('Ctrl Pts',(5.87237021586824,0.727500214519055,53.7209545648735));
#53143=CARTESIAN_POINT('Ctrl Pts',(5.75123926581264,1.70526732596456,53.7673457173475));
#53144=CARTESIAN_POINT('Ctrl Pts',(5.38060626298342,2.65212480633379,53.8137368698215));
#53145=CARTESIAN_POINT('Ctrl Pts',(4.8057875865732,3.45230273688165,53.8601280222955));
#53146=CARTESIAN_POINT('Ctrl Pts',(4.23096891016299,4.25248066742951,53.9065191747695));
#53147=CARTESIAN_POINT('Ctrl Pts',(3.45196456017177,4.905979048156,53.9529103272435));
#53148=CARTESIAN_POINT('Ctrl Pts',(2.56402146886796,5.3328962507746,53.9993014797174));
#53149=CARTESIAN_POINT('Ctrl Pts',(1.67607837756421,5.75981345339318,54.0456926321914));
#53150=CARTESIAN_POINT('Ctrl Pts',(0.679196544947876,5.96014947790391,54.0920837846654));
#53151=CARTESIAN_POINT('Ctrl Pts',(-0.304737756597728,5.90940973482508,
54.1384749371394));
#53152=CARTESIAN_POINT('Ctrl Pts',(-1.28867205814344,5.85866999174624,54.1848660896134));
#53153=CARTESIAN_POINT('Ctrl Pts',(-2.25965882861843,5.5568544810778,54.2312572420874));
#53154=CARTESIAN_POINT('Ctrl Pts',(-3.09897792074494,5.04086543770779,54.2776483945614));
#53155=CARTESIAN_POINT('Ctrl Pts',(-3.93829701287136,4.52487639433785,54.3240395470353));
#53156=CARTESIAN_POINT('Ctrl Pts',(-4.64594842664933,3.7947138182664,54.3704306995093));
#53157=CARTESIAN_POINT('Ctrl Pts',(-5.135409376579,2.93965287904646,54.4168218519833));
#53158=CARTESIAN_POINT('Ctrl Pts',(-5.62487032650872,2.08459193982642,54.4632130044573));
#53159=CARTESIAN_POINT('Ctrl Pts',(-5.89614081259009,1.10463263745785,54.5096041569313));
#53160=CARTESIAN_POINT('Ctrl Pts',(-5.91605326443084,0.11959216846805,54.5559953094053));
#53161=CARTESIAN_POINT('Ctrl Pts',(-5.91685871338391,0.0797477625241243,
54.5578718088686));
#53162=CARTESIAN_POINT('Ctrl Pts',(-5.91725289962306,0.0398950429634057,
54.5597483083319));
#53163=CARTESIAN_POINT('Ctrl Pts',(-5.91723769598478,4.20217595612923E-5,
54.5616248077952));
#53164=CARTESIAN_POINT('Origin',(0.,0.,0.));
#53165=CARTESIAN_POINT('',(-5.91627540825074,-5.94123360231347E-5,56.5633751922049));
#53166=CARTESIAN_POINT('',(-5.9163456729308,-9.83204200377886E-5,56.3116248077952));
#53167=CARTESIAN_POINT('',(-5.91675,-7.2459289488551E-16,0.));
#53168=CARTESIAN_POINT('Ctrl Pts',(-5.91627540825074,-5.94123360231347E-5,
56.5633751922049));
#53169=CARTESIAN_POINT('Ctrl Pts',(-5.91607976903247,0.557640762099893,
56.5371278945414));
#53170=CARTESIAN_POINT('Ctrl Pts',(-5.83786039751333,1.11539468426929,56.510880596878));
#53171=CARTESIAN_POINT('Ctrl Pts',(-5.68235729093,1.65069804519026,56.4846332992146));
#53172=CARTESIAN_POINT('Ctrl Pts',(-5.40751115552233,2.59682743933861,56.4382421467406));
#53173=CARTESIAN_POINT('Ctrl Pts',(-4.89123613253373,3.47282287809166,56.3918509942667));
#53174=CARTESIAN_POINT('Ctrl Pts',(-4.19665589020436,4.17157856900639,56.3454598417927));
#53175=CARTESIAN_POINT('Ctrl Pts',(-3.50207564787502,4.87033425992108,56.2990686893187));
#53176=CARTESIAN_POINT('Ctrl Pts',(-2.62919018620492,5.39185020299748,56.2526775368446));
#53177=CARTESIAN_POINT('Ctrl Pts',(-1.68472504844259,5.67236193567815,56.2062863843706));
#53178=CARTESIAN_POINT('Ctrl Pts',(-0.740259910680251,5.95287366835883,
56.1598952318966));
#53179=CARTESIAN_POINT('Ctrl Pts',(0.275784903174342,5.99238119064378,56.1135040794227));
#53180=CARTESIAN_POINT('Ctrl Pts',(1.23918011048882,5.78605401564393,56.0671129269488));
#53181=CARTESIAN_POINT('Ctrl Pts',(2.20257531780331,5.57972684064408,56.0207217744748));
#53182=CARTESIAN_POINT('Ctrl Pts',(3.11332091857771,5.12756496835941,55.9743306220008));
#53183=CARTESIAN_POINT('Ctrl Pts',(3.86006230413533,4.48485311090271,55.9279394695268));
#53184=CARTESIAN_POINT('Ctrl Pts',(4.60680368969294,3.84214125344602,55.8815483170528));
#53185=CARTESIAN_POINT('Ctrl Pts',(5.18954086003379,3.00887941081727,55.8351571645788));
#53186=CARTESIAN_POINT('Ctrl Pts',(5.53702398478864,2.0869484445131,55.7887660121048));
#53187=CARTESIAN_POINT('Ctrl Pts',(5.88450710954352,1.16501747820888,55.7423748596309));
#53188=CARTESIAN_POINT('Ctrl Pts',(5.99673618871238,0.154417388229369,55.6959837071569));
#53189=CARTESIAN_POINT('Ctrl Pts',(5.85998925077836,-0.82128825569492,55.6495925546829));
#53190=CARTESIAN_POINT('Ctrl Pts',(5.72324231284433,-1.79699389961915,55.6032014022089));
#53191=CARTESIAN_POINT('Ctrl Pts',(5.3375193578074,-2.73780509748804,55.5568102497349));
#53192=CARTESIAN_POINT('Ctrl Pts',(4.74998177593861,-3.52869119454103,55.5104190972609));
#53193=CARTESIAN_POINT('Ctrl Pts',(4.16244419406982,-4.31957729159402,55.4640279447869));
#53194=CARTESIAN_POINT('Ctrl Pts',(3.37309198536915,-4.96053828783114,55.4176367923129));
#53195=CARTESIAN_POINT('Ctrl Pts',(2.47843728915764,-5.37320546991209,55.371245639839));
#53196=CARTESIAN_POINT('Ctrl Pts',(1.58378259294619,-5.78587265199302,55.324854487365));
#53197=CARTESIAN_POINT('Ctrl Pts',(0.583825409223878,-5.97024601991783,
55.278463334891));
#53198=CARTESIAN_POINT('Ctrl Pts',(-0.399171974063911,-5.90378269868584,
55.232072182417));
#53199=CARTESIAN_POINT('Ctrl Pts',(-1.38216935735181,-5.83731937745384,
55.185681029943));
#53200=CARTESIAN_POINT('Ctrl Pts',(-2.34820694020522,-5.52001936706497,
55.139289877469));
#53201=CARTESIAN_POINT('Ctrl Pts',(-3.17916970025765,-4.9906781538328,55.0928987249951));
#53202=CARTESIAN_POINT('Ctrl Pts',(-4.01013246031003,-4.46133694060066,
55.0465075725211));
#53203=CARTESIAN_POINT('Ctrl Pts',(-4.70602039756146,-3.71995452452523,
55.0001164200471));
#53204=CARTESIAN_POINT('Ctrl Pts',(-5.18174901764866,-2.85717789720512,
54.9537252675731));
#53205=CARTESIAN_POINT('Ctrl Pts',(-5.65747763773589,-1.99440126988496,
54.9073341150992));
#53206=CARTESIAN_POINT('Ctrl Pts',(-5.91304694065887,-1.01023043132008,
54.8609429626251));
#53207=CARTESIAN_POINT('Ctrl Pts',(-5.91720910079805,-0.0249975121364856,
54.8145518101512));
#53208=CARTESIAN_POINT('Ctrl Pts',(-5.91724428906172,-0.0166680306718219,
54.8141596041691));
#53209=CARTESIAN_POINT('Ctrl Pts',(-5.91726150783685,-0.00833847329425605,
54.813767398187));
#53210=CARTESIAN_POINT('Ctrl Pts',(-5.91726077539081,-8.91287485260684E-6,
54.8133751922049));
#53211=CARTESIAN_POINT('Ctrl Pts',(-5.91723769598478,4.20217595612923E-5,
54.5616248077952));
#53212=CARTESIAN_POINT('Ctrl Pts',(-5.91687703258142,-0.945358414009718,
54.6061394608058));
#53213=CARTESIAN_POINT('Ctrl Pts',(-5.68613561487586,-1.89092859694345,
54.6506541138165));
#53214=CARTESIAN_POINT('Ctrl Pts',(-5.25001479529728,-2.72971301852433,
54.6951687668272));
#53215=CARTESIAN_POINT('Ctrl Pts',(-4.79550945672283,-3.60385610091598,
54.7415599193012));
#53216=CARTESIAN_POINT('Ctrl Pts',(-4.11794436197377,-4.3620206300883,54.7879510717752));
#53217=CARTESIAN_POINT('Ctrl Pts',(-3.30016371684655,-4.91150770704385,
54.8343422242492));
#53218=CARTESIAN_POINT('Ctrl Pts',(-2.48238307171933,-5.46099478399941,
54.8807333767231));
#53219=CARTESIAN_POINT('Ctrl Pts',(-1.52438687621396,-5.80180440873821,
54.9271245291971));
#53220=CARTESIAN_POINT('Ctrl Pts',(-0.543306952184463,-5.8922666326338,
54.9735156816711));
#53221=CARTESIAN_POINT('Ctrl Pts',(0.437772971845032,-5.98272885652939,
55.0199068341451));
#53222=CARTESIAN_POINT('Ctrl Pts',(1.44193662439864,-5.82284367958176,55.0662979866191));
#53223=CARTESIAN_POINT('Ctrl Pts',(2.34640740300649,-5.43215986633843,55.1126891390931));
#53224=CARTESIAN_POINT('Ctrl Pts',(3.2508781816143,-5.04147605309511,55.1590802915671));
#53225=CARTESIAN_POINT('Ctrl Pts',(4.05565608627635,-4.41999360355611,55.205471444041));
#53226=CARTESIAN_POINT('Ctrl Pts',(4.66234291603613,-3.64369963740555,55.251862596515));
#53227=CARTESIAN_POINT('Ctrl Pts',(5.26902974579598,-2.8674056712549,55.298253748989));
#53228=CARTESIAN_POINT('Ctrl Pts',(5.6776255006535,-1.93630018849265,55.344644901463));
#53229=CARTESIAN_POINT('Ctrl Pts',(5.83817218975984,-0.964227150134441,
55.391036053937));
#53230=CARTESIAN_POINT('Ctrl Pts',(5.99871887886617,0.00784588822371104,
55.437427206411));
#53231=CARTESIAN_POINT('Ctrl Pts',(5.91121650222135,1.02088648217782,55.483818358885));
#53232=CARTESIAN_POINT('Ctrl Pts',(5.5863637586731,1.95103266762128,55.5302095113589));
#53233=CARTESIAN_POINT('Ctrl Pts',(5.26151101512484,2.88117885306474,55.5766006638329));
#53234=CARTESIAN_POINT('Ctrl Pts',(4.69930790467315,3.72843062999755,55.6229918163069));
#53235=CARTESIAN_POINT('Ctrl Pts',(3.96849360904772,4.38919662230903,55.6693829687809));
#53236=CARTESIAN_POINT('Ctrl Pts',(3.23767931342226,5.04996261462054,55.7157741212549));
#53237=CARTESIAN_POINT('Ctrl Pts',(2.3382538326232,5.52424282231063,55.7621652737288));
#53238=CARTESIAN_POINT('Ctrl Pts',(1.38018769229769,5.75404817918408,55.8085564262028));
#53239=CARTESIAN_POINT('Ctrl Pts',(0.422121551972288,5.9838535360575,55.8549475786768));
#53240=CARTESIAN_POINT('Ctrl Pts',(-0.594585247879595,5.96918404211424,
55.9013387311508));
#53241=CARTESIAN_POINT('Ctrl Pts',(-1.54562248523716,5.7118333000422,55.9477298836248));
#53242=CARTESIAN_POINT('Ctrl Pts',(-2.49665972259472,5.45448255797015,55.9941210360988));
#53243=CARTESIAN_POINT('Ctrl Pts',(-3.38202739745815,4.95445056776933,56.0405121885727));
#53244=CARTESIAN_POINT('Ctrl Pts',(-4.09347379729039,4.27287500229513,56.0869033410467));
#53245=CARTESIAN_POINT('Ctrl Pts',(-4.80492019712272,3.59129943682085,56.1332944935207));
#53246=CARTESIAN_POINT('Ctrl Pts',(-5.34244532192383,2.72818029607314,56.1796856459947));
#53247=CARTESIAN_POINT('Ctrl Pts',(-5.64032730614178,1.78904901943268,56.2260767984687));
#53248=CARTESIAN_POINT('Ctrl Pts',(-5.823431263147,1.21177794561567,56.2545928015775));
#53249=CARTESIAN_POINT('Ctrl Pts',(-5.91598865378374,0.605786509134923,
56.2831088046863));
#53250=CARTESIAN_POINT('Ctrl Pts',(-5.9163456729308,-9.83204200377886E-5,
56.3116248077952));
#53251=CARTESIAN_POINT('Origin',(0.,0.,0.));
#53252=CARTESIAN_POINT('',(-5.91702729634208,0.000124615492362937,58.3133751922049));
#53253=CARTESIAN_POINT('',(-5.91688099001312,0.000147016541328388,58.0616248077952));
#53254=CARTESIAN_POINT('',(-5.91675,-7.2459289488551E-16,0.));
#53255=CARTESIAN_POINT('Ctrl Pts',(-5.91702729634208,0.000124615492362937,
58.3133751922049));
#53256=CARTESIAN_POINT('Ctrl Pts',(-5.91715596758306,0.138093166993387,
58.3068795433699));
#53257=CARTESIAN_POINT('Ctrl Pts',(-5.91242878598758,0.27605291677057,58.3003838945349));
#53258=CARTESIAN_POINT('Ctrl Pts',(-5.90278469289257,0.413668088609088,
58.2938882457));
#53259=CARTESIAN_POINT('Ctrl Pts',(-5.83390772546236,1.39649930096326,58.247497093226));
#53260=CARTESIAN_POINT('Ctrl Pts',(-5.51423647159942,2.36175480989941,58.201105940752));
#53261=CARTESIAN_POINT('Ctrl Pts',(-4.98285634368328,3.19141521529174,58.154714788278));
#53262=CARTESIAN_POINT('Ctrl Pts',(-4.45147621576713,4.02107562068407,58.108323635804));
#53263=CARTESIAN_POINT('Ctrl Pts',(-3.70838721379777,4.71514092253258,58.0619324833301));
#53264=CARTESIAN_POINT('Ctrl Pts',(-2.84444498940382,5.18874947559003,58.0155413308561));
#53265=CARTESIAN_POINT('Ctrl Pts',(-1.98050276500986,5.66235802864748,57.9691501783821));
#53266=CARTESIAN_POINT('Ctrl Pts',(-0.995707318191299,5.91550983291386,
57.9227590259081));
#53267=CARTESIAN_POINT('Ctrl Pts',(-0.0104671488781131,5.91725264434219,
57.8763678734341));
#53268=CARTESIAN_POINT('Ctrl Pts',(0.974773020435017,5.91899545577053,57.8299767209601));
#53269=CARTESIAN_POINT('Ctrl Pts',(1.96045791224277,5.66932927436084,57.7835855684861));
#53270=CARTESIAN_POINT('Ctrl Pts',(2.82607027637954,5.19878016568737,57.7371944160122));
#53271=CARTESIAN_POINT('Ctrl Pts',(3.6916826405164,4.72823105701384,57.6908032635382));
#53272=CARTESIAN_POINT('Ctrl Pts',(4.43722247698224,4.03679902107647,57.6444121110642));
#53273=CARTESIAN_POINT('Ctrl Pts',(4.97153447668531,3.2090237402222,57.5980209585902));
#53274=CARTESIAN_POINT('Ctrl Pts',(5.50584647638837,2.38124845936792,57.5516298061162));
#53275=CARTESIAN_POINT('Ctrl Pts',(5.82893063932866,1.41712993359675,57.5052386536423));
#53276=CARTESIAN_POINT('Ctrl Pts',(5.90128426518759,0.434548546919226,57.4588475011683));
#53277=CARTESIAN_POINT('Ctrl Pts',(5.97363789104652,-0.548032839758186,
57.4124563486943));
#53278=CARTESIAN_POINT('Ctrl Pts',(5.79526097982415,-1.54907708734194,57.3660651962203));
#53279=CARTESIAN_POINT('Ctrl Pts',(5.38796323461345,-2.44618899528104,57.3196740437463));
#53280=CARTESIAN_POINT('Ctrl Pts',(4.98066548940273,-3.34330090322018,57.2732828912723));
#53281=CARTESIAN_POINT('Ctrl Pts',(4.34444691020367,-4.13648047151466,57.2268917387983));
#53282=CARTESIAN_POINT('Ctrl Pts',(3.55709636677232,-4.72874759906632,57.1805005863244));
#53283=CARTESIAN_POINT('Ctrl Pts',(2.76974582334101,-5.32101472661796,57.1341094338504));
#53284=CARTESIAN_POINT('Ctrl Pts',(1.83126331567744,-5.71236941342681,57.0877182813764));
#53285=CARTESIAN_POINT('Ctrl Pts',(0.856394775358902,-5.85496169132799,
57.0413271289024));
#53286=CARTESIAN_POINT('Ctrl Pts',(-0.118473764959746,-5.99755396922917,
56.9949359764284));
#53287=CARTESIAN_POINT('Ctrl Pts',(-1.12972833793337,-5.89138383822262,
56.9485448239544));
#53288=CARTESIAN_POINT('Ctrl Pts',(-2.05372535181664,-5.54943245724155,
56.9021536714805));
#53289=CARTESIAN_POINT('Ctrl Pts',(-2.97772236569985,-5.2074810762605,56.8557625190065));
#53290=CARTESIAN_POINT('Ctrl Pts',(-3.81446182049285,-4.62974844530485,
56.8093713665324));
#53291=CARTESIAN_POINT('Ctrl Pts',(-4.46163765567354,-3.88687250210966,
56.7629802140585));
#53292=CARTESIAN_POINT('Ctrl Pts',(-5.10881349085423,-3.14399655891447,
56.7165890615845));
#53293=CARTESIAN_POINT('Ctrl Pts',(-5.56642570642268,-2.23597730347984,
56.6701979091106));
#53294=CARTESIAN_POINT('Ctrl Pts',(-5.77852319029356,-1.27383600099065,
56.6238067566366));
#53295=CARTESIAN_POINT('Ctrl Pts',(-5.87061965034974,-0.856057315379074,
56.603662901826));
#53296=CARTESIAN_POINT('Ctrl Pts',(-5.91642555429848,-0.428074192589743,
56.5835190470154));
#53297=CARTESIAN_POINT('Ctrl Pts',(-5.91627540825074,-5.94123360231347E-5,
56.5633751922049));
#53298=CARTESIAN_POINT('Ctrl Pts',(-5.9163456729308,-9.83204200377886E-5,
56.3116248077952));
#53299=CARTESIAN_POINT('Ctrl Pts',(-5.91656946904121,-0.379894948476797,
56.3294999571603));
#53300=CARTESIAN_POINT('Ctrl Pts',(-5.88056440059847,-0.759649686812157,
56.3473751065255));
#53301=CARTESIAN_POINT('Ctrl Pts',(-5.80792311789336,-1.1322621476414,56.3652502558907));
#53302=CARTESIAN_POINT('Ctrl Pts',(-5.61939810179222,-2.09929862554175,
56.4116414083646));
#53303=CARTESIAN_POINT('Ctrl Pts',(-5.18410922595517,-3.0182281688093,56.4580325608386));
#53304=CARTESIAN_POINT('Ctrl Pts',(-4.55527818301399,-3.77669553839045,
56.5044237133126));
#53305=CARTESIAN_POINT('Ctrl Pts',(-3.92644714007281,-4.53516290797161,
56.5508148657866));
#53306=CARTESIAN_POINT('Ctrl Pts',(-3.10407393002749,-5.13316810386637,
56.5972060182606));
#53307=CARTESIAN_POINT('Ctrl Pts',(-2.18870808823997,-5.4975945120402,56.6435971707346));
#53308=CARTESIAN_POINT('Ctrl Pts',(-1.2733422464525,-5.862020920214,56.6899883232086));
#53309=CARTESIAN_POINT('Ctrl Pts',(-0.264983772922841,-5.9928685406669,
56.7363794756825));
#53310=CARTESIAN_POINT('Ctrl Pts',(0.713077839509047,-5.87413895895754,
56.7827706281565));
#53311=CARTESIAN_POINT('Ctrl Pts',(1.69113945194105,-5.75540937724817,56.8291617806305));
#53312=CARTESIAN_POINT('Ctrl Pts',(2.63890420327526,-5.38710259337649,56.8755529331045));
#53313=CARTESIAN_POINT('Ctrl Pts',(3.44049124499301,-4.81425056550529,56.9219440855785));
#53314=CARTESIAN_POINT('Ctrl Pts',(4.24207828671072,-4.24139853763412,56.9683352380525));
#53315=CARTESIAN_POINT('Ctrl Pts',(4.89748761881198,-3.46400126576346,57.0147263905264));
#53316=CARTESIAN_POINT('Ctrl Pts',(5.32658396571914,-2.57710918870065,57.0611175430004));
#53317=CARTESIAN_POINT('Ctrl Pts',(5.75568031262631,-1.69021711163785,57.1075086954744));
#53318=CARTESIAN_POINT('Ctrl Pts',(5.95846367433938,-0.693830229382904,
57.1538998479484));
#53319=CARTESIAN_POINT('Ctrl Pts',(5.91014023151901,0.290225702035549,57.2002910004224));
#53320=CARTESIAN_POINT('Ctrl Pts',(5.86181678869864,1.274281633454,57.2466821528964));
#53321=CARTESIAN_POINT('Ctrl Pts',(5.56238654134484,2.24600661403597,57.2930733053703));
#53322=CARTESIAN_POINT('Ctrl Pts',(5.0484600841085,3.08659023738248,57.3394644578443));
#53323=CARTESIAN_POINT('Ctrl Pts',(4.53453362687216,3.927173860729,57.3858556103183));
#53324=CARTESIAN_POINT('Ctrl Pts',(3.80611095975329,4.63661612684007,57.4322467627923));
#53325=CARTESIAN_POINT('Ctrl Pts',(2.95225451794705,5.12817528713702,57.4786379152663));
#53326=CARTESIAN_POINT('Ctrl Pts',(2.09839807614086,5.61973444743394,57.5250290677402));
#53327=CARTESIAN_POINT('Ctrl Pts',(1.11910785964732,5.89341050191678,57.5714202202142));
#53328=CARTESIAN_POINT('Ctrl Pts',(0.134119257521085,5.91574175730344,57.6178113726882));
#53329=CARTESIAN_POINT('Ctrl Pts',(-0.850869344605262,5.93807301269011,
57.6642025251622));
#53330=CARTESIAN_POINT('Ctrl Pts',(-1.84155633236431,5.70905946898055,57.7105936776362));
#53331=CARTESIAN_POINT('Ctrl Pts',(-2.71681286170871,5.25670204489428,57.7569848301102));
#53332=CARTESIAN_POINT('Ctrl Pts',(-3.5920693910531,4.80434462080802,57.8033759825841));
#53333=CARTESIAN_POINT('Ctrl Pts',(-4.35189546198286,4.12864331634505,57.8497671350581));
#53334=CARTESIAN_POINT('Ctrl Pts',(-4.90338902290551,3.31221445628018,57.8961582875321));
#53335=CARTESIAN_POINT('Ctrl Pts',(-5.4548825838281,2.49578559621541,57.9425494400061));
#53336=CARTESIAN_POINT('Ctrl Pts',(-5.79804363474364,1.53862918054877,57.9889405924801));
#53337=CARTESIAN_POINT('Ctrl Pts',(-5.89091472397156,0.557774353333574,
58.0353317449541));
#53338=CARTESIAN_POINT('Ctrl Pts',(-5.90846020592207,0.372468346802949,
58.0440960992345));
#53339=CARTESIAN_POINT('Ctrl Pts',(-5.91707236649847,0.186316499212652,
58.0528604535148));
#53340=CARTESIAN_POINT('Ctrl Pts',(-5.91688099001312,0.000147016541328388,
58.0616248077952));
#53341=CARTESIAN_POINT('Origin',(0.,0.,0.));
#53342=CARTESIAN_POINT('',(-5.91658334351688,-0.000149097059289338,60.0633751922048));
#53343=CARTESIAN_POINT('',(-5.91673072200561,-0.000155070081382937,59.8116248077951));
#53344=CARTESIAN_POINT('',(-5.91675,-7.2459289488551E-16,0.));
#53345=CARTESIAN_POINT('Ctrl Pts',(-5.91658334351688,-0.000149097059289338,
60.0633751922048));
#53346=CARTESIAN_POINT('Ctrl Pts',(-5.91591710183977,0.703798585125833,
60.0302400397244));
#53347=CARTESIAN_POINT('Ctrl Pts',(-5.79023326449385,1.40797780184198,59.9971048872439));
#53348=CARTESIAN_POINT('Ctrl Pts',(-5.54437260154774,2.06734633609866,59.9639697347634));
#53349=CARTESIAN_POINT('Ctrl Pts',(-5.20015328616037,2.99050086895518,59.9175785822894));
#53350=CARTESIAN_POINT('Ctrl Pts',(-4.62036770117985,3.82581912179531,59.8711874298154));
#53351=CARTESIAN_POINT('Ctrl Pts',(-3.87590479394297,4.47116880093722,59.8247962773414));
#53352=CARTESIAN_POINT('Ctrl Pts',(-3.13144188670613,5.11651848007909,59.7784051248674));
#53353=CARTESIAN_POINT('Ctrl Pts',(-2.22230165721294,5.57189958552276,59.7320139723935));
#53354=CARTESIAN_POINT('Ctrl Pts',(-1.25964242937086,5.78163379749245,59.6856228199195));
#53355=CARTESIAN_POINT('Ctrl Pts',(-0.29698320152883,5.99136800946213,59.6392316674455));
#53356=CARTESIAN_POINT('Ctrl Pts',(0.719195024662093,5.95545532795785,59.5928405149715));
#53357=CARTESIAN_POINT('Ctrl Pts',(1.66464665457408,5.67828670759027,59.5464493624975));
#53358=CARTESIAN_POINT('Ctrl Pts',(2.61009828448608,5.40111808722269,59.5000582100235));
#53359=CARTESIAN_POINT('Ctrl Pts',(3.48482331811929,4.88269352799172,59.4536670575496));
#53360=CARTESIAN_POINT('Ctrl Pts',(4.18187129231742,4.1863995166099,59.4072759050756));
#53361=CARTESIAN_POINT('Ctrl Pts',(4.87891926651564,3.490105505228,59.3608847526016));
#53362=CARTESIAN_POINT('Ctrl Pts',(5.39829018127884,2.61594204169528,59.3144936001276));
#53363=CARTESIAN_POINT('Ctrl Pts',(5.67648184134843,1.67079092738194,59.2681024476536));
#53364=CARTESIAN_POINT('Ctrl Pts',(5.954673501418,0.725639813068655,59.2217112951796));
#53365=CARTESIAN_POINT('Ctrl Pts',(5.99168590679389,-0.2904989520251,59.1753201427057));
#53366=CARTESIAN_POINT('Ctrl Pts',(5.78299364235101,-1.25338459808161,59.1289289902317));
#53367=CARTESIAN_POINT('Ctrl Pts',(5.57430137790812,-2.21627024413813,59.0825378377577));
#53368=CARTESIAN_POINT('Ctrl Pts',(5.11990444364646,-3.12590277115739,59.0361466852837));
#53369=CARTESIAN_POINT('Ctrl Pts',(4.47536082717046,-3.87106366323371,58.9897555328097));
#53370=CARTESIAN_POINT('Ctrl Pts',(3.83081721069445,-4.61622455531003,58.9433643803357));
#53371=CARTESIAN_POINT('Ctrl Pts',(2.99612691200424,-5.19691381244332,58.8969732278618));
#53372=CARTESIAN_POINT('Ctrl Pts',(2.07334544638051,-5.54213199753971,58.8505820753878));
#53373=CARTESIAN_POINT('Ctrl Pts',(1.15056398075677,-5.88735018263611,58.8041909229138));
#53374=CARTESIAN_POINT('Ctrl Pts',(0.13969134819945,-5.99709729569552,58.7577997704398));
#53375=CARTESIAN_POINT('Ctrl Pts',(-0.835675558454431,-5.85795482904931,
58.7114086179658));
#53376=CARTESIAN_POINT('Ctrl Pts',(-1.81104246510831,-5.71881236240311,
58.6650174654918));
#53377=CARTESIAN_POINT('Ctrl Pts',(-2.75090364585892,-5.33078031605133,
58.6186263130179));
#53378=CARTESIAN_POINT('Ctrl Pts',(-3.5403446021856,-4.74130240714043,58.5722351605439));
#53379=CARTESIAN_POINT('Ctrl Pts',(-4.32978555851227,-4.15182449822952,
58.5258440080699));
#53380=CARTESIAN_POINT('Ctrl Pts',(-4.96880629041501,-3.36090072675949,
58.4794528555959));
#53381=CARTESIAN_POINT('Ctrl Pts',(-5.37927531586764,-2.46523538313838,
58.4330617031219));
#53382=CARTESIAN_POINT('Ctrl Pts',(-5.73227082525564,-1.6949803222015,58.3931661994829));
#53383=CARTESIAN_POINT('Ctrl Pts',(-5.91623701286255,-0.847261840938569,
58.3532706958439));
#53384=CARTESIAN_POINT('Ctrl Pts',(-5.91702729634208,0.000124615492362937,
58.3133751922049));
#53385=CARTESIAN_POINT('Ctrl Pts',(-5.91688099001312,0.000147016541328388,
58.0616248077952));
#53386=CARTESIAN_POINT('Ctrl Pts',(-5.91605937963967,-0.799108847634678,
58.0992516059888));
#53387=CARTESIAN_POINT('Ctrl Pts',(-5.75297761825815,-1.59868974831479,
58.1368784041824));
#53388=CARTESIAN_POINT('Ctrl Pts',(-5.43790532219926,-2.33306112674712,
58.174505202376));
#53389=CARTESIAN_POINT('Ctrl Pts',(-5.04944370365874,-3.23848854084873,
58.22089635485));
#53390=CARTESIAN_POINT('Ctrl Pts',(-4.42993933903741,-4.04479013028813,
58.267287507324));
#53391=CARTESIAN_POINT('Ctrl Pts',(-3.65513749247627,-4.65338139694523,
58.313678659798));
#53392=CARTESIAN_POINT('Ctrl Pts',(-2.88033564591512,-5.26197266360233,
58.360069812272));
#53393=CARTESIAN_POINT('Ctrl Pts',(-1.95023631741417,-5.67285360747713,
58.4064609647459));
#53394=CARTESIAN_POINT('Ctrl Pts',(-0.978560447999752,-5.83578683332009,
58.4528521172199));
#53395=CARTESIAN_POINT('Ctrl Pts',(-0.00688457858533637,-5.99872005916305,
58.4992432696939));
#53396=CARTESIAN_POINT('Ctrl Pts',(1.00636783174254,-5.91370556697417,58.5456344221679));
#53397=CARTESIAN_POINT('Ctrl Pts',(1.93730892061392,-5.59113786813126,58.5920255746419));
#53398=CARTESIAN_POINT('Ctrl Pts',(2.86825000948531,-5.26857016928834,58.6384167271159));
#53399=CARTESIAN_POINT('Ctrl Pts',(3.7168797769002,-4.7084492637914,58.6848078795899));
#53400=CARTESIAN_POINT('Ctrl Pts',(4.37943836326497,-3.97925974732797,58.7311990320639));
#53401=CARTESIAN_POINT('Ctrl Pts',(5.04199694962974,-3.25007023086454,58.7775901845378));
#53402=CARTESIAN_POINT('Ctrl Pts',(5.51848435494438,-2.35181210343462,58.8239813370118));
#53403=CARTESIAN_POINT('Ctrl Pts',(5.75064164442725,-1.39431316128073,58.8703724894858));
#53404=CARTESIAN_POINT('Ctrl Pts',(5.98279893391012,-0.436814219126841,
58.9167636419597));
#53405=CARTESIAN_POINT('Ctrl Pts',(5.97062610756122,0.579925537751025,58.9631547944338));
#53406=CARTESIAN_POINT('Ctrl Pts',(5.71561150670597,1.53159185775846,59.0095459469077));
#53407=CARTESIAN_POINT('Ctrl Pts',(5.46059690585071,2.48325817776589,59.0559370993817));
#53408=CARTESIAN_POINT('Ctrl Pts',(4.96274053048909,3.36985106090288,59.1023282518557));
#53409=CARTESIAN_POINT('Ctrl Pts',(4.28291404643916,4.08296899145165,59.1487194043297));
#53410=CARTESIAN_POINT('Ctrl Pts',(3.60308756238927,4.79608692200038,59.1951105568037));
#53411=CARTESIAN_POINT('Ctrl Pts',(2.74129096965108,5.33572989996091,59.2415017092776));
#53412=CARTESIAN_POINT('Ctrl Pts',(1.80289400293608,5.63591711512144,59.2878928617516));
#53413=CARTESIAN_POINT('Ctrl Pts',(0.864497036220978,5.93610433028201,59.3342840142256));
#53414=CARTESIAN_POINT('Ctrl Pts',(-0.150500304470951,5.99683578264253,
59.3806751666996));
#53415=CARTESIAN_POINT('Ctrl Pts',(-1.11799680845635,5.81068598795556,59.4270663191736));
#53416=CARTESIAN_POINT('Ctrl Pts',(-2.08549331244169,5.6245361932686,59.4734574716476));
#53417=CARTESIAN_POINT('Ctrl Pts',(-3.0054889797205,5.19150515153418,59.5198486241216));
#53418=CARTESIAN_POINT('Ctrl Pts',(-3.76549821889715,4.56453849560105,59.5662397765955));
#53419=CARTESIAN_POINT('Ctrl Pts',(-4.52550745807381,3.93757183966792,59.6126309290695));
#53420=CARTESIAN_POINT('Ctrl Pts',(-5.1255302691483,3.11666956953608,59.6590220815435));
#53421=CARTESIAN_POINT('Ctrl Pts',(-5.49220334927571,2.20220137238773,59.7054132340175));
#53422=CARTESIAN_POINT('Ctrl Pts',(-5.77203346648078,1.50431609894628,59.7408170919434));
#53423=CARTESIAN_POINT('Ctrl Pts',(-5.91595773098113,0.751936838973634,
59.7762209498693));
#53424=CARTESIAN_POINT('Ctrl Pts',(-5.91673072200561,-0.000155070081382937,
59.8116248077951));
#53425=CARTESIAN_POINT('Origin',(0.,0.,0.));
#53426=CARTESIAN_POINT('',(-5.91657547456529,0.000148352692112552,61.8133751922048));
#53427=CARTESIAN_POINT('',(-5.91644646386006,0.000128480793576948,61.5616248077951));
#53428=CARTESIAN_POINT('',(-5.91675,-7.2459289488551E-16,0.));
#53429=CARTESIAN_POINT('Ctrl Pts',(-5.91657547456529,0.000148352692112552,
61.8133751922048));
#53430=CARTESIAN_POINT('Ctrl Pts',(-5.9168426692125,0.284478488460568,61.7999916885528));
#53431=CARTESIAN_POINT('Ctrl Pts',(-5.89671750618213,0.568771121108608,
61.7866081849008));
#53432=CARTESIAN_POINT('Ctrl Pts',(-5.85588508619642,0.850057825547872,
61.7732246812488));
#53433=CARTESIAN_POINT('Ctrl Pts',(-5.71434793189889,1.82508011670782,61.7268335287748));
#53434=CARTESIAN_POINT('Ctrl Pts',(-5.32400912976953,2.76398560624496,61.6804423763008));
#53435=CARTESIAN_POINT('Ctrl Pts',(-4.73259444730769,3.55197665989223,61.6340512238268));
#53436=CARTESIAN_POINT('Ctrl Pts',(-4.14117976484579,4.33996771353959,61.5876600713528));
#53437=CARTESIAN_POINT('Ctrl Pts',(-3.34868920205137,4.97704433129704,61.5412689188788));
#53438=CARTESIAN_POINT('Ctrl Pts',(-2.45201861239238,5.38531272584916,61.4948777664049));
#53439=CARTESIAN_POINT('Ctrl Pts',(-1.55534802273349,5.79358112040123,61.4484866139309));
#53440=CARTESIAN_POINT('Ctrl Pts',(-0.554497406209885,5.97304129174803,
61.4020954614569));
#53441=CARTESIAN_POINT('Ctrl Pts',(0.428161709040809,5.90175109301285,61.3557043089829));
#53442=CARTESIAN_POINT('Ctrl Pts',(1.41082082429162,5.83046089427766,61.3093131565089));
#53443=CARTESIAN_POINT('Ctrl Pts',(2.37528843826953,5.50842032546052,61.2629220040349));
#53444=CARTESIAN_POINT('Ctrl Pts',(3.20364148603252,4.97500448728938,61.2165308515609));
#53445=CARTESIAN_POINT('Ctrl Pts',(4.0319945337955,4.44158864911823,61.1701396990869));
#53446=CARTESIAN_POINT('Ctrl Pts',(4.72423301534339,3.69679754159311,61.123748546613));
#53447=CARTESIAN_POINT('Ctrl Pts',(5.19571864559717,2.8316949295584,61.077357394139));
#53448=CARTESIAN_POINT('Ctrl Pts',(5.6672042758509,1.96659231752379,61.030966241665));
#53449=CARTESIAN_POINT('Ctrl Pts',(5.91793705481057,0.981178200979634,60.984575089191));
#53450=CARTESIAN_POINT('Ctrl Pts',(5.91726050698192,-0.00406327743461797,
60.938183936717));
#53451=CARTESIAN_POINT('Ctrl Pts',(5.91658395915327,-0.989304755848871,
60.8917927842431));
#53452=CARTESIAN_POINT('Ctrl Pts',(5.66449808453628,-1.97437359613322,60.8454016317691));
#53453=CARTESIAN_POINT('Ctrl Pts',(5.19182479843574,-2.83882787095668,60.7990104792951));
#53454=CARTESIAN_POINT('Ctrl Pts',(4.71915151233514,-3.70328214578024,60.7526193268211));
#53455=CARTESIAN_POINT('Ctrl Pts',(4.02589081475093,-4.44712185514289,60.7062281743471));
#53456=CARTESIAN_POINT('Ctrl Pts',(3.19680597404423,-4.97939956041544,60.6598370218731));
#53457=CARTESIAN_POINT('Ctrl Pts',(2.36772113333763,-5.51167726568792,60.6134458693991));
#53458=CARTESIAN_POINT('Ctrl Pts',(1.40281214950857,-5.83239296687034,60.5670547169252));
#53459=CARTESIAN_POINT('Ctrl Pts',(0.420056053873144,-5.90233354952841,
60.5206635644512));
#53460=CARTESIAN_POINT('Ctrl Pts',(-0.562700041762392,-5.97227413218649,
60.4742724119772));
#53461=CARTESIAN_POINT('Ctrl Pts',(-1.5633032492043,-5.79143959632015,60.4278812595032));
#53462=CARTESIAN_POINT('Ctrl Pts',(-2.45941229276507,-5.38194013273498,
60.3814901070292));
#53463=CARTESIAN_POINT('Ctrl Pts',(-3.35552133632579,-4.97244066914982,
60.3350989545552));
#53464=CARTESIAN_POINT('Ctrl Pts',(-4.14713621600539,-4.33427627784585,
60.2887078020812));
#53465=CARTESIAN_POINT('Ctrl Pts',(-4.73746814131828,-3.54547373818747,
60.2423166496073));
#53466=CARTESIAN_POINT('Ctrl Pts',(-5.32780006663118,-2.75667119852909,
60.1959254971333));
#53467=CARTESIAN_POINT('Ctrl Pts',(-5.71684903757736,-1.8172305105163,60.1495343446593));
#53468=CARTESIAN_POINT('Ctrl Pts',(-5.85704700015334,-0.842014760073484,
60.1031431921854));
#53469=CARTESIAN_POINT('Ctrl Pts',(-5.89710774647858,-0.563352573597715,
60.0898871921919));
#53470=CARTESIAN_POINT('Ctrl Pts',(-5.91684987917482,-0.281769363510951,
60.0766311921983));
#53471=CARTESIAN_POINT('Ctrl Pts',(-5.91658334351688,-0.000149097059289338,
60.0633751922048));
#53472=CARTESIAN_POINT('Ctrl Pts',(-5.91673072200561,-0.000155070081382937,
59.8116248077951));
#53473=CARTESIAN_POINT('Ctrl Pts',(-5.91697061337809,-0.233560574909101,
59.8226121023432));
#53474=CARTESIAN_POINT('Ctrl Pts',(-5.90342332074282,-0.466938404398139,
59.8335993968914));
#53475=CARTESIAN_POINT('Ctrl Pts',(-5.87587228115627,-0.698651164660174,
59.8445866914395));
#53476=CARTESIAN_POINT('Ctrl Pts',(-5.75954478372911,-1.67700138039482,
59.8909778439134));
#53477=CARTESIAN_POINT('Ctrl Pts',(-5.39356643969452,-2.62566768769933,
59.9373689963874));
#53478=CARTESIAN_POINT('Ctrl Pts',(-4.82268451464387,-3.42865900703989,
59.9837601488614));
#53479=CARTESIAN_POINT('Ctrl Pts',(-4.25180258959316,-4.23165032638054,
60.0301513013354));
#53480=CARTESIAN_POINT('Ctrl Pts',(-3.47601708352634,-4.88896665775721,
60.0765424538094));
#53481=CARTESIAN_POINT('Ctrl Pts',(-2.59018136863848,-5.32023956151416,
60.1229336062834));
#53482=CARTESIAN_POINT('Ctrl Pts',(-1.70434565375068,-5.75151246527109,
60.1693247587573));
#53483=CARTESIAN_POINT('Ctrl Pts',(-0.708459730041834,-5.95674194140831,
60.2157159112313));
#53484=CARTESIAN_POINT('Ctrl Pts',(0.275711897420253,-5.9108350902356,60.2621070637053));
#53485=CARTESIAN_POINT('Ctrl Pts',(1.25988352488228,-5.8649282390629,60.3084982161793));
#53486=CARTESIAN_POINT('Ctrl Pts',(2.23234085609756,-5.56788506058028,60.3548893686533));
#53487=CARTESIAN_POINT('Ctrl Pts',(3.07418394196869,-5.05602428843925,60.4012805211273));
#53488=CARTESIAN_POINT('Ctrl Pts',(3.91602702783991,-4.54416351629815,60.4476716736012));
#53489=CARTESIAN_POINT('Ctrl Pts',(4.62725586836695,-3.81748515049858,60.4940628260752));
#53490=CARTESIAN_POINT('Ctrl Pts',(5.12091027494375,-2.96483835483668,60.5404539785492));
#53491=CARTESIAN_POINT('Ctrl Pts',(5.61456468152053,-2.11219155917483,60.5868451310232));
#53492=CARTESIAN_POINT('Ctrl Pts',(5.8906446541471,-1.13357633365067,60.6332362834972));
#53493=CARTESIAN_POINT('Ctrl Pts',(5.91539457842234,-0.148645537839881,
60.6796274359712));
#53494=CARTESIAN_POINT('Ctrl Pts',(5.94014450269758,0.836285257970903,60.7260185884451));
#53495=CARTESIAN_POINT('Ctrl Pts',(5.71356437862149,1.8275316240683,60.7724097409191));
#53496=CARTESIAN_POINT('Ctrl Pts',(5.26335759672681,2.70389632259119,60.8188008933931));
#53497=CARTESIAN_POINT('Ctrl Pts',(4.81315081483215,3.58026102111402,60.8651920458671));
#53498=CARTESIAN_POINT('Ctrl Pts',(4.13931737511893,4.34174405206235,60.9115831983411));
#53499=CARTESIAN_POINT('Ctrl Pts',(3.32424522315754,4.89524077146601,60.9579743508151));
#53500=CARTESIAN_POINT('Ctrl Pts',(2.50917307119606,5.44873749086974,61.0043655032891));
#53501=CARTESIAN_POINT('Ctrl Pts',(1.55286220698639,5.79424789872876,61.050756655763));
#53502=CARTESIAN_POINT('Ctrl Pts',(0.572238391115561,5.88952729327051,61.097147808237));
#53503=CARTESIAN_POINT('Ctrl Pts',(-0.408385424755208,5.98480668781225,
61.143538960711));
#53504=CARTESIAN_POINT('Ctrl Pts',(-1.41332219228712,5.82985506903674,61.189930113185));
#53505=CARTESIAN_POINT('Ctrl Pts',(-2.31970078218799,5.44361798762822,61.236321265659));
#53506=CARTESIAN_POINT('Ctrl Pts',(-3.22607937208887,5.05738090621969,61.282712418133));
#53507=CARTESIAN_POINT('Ctrl Pts',(-4.0338997843587,4.43985836217815,61.3291035706069));
#53508=CARTESIAN_POINT('Ctrl Pts',(-4.64439181811148,3.66655330720706,61.3754947230809));
#53509=CARTESIAN_POINT('Ctrl Pts',(-5.25488385186429,2.89324825223592,61.4218858755549));
#53510=CARTESIAN_POINT('Ctrl Pts',(-5.66804750710004,1.96416068633522,61.4682770280289));
#53511=CARTESIAN_POINT('Ctrl Pts',(-5.83336628722356,0.992887845105691,
61.5146681805029));
#53512=CARTESIAN_POINT('Ctrl Pts',(-5.88914425298273,0.665183858659447,
61.5303203896003));
#53513=CARTESIAN_POINT('Ctrl Pts',(-5.91670846302273,0.332677654485142,
61.5459725986977));
#53514=CARTESIAN_POINT('Ctrl Pts',(-5.91644646386006,0.000128480793576948,
61.5616248077951));
#53515=CARTESIAN_POINT('Origin',(0.,0.,0.));
#53516=CARTESIAN_POINT('',(-5.91675,7.2459289488551E-16,66.));
#53517=CARTESIAN_POINT('Origin',(0.,0.,66.));
#53518=CARTESIAN_POINT('',(-5.91675,-7.2459289488551E-16,64.));
#53519=CARTESIAN_POINT('',(-5.91675,-7.2459289488551E-16,0.));
#53520=CARTESIAN_POINT('',(-0.0185920708322156,-5.91672078920428,64.));
#53521=CARTESIAN_POINT('Origin',(0.,0.,64.));
#53522=CARTESIAN_POINT('',(-5.9170192319132,-0.000147776431128344,63.5633751922049));
#53523=CARTESIAN_POINT('Ctrl Pts',(-0.0185920708322163,-5.91672078920428,
64.));
#53524=CARTESIAN_POINT('Ctrl Pts',(-1.00409531133336,-5.91362404918467,
63.953608847526));
#53525=CARTESIAN_POINT('Ctrl Pts',(-1.98830837177191,-5.65954316834941,
63.907217695052));
#53526=CARTESIAN_POINT('Ctrl Pts',(-2.85153274099139,-5.18487830611679,
63.8608265425781));
#53527=CARTESIAN_POINT('Ctrl Pts',(-3.71475711021086,-4.71021344388416,
63.8144353901041));
#53528=CARTESIAN_POINT('Ctrl Pts',(-4.45699278821126,-4.01496460025418,
63.7680442376301));
#53529=CARTESIAN_POINT('Ctrl Pts',(-4.98725841148824,-3.18453283331056,
63.7216530851561));
#53530=CARTESIAN_POINT('Ctrl Pts',(-5.51752403476525,-2.35410106636689,
63.6752619326821));
#53531=CARTESIAN_POINT('Ctrl Pts',(-5.83581960331881,-1.38848637610957,
63.6288707802081));
#53532=CARTESIAN_POINT('Ctrl Pts',(-5.90333451661355,-0.405580965178079,
63.5824796277342));
#53533=CARTESIAN_POINT('Ctrl Pts',(-5.91260233486136,-0.27065686828223,
63.5761114825577));
#53534=CARTESIAN_POINT('Ctrl Pts',(-5.91714463294472,-0.135406958180736,
63.5697433373813));
#53535=CARTESIAN_POINT('Ctrl Pts',(-5.9170192319132,-0.000147776431128344,
63.5633751922049));
#53536=CARTESIAN_POINT('',(-5.9171574445836,-8.64418186984388E-5,63.3116248077951));
#53537=CARTESIAN_POINT('',(-5.91675,-7.2459289488551E-16,0.));
#53538=CARTESIAN_POINT('',(4.63776713187073,-3.67456288307085,64.));
#53539=CARTESIAN_POINT('Ctrl Pts',(-5.9171574445836,-8.64418186984388E-5,
63.3116248077951));
#53540=CARTESIAN_POINT('Ctrl Pts',(-5.91721937759278,-0.0871536346831795,
63.3157242475262));
#53541=CARTESIAN_POINT('Ctrl Pts',(-5.91533756169338,-0.174218156234632,
63.3198236872572));
#53542=CARTESIAN_POINT('Ctrl Pts',(-5.91149447524869,-0.261196029287235,
63.3239231269883));
#53543=CARTESIAN_POINT('Ctrl Pts',(-5.86800433490684,-1.24547779347176,
63.3703142794623));
#53544=CARTESIAN_POINT('Ctrl Pts',(-5.57334936954011,-2.21866315124588,
63.4167054319362));
#53545=CARTESIAN_POINT('Ctrl Pts',(-5.06355767648185,-3.06175989147063,
63.4630965844102));
#53546=CARTESIAN_POINT('Ctrl Pts',(-4.55376598342356,-3.90485663169542,
63.5094877368842));
#53547=CARTESIAN_POINT('Ctrl Pts',(-3.82883756267365,-4.61786475437092,
63.5558788893582));
#53548=CARTESIAN_POINT('Ctrl Pts',(-2.97740495481013,-5.11361285815225,
63.6022700418322));
#53549=CARTESIAN_POINT('Ctrl Pts',(-2.12597234694665,-5.60936096193355,
63.6486611943062));
#53550=CARTESIAN_POINT('Ctrl Pts',(-1.14803555196965,-5.88784904682074,
63.6950523467801));
#53551=CARTESIAN_POINT('Ctrl Pts',(-0.163169671587142,-5.91501470558879,
63.7414434992541));
#53552=CARTESIAN_POINT('Ctrl Pts',(0.821696208795361,-5.94218036435685,
63.7878346517281));
#53553=CARTESIAN_POINT('Ctrl Pts',(1.8134911745833,-5.71802359700571,63.8342258042021));
#53554=CARTESIAN_POINT('Ctrl Pts',(2.6909610407991,-5.26997560876332,63.8806169566761));
#53555=CARTESIAN_POINT('Ctrl Pts',(3.44365501703819,-4.88563987850002,63.9204113044507));
#53556=CARTESIAN_POINT('Ctrl Pts',(4.11222612983174,-4.33656017974518,63.9602056522253));
#53557=CARTESIAN_POINT('Ctrl Pts',(4.63776713187073,-3.67456288307085,64.));
#53558=CARTESIAN_POINT('Origin',(0.,0.,64.));
#53559=CARTESIAN_POINT('Origin',(0.,0.,-3.23514056400933));
#53560=CARTESIAN_POINT('',(-4.91810492716115,0.000123316961498904,62.3898594359907));
#53561=CARTESIAN_POINT('',(-4.91858868497457,-7.18540524885514E-5,62.7351405640092));
#53562=CARTESIAN_POINT('',(-4.91825,1.47989506776076E-12,-3.23514056400933));
#53563=CARTESIAN_POINT('',(-4.31134524531351,2.36723698448027,64.));
#53564=CARTESIAN_POINT('Ctrl Pts',(-4.91810492716115,0.000123316961498816,
62.3898594359907));
#53565=CARTESIAN_POINT('Ctrl Pts',(-4.9175571550679,-0.582778007190868,
62.4228670848126));
#53566=CARTESIAN_POINT('Ctrl Pts',(-4.66822121487943,-1.98538387797463,
62.5022658861086));
#53567=CARTESIAN_POINT('Ctrl Pts',(-3.36401880748098,-3.86991586995366,
62.6280558398784));
#53568=CARTESIAN_POINT('Ctrl Pts',(-1.09843433267496,-5.00862398811822,
62.7672292973006));
#53569=CARTESIAN_POINT('Ctrl Pts',(1.4357556111677,-4.92254766049344,62.9064027547223));
#53570=CARTESIAN_POINT('Ctrl Pts',(3.61885342162015,-3.63273659425221,63.0455762121445));
#53571=CARTESIAN_POINT('Ctrl Pts',(4.91701390374655,-1.45459279213023,63.1847496695662));
#53572=CARTESIAN_POINT('Ctrl Pts',(5.01279380401881,1.07924733972977,63.3239231269884));
#53573=CARTESIAN_POINT('Ctrl Pts',(3.88276674436703,3.34917871604949,63.4630965844101));
#53574=CARTESIAN_POINT('Ctrl Pts',(1.80327337436161,4.80010868768094,63.6022700418323));
#53575=CARTESIAN_POINT('Ctrl Pts',(-0.717195690581678,5.07726303778206,
63.741443499254));
#53576=CARTESIAN_POINT('Ctrl Pts',(-2.95110573148774,4.15852613293832,63.8740201519768));
#53577=CARTESIAN_POINT('Ctrl Pts',(-3.97259884441697,2.98278400958921,63.9602056522253));
#53578=CARTESIAN_POINT('Ctrl Pts',(-4.31134524531351,2.36723698448027,64.));
#53579=CARTESIAN_POINT('',(0.837162017642518,4.84647736182856,64.));
#53580=CARTESIAN_POINT('Origin',(0.,0.,64.));
#53581=CARTESIAN_POINT('Ctrl Pts',(-4.91858868497457,-7.18540524887162E-5,
62.7351405640092));
#53582=CARTESIAN_POINT('Ctrl Pts',(-4.91864016628146,-0.0724457453455965,
62.7392400037402));
#53583=CARTESIAN_POINT('Ctrl Pts',(-4.89937421430555,-0.963808652612014,
62.7897305959453));
#53584=CARTESIAN_POINT('Ctrl Pts',(-4.38787150941422,-2.6531979430407,62.8866123406244));
#53585=CARTESIAN_POINT('Ctrl Pts',(-2.5800990640586,-4.43124443783022,63.0257857980463));
#53586=CARTESIAN_POINT('Ctrl Pts',(-0.141393199236074,-5.12571725998609,
63.1649592554683));
#53587=CARTESIAN_POINT('Ctrl Pts',(2.33187113869595,-4.56673182658543,63.3041327128902));
#53588=CARTESIAN_POINT('Ctrl Pts',(4.23494465804981,-2.89109992630838,63.4433061703121));
#53589=CARTESIAN_POINT('Ctrl Pts',(5.10236059910481,-0.508337431653702,
63.5824796277342));
#53590=CARTESIAN_POINT('Ctrl Pts',(4.72219820521398,1.9984257720543,63.721653085156));
#53591=CARTESIAN_POINT('Ctrl Pts',(3.18703877163087,4.01712720269185,63.8608265425781));
#53592=CARTESIAN_POINT('Ctrl Pts',(1.64440293964314,4.70703764334184,63.953608847526));
#53593=CARTESIAN_POINT('Ctrl Pts',(0.837162017642518,4.84647736182856,64.));
#53594=CARTESIAN_POINT('Origin',(0.,0.,-3.23514056400933));
#53595=CARTESIAN_POINT('',(-4.91811146816273,-0.000123935709421355,60.6398594359907));
#53596=CARTESIAN_POINT('',(-4.91799768806857,0.000106798609499636,60.9851405640092));
#53597=CARTESIAN_POINT('',(-4.91825,1.47989506776076E-12,-3.23514056400933));
#53598=CARTESIAN_POINT('Ctrl Pts',(-4.91811146816274,-0.000123935709421541,
60.6398594359907));
#53599=CARTESIAN_POINT('Ctrl Pts',(-4.91833302374643,-0.234218476711904,
60.6531154359842));
#53600=CARTESIAN_POINT('Ctrl Pts',(-4.84449183696287,-1.28741970532662,
60.7127625884516));
#53601=CARTESIAN_POINT('Ctrl Pts',(-4.10529641718065,-3.07236274745144,
60.8188008933932));
#53602=CARTESIAN_POINT('Ctrl Pts',(-2.13122625265585,-4.663769525259,60.957974350815));
#53603=CARTESIAN_POINT('Ctrl Pts',(0.364003421574487,-5.11472120786763,
61.0971478082371));
#53604=CARTESIAN_POINT('Ctrl Pts',(2.77022150230343,-4.31494430466559,61.236321265659));
#53605=CARTESIAN_POINT('Ctrl Pts',(4.49902334075878,-2.46001229778389,61.375494723081));
#53606=CARTESIAN_POINT('Ctrl Pts',(5.12765629947872,-0.00352107013592945,
61.5146681805029));
#53607=CARTESIAN_POINT('Ctrl Pts',(4.50239758982308,2.45383118170519,61.6538416379248));
#53608=CARTESIAN_POINT('Ctrl Pts',(2.77614487750337,4.31113571438885,61.7930150953468));
#53609=CARTESIAN_POINT('Ctrl Pts',(0.371027452000867,5.11421647371715,61.9321885527688));
#53610=CARTESIAN_POINT('Ctrl Pts',(-2.12481919255064,4.6666920788757,62.0713620101907));
#53611=CARTESIAN_POINT('Ctrl Pts',(-4.10107307033674,3.0779979096349,62.2105354676127));
#53612=CARTESIAN_POINT('Ctrl Pts',(-4.84361095490587,1.29192670121819,62.3167012762126));
#53613=CARTESIAN_POINT('Ctrl Pts',(-4.91832703052422,0.236470414648976,
62.3764759323386));
#53614=CARTESIAN_POINT('Ctrl Pts',(-4.91810492716115,0.000123316961498816,
62.3898594359907));
#53615=CARTESIAN_POINT('Ctrl Pts',(-4.91799768806857,0.000106798609499498,
60.9851405640092));
#53616=CARTESIAN_POINT('Ctrl Pts',(-4.91756998676071,-0.542764083599964,
61.0158795073858));
#53617=CARTESIAN_POINT('Ctrl Pts',(-4.69265409152509,-1.90528028643671,
61.0930096032364));
#53618=CARTESIAN_POINT('Ctrl Pts',(-3.45757268999299,-3.78656344121777,
61.2165308515608));
#53619=CARTESIAN_POINT('Ctrl Pts',(-1.22048811252045,-4.98028918333677,
61.355704308983));
#53620=CARTESIAN_POINT('Ctrl Pts',(1.31504858454702,-4.95615968794384,61.4948777664048));
#53621=CARTESIAN_POINT('Ctrl Pts',(3.52900980989584,-3.72007544198956,61.6340512238268));
#53622=CARTESIAN_POINT('Ctrl Pts',(4.8800044701548,-1.57430240300827,61.7732246812487));
#53623=CARTESIAN_POINT('Ctrl Pts',(5.0376669914975,0.956442797563212,61.9123981386707));
#53624=CARTESIAN_POINT('Ctrl Pts',(3.96344342536178,3.25330411499177,62.0515715960926));
#53625=CARTESIAN_POINT('Ctrl Pts',(1.92001895732006,4.75461875552336,62.1907450535146));
#53626=CARTESIAN_POINT('Ctrl Pts',(-0.592917275387842,5.09326210086,62.3299185109366));
#53627=CARTESIAN_POINT('Ctrl Pts',(-2.96086476568654,4.18642510396251,62.4690919683585));
#53628=CARTESIAN_POINT('Ctrl Pts',(-4.55635401914054,2.31272501981761,62.6041659860494));
#53629=CARTESIAN_POINT('Ctrl Pts',(-4.91805758004674,0.746570619418092,
62.6928488512663));
#53630=CARTESIAN_POINT('Ctrl Pts',(-4.91858868497457,-7.18540524887162E-5,
62.7351405640092));
#53631=CARTESIAN_POINT('Origin',(0.,0.,-3.23514056400933));
#53632=CARTESIAN_POINT('',(-4.91848050031426,0.00010358560867039,58.8898594359906));
#53633=CARTESIAN_POINT('',(-4.91823397532498,-0.000128900733881165,59.2351405640092));
#53634=CARTESIAN_POINT('',(-4.91825,1.47989506776076E-12,-3.23514056400933));
#53635=CARTESIAN_POINT('Ctrl Pts',(-4.91848050031426,0.00010358560867018,
58.8898594359906));
#53636=CARTESIAN_POINT('Ctrl Pts',(-4.91782358364168,-0.704279469166761,
58.9297549396297));
#53637=CARTESIAN_POINT('Ctrl Pts',(-4.58708483673057,-2.2283277297391,59.0160415957427));
#53638=CARTESIAN_POINT('Ctrl Pts',(-3.06791804765684,-4.10861903535706,
59.1487194043298));
#53639=CARTESIAN_POINT('Ctrl Pts',(-0.724162310693165,-5.07626442106874,
59.2878928617516));
#53640=CARTESIAN_POINT('Ctrl Pts',(1.79667649020643,-4.80258525321274,59.4270663191736));
#53641=CARTESIAN_POINT('Ctrl Pts',(3.87816492297812,-3.35450567968201,59.5662397765956));
#53642=CARTESIAN_POINT('Ctrl Pts',(5.01130611802573,-1.08613190555986,59.7054132340175));
#53643=CARTESIAN_POINT('Ctrl Pts',(4.91900734112638,1.44783918401923,59.8445866914394));
#53644=CARTESIAN_POINT('Ctrl Pts',(3.6238388779325,3.62776285217508,59.9837601488615));
#53645=CARTESIAN_POINT('Ctrl Pts',(1.44251480813104,4.92057136450247,60.1229336062833));
#53646=CARTESIAN_POINT('Ctrl Pts',(-1.09155468659011,5.01012773200588,60.2621070637055));
#53647=CARTESIAN_POINT('Ctrl Pts',(-3.35870080584726,3.87453228424406,60.4012805211271));
#53648=CARTESIAN_POINT('Ctrl Pts',(-4.66681476051984,1.9898847672322,60.5271979785559));
#53649=CARTESIAN_POINT('Ctrl Pts',(-4.91755766022277,0.58502681223606,60.6067242835102));
#53650=CARTESIAN_POINT('Ctrl Pts',(-4.91811146816274,-0.000123935709421541,
60.6398594359907));
#53651=CARTESIAN_POINT('Ctrl Pts',(-4.91823397532498,-0.000128900733881599,
59.2351405640092));
#53652=CARTESIAN_POINT('Ctrl Pts',(-4.91843338306455,-0.19414531584724,
59.2461278585573));
#53653=CARTESIAN_POINT('Ctrl Pts',(-4.85962517914547,-1.20722825103876,
59.3035063055794));
#53654=CARTESIAN_POINT('Ctrl Pts',(-4.17914144614525,-2.97113587204582,
59.4072759050756));
#53655=CARTESIAN_POINT('Ctrl Pts',(-2.24454539330572,-4.61030233004723,
59.5464493624975));
#53656=CARTESIAN_POINT('Ctrl Pts',(0.238920670469636,-5.12208829582852,
59.6856228199195));
#53657=CARTESIAN_POINT('Ctrl Pts',(2.6639622571092,-4.38134416472343,59.8247962773414));
#53658=CARTESIAN_POINT('Ctrl Pts',(4.43757171073933,-2.56920783687788,59.9639697347634));
#53659=CARTESIAN_POINT('Ctrl Pts',(5.12603936208722,-0.128810152540617,
60.1031431921853));
#53660=CARTESIAN_POINT('Ctrl Pts',(4.56101074237015,2.34308612838655,60.2423166496072));
#53661=CARTESIAN_POINT('Ctrl Pts',(2.88065515110656,4.24201573516153,60.3814901070293));
#53662=CARTESIAN_POINT('Ctrl Pts',(0.495878420013193,5.10362382919256,60.5206635644512));
#53663=CARTESIAN_POINT('Ctrl Pts',(-2.01015796326168,4.7172170354076,60.6598370218731));
#53664=CARTESIAN_POINT('Ctrl Pts',(-4.02464027668354,3.1772853572572,60.7990104792952));
#53665=CARTESIAN_POINT('Ctrl Pts',(-4.82739314863554,1.37212243363073,60.9074449933404));
#53666=CARTESIAN_POINT('Ctrl Pts',(-4.91821547272759,0.276535576824915,
60.9694883549118));
#53667=CARTESIAN_POINT('Ctrl Pts',(-4.91799768806857,0.000106798609499498,
60.9851405640092));
#53668=CARTESIAN_POINT('Origin',(0.,0.,-3.23514056400933));
#53669=CARTESIAN_POINT('',(-4.91785549949367,-4.93860172708709E-5,57.1398594359907));
#53670=CARTESIAN_POINT('',(-4.91835888437606,0.000122206298215147,57.4851405640092));
#53671=CARTESIAN_POINT('',(-4.91825,1.47989506776076E-12,-3.23514056400933));
#53672=CARTESIAN_POINT('Ctrl Pts',(-4.91785549949367,-4.93860172707736E-5,
57.1398594359907));
#53673=CARTESIAN_POINT('Ctrl Pts',(-4.91798030716673,-0.355833168158426,
57.1600032908012));
#53674=CARTESIAN_POINT('Ctrl Pts',(-4.79221627138776,-1.53089751854342,
57.2265382980858));
#53675=CARTESIAN_POINT('Ctrl Pts',(-3.86627298300154,-3.36820497383239,
57.3394644578443));
#53676=CARTESIAN_POINT('Ctrl Pts',(-1.77967451752562,-4.80891153344568,
57.4786379152663));
#53677=CARTESIAN_POINT('Ctrl Pts',(0.742116737907104,-5.07367069015669,
57.6178113726882));
#53678=CARTESIAN_POINT('Ctrl Pts',(3.08243444271975,-4.09773955140781,57.7569848301102));
#53679=CARTESIAN_POINT('Ctrl Pts',(4.66898889937891,-2.11976748307766,57.8961582875321));
#53680=CARTESIAN_POINT('Ctrl Pts',(5.1138119408897,0.376562024175001,58.0353317449541));
#53681=CARTESIAN_POINT('Ctrl Pts',(4.30812874434728,2.78080891953505,58.1745052023761));
#53682=CARTESIAN_POINT('Ctrl Pts',(2.4489570872563,4.50505057791964,58.313678659798));
#53683=CARTESIAN_POINT('Ctrl Pts',(-0.00907040374824587,5.12764948613034,
58.45285211722));
#53684=CARTESIAN_POINT('Ctrl Pts',(-2.46487986315524,4.49635839152627,58.5920255746418));
#53685=CARTESIAN_POINT('Ctrl Pts',(-4.31793981191222,2.76555009094761,58.7311990320639));
#53686=CARTESIAN_POINT('Ctrl Pts',(-4.88659449671919,1.04848275830739,58.8304769858468));
#53687=CARTESIAN_POINT('Ctrl Pts',(-4.91858745722994,0.114788814563554,
58.8833637871557));
#53688=CARTESIAN_POINT('Ctrl Pts',(-4.91848050031426,0.00010358560867018,
58.8898594359906));
#53689=CARTESIAN_POINT('Ctrl Pts',(-4.91835888437606,0.000122206298215008,
57.4851405640092));
#53690=CARTESIAN_POINT('Ctrl Pts',(-4.91767592747949,-0.664252687686942,
57.5227673622028));
#53691=CARTESIAN_POINT('Ctrl Pts',(-4.61497929133975,-2.14835763545905,
57.6067853128706));
#53692=CARTESIAN_POINT('Ctrl Pts',(-3.16739287834083,-4.03243027853956,
57.7371944160121));
#53693=CARTESIAN_POINT('Ctrl Pts',(-0.847980520678397,-5.05705454129148,
57.8763678734341));
#53694=CARTESIAN_POINT('Ctrl Pts',(1.67879279259075,-4.84505173931014,58.0155413308561));
#53695=CARTESIAN_POINT('Ctrl Pts',(3.79504243314771,-3.44826398752403,58.1547147882779));
#53696=CARTESIAN_POINT('Ctrl Pts',(4.98327119785246,-1.20825484302812,58.2938882457));
#53697=CARTESIAN_POINT('Ctrl Pts',(4.95291551110372,1.32721495505253,58.4330617031219));
#53698=CARTESIAN_POINT('Ctrl Pts',(3.71139840215604,3.53813418308582,58.5722351605439));
#53699=CARTESIAN_POINT('Ctrl Pts',(1.56231431431994,4.88385560600616,58.7114086179658));
#53700=CARTESIAN_POINT('Ctrl Pts',(-0.968810376189768,5.0353031737954,58.8505820753878));
#53701=CARTESIAN_POINT('Ctrl Pts',(-3.26302697682058,3.95544264850191,58.9897555328096));
#53702=CARTESIAN_POINT('Ctrl Pts',(-4.6411916976814,2.06995008540387,59.1179416956836));
#53703=CARTESIAN_POINT('Ctrl Pts',(-4.91759143286374,0.625041341663855,
59.1997367060834));
#53704=CARTESIAN_POINT('Ctrl Pts',(-4.91823397532498,-0.000128900733881599,
59.2351405640092));
#53705=CARTESIAN_POINT('Origin',(0.,0.,-3.23514056400933));
#53706=CARTESIAN_POINT('',(-4.91867501376679,-7.41635971235237E-6,55.3898594359907));
#53707=CARTESIAN_POINT('',(-4.91791390643375,-8.17280424678102E-5,55.7351405640092));
#53708=CARTESIAN_POINT('',(-4.91825,1.47989506776076E-12,-3.23514056400933));
#53709=CARTESIAN_POINT('Ctrl Pts',(-4.91867457786214,-7.40875330833691E-6,
55.3898594359907));
#53710=CARTESIAN_POINT('Ctrl Pts',(-4.91867518670192,-0.00693128766223378,
55.3902516419728));
#53711=CARTESIAN_POINT('Ctrl Pts',(-4.91696789858484,-0.832829426367756,
55.4370350004289));
#53712=CARTESIAN_POINT('Ctrl Pts',(-4.4902920805669,-2.47591368105495,55.530209511359));
#53713=CARTESIAN_POINT('Ctrl Pts',(-2.75493862771526,-4.32471787315188,
55.6693829687808));
#53714=CARTESIAN_POINT('Ctrl Pts',(-0.345906130887604,-5.11597698132539,
55.808556426203));
#53715=CARTESIAN_POINT('Ctrl Pts',(2.14771253755835,-4.65620042318322,55.9477298836247));
#53716=CARTESIAN_POINT('Ctrl Pts',(4.11614022189969,-3.05781968050709,56.0869033410469));
#53717=CARTESIAN_POINT('Ctrl Pts',(5.07802736785512,-0.711694861686717,
56.2260767984686));
#53718=CARTESIAN_POINT('Ctrl Pts',(4.79815885796941,1.80846429285365,56.3652502558907));
#53719=CARTESIAN_POINT('Ctrl Pts',(3.34497235117331,3.88639054840388,56.5044237133125));
#53720=CARTESIAN_POINT('Ctrl Pts',(1.07382287671086,5.01395811253837,56.6435971707346));
#53721=CARTESIAN_POINT('Ctrl Pts',(-1.45991392427294,4.91543719912591,56.7827706281565));
#53722=CARTESIAN_POINT('Ctrl Pts',(-3.63665060667076,3.61491962425697,56.9219440855785));
#53723=CARTESIAN_POINT('Ctrl Pts',(-4.73775454991443,1.74660915227116,57.0409736881899));
#53724=CARTESIAN_POINT('Ctrl Pts',(-4.91769287599503,0.463534318367552,
57.1136121383273));
#53725=CARTESIAN_POINT('Ctrl Pts',(-4.91785549949367,-4.93860172707736E-5,
57.1398594359907));
#53726=CARTESIAN_POINT('Ctrl Pts',(-4.91791390643376,-8.1728042467602E-5,
55.7351405640092));
#53727=CARTESIAN_POINT('Ctrl Pts',(-4.91809993511853,-0.315784565908389,
55.7530157133744));
#53728=CARTESIAN_POINT('Ctrl Pts',(-4.81049686766967,-1.45070185646176,
55.8172820152136));
#53729=CARTESIAN_POINT('Ctrl Pts',(-3.94741803979709,-3.27273011660468,
55.9279394695267));
#53730=CARTESIAN_POINT('Ctrl Pts',(-1.89664504433241,-4.76399088715083,
56.0671129269487));
#53731=CARTESIAN_POINT('Ctrl Pts',(0.617924134239044,-5.09028892710146,
56.2062863843707));
#53732=CARTESIAN_POINT('Ctrl Pts',(2.98138920623766,-4.17183293025696,56.3454598417926));
#53733=CARTESIAN_POINT('Ctrl Pts',(4.61580013163112,-2.23321757602816,56.4846332992146));
#53734=CARTESIAN_POINT('Ctrl Pts',(5.12148615964254,0.251497740818248,56.6238067566365));
#53735=CARTESIAN_POINT('Ctrl Pts',(4.37478933416524,2.67471304605202,56.7629802140585));
#53736=CARTESIAN_POINT('Ctrl Pts',(2.55830319774378,4.44386727360986,56.9021536714803));
#53737=CARTESIAN_POINT('Ctrl Pts',(0.116222271253945,5.12634021312587,57.0413271289025));
#53738=CARTESIAN_POINT('Ctrl Pts',(-2.35427907367985,4.55524331296145,57.1805005863242));
#53739=CARTESIAN_POINT('Ctrl Pts',(-4.24907667710245,2.87022977985227,57.3196740437464));
#53740=CARTESIAN_POINT('Ctrl Pts',(-4.87346654761257,1.12866042388539,57.4212207029745));
#53741=CARTESIAN_POINT('Ctrl Pts',(-4.91851796451275,0.154874064690948,
57.4763762097288));
#53742=CARTESIAN_POINT('Ctrl Pts',(-4.91835888437606,0.000122206298215008,
57.4851405640092));
#53743=CARTESIAN_POINT('Origin',(0.,0.,-3.23514056400933));
#53744=CARTESIAN_POINT('',(-4.91787233544528,6.11763386092418E-5,53.6398594359907));
#53745=CARTESIAN_POINT('',(-4.91865539329482,3.49302451308799E-5,53.9851405640092));
#53746=CARTESIAN_POINT('',(-4.91825,1.47989506776076E-12,-3.23514056400933));
#53747=CARTESIAN_POINT('Ctrl Pts',(-4.91787233544528,6.11763386090813E-5,
53.6398594359907));
#53748=CARTESIAN_POINT('Ctrl Pts',(-4.91766399181008,-0.477372253351672,
53.6668911456183));
#53749=CARTESIAN_POINT('Ctrl Pts',(-4.73018855874724,-1.77432527829267,
53.7403140077199));
#53750=CARTESIAN_POINT('Ctrl Pts',(-3.6059785727194,-3.64551643226655,53.8601280222955));
#53751=CARTESIAN_POINT('Ctrl Pts',(-1.41833159220866,-4.92759647489319,
53.9993014797174));
#53752=CARTESIAN_POINT('Ctrl Pts',(1.11614716940514,-5.00470648700459,54.1384749371395));
#53753=CARTESIAN_POINT('Ctrl Pts',(3.3776888316379,-3.85799036824427,54.2776483945613));
#53754=CARTESIAN_POINT('Ctrl Pts',(4.81326720014988,-1.76786039742912,54.4168218519834));
#53755=CARTESIAN_POINT('Ctrl Pts',(5.07183305260184,0.754573396941915,54.5559953094052));
#53756=CARTESIAN_POINT('Ctrl Pts',(4.09015797637785,3.09248755100316,54.6951687668272));
#53757=CARTESIAN_POINT('Ctrl Pts',(2.10829593137106,4.6741801196147,54.8343422242492));
#53758=CARTESIAN_POINT('Ctrl Pts',(-0.389118356134408,5.11287183779883,
54.9735156816711));
#53759=CARTESIAN_POINT('Ctrl Pts',(-2.79137956853432,4.30128720608217,55.1126891390931));
#53760=CARTESIAN_POINT('Ctrl Pts',(-4.50620442915501,2.44313837439632,55.251470390533));
#53761=CARTESIAN_POINT('Ctrl Pts',(-4.91860317153563,0.812043273740878,
55.3438604894988));
#53762=CARTESIAN_POINT('Ctrl Pts',(-4.91867457786214,-7.40875330833691E-6,
55.3898594359907));
#53763=CARTESIAN_POINT('Ctrl Pts',(-4.91865539329482,3.49302451308105E-5,
53.9851405640092));
#53764=CARTESIAN_POINT('Ctrl Pts',(-4.9183555947936,-0.785821442463661,
54.0296552170199));
#53765=CARTESIAN_POINT('Ctrl Pts',(-4.52666642387898,-2.39094983544162,
54.1205610225047));
#53766=CARTESIAN_POINT('Ctrl Pts',(-2.8597871012007,-4.25611199721682,54.2578579804633));
#53767=CARTESIAN_POINT('Ctrl Pts',(-0.470807616579455,-5.10599762879083,
54.3970314378853));
#53768=CARTESIAN_POINT('Ctrl Pts',(2.0333008302056,-4.70728789547995,54.5362048953072));
#53769=CARTESIAN_POINT('Ctrl Pts',(4.04019596500318,-3.15748130024849,54.6753783527292));
#53770=CARTESIAN_POINT('Ctrl Pts',(5.05912159376628,-0.835559870107751,
54.8145518101511));
#53771=CARTESIAN_POINT('Ctrl Pts',(4.84091469102418,1.69068523128142,54.9537252675731));
#53772=CARTESIAN_POINT('Ctrl Pts',(3.4389344917701,3.80349854191647,55.092898724995));
#53773=CARTESIAN_POINT('Ctrl Pts',(1.1960142884793,4.98622316175281,55.232072182417));
#53774=CARTESIAN_POINT('Ctrl Pts',(-1.33937332382694,4.94964147150757,55.3712456398389));
#53775=CARTESIAN_POINT('Ctrl Pts',(-3.54723721881863,3.70269897648656,55.5104190972609));
#53776=CARTESIAN_POINT('Ctrl Pts',(-4.7155139620973,1.82676430424734,55.6317174053177));
#53777=CARTESIAN_POINT('Ctrl Pts',(-4.91761713719032,0.503555076445749,
55.7066245609004));
#53778=CARTESIAN_POINT('Ctrl Pts',(-4.91791390643376,-8.1728042467602E-5,
55.7351405640092));
#53779=CARTESIAN_POINT('Origin',(0.,0.,-3.23514056400933));
#53780=CARTESIAN_POINT('',(-4.91843986782789,-0.000111326259341174,51.8898594359907));
#53781=CARTESIAN_POINT('',(-4.91783388548041,2.58376204584354E-5,52.2351405640092));
#53782=CARTESIAN_POINT('',(-4.91825,1.47989506776076E-12,-3.23514056400933));
#53783=CARTESIAN_POINT('Ctrl Pts',(-4.91843986782789,-0.000111326259340933,
51.8898594359907));
#53784=CARTESIAN_POINT('Ctrl Pts',(-4.91856549876998,-0.128648965742937,
51.8971394967898));
#53785=CARTESIAN_POINT('Ctrl Pts',(-4.88216901645989,-1.07620347337075,
51.950810710063));
#53786=CARTESIAN_POINT('Ctrl Pts',(-4.29441973117786,-2.80193338559416,
52.0508730758102));
#53787=CARTESIAN_POINT('Ctrl Pts',(-2.42680243173636,-4.51702352021277,
52.190046533232));
#53788=CARTESIAN_POINT('Ctrl Pts',(0.0342531119126611,-5.12754310066344,
52.3292199906541));
#53789=CARTESIAN_POINT('Ctrl Pts',(2.48693256926547,-4.48419869327436,52.468393448076));
#53790=CARTESIAN_POINT('Ctrl Pts',(4.33146985646582,-2.74431055228173,52.6075669054979));
#53791=CARTESIAN_POINT('Ctrl Pts',(5.1168109631927,-0.333342304227799,52.7467403629199));
#53792=CARTESIAN_POINT('Ctrl Pts',(4.65091246580963,2.15913981951461,52.8859138203419));
#53793=CARTESIAN_POINT('Ctrl Pts',(3.04770287479204,4.12363658823389,53.0250872777638));
#53794=CARTESIAN_POINT('Ctrl Pts',(0.699223121180822,5.07975969428112,53.1642607351858));
#53795=CARTESIAN_POINT('Ctrl Pts',(-1.82024119051244,4.79370352996499,53.3034341926077));
#53796=CARTESIAN_POINT('Ctrl Pts',(-3.89459273900518,3.33541885257685,53.4426076500297));
#53797=CARTESIAN_POINT('Ctrl Pts',(-4.79865591701777,1.50316999994343,53.554749397824));
#53798=CARTESIAN_POINT('Ctrl Pts',(-4.91802154601144,0.341987207742299,
53.6204999931443));
#53799=CARTESIAN_POINT('Ctrl Pts',(-4.91787233544528,6.11763386090813E-5,
53.6398594359907));
#53800=CARTESIAN_POINT('Ctrl Pts',(-4.91783388548041,2.58376204580538E-5,
52.2351405640092));
#53801=CARTESIAN_POINT('Ctrl Pts',(-4.91775404158717,-0.437347553613739,
52.2599035681915));
#53802=CARTESIAN_POINT('Ctrl Pts',(-4.75171544922939,-1.69415819232811,
52.3310577248477));
#53803=CARTESIAN_POINT('Ctrl Pts',(-3.69397722364766,-3.5563188648122,52.448603033978));
#53804=CARTESIAN_POINT('Ctrl Pts',(-1.53830997137995,-4.891469516311,52.5877764913998));
#53805=CARTESIAN_POINT('Ctrl Pts',(0.993527980457018,-5.03048444477228,
52.7269499488219));
#53806=CARTESIAN_POINT('Ctrl Pts',(3.28241352191931,-3.93936962827405,52.8661234062438));
#53807=CARTESIAN_POINT('Ctrl Pts',(4.76863392190279,-1.88494087862853,53.0052968636658));
#53808=CARTESIAN_POINT('Ctrl Pts',(5.08875620657422,0.630421975425304,53.1444703210877));
#53809=CARTESIAN_POINT('Ctrl Pts',(4.16449925833512,2.9916245627373,53.2836437785097));
#53810=CARTESIAN_POINT('Ctrl Pts',(2.22187629251225,4.62127010007193,53.4228172359315));
#53811=CARTESIAN_POINT('Ctrl Pts',(-0.264073294642276,5.12085314104043,
53.5619906933537));
#53812=CARTESIAN_POINT('Ctrl Pts',(-2.68544770655171,4.36820812375314,53.7011641507754));
#53813=CARTESIAN_POINT('Ctrl Pts',(-4.45013604008643,2.54738313211239,53.8403376081976));
#53814=CARTESIAN_POINT('Ctrl Pts',(-4.9102397975167,0.885267346271903,53.9349964126087));
#53815=CARTESIAN_POINT('Ctrl Pts',(-4.91866803119467,0.0331624278634732,
53.9832640645459));
#53816=CARTESIAN_POINT('Ctrl Pts',(-4.91865539329482,3.49302451308105E-5,
53.9851405640092));
#53817=CARTESIAN_POINT('Origin',(0.,0.,-3.23514056400933));
#53818=CARTESIAN_POINT('',(-4.91815264668802,0.000126960182705925,50.1398594359907));
#53819=CARTESIAN_POINT('',(-4.91855089394144,-8.54444238024277E-5,50.4851405640092));
#53820=CARTESIAN_POINT('',(-4.91825,1.47989506776076E-12,-3.23514056400933));
#53821=CARTESIAN_POINT('Ctrl Pts',(-4.91815264668802,0.000126960182705964,
50.1398594359907));
#53822=CARTESIAN_POINT('Ctrl Pts',(-4.91756388563138,-0.598861721200149,
50.1737790004354));
#53823=CARTESIAN_POINT('Ctrl Pts',(-4.65808367092927,-2.01757209091749,
50.254089717354));
#53824=CARTESIAN_POINT('Ctrl Pts',(-3.32584524149952,-3.90277144532342,
50.3807915867467));
#53825=CARTESIAN_POINT('Ctrl Pts',(-1.0491854679113,-5.01917138368084,50.5199650441687));
#53826=CARTESIAN_POINT('Ctrl Pts',(1.48403692230487,-4.90820801699284,50.6591385015906));
#53827=CARTESIAN_POINT('Ctrl Pts',(3.65436027550235,-3.59701577723358,50.7983119590126));
#53828=CARTESIAN_POINT('Ctrl Pts',(4.93106447073476,-1.40622711902959,50.9374854164345));
#53829=CARTESIAN_POINT('Ctrl Pts',(5.00195058892939,1.12843335237216,51.0766588738565));
#53830=CARTESIAN_POINT('Ctrl Pts',(3.8496844899148,3.38715232207621,51.2158323312784));
#53831=CARTESIAN_POINT('Ctrl Pts',(1.75603561718453,4.81759384299012,51.3550057887004));
#53832=CARTESIAN_POINT('Ctrl Pts',(-0.767025505920936,5.06996483203814,
51.4941792461224));
#53833=CARTESIAN_POINT('Ctrl Pts',(-3.10252201167498,4.08255173781169,51.6333527035442));
#53834=CARTESIAN_POINT('Ctrl Pts',(-4.59686080493138,2.20068426365062,51.7652461001671));
#53835=CARTESIAN_POINT('Ctrl Pts',(-4.91776493345185,0.690438868332923,
51.8507483443159));
#53836=CARTESIAN_POINT('Ctrl Pts',(-4.91843986782789,-0.000111326259340933,
51.8898594359907));
#53837=CARTESIAN_POINT('Ctrl Pts',(-4.91855089394144,-8.5444423802896E-5,
50.4851405640092));
#53838=CARTESIAN_POINT('Ctrl Pts',(-4.91862266471435,-0.0885607691173009,
50.490151919363));
#53839=CARTESIAN_POINT('Ctrl Pts',(-4.89464160083773,-0.996031568323749,
50.5415544271908));
#53840=CARTESIAN_POINT('Ctrl Pts',(-4.36160057317046,-2.69616617387836,
50.6393480874925));
#53841=CARTESIAN_POINT('Ctrl Pts',(-2.53644770583317,-4.45637797236955,
50.7785215449146));
#53842=CARTESIAN_POINT('Ctrl Pts',(-0.0910444821465626,-5.12684917852256,
50.9176950023364));
#53843=CARTESIAN_POINT('Ctrl Pts',(2.37662230816716,-4.54362608511847,51.0568684597585));
#53844=CARTESIAN_POINT('Ctrl Pts',(4.26312165309721,-2.84932717811426,51.1960419171803));
#53845=CARTESIAN_POINT('Ctrl Pts',(5.10713834860655,-0.458267918623071,
51.3352153746024));
#53846=CARTESIAN_POINT('Ctrl Pts',(4.70228073325844,2.04485390741571,51.4743888320243));
#53847=CARTESIAN_POINT('Ctrl Pts',(3.14755068263376,4.04793728920033,51.6135622894463));
#53848=CARTESIAN_POINT('Ctrl Pts',(0.823134181134756,5.06115813988206,51.7527357468682));
#53849=CARTESIAN_POINT('Ctrl Pts',(-1.70256747518846,4.83674845216052,51.8919092042902));
#53850=CARTESIAN_POINT('Ctrl Pts',(-3.8119317156975,3.42958425933908,52.0310826617121));
#53851=CARTESIAN_POINT('Ctrl Pts',(-4.77968458069813,1.58336278879033,52.1454931149518));
#53852=CARTESIAN_POINT('Ctrl Pts',(-4.91790362158959,0.382030238009249,
52.2135124157175));
#53853=CARTESIAN_POINT('Ctrl Pts',(-4.91783388548041,2.58376204580538E-5,
52.2351405640092));
#53854=CARTESIAN_POINT('Origin',(0.,0.,-3.23514056400933));
#53855=CARTESIAN_POINT('',(-4.91806577589784,-0.000118764820635008,48.3898594359907));
#53856=CARTESIAN_POINT('',(-4.91803852105498,0.000114651850740416,48.7351405640092));
#53857=CARTESIAN_POINT('',(-4.91825,1.47989506776076E-12,-3.23514056400933));
#53858=CARTESIAN_POINT('Ctrl Pts',(-4.91806577589784,-0.000118764820635602,
48.3898594359907));
#53859=CARTESIAN_POINT('Ctrl Pts',(-4.91828944893322,-0.250323965044822,
48.4040273516069));
#53860=CARTESIAN_POINT('Ctrl Pts',(-4.83812024217588,-1.31965428743371,
48.4645864196971));
#53861=CARTESIAN_POINT('Ctrl Pts',(-4.07492088157485,-3.11253776422747,
48.5715366402614));
#53862=CARTESIAN_POINT('Ctrl Pts',(-2.08531475831404,-4.68447797343466,
48.7107100976832));
#53863=CARTESIAN_POINT('Ctrl Pts',(0.414223905235385,-5.11089914605722,
48.8498835551053));
#53864=CARTESIAN_POINT('Ctrl Pts',(2.81247030707573,-4.28752636104482,48.9890570125271));
#53865=CARTESIAN_POINT('Ctrl Pts',(4.52296915308285,-2.41570312023185,49.1282304699492));
#53866=CARTESIAN_POINT('Ctrl Pts',(5.12744352931481,0.0468441941396368,
49.2674039273711));
#53867=CARTESIAN_POINT('Ctrl Pts',(4.47807826639135,2.49793646134371,49.4065773847931));
#53868=CARTESIAN_POINT('Ctrl Pts',(2.73366592873352,4.33819572114011,49.545750842215));
#53869=CARTESIAN_POINT('Ctrl Pts',(0.320776467523109,5.11761409083573,49.6849242996369));
#53870=CARTESIAN_POINT('Ctrl Pts',(-2.17055408191953,4.64559646356626,49.8240977570589));
#53871=CARTESIAN_POINT('Ctrl Pts',(-4.13110808915714,3.03756769151527,49.9632712144808));
#53872=CARTESIAN_POINT('Ctrl Pts',(-4.84983985353235,1.25969268032143,50.0685251074581));
#53873=CARTESIAN_POINT('Ctrl Pts',(-4.91836912309232,0.220363870376499,
50.1273878479614));
#53874=CARTESIAN_POINT('Ctrl Pts',(-4.91815264668802,0.000126960182705964,
50.1398594359907));
#53875=CARTESIAN_POINT('Ctrl Pts',(-4.91803852105498,0.00011465185073993,
48.7351405640092));
#53876=CARTESIAN_POINT('Ctrl Pts',(-4.91756009930081,-0.558847982386848,
48.7667914230085));
#53877=CARTESIAN_POINT('Ctrl Pts',(-4.68296776004553,-1.93748212711608,
48.8448334344818));
#53878=CARTESIAN_POINT('Ctrl Pts',(-3.4202133466128,-3.8203419036388,48.9692665984293));
#53879=CARTESIAN_POINT('Ctrl Pts',(-1.17151161743895,-4.99203687158382,
49.108440055851));
#53880=CARTESIAN_POINT('Ctrl Pts',(1.36366575896105,-4.94300387364647,49.2476135132731));
#53881=CARTESIAN_POINT('Ctrl Pts',(3.56537906630424,-3.68523319623146,49.386786970695));
#53882=CARTESIAN_POINT('Ctrl Pts',(4.89523223976419,-1.52629384976162,49.5259604281169));
#53883=CARTESIAN_POINT('Ctrl Pts',(5.02802957243399,1.00587783342514,49.6651338855389));
#53884=CARTESIAN_POINT('Ctrl Pts',(3.93129746246441,3.29207713437395,49.8043073429608));
#53885=CARTESIAN_POINT('Ctrl Pts',(1.87322534678482,4.77324820192809,49.9434808003828));
#53886=CARTESIAN_POINT('Ctrl Pts',(-0.642916015185119,5.08719280099207,
50.0826542578048));
#53887=CARTESIAN_POINT('Ctrl Pts',(-3.00184187982617,4.15714047460132,50.2218277152267));
#53888=CARTESIAN_POINT('Ctrl Pts',(-4.56820390101119,2.28061542819862,50.3559898172948));
#53889=CARTESIAN_POINT('Ctrl Pts',(-4.91795826783286,0.730473601480565,
50.443760766889));
#53890=CARTESIAN_POINT('Ctrl Pts',(-4.91855089394144,-8.5444423802896E-5,
50.4851405640092));
#53891=CARTESIAN_POINT('Origin',(0.,0.,-3.23514056400933));
#53892=CARTESIAN_POINT('',(-4.91852492696798,9.29568479803354E-5,46.6398594359908));
#53893=CARTESIAN_POINT('',(-4.91818357904255,-0.000128304591264783,46.9851405640093));
#53894=CARTESIAN_POINT('',(-4.91825,1.47989506776076E-12,-3.23514056400933));
#53895=CARTESIAN_POINT('Ctrl Pts',(-4.91852492696797,9.29568479802155E-5,
46.6398594359907));
#53896=CARTESIAN_POINT('Ctrl Pts',(-4.91790253050555,-0.720371784076569,
46.6806668552525));
#53897=CARTESIAN_POINT('Ctrl Pts',(-4.57554428714781,-2.26045534775418,
46.7678654269881));
#53898=CARTESIAN_POINT('Ctrl Pts',(-3.02741419179187,-4.13855467961632,
46.901455151198));
#53899=CARTESIAN_POINT('Ctrl Pts',(-0.674267066511626,-5.08313244445339,
47.0406286086197));
#53900=CARTESIAN_POINT('Ctrl Pts',(1.84376198687486,-4.78470618330867,47.179802066042));
#53901=CARTESIAN_POINT('Ctrl Pts',(3.91092661804106,-3.31625157567016,47.3189755234636));
#53902=CARTESIAN_POINT('Ctrl Pts',(5.02173262887484,-1.03685723652329,47.4581489808859));
#53903=CARTESIAN_POINT('Ctrl Pts',(4.90454902045194,1.49608503462231,47.5973224383075));
#53904=CARTESIAN_POINT('Ctrl Pts',(3.58803129184512,3.66318208304981,47.7364958957298));
#53905=CARTESIAN_POINT('Ctrl Pts',(1.39411416634107,4.93450273239808,47.8756693531515));
#53906=CARTESIAN_POINT('Ctrl Pts',(-1.14071273091822,4.99916452923466,48.0148428105736));
#53907=CARTESIAN_POINT('Ctrl Pts',(-3.39659538808254,3.84135539809756,48.1540162679954));
#53908=CARTESIAN_POINT('Ctrl Pts',(-4.67679570780214,1.95769151108293,48.2790218098013));
#53909=CARTESIAN_POINT('Ctrl Pts',(-4.91755705821536,0.568943166959013,
48.3576361991329));
#53910=CARTESIAN_POINT('Ctrl Pts',(-4.91806577589784,-0.000118764820635602,
48.3898594359907));
#53911=CARTESIAN_POINT('Ctrl Pts',(-4.91818357904256,-0.000128304591265078,
46.9851405640093));
#53912=CARTESIAN_POINT('Ctrl Pts',(-4.91839457111651,-0.210253745911707,
46.9970397741801));
#53913=CARTESIAN_POINT('Ctrl Pts',(-4.853665043705,-1.23946090468466,47.055330136825));
#53914=CARTESIAN_POINT('Ctrl Pts',(-4.14975662342901,-3.01204109589393,
47.1600116519437));
#53915=CARTESIAN_POINT('Ctrl Pts',(-2.19915360039652,-4.63212640575685,
47.2991851093658));
#53916=CARTESIAN_POINT('Ctrl Pts',(0.289219549406528,-5.11949447204388,
47.4383585667875));
#53917=CARTESIAN_POINT('Ctrl Pts',(2.7068683833997,-4.35496672226068,47.5775320242097));
#53918=CARTESIAN_POINT('Ctrl Pts',(4.4625930328204,-2.52549698484668,47.7167054816315));
#53919=CARTESIAN_POINT('Ctrl Pts',(5.12705728980988,-0.0784547261432202,
47.8558789390536));
#53920=CARTESIAN_POINT('Ctrl Pts',(4.53777635673904,2.38777246262433,47.9950523964754));
#53921=CARTESIAN_POINT('Ctrl Pts',(2.83885007366626,4.27010560247541,48.1342258538975));
#53922=CARTESIAN_POINT('Ctrl Pts',(0.445725457324341,5.10824827252355,48.2733993113193));
#53923=CARTESIAN_POINT('Ctrl Pts',(-2.0563946542149,4.69724521641816,48.4125727687414));
#53924=CARTESIAN_POINT('Ctrl Pts',(-4.05565420445089,3.13760108537823,48.5517462261632));
#53925=CARTESIAN_POINT('Ctrl Pts',(-4.83403602491591,1.33988709455419,48.659268824586));
#53926=CARTESIAN_POINT('Ctrl Pts',(-4.91826132944894,0.260432176572912,
48.7204002705346));
#53927=CARTESIAN_POINT('Ctrl Pts',(-4.91803852105498,0.00011465185073993,
48.7351405640092));
#53928=CARTESIAN_POINT('Origin',(0.,0.,-3.23514056400933));
#53929=CARTESIAN_POINT('',(-4.91784060085492,-3.50728131554851E-5,44.8898594359907));
#53930=CARTESIAN_POINT('',(-4.9184091500483,0.000116117112846786,45.2351405640092));
#53931=CARTESIAN_POINT('',(-4.91825,1.47989506776076E-12,-3.23514056400933));
#53932=CARTESIAN_POINT('Ctrl Pts',(-4.91784060085492,-3.50728131557135E-5,
44.8898594359907));
#53933=CARTESIAN_POINT('Ctrl Pts',(-4.9179329091661,-0.371928468127181,
44.910915206424));
#53934=CARTESIAN_POINT('Ctrl Pts',(-4.78457091277955,-1.5631312913108,44.9783621293313));
#53935=CARTESIAN_POINT('Ctrl Pts',(-3.83300314301673,-3.40601797271547,
45.0922002047124));
#53936=CARTESIAN_POINT('Ctrl Pts',(-1.73235436152806,-4.82615995289543,
45.2313736621346));
#53937=CARTESIAN_POINT('Ctrl Pts',(0.791915773395165,-5.06613668713003,
45.3705471195564));
#53938=CARTESIAN_POINT('Ctrl Pts',(3.12253474826594,-4.06726545368122,45.5097205769784));
#53939=CARTESIAN_POINT('Ctrl Pts',(4.68958454492302,-2.07380527553964,45.6488940344003));
#53940=CARTESIAN_POINT('Ctrl Pts',(5.10986656930181,0.426772970991213,45.7880674918224));
#53941=CARTESIAN_POINT('Ctrl Pts',(4.28060713724999,2.82299026944149,45.9272409492442));
#53942=CARTESIAN_POINT('Ctrl Pts',(2.40458924210636,4.52888751257782,46.0664144066663));
#53943=CARTESIAN_POINT('Ctrl Pts',(-0.0594349938974569,5.12731303962781,
46.205587864088));
#53944=CARTESIAN_POINT('Ctrl Pts',(-2.50892529093627,4.47193083682398,46.3447613215102));
#53945=CARTESIAN_POINT('Ctrl Pts',(-4.34489542661782,2.72300482125766,46.4839347789319));
#53946=CARTESIAN_POINT('Ctrl Pts',(-4.89158902769067,1.01625748485721,46.5823008170923));
#53947=CARTESIAN_POINT('Ctrl Pts',(-4.91861009030007,0.0986751013434063,
46.6342757027785));
#53948=CARTESIAN_POINT('Ctrl Pts',(-4.91852492696797,9.29568479802155E-5,
46.6398594359907));
#53949=CARTESIAN_POINT('Ctrl Pts',(-4.9184091500483,0.000116117112846665,
45.2351405640092));
#53950=CARTESIAN_POINT('Ctrl Pts',(-4.91772730570839,-0.680340376321463,
45.2736792778256));
#53951=CARTESIAN_POINT('Ctrl Pts',(-4.60390647175906,-2.18050870666077,
45.358609144116));
#53952=CARTESIAN_POINT('Ctrl Pts',(-3.12763256847743,-4.06334666422225,
45.4899301628804));
#53953=CARTESIAN_POINT('Ctrl Pts',(-0.798267987718407,-5.06513966409919,
45.6291036203023));
#53954=CARTESIAN_POINT('Ctrl Pts',(1.72630109211463,-4.82832850336539,45.7682770777242));
#53955=CARTESIAN_POINT('Ctrl Pts',(3.82872905502739,-3.41082181009738,45.9074505351462));
#53956=CARTESIAN_POINT('Ctrl Pts',(4.99489858245798,-1.15924964869784,46.0466239925681));
#53957=CARTESIAN_POINT('Ctrl Pts',(4.93964035540605,1.37579967883806,46.1857974499902));
#53958=CARTESIAN_POINT('Ctrl Pts',(3.67646694696398,3.57441776866221,46.3249709074119));
#53959=CARTESIAN_POINT('Ctrl Pts',(1.51426852463472,4.89896544510649,46.4641443648341));
#53960=CARTESIAN_POINT('Ctrl Pts',(-1.01822162097875,5.02554438122063,46.6033178222559));
#53961=CARTESIAN_POINT('Ctrl Pts',(-3.30172089569737,3.92320159104299,46.7424912796779));
#53962=CARTESIAN_POINT('Ctrl Pts',(-4.65162733209287,2.0377723478988,46.869765526929));
#53963=CARTESIAN_POINT('Ctrl Pts',(-4.91757198160569,0.608957045980571,
46.9506486217061));
#53964=CARTESIAN_POINT('Ctrl Pts',(-4.91818357904256,-0.000128304591265078,
46.9851405640093));
#53965=CARTESIAN_POINT('Origin',(0.,0.,-3.23514056400933));
#53966=CARTESIAN_POINT('',(-4.91866555055193,-2.44668497558952E-5,43.1398594359907));
#53967=CARTESIAN_POINT('',(-4.91788690158348,-6.94023299557811E-5,43.4851405640093));
#53968=CARTESIAN_POINT('',(-4.91825,1.47989506776076E-12,-3.23514056400933));
#53969=CARTESIAN_POINT('Ctrl Pts',(-4.91866555055193,-2.44668497561802E-5,
43.1398594359907));
#53970=CARTESIAN_POINT('Ctrl Pts',(-4.91867189362211,-0.0230471355164739,
43.1411635575955));
#53971=CARTESIAN_POINT('Ctrl Pts',(-4.91288415686364,-0.865045545929546,
43.1888588316743));
#53972=CARTESIAN_POINT('Ctrl Pts',(-4.4657564416411,-2.51989899178081,43.2829452582272));
#53973=CARTESIAN_POINT('Ctrl Pts',(-2.71232729414031,-4.35156893249991,
43.4221187156491));
#53974=CARTESIAN_POINT('Ctrl Pts',(-0.29563906707815,-5.11912776426357,
43.5612921730711));
#53975=CARTESIAN_POINT('Ctrl Pts',(2.19334327284283,-4.63488045286089,43.700465630493));
#53976=CARTESIAN_POINT('Ctrl Pts',(4.14597631470871,-3.01724243684715,43.8396390879149));
#53977=CARTESIAN_POINT('Ctrl Pts',(5.08477284786202,-0.661782902832914,
43.978812545337));
#53978=CARTESIAN_POINT('Ctrl Pts',(4.78016421891062,1.85550574374848,44.1179860027588));
#53979=CARTESIAN_POINT('Ctrl Pts',(3.30663791293829,3.91905820798263,44.2571594601809));
#53980=CARTESIAN_POINT('Ctrl Pts',(1.0245227529157,5.02426359316417,44.3963329176028));
#53981=CARTESIAN_POINT('Ctrl Pts',(-1.50812412558962,4.90086044962019,44.5355063750247));
#53982=CARTESIAN_POINT('Ctrl Pts',(-3.67198180171369,3.57902517073021,44.6746798324467));
#53983=CARTESIAN_POINT('Ctrl Pts',(-4.74638679107565,1.71438527582161,44.7927975194353));
#53984=CARTESIAN_POINT('Ctrl Pts',(-4.91772953076433,0.447446119031382,
44.86452405395));
#53985=CARTESIAN_POINT('Ctrl Pts',(-4.91784060085492,-3.50728131557135E-5,
44.8898594359907));
#53986=CARTESIAN_POINT('Ctrl Pts',(-4.91788690158348,-6.94023299559199E-5,
43.4851405640093));
#53987=CARTESIAN_POINT('Ctrl Pts',(-4.91805177856022,-0.331883298593633,
43.5039276289972));
#53988=CARTESIAN_POINT('Ctrl Pts',(-4.80327533823206,-1.48293720817835,
43.5691058464591));
#53989=CARTESIAN_POINT('Ctrl Pts',(-3.91508206282783,-3.3113447477378,43.680675216395));
#53990=CARTESIAN_POINT('Ctrl Pts',(-1.84976046732335,-4.78239038667639,
43.8198486738169));
#53991=CARTESIAN_POINT('Ctrl Pts',(0.667892389093657,-5.08397397255705,
43.9590221312389));
#53992=CARTESIAN_POINT('Ctrl Pts',(3.02222214943982,-4.14234774934242,44.0981955886608));
#53993=CARTESIAN_POINT('Ctrl Pts',(4.63751267753772,-2.18777232881387,44.2373690460827));
#53994=CARTESIAN_POINT('Ctrl Pts',(5.1187688298422,0.301790098715543,44.3765425035047));
#53995=CARTESIAN_POINT('Ctrl Pts',(4.34830661102557,2.71755427058194,44.5157159609267));
#53996=CARTESIAN_POINT('Ctrl Pts',(2.51453103518521,4.46878118396249,44.6548894183486));
#53997=CARTESIAN_POINT('Ctrl Pts',(0.0658644970599633,5.12723448508783,
44.7940628757706));
#53998=CARTESIAN_POINT('Ctrl Pts',(-2.3989082188817,4.5318992656974,44.9332363331925));
#53999=CARTESIAN_POINT('Ctrl Pts',(-4.27706380323859,2.82835585103309,45.0724097906145));
#54000=CARTESIAN_POINT('Ctrl Pts',(-4.87886413646883,1.09643166737844,45.1730445342201));
#54001=CARTESIAN_POINT('Ctrl Pts',(-4.91854807894143,0.138762230195914,
45.2272881253516));
#54002=CARTESIAN_POINT('Ctrl Pts',(-4.9184091500483,0.000116117112846665,
45.2351405640092));
#54003=CARTESIAN_POINT('Origin',(0.,0.,-3.23514056400933));
#54004=CARTESIAN_POINT('',(-4.91789641267672,7.41105149974438E-5,41.3898594359907));
#54005=CARTESIAN_POINT('',(-4.91866999096577,1.81579422332736E-5,41.7351405640092));
#54006=CARTESIAN_POINT('',(-4.91825,1.47989506776076E-12,-3.23514056400933));
#54007=CARTESIAN_POINT('Ctrl Pts',(-4.91789641267672,7.41105149971999E-5,
41.3898594359907));
#54008=CARTESIAN_POINT('Ctrl Pts',(-4.9176339004058,-0.493458636834103,
41.4178030612411));
#54009=CARTESIAN_POINT('Ctrl Pts',(-4.72122846096945,-1.80654367572432,
41.4921378389654));
#54010=CARTESIAN_POINT('Ctrl Pts',(-3.56999746819571,-3.68075937843173,
41.6128637691637));
#54011=CARTESIAN_POINT('Ctrl Pts',(-1.36986311464964,-4.94128997043882,
41.7520372265857));
#54012=CARTESIAN_POINT('Ctrl Pts',(1.16525077861143,-4.99350199236792,41.8912106840076));
#54013=CARTESIAN_POINT('Ctrl Pts',(3.4154200191569,-3.82462777503633,42.0303841414296));
#54014=CARTESIAN_POINT('Ctrl Pts',(4.83039936830708,-1.72049802891365,42.1695575988515));
#54015=CARTESIAN_POINT('Ctrl Pts',(5.06417678586922,0.804353781802734,42.3087310562735));
#54016=CARTESIAN_POINT('Ctrl Pts',(4.05958550029279,3.13251290350884,42.4479045136954));
#54017=CARTESIAN_POINT('Ctrl Pts',(2.06228328777852,4.69466283835021,42.5870779711175));
#54018=CARTESIAN_POINT('Ctrl Pts',(-0.439319463318189,5.10880318019658,
42.7262514285393));
#54019=CARTESIAN_POINT('Ctrl Pts',(-2.83349320925637,4.2736621015161,42.8654248859613));
#54020=CARTESIAN_POINT('Ctrl Pts',(-4.51883670867307,2.41107924578458,43.0032942217785));
#54021=CARTESIAN_POINT('Ctrl Pts',(-4.91844625336389,0.795931806725344,
43.0947724051215));
#54022=CARTESIAN_POINT('Ctrl Pts',(-4.91866555055193,-2.44668497561802E-5,
43.1398594359907));
#54023=CARTESIAN_POINT('Ctrl Pts',(-4.91866999096577,1.81579422333582E-5,
41.7351405640093));
#54024=CARTESIAN_POINT('Ctrl Pts',(-4.91850286965307,-0.801930133740765,
41.7805671326427));
#54025=CARTESIAN_POINT('Ctrl Pts',(-4.5141559940908,-2.42301760416976,41.8723848537502));
#54026=CARTESIAN_POINT('Ctrl Pts',(-2.81784457349484,-4.28399621342882,
42.0105937273315));
#54027=CARTESIAN_POINT('Ctrl Pts',(-0.420632547238203,-5.1103757060759,
42.1497671847535));
#54028=CARTESIAN_POINT('Ctrl Pts',(2.07943887829429,-4.68708924050791,42.2889406421754));
#54029=CARTESIAN_POINT('Ctrl Pts',(4.07101462212891,-3.11764519204149,42.4281140995974));
#54030=CARTESIAN_POINT('Ctrl Pts',(5.06708461819206,-0.785827633217498,
42.5672875570193));
#54031=CARTESIAN_POINT('Ctrl Pts',(4.82407484420597,1.73815232202072,42.7064610144413));
#54032=CARTESIAN_POINT('Ctrl Pts',(3.40140970642374,3.83709311928876,42.8456344718632));
#54033=CARTESIAN_POINT('Ctrl Pts',(1.14698068971451,4.99773017423599,42.9848079292852));
#54034=CARTESIAN_POINT('Ctrl Pts',(-1.38792530268207,4.93624705127506,43.1239813867072));
#54035=CARTESIAN_POINT('Ctrl Pts',(-3.58343491738278,3.66767852870569,43.2631548441291));
#54036=CARTESIAN_POINT('Ctrl Pts',(-4.7245853073055,1.79454803810771,43.3835412365631));
#54037=CARTESIAN_POINT('Ctrl Pts',(-4.9176446456221,0.48746922211443,43.4575364765232));
#54038=CARTESIAN_POINT('Ctrl Pts',(-4.91788690158348,-6.94023299559199E-5,
43.4851405640093));
#54039=CARTESIAN_POINT('Origin',(0.,0.,-3.23514056400933));
#54040=CARTESIAN_POINT('',(-4.9183905850055,-0.000118608231170829,39.6398594359908));
#54041=CARTESIAN_POINT('',(-4.9178455584335,4.04671957601743E-5,39.9851405640093));
#54042=CARTESIAN_POINT('',(-4.91825,1.47989506776076E-12,-3.23514056400933));
#54043=CARTESIAN_POINT('Ctrl Pts',(-4.9183905850055,-0.000118608231171394,
39.6398594359908));
#54044=CARTESIAN_POINT('Ctrl Pts',(-4.91853719113951,-0.144761324033651,
39.6480514124127));
#54045=CARTESIAN_POINT('Ctrl Pts',(-4.87687342658784,-1.10843139516826,
39.7026345413085));
#54046=CARTESIAN_POINT('Ctrl Pts',(-4.26669129572166,-2.84397906318768,
39.8036088226782));
#54047=CARTESIAN_POINT('Ctrl Pts',(-2.3823180541456,-4.54064226885678,39.9427822801004));
#54048=CARTESIAN_POINT('Ctrl Pts',(0.0846154423188459,-5.12695930857248,
40.0819557375222));
#54049=CARTESIAN_POINT('Ctrl Pts',(2.53085749770598,-4.45955511807427,40.2211291949443));
#54050=CARTESIAN_POINT('Ctrl Pts',(4.35821619854518,-2.70163341176691,40.3603026523661));
#54051=CARTESIAN_POINT('Ctrl Pts',(5.11983830092096,-0.283067654915984,
40.4994761097881));
#54052=CARTESIAN_POINT('Ctrl Pts',(4.62948050901625,2.20471806394278,40.6386495672101));
#54053=CARTESIAN_POINT('Ctrl Pts',(3.00705248801675,4.15337294968188,40.7778230246319));
#54054=CARTESIAN_POINT('Ctrl Pts',(0.649294748622445,5.08638259023525,40.916996482054));
#54055=CARTESIAN_POINT('Ctrl Pts',(-1.86723831197507,4.77559343025863,41.0561699394759));
#54056=CARTESIAN_POINT('Ctrl Pts',(-3.92716616611468,3.29700431127425,41.1953433968979));
#54057=CARTESIAN_POINT('Ctrl Pts',(-4.80598396548452,1.47093491011835,41.3065732290695));
#54058=CARTESIAN_POINT('Ctrl Pts',(-4.91806971525364,0.325889344254859,
41.3714119087671));
#54059=CARTESIAN_POINT('Ctrl Pts',(-4.91789641267672,7.41105149971999E-5,
41.3898594359907));
#54060=CARTESIAN_POINT('Ctrl Pts',(-4.9178455584335,4.04671957601049E-5,
39.9851405640093));
#54061=CARTESIAN_POINT('Ctrl Pts',(-4.91771552974485,-0.453436438311404,
40.0108154838143));
#54062=CARTESIAN_POINT('Ctrl Pts',(-4.74319322071268,-1.72638364779156,
40.0828815560932));
#54063=CARTESIAN_POINT('Ctrl Pts',(-3.65886799445027,-3.59243045809301,
40.2013387808461));
#54064=CARTESIAN_POINT('Ctrl Pts',(-1.49019055396033,-4.90634321159193,
40.3405122382681));
#54065=CARTESIAN_POINT('Ctrl Pts',(1.04289070214805,-5.02048310229404,40.4796856956901));
#54066=CARTESIAN_POINT('Ctrl Pts',(3.32094863246379,-3.90693892677934,40.618859153112));
#54067=CARTESIAN_POINT('Ctrl Pts',(4.7869182362722,-1.83801126119823,40.758032610534));
#54068=CARTESIAN_POINT('Ctrl Pts',(5.0823185691137,0.680374572635465,40.8972060679559));
#54069=CARTESIAN_POINT('Ctrl Pts',(4.13491389701701,3.03238497907216,41.0363795253779));
#54070=CARTESIAN_POINT('Ctrl Pts',(2.17637786502656,4.64287098524924,41.1755529827997));
#54071=CARTESIAN_POINT('Ctrl Pts',(-0.314358828238725,5.11801232161034,
41.3147264402218));
#54072=CARTESIAN_POINT('Ctrl Pts',(-2.72822377098922,4.34162027962559,41.4538998976437));
#54073=CARTESIAN_POINT('Ctrl Pts',(-4.47494238848132,2.50354992297337,41.5930733550657));
#54074=CARTESIAN_POINT('Ctrl Pts',(-4.91442322697852,0.853050173826952,
41.6868202438542));
#54075=CARTESIAN_POINT('Ctrl Pts',(-4.91867353960531,0.0170466588037495,
41.7341759801687));
#54076=CARTESIAN_POINT('Ctrl Pts',(-4.91866999096577,1.81579422333582E-5,
41.7351405640093));
#54077=CARTESIAN_POINT('Origin',(0.,0.,-3.23514056400933));
#54078=CARTESIAN_POINT('',(-4.91820219920178,0.000128750537505862,37.8898594359907));
#54079=CARTESIAN_POINT('',(-4.91850879678059,-9.71121811843556E-5,38.2351405640093));
#54080=CARTESIAN_POINT('',(-4.91825,1.47989506776076E-12,-3.23514056400933));
#54081=CARTESIAN_POINT('Ctrl Pts',(-4.91820219920178,0.000128750537505828,
37.8898594359907));
#54082=CARTESIAN_POINT('Ctrl Pts',(-4.91757825260023,-0.614945723327355,
37.9246909160581));
#54083=CARTESIAN_POINT('Ctrl Pts',(-4.64776325516924,-2.04975402890738,
38.0059135485996));
#54084=CARTESIAN_POINT('Ctrl Pts',(-3.28735082876793,-3.93525044354685,
38.1335273336149));
#54085=CARTESIAN_POINT('Ctrl Pts',(-0.999835326585605,-5.02923461816492,
38.2727007910369));
#54086=CARTESIAN_POINT('Ctrl Pts',(1.53217495314691,-4.89339467423037,38.4118742484588));
#54087=CARTESIAN_POINT('Ctrl Pts',(3.68951476027582,-3.56094823867799,38.5510477058808));
#54088=CARTESIAN_POINT('Ctrl Pts',(4.94463890588947,-1.35772516187962,38.6902211633027));
#54089=CARTESIAN_POINT('Ctrl Pts',(4.99062554934078,1.17750929979514,38.8293946207247));
#54090=CARTESIAN_POINT('Ctrl Pts',(3.81622934465927,3.42480147071306,38.9685680781466));
#54091=CARTESIAN_POINT('Ctrl Pts',(1.70863132174512,4.83460965654813,39.1077415355686));
#54092=CARTESIAN_POINT('Ctrl Pts',(-0.81678693997971,5.06218634776669,39.2469149929905));
#54093=CARTESIAN_POINT('Ctrl Pts',(-3.14247216978798,4.05188106771966,39.3860884504125));
#54094=CARTESIAN_POINT('Ctrl Pts',(-4.60805110144555,2.16853876589775,39.5170699314125));
#54095=CARTESIAN_POINT('Ctrl Pts',(-4.91770696078166,0.674350198934236,
39.6016602599387));
#54096=CARTESIAN_POINT('Ctrl Pts',(-4.9183905850055,-0.000118608231171394,
39.6398594359908));
#54097=CARTESIAN_POINT('Ctrl Pts',(-4.91850879678059,-9.71121811845985E-5,
38.2351405640093));
#54098=CARTESIAN_POINT('Ctrl Pts',(-4.91860204053572,-0.10467486996608,
38.2410638349858));
#54099=CARTESIAN_POINT('Ctrl Pts',(-4.8897482500804,-1.02825589750399,38.2933782584363));
#54100=CARTESIAN_POINT('Ctrl Pts',(-4.33490776837895,-2.73887682028504,
38.3920838343608));
#54101=CARTESIAN_POINT('Ctrl Pts',(-2.4925537144267,-4.48107660922512,38.5312572917828));
#54102=CARTESIAN_POINT('Ctrl Pts',(-0.0406829233315988,-5.12749612352813,
38.6704307492046));
#54103=CARTESIAN_POINT('Ctrl Pts',(2.42113626829065,-4.52006313754736,38.8096042066267));
#54104=CARTESIAN_POINT('Ctrl Pts',(4.29090279124404,-2.80731630443399,38.9487776640485));
#54105=CARTESIAN_POINT('Ctrl Pts',(5.11139320288289,-0.408082249760327,
39.0879511214706));
#54106=CARTESIAN_POINT('Ctrl Pts',(4.6819688426782,2.09094221661848,39.2271245788925));
#54107=CARTESIAN_POINT('Ctrl Pts',(3.10763901629375,4.0786580319335,39.3662980363144));
#54108=CARTESIAN_POINT('Ctrl Pts',(0.773382540198208,5.06899901790909,39.5054714937364));
#54109=CARTESIAN_POINT('Ctrl Pts',(-1.74999307091798,4.81979209601264,39.6446449511584));
#54110=CARTESIAN_POINT('Ctrl Pts',(-3.84543404598807,3.39197709234639,39.7838184085803));
#54111=CARTESIAN_POINT('Ctrl Pts',(-4.7874375644823,1.55112965427828,39.8973169461972));
#54112=CARTESIAN_POINT('Ctrl Pts',(-4.91795047422635,0.365935790564356,
39.9644243313403));
#54113=CARTESIAN_POINT('Ctrl Pts',(-4.9178455584335,4.04671957601049E-5,
39.9851405640093));
#54114=CARTESIAN_POINT('Origin',(0.,0.,-3.23514056400933));
#54115=CARTESIAN_POINT('',(-4.91802291969686,-0.000111909727839232,36.1398594359907));
#54116=CARTESIAN_POINT('',(-4.91808249072253,0.000120892635755293,36.4851405640093));
#54117=CARTESIAN_POINT('',(-4.91825,1.47989506776076E-12,-3.23514056400933));
#54118=CARTESIAN_POINT('Ctrl Pts',(-4.91802291969686,-0.000111909727839483,
36.1398594359907));
#54119=CARTESIAN_POINT('Ctrl Pts',(-4.91824438810614,-0.266428183199001,
36.1549392672297));
#54120=CARTESIAN_POINT('Ctrl Pts',(-4.83158217849615,-1.35188938642552,
36.2164102509426));
#54121=CARTESIAN_POINT('Ctrl Pts',(-4.04415220241896,-3.15241248704969,
36.3242723871296));
#54122=CARTESIAN_POINT('Ctrl Pts',(-2.0392020752804,-4.70473446870373,36.4634458445515));
#54123=CARTESIAN_POINT('Ctrl Pts',(0.464404425081292,-5.10658399077132,
36.6026193019735));
#54124=CARTESIAN_POINT('Ctrl Pts',(2.85444776800653,-4.25969476190013,36.7417927593954));
#54125=CARTESIAN_POINT('Ctrl Pts',(4.54647859476008,-2.3711608786047,36.8809662168174));
#54126=CARTESIAN_POINT('Ctrl Pts',(5.12673606933716,0.0972049391453199,
37.0201396742393));
#54127=CARTESIAN_POINT('Ctrl Pts',(4.45332690351699,2.5418007426328,37.1593131316613));
#54128=CARTESIAN_POINT('Ctrl Pts',(2.69092323862078,4.3648371846711,37.2984865890832));
#54129=CARTESIAN_POINT('Ctrl Pts',(0.270494535863632,5.12051796509932,37.4376600465052));
#54130=CARTESIAN_POINT('Ctrl Pts',(-2.21607956065588,4.62405264953592,37.576833503927));
#54131=CARTESIAN_POINT('Ctrl Pts',(-4.16074453993469,2.9968444067453,37.7160069613491));
#54132=CARTESIAN_POINT('Ctrl Pts',(-4.85590344258394,1.22745946040092,37.8203489387036));
#54133=CARTESIAN_POINT('Ctrl Pts',(-4.91840927103161,0.204256149366557,
37.8782997635842));
#54134=CARTESIAN_POINT('Ctrl Pts',(-4.91820219920178,0.000128750537505828,
37.8898594359907));
#54135=CARTESIAN_POINT('Ctrl Pts',(-4.91808249072253,0.000120892635755154,
36.4851405640093));
#54136=CARTESIAN_POINT('Ctrl Pts',(-4.91755648739828,-0.574931667043208,
36.5177033386313));
#54137=CARTESIAN_POINT('Ctrl Pts',(-4.67310068886124,-1.9696788349413,36.5966572657274));
#54138=CARTESIAN_POINT('Ctrl Pts',(-3.38252402474393,-3.85375178482954,
36.7220023452973));
#54139=CARTESIAN_POINT('Ctrl Pts',(-1.12242209698828,-5.0033029323877,36.8611758027193));
#54140=CARTESIAN_POINT('Ctrl Pts',(1.41215136985344,-4.92937116736687,37.0003492601412));
#54141=CARTESIAN_POINT('Ctrl Pts',(3.60140433654983,-3.6500353973252,37.1395227175632));
#54142=CARTESIAN_POINT('Ctrl Pts',(4.90998772824735,-1.47813805360231,37.2786961749851));
#54143=CARTESIAN_POINT('Ctrl Pts',(5.01790704510018,1.05521584700991,37.4178696324071));
#54144=CARTESIAN_POINT('Ctrl Pts',(3.89877223200052,3.33053249196408,37.5570430898291));
#54145=CARTESIAN_POINT('Ctrl Pts',(1.82625097191763,4.79141722088745,37.696216547251));
#54146=CARTESIAN_POINT('Ctrl Pts',(-0.692852653537991,5.08063251943419,
37.835390004673));
#54147=CARTESIAN_POINT('Ctrl Pts',(-3.04252952350951,4.12745511127861,37.9745634620949));
#54148=CARTESIAN_POINT('Ctrl Pts',(-4.57986334488089,2.24849431797034,38.1078136485404));
#54149=CARTESIAN_POINT('Ctrl Pts',(-4.91787175396287,0.714379791895642,
38.1946726825118));
#54150=CARTESIAN_POINT('Ctrl Pts',(-4.91850879678059,-9.71121811845985E-5,
38.2351405640093));
#54151=CARTESIAN_POINT('Origin',(0.,0.,-3.23514056400933));
#54152=CARTESIAN_POINT('',(-4.91856546994177,8.07004106879134E-5,34.3898594359908));
#54153=CARTESIAN_POINT('',(-4.91813464082657,-0.000125816539483792,34.7351405640093));
#54154=CARTESIAN_POINT('',(-4.91825,1.47989506776076E-12,-3.23514056400933));
#54155=CARTESIAN_POINT('Ctrl Pts',(-4.91856546994177,8.07004106878097E-5,
34.3898594359908));
#54156=CARTESIAN_POINT('Ctrl Pts',(-4.91799365147455,-0.736466546762098,
34.4315787708752));
#54157=CARTESIAN_POINT('Ctrl Pts',(-4.56381414385588,-2.29257248088249,
34.5196892582337));
#54158=CARTESIAN_POINT('Ctrl Pts',(-2.98661825458746,-4.16809104101649,
34.6541908980661));
#54159=CARTESIAN_POINT('Ctrl Pts',(-0.624306769841251,-5.08951005323373,
34.7933643554881));
#54160=CARTESIAN_POINT('Ctrl Pts',(1.89066959956818,-4.76636549061291,34.93253781291));
#54161=CARTESIAN_POINT('Ctrl Pts',(3.94331099153097,-3.27767752362979,35.071711270332));
#54162=CARTESIAN_POINT('Ctrl Pts',(5.03167464890124,-0.987482532727304,
35.2108847277539));
#54163=CARTESIAN_POINT('Ctrl Pts',(4.88961751469062,1.54418654471136,35.3500581851759));
#54164=CARTESIAN_POINT('Ctrl Pts',(3.55187753674385,3.69824789445101,35.4892316425978));
#54165=CARTESIAN_POINT('Ctrl Pts',(1.34557902206557,4.94795802530842,35.6284051000198));
#54166=CARTESIAN_POINT('Ctrl Pts',(-1.18976072063133,4.98771901298376,35.7675785574417));
#54167=CARTESIAN_POINT('Ctrl Pts',(-3.43416227081397,3.807807902528,35.9067520148637));
#54168=CARTESIAN_POINT('Ctrl Pts',(-4.68659538479648,1.92549284030058,36.0308456410467));
#54169=CARTESIAN_POINT('Ctrl Pts',(-4.91756306915899,0.552859423746898,
36.1085481147557));
#54170=CARTESIAN_POINT('Ctrl Pts',(-4.91802291969686,-0.000111909727839483,
36.1398594359907));
#54171=CARTESIAN_POINT('Ctrl Pts',(-4.91813464082657,-0.000125816539484104,
34.7351405640093));
#54172=CARTESIAN_POINT('Ctrl Pts',(-4.91835367199364,-0.226361035175407,
34.7479516898028));
#54173=CARTESIAN_POINT('Ctrl Pts',(-4.84753997352677,-1.27169443624834,
34.8071539680704));
#54174=CARTESIAN_POINT('Ctrl Pts',(-4.11997143710345,-3.05265572158056,
34.912747398812));
#54175=CARTESIAN_POINT('Ctrl Pts',(-2.15354963574969,-4.65350357939147,
35.0519208562339));
#54176=CARTESIAN_POINT('Ctrl Pts',(0.339490524783248,-5.11640672548902,
35.1910943136559));
#54177=CARTESIAN_POINT('Ctrl Pts',(2.74951335423154,-4.32816911776206,35.3302677710778));
#54178=CARTESIAN_POINT('Ctrl Pts',(4.48718380920458,-2.4815424758523,35.4694412284998));
#54179=CARTESIAN_POINT('Ctrl Pts',(5.12758056511281,-0.0280917305306554,
35.6086146859217));
#54180=CARTESIAN_POINT('Ctrl Pts',(4.51410417181047,2.43222842740771,35.7477881433437));
#54181=CARTESIAN_POINT('Ctrl Pts',(2.79677110733593,4.29778349503762,35.8869616007656));
#54182=CARTESIAN_POINT('Ctrl Pts',(0.395529491558261,5.1123798781345,36.0261350581876));
#54183=CARTESIAN_POINT('Ctrl Pts',(-2.10243294662056,4.67682021270983,36.1653085156095));
#54184=CARTESIAN_POINT('Ctrl Pts',(-4.08627684754628,3.09761410157141,36.3044819730315));
#54185=CARTESIAN_POINT('Ctrl Pts',(-4.84051203245055,1.30765216918706,36.4110926558314));
#54186=CARTESIAN_POINT('Ctrl Pts',(-4.91830586765535,0.24432748044256,36.4713121861573));
#54187=CARTESIAN_POINT('Ctrl Pts',(-4.91808249072253,0.000120892635755154,
36.4851405640093));
#54188=CARTESIAN_POINT('Origin',(0.,0.,-3.23514056400933));
#54189=CARTESIAN_POINT('',(-4.91783086310991,-2.02920551994784E-5,32.6398594359908));
#54190=CARTESIAN_POINT('',(-4.91845769753215,0.000108139753099631,32.9851405640093));
#54191=CARTESIAN_POINT('',(-4.91825,1.47989506776076E-12,-3.23514056400933));
#54192=CARTESIAN_POINT('Ctrl Pts',(-4.91783086310991,-2.02920551998012E-5,
32.6398594359908));
#54193=CARTESIAN_POINT('Ctrl Pts',(-4.91788645067138,-0.388022414657125,
32.6618271220468));
#54194=CARTESIAN_POINT('Ctrl Pts',(-4.77675395009793,-1.59536399838191,
32.7301859605768));
#54195=CARTESIAN_POINT('Ctrl Pts',(-3.79936349942357,-3.44350236301427,
32.8449359515807));
#54196=CARTESIAN_POINT('Ctrl Pts',(-1.68486707003129,-4.84294275014284,
32.9841094090027));
#54197=CARTESIAN_POINT('Ctrl Pts',(0.841638405786343,-5.05811390922963,
33.1232828664246));
#54198=CARTESIAN_POINT('Ctrl Pts',(3.16233379535394,-4.03639895099572,33.2624563238466));
#54199=CARTESIAN_POINT('Ctrl Pts',(4.70972774489857,-2.02764298972218,33.4016297812685));
#54200=CARTESIAN_POINT('Ctrl Pts',(5.10542820383288,0.476942743256107,33.5408032386905));
#54201=CARTESIAN_POINT('Ctrl Pts',(4.25267254224057,2.86489926058667,33.6799766961124));
#54202=CARTESIAN_POINT('Ctrl Pts',(2.35998940503126,4.55228750552699,33.8191501535344));
#54203=CARTESIAN_POINT('Ctrl Pts',(-0.109793849828778,5.12648191602942,
33.9583236109563));
#54204=CARTESIAN_POINT('Ctrl Pts',(-2.55272866057358,4.44707183552539,34.0974970683783));
#54205=CARTESIAN_POINT('Ctrl Pts',(-4.37143185095318,2.68019683928419,34.2366705258002));
#54206=CARTESIAN_POINT('Ctrl Pts',(-4.89642245145228,0.984033726224288,
34.3341246483377));
#54207=CARTESIAN_POINT('Ctrl Pts',(-4.9186295033589,0.0825607877462077,
34.3851876184012));
#54208=CARTESIAN_POINT('Ctrl Pts',(-4.91856546994177,8.07004106878097E-5,
34.3898594359908));
#54209=CARTESIAN_POINT('Ctrl Pts',(-4.91845769753216,0.000108139753099545,
32.9851405640093));
#54210=CARTESIAN_POINT('Ctrl Pts',(-4.9177893045039,-0.696429685266491,
33.0245911934484));
#54211=CARTESIAN_POINT('Ctrl Pts',(-4.5926463194941,-2.21265079041603,33.1104329753614));
#54212=CARTESIAN_POINT('Ctrl Pts',(-3.0875705083242,-4.0938710230262,33.2426659097486));
#54213=CARTESIAN_POINT('Ctrl Pts',(-0.748478438807404,-5.07273610822475,
33.3818393671704));
#54214=CARTESIAN_POINT('Ctrl Pts',(1.77364284015155,-4.81113943599913,33.5210128245925));
#54215=CARTESIAN_POINT('Ctrl Pts',(3.86204628565767,-3.37305056061788,33.6601862820144));
#54216=CARTESIAN_POINT('Ctrl Pts',(5.00604406515782,-1.11013261133297,33.7993597394364));
#54217=CARTESIAN_POINT('Ctrl Pts',(4.92588862905106,1.42425166709831,33.9385331968583));
#54218=CARTESIAN_POINT('Ctrl Pts',(3.64118079059058,3.61035649864124,34.0777066542803));
#54219=CARTESIAN_POINT('Ctrl Pts',(1.4660766401138,4.91360263781672,34.2168801117022));
#54220=CARTESIAN_POINT('Ctrl Pts',(-1.06753462895041,5.01530073006979,34.3560535691242));
#54221=CARTESIAN_POINT('Ctrl Pts',(-3.34009626844846,3.89058202773615,34.4952270265461));
#54222=CARTESIAN_POINT('Ctrl Pts',(-4.66187956111484,2.00558801068489,34.6215893581745));
#54223=CARTESIAN_POINT('Ctrl Pts',(-4.9175605248158,0.592873175137666,34.7015605373289));
#54224=CARTESIAN_POINT('Ctrl Pts',(-4.91813464082657,-0.000125816539484104,
34.7351405640093));
#54225=CARTESIAN_POINT('Origin',(0.,0.,-3.23514056400933));
#54226=CARTESIAN_POINT('',(-4.91864785516252,-4.10080702071888E-5,30.8898594359907));
#54227=CARTESIAN_POINT('',(-4.91786460607134,-5.61405901616796E-5,31.2351405640093));
#54228=CARTESIAN_POINT('',(-4.91825,1.47989506776076E-12,-3.23514056400933));
#54229=CARTESIAN_POINT('Ctrl Pts',(-4.91864785516252,-4.10080702073533E-5,
30.8898594359907));
#54230=CARTESIAN_POINT('Ctrl Pts',(-4.9186650757863,-0.0391628390810305,
30.8920754732183));
#54231=CARTESIAN_POINT('Ctrl Pts',(-4.90864151106169,-0.897263340327606,
30.9406826629198));
#54232=CARTESIAN_POINT('Ctrl Pts',(-4.44078995181737,-2.56364118563321,
31.0356810050954));
#54233=CARTESIAN_POINT('Ctrl Pts',(-2.66945427843709,-4.37800015762571,
31.1748544625173));
#54234=CARTESIAN_POINT('Ctrl Pts',(-0.245343480361355,-5.12178465981157,
31.3140279199393));
#54235=CARTESIAN_POINT('Ctrl Pts',(2.23876239696327,-4.61311331475612,31.4532013773612));
#54236=CARTESIAN_POINT('Ctrl Pts',(4.17541240862802,-2.97637409320671,31.5923748347831));
#54237=CARTESIAN_POINT('Ctrl Pts',(5.09102775500046,-0.611807095947689,
31.7315482922051));
#54238=CARTESIAN_POINT('Ctrl Pts',(4.7617083952635,1.90236817764437,31.8707217496271));
#54239=CARTESIAN_POINT('Ctrl Pts',(3.26798445418964,3.95134776146213,32.009895207049));
#54240=CARTESIAN_POINT('Ctrl Pts',(0.975123784377534,5.03408433878279,32.149068664471));
#54241=CARTESIAN_POINT('Ctrl Pts',(-1.5561888248749,4.8858108708966,32.2882421218929));
#54242=CARTESIAN_POINT('Ctrl Pts',(-3.70695872829678,3.5427854170894,32.4274155793149));
#54243=CARTESIAN_POINT('Ctrl Pts',(-4.75484390387066,1.6821589453014,32.5446213506808));
#54244=CARTESIAN_POINT('Ctrl Pts',(-4.91776906138271,0.431356812812067,
32.6154359695728));
#54245=CARTESIAN_POINT('Ctrl Pts',(-4.91783086310991,-2.02920551998012E-5,
32.6398594359908));
#54246=CARTESIAN_POINT('Ctrl Pts',(-4.91786460607134,-5.61405901617837E-5,
31.2351405640093));
#54247=CARTESIAN_POINT('Ctrl Pts',(-4.91800366546841,-0.347980646584003,
31.2548395446199));
#54248=CARTESIAN_POINT('Ctrl Pts',(-4.79588397241455,-1.51517210046812,
31.3209296777045));
#54249=CARTESIAN_POINT('Ctrl Pts',(-3.882368363373,-3.34963990424751,31.4334109632632));
#54250=CARTESIAN_POINT('Ctrl Pts',(-1.80269742761279,-4.80032848683557,
31.5725844206851));
#54251=CARTESIAN_POINT('Ctrl Pts',(0.717796206480772,-5.07716852221872,
31.7117578781071));
#54252=CARTESIAN_POINT('Ctrl Pts',(3.06276351222464,-4.1124629196179,31.850931335529));
#54253=CARTESIAN_POINT('Ctrl Pts',(4.65877780170794,-2.14211600791371,31.990104792951));
#54254=CARTESIAN_POINT('Ctrl Pts',(5.11555764728126,0.352053340261175,32.1292782503729));
#54255=CARTESIAN_POINT('Ctrl Pts',(4.32140436840864,2.760133308691,32.2684517077949));
#54256=CARTESIAN_POINT('Ctrl Pts',(2.47051627364734,4.49326395159359,32.4076251652168));
#54257=CARTESIAN_POINT('Ctrl Pts',(0.0155003683372346,5.12763408753279,
32.5467986226388));
#54258=CARTESIAN_POINT('Ctrl Pts',(-2.44330592025679,4.50811798615397,32.6859720800608));
#54259=CARTESIAN_POINT('Ctrl Pts',(-4.30463828331925,2.78620904578768,32.8251455374827));
#54260=CARTESIAN_POINT('Ctrl Pts',(-4.88409932027737,1.06420425567212,32.9248683654655));
#54261=CARTESIAN_POINT('Ctrl Pts',(-4.91857528747368,0.122649576681999,
32.9782000409744));
#54262=CARTESIAN_POINT('Ctrl Pts',(-4.91845769753216,0.000108139753099545,
32.9851405640093));
#54263=CARTESIAN_POINT('Origin',(0.,0.,-3.23514056400933));
#54264=CARTESIAN_POINT('',(-4.91792510490206,8.60427107810521E-5,29.1398594359908));
#54265=CARTESIAN_POINT('',(-4.91867551204664,9.95602900351817E-7,29.4851405640093));
#54266=CARTESIAN_POINT('',(-4.91825,1.47989506776076E-12,-3.23514056400933));
#54267=CARTESIAN_POINT('Ctrl Pts',(-4.91792510490206,8.60427107807205E-5,
29.1398594359908));
#54268=CARTESIAN_POINT('Ctrl Pts',(-4.91760801436112,-0.509544199604375,
29.1687149768638));
#54269=CARTESIAN_POINT('Ctrl Pts',(-4.71209097325018,-1.83875860727307,
29.2439616702109));
#54270=CARTESIAN_POINT('Ctrl Pts',(-3.5336719345399,-3.71564720928695,29.3655995160319));
#54271=CARTESIAN_POINT('Ctrl Pts',(-1.3212624743179,-4.95450673617428,29.5047729734539));
#54272=CARTESIAN_POINT('Ctrl Pts',(1.21424196580137,-4.98181573056689,29.6439464308758));
#54273=CARTESIAN_POINT('Ctrl Pts',(3.45282169099331,-3.79089618626559,29.7831198882978));
#54274=CARTESIAN_POINT('Ctrl Pts',(4.84706550524806,-1.67296966878402,29.9222933457197));
#54275=CARTESIAN_POINT('Ctrl Pts',(5.05603193335185,0.854056563561975,30.0614668031417));
#54276=CARTESIAN_POINT('Ctrl Pts',(4.02862136020189,3.17223603487539,30.2006402605636));
#54277=CARTESIAN_POINT('Ctrl Pts',(2.01607167753466,4.71469262156925,30.3398137179856));
#54278=CARTESIAN_POINT('Ctrl Pts',(-0.48947818547963,5.10424163130788,30.4789871754075));
#54279=CARTESIAN_POINT('Ctrl Pts',(-2.87533347790578,4.24562467908683,30.6181606328295));
#54280=CARTESIAN_POINT('Ctrl Pts',(-4.53127503174689,2.37900648499639,30.7551180530239));
#54281=CARTESIAN_POINT('Ctrl Pts',(-4.91830457435893,0.779824678331975,
30.8456843207443));
#54282=CARTESIAN_POINT('Ctrl Pts',(-4.91864785516252,-4.10080702073533E-5,
30.8898594359907));
#54283=CARTESIAN_POINT('Ctrl Pts',(-4.91867550406428,9.95584223391723E-7,
29.4851405640093));
#54284=CARTESIAN_POINT('Ctrl Pts',(-4.91866563344334,-0.818043332890193,
29.5314790482654));
#54285=CARTESIAN_POINT('Ctrl Pts',(-4.50145125695214,-2.45507147256078,
29.6242086849956));
#54286=CARTESIAN_POINT('Ctrl Pts',(-2.77563018347832,-4.31146711475466,
29.7633294741997));
#54287=CARTESIAN_POINT('Ctrl Pts',(-0.370416895766376,-5.11426074035902,
29.9025029316217));
#54288=CARTESIAN_POINT('Ctrl Pts',(2.1253763045803,-4.66643838071129,30.0416763890436));
#54289=CARTESIAN_POINT('Ctrl Pts',(4.10144051258044,-3.07750829711484,30.1808498464656));
#54290=CARTESIAN_POINT('Ctrl Pts',(5.07455877628885,-0.736019580606846,
30.3200233038876));
#54291=CARTESIAN_POINT('Ctrl Pts',(4.8067695763542,1.7854517178805,30.4591967613095));
#54292=CARTESIAN_POINT('Ctrl Pts',(3.36355675709311,3.87031749845671,30.5983702187315));
#54293=CARTESIAN_POINT('Ctrl Pts',(1.09783643160968,5.00875501162488,30.7375436761534));
#54294=CARTESIAN_POINT('Ctrl Pts',(-1.43634337614621,4.92237638776717,30.8767171335754));
#54295=CARTESIAN_POINT('Ctrl Pts',(-3.61928689038582,3.63230422763955,31.0158905909973));
#54296=CARTESIAN_POINT('Ctrl Pts',(-4.7334795615999,1.76232844516563,31.1353650678086));
#54297=CARTESIAN_POINT('Ctrl Pts',(-4.9176761802132,0.47138250352112,31.208448392146));
#54298=CARTESIAN_POINT('Ctrl Pts',(-4.91786460607134,-5.61405901617837E-5,
31.2351405640093));
#54299=CARTESIAN_POINT('Origin',(0.,0.,-3.23514056400933));
#54300=CARTESIAN_POINT('',(-4.91833988482916,-0.000123980294687707,27.3898594359908));
#54301=CARTESIAN_POINT('',(-4.91786234455194,5.45566455475988E-5,27.7351405640093));
#54302=CARTESIAN_POINT('',(-4.91825,1.47989506776076E-12,-3.23514056400933));
#54303=CARTESIAN_POINT('Ctrl Pts',(-4.91833988482916,-0.000123980294688027,
27.3898594359908));
#54304=CARTESIAN_POINT('Ctrl Pts',(-4.91850603363977,-0.160872832603585,
27.3989633280354));
#54305=CARTESIAN_POINT('Ctrl Pts',(-4.87141522988022,-1.14066063085594,
27.454458372554));
#54306=CARTESIAN_POINT('Ctrl Pts',(-4.23855121493717,-2.88575035704607,
27.5563445695465));
#54307=CARTESIAN_POINT('Ctrl Pts',(-2.33760383332739,-4.56382294170687,
27.6955180269685));
#54308=CARTESIAN_POINT('Ctrl Pts',(0.134969609127406,-5.12588087351325,
27.8346914843905));
#54309=CARTESIAN_POINT('Ctrl Pts',(2.57453825200954,-4.43448129027247,27.9738649418124));
#54310=CARTESIAN_POINT('Ctrl Pts',(4.38454206508205,-2.65869562085676,28.1130383992344));
#54311=CARTESIAN_POINT('Ctrl Pts',(5.12237168270734,-0.232765695571575,
28.2522118566563));
#54312=CARTESIAN_POINT('Ctrl Pts',(4.60760190542052,2.25008359978071,28.3913853140782));
#54313=CARTESIAN_POINT('Ctrl Pts',(2.96611198437499,4.18270859862171,28.5305587715002));
#54314=CARTESIAN_POINT('Ctrl Pts',(0.59930373287477,5.09251475801487,28.6697322289221));
#54315=CARTESIAN_POINT('Ctrl Pts',(-1.91405528449465,4.75702258694817,28.8089056863441));
#54316=CARTESIAN_POINT('Ctrl Pts',(-3.95936070487888,3.25827167889634,28.948079143766));
#54317=CARTESIAN_POINT('Ctrl Pts',(-4.81314243584705,1.43869944420298,29.058397060315));
#54318=CARTESIAN_POINT('Ctrl Pts',(-4.91811780191622,0.309790096730312,
29.1223238243899));
#54319=CARTESIAN_POINT('Ctrl Pts',(-4.91792510490206,8.60427107807205E-5,
29.1398594359908));
#54320=CARTESIAN_POINT('Ctrl Pts',(-4.91786234455194,5.455664554746E-5,
27.7351405640093));
#54321=CARTESIAN_POINT('Ctrl Pts',(-4.91768006061354,-0.469524247219173,
27.761727399437));
#54322=CARTESIAN_POINT('Ctrl Pts',(-4.73449557411608,-1.75860652475638,
27.8347053873387));
#54323=CARTESIAN_POINT('Ctrl Pts',(-3.62340576199759,-3.62819545793354,
27.9540745277144));
#54324=CARTESIAN_POINT('Ctrl Pts',(-1.44192736471906,-4.92074354868461,
28.0932479851363));
#54325=CARTESIAN_POINT('Ctrl Pts',(1.09215280697808,-5.0099973895459,28.2324214425583));
#54326=CARTESIAN_POINT('Ctrl Pts',(3.35916334181333,-3.8741312884393,28.3715948999802));
#54327=CARTESIAN_POINT('Ctrl Pts',(4.80474071443369,-1.79090431461596,28.5107683574022));
#54328=CARTESIAN_POINT('Ctrl Pts',(5.0753905955706,0.730261528111896,28.6499418148241));
#54329=CARTESIAN_POINT('Ctrl Pts',(4.10492960409817,3.07285283449196,28.7891152722461));
#54330=CARTESIAN_POINT('Ctrl Pts',(2.1306694631793,4.66402393172698,28.928288729668));
#54331=CARTESIAN_POINT('Ctrl Pts',(-0.36461403286742,5.11467772240667,29.06746218709));
#54332=CARTESIAN_POINT('Ctrl Pts',(-2.77073661962518,4.31461356111005,29.2066356445119));
#54333=CARTESIAN_POINT('Ctrl Pts',(-4.49931699972899,2.45947517429971,29.3458091019339));
#54334=CARTESIAN_POINT('Ctrl Pts',(-4.9184479131161,0.820834680615058,29.4386440750997));
#54335=CARTESIAN_POINT('Ctrl Pts',(-4.91867551528321,0.000930782942780498,
29.4850878957915));
#54336=CARTESIAN_POINT('Ctrl Pts',(-4.91867550406428,9.95584223391723E-7,
29.4851405640093));
#54337=CARTESIAN_POINT('Origin',(0.,0.,-3.23514056400933));
#54338=CARTESIAN_POINT('',(-4.91825297823531,0.000128629553767107,25.6398594359908));
#54339=CARTESIAN_POINT('',(-4.91846315696893,-0.00010709994074265,25.9851405640093));
#54340=CARTESIAN_POINT('',(-4.91825,1.47989506776076E-12,-3.23514056400933));
#54341=CARTESIAN_POINT('Ctrl Pts',(-4.91825297823531,0.000128629553767055,
25.6398594359908));
#54342=CARTESIAN_POINT('Ctrl Pts',(-4.91760082664806,-0.631030237377122,
25.6756028316809));
#54343=CARTESIAN_POINT('Ctrl Pts',(-4.63725911016808,-2.08192918048296,
25.757737379845));
#54344=CARTESIAN_POINT('Ctrl Pts',(-3.24853925631766,-3.96734977346339,
25.8862630804831));
#54345=CARTESIAN_POINT('Ctrl Pts',(-0.950388722330458,-5.03881263804321,
26.0254365379051));
#54346=CARTESIAN_POINT('Ctrl Pts',(1.58016516156227,-4.87810922253918,26.164609995327));
#54347=CARTESIAN_POINT('Ctrl Pts',(3.72431328503039,-3.52453714404928,26.303783452749));
#54348=CARTESIAN_POINT('Ctrl Pts',(4.95773628813266,-1.30909221301232,26.4429569101709));
#54349=CARTESIAN_POINT('Ctrl Pts',(4.97881902010364,1.22647164251408,26.5821303675929));
#54350=CARTESIAN_POINT('Ctrl Pts',(3.78240601411158,3.462120198556,26.7213038250149));
#54351=CARTESIAN_POINT('Ctrl Pts',(1.66106217957725,4.85115903268642,26.8604772824368));
#54352=CARTESIAN_POINT('Ctrl Pts',(-0.866469571400946,5.05391946974555,
26.9996507398587));
#54353=CARTESIAN_POINT('Ctrl Pts',(-3.182119145904,4.02081947693602,27.1388241972807));
#54354=CARTESIAN_POINT('Ctrl Pts',(-4.61905440019765,2.13638449485411,27.268893762658));
#54355=CARTESIAN_POINT('Ctrl Pts',(-4.9176593809369,0.658263035982611,27.3525721755614));
#54356=CARTESIAN_POINT('Ctrl Pts',(-4.91833988482916,-0.000123980294688027,
27.3898594359908));
#54357=CARTESIAN_POINT('Ctrl Pts',(-4.91846315696893,-0.000107099940742945,
25.9851405640093));
#54358=CARTESIAN_POINT('Ctrl Pts',(-4.91857823666502,-0.120788336375971,
25.9919757506085));
#54359=CARTESIAN_POINT('Ctrl Pts',(-4.88469360351122,-1.06048172000503,
26.0452020896818));
#54360=CARTESIAN_POINT('Ctrl Pts',(-4.30779673681465,-2.7813232230965,26.144819581229));
#54361=CARTESIAN_POINT('Ctrl Pts',(-2.44841924438686,-4.50534291711108,
26.2839930386509));
#54362=CARTESIAN_POINT('Ctrl Pts',(0.00968256052368256,-5.12764837377413,
26.4231664960729));
#54363=CARTESIAN_POINT('Ctrl Pts',(2.46541664005145,-4.49606409963251,26.5623399534948));
#54364=CARTESIAN_POINT('Ctrl Pts',(4.31826994816623,-2.76503458419805,26.7015134109168));
#54365=CARTESIAN_POINT('Ctrl Pts',(5.11515491599038,-0.357857209604937,
26.8406868683387));
#54366=CARTESIAN_POINT('Ctrl Pts',(4.66120524128334,2.13682879419003,26.9798603257607));
#54367=CARTESIAN_POINT('Ctrl Pts',(3.06742752861815,4.10898527056527,27.1190337831826));
#54368=CARTESIAN_POINT('Ctrl Pts',(0.723556284229189,5.07635084490811,27.2582072406046));
#54369=CARTESIAN_POINT('Ctrl Pts',(-1.79724982938647,4.80237073202571,27.3973806980266));
#54370=CARTESIAN_POINT('Ctrl Pts',(-3.87856537335147,3.35404267141695,27.5365541554485));
#54371=CARTESIAN_POINT('Ctrl Pts',(-4.79501921332612,1.51889555036017,27.6491407774428));
#54372=CARTESIAN_POINT('Ctrl Pts',(-4.91799812637216,0.349839980910759,
27.715336246963));
#54373=CARTESIAN_POINT('Ctrl Pts',(-4.91786234455194,5.455664554746E-5,
27.7351405640093));
#54374=CARTESIAN_POINT('Origin',(0.,0.,-3.23514056400933));
#54375=CARTESIAN_POINT('',(-4.91798336942312,-0.000103487961194405,23.8898594359907));
#54376=CARTESIAN_POINT('',(-4.91812910911164,0.000125410111702917,24.2351405640093));
#54377=CARTESIAN_POINT('',(-4.91825,1.47989506776076E-12,-3.23514056400933));
#54378=CARTESIAN_POINT('Ctrl Pts',(-4.91798336942312,-0.000103487961194554,
23.8898594359907));
#54379=CARTESIAN_POINT('Ctrl Pts',(-4.91819811111129,-0.282531091654608,
23.9058511828524));
#54380=CARTESIAN_POINT('Ctrl Pts',(-4.82487700658905,-1.38412483582262,
23.9682340821881));
#54381=CARTESIAN_POINT('Ctrl Pts',(-4.01299334824328,-3.19198306884484,
24.0770081339978));
#54382=CARTESIAN_POINT('Ctrl Pts',(-1.99289265244315,-4.72453705675752,
24.2161815914197));
#54383=CARTESIAN_POINT('Ctrl Pts',(0.514540139737736,-5.10177615830366,
24.3553550488417));
#54384=CARTESIAN_POINT('Ctrl Pts',(2.89614983519387,-4.23145219244452,24.4945285062636));
#54385=CARTESIAN_POINT('Ctrl Pts',(4.56954939756152,-2.32638987018126,24.6337019636856));
#54386=CARTESIAN_POINT('Ctrl Pts',(5.12553398792908,0.147556305933546,24.7728754211075));
#54387=CARTESIAN_POINT('Ctrl Pts',(4.42814588893175,2.58541979399356,24.9120488785295));
#54388=CARTESIAN_POINT('Ctrl Pts',(2.64792093141759,4.39105753387467,25.0512223359514));
#54389=CARTESIAN_POINT('Ctrl Pts',(0.220186507211287,5.12292781784782,25.1903957933734));
#54390=CARTESIAN_POINT('Ctrl Pts',(-2.26139123465815,4.60206271237672,25.3295692507953));
#54391=CARTESIAN_POINT('Ctrl Pts',(-4.18997956700173,2.95583198997252,25.4687427082172));
#54392=CARTESIAN_POINT('Ctrl Pts',(-4.86180231945706,1.19522716609489,25.5721727699491));
#54393=CARTESIAN_POINT('Ctrl Pts',(-4.91844725052962,0.188147310411823,
25.6292116792069));
#54394=CARTESIAN_POINT('Ctrl Pts',(-4.91825297823531,0.000128629553767055,
25.6398594359908));
#54395=CARTESIAN_POINT('Ctrl Pts',(-4.91812910911164,0.000125410111702882,
24.2351405640093));
#54396=CARTESIAN_POINT('Ctrl Pts',(-4.91755969077297,-0.591015325586734,
24.2686152542541));
#54397=CARTESIAN_POINT('Ctrl Pts',(-4.66305203111981,-2.00186995761876,
24.3484810969728));
#54398=CARTESIAN_POINT('Ctrl Pts',(-3.34450836095903,-3.8867898606076,24.4747380921655));
#54399=CARTESIAN_POINT('Ctrl Pts',(-1.07322428658152,-5.01408628044417,
24.6139115495875));
#54400=CARTESIAN_POINT('Ctrl Pts',(1.46050073805254,-4.91526288118904,24.7530850070094));
#54401=CARTESIAN_POINT('Ctrl Pts',(3.63708214756602,-3.61448544732211,24.8922584644314));
#54402=CARTESIAN_POINT('Ctrl Pts',(4.92426950692363,-1.42983964843226,25.0314319218533));
#54403=CARTESIAN_POINT('Ctrl Pts',(5.0073003960314,1.10445205461833,25.1706053792753));
#54404=CARTESIAN_POINT('Ctrl Pts',(3.86587085260431,3.36866652371991,25.3097788366973));
#54405=CARTESIAN_POINT('Ctrl Pts',(1.77910040251715,4.80912396958221,25.4489522941192));
#54406=CARTESIAN_POINT('Ctrl Pts',(-0.742722446286816,5.07358206446181,
25.5881257515412));
#54407=CARTESIAN_POINT('Ctrl Pts',(-3.08292362754424,4.0973715359699,25.7272992089631));
#54408=CARTESIAN_POINT('Ctrl Pts',(-4.59133353590126,2.2163629543867,25.8596374797858));
#54409=CARTESIAN_POINT('Ctrl Pts',(-4.9177971782915,0.698288298756671,25.9455845981345));
#54410=CARTESIAN_POINT('Ctrl Pts',(-4.91846315696893,-0.000107099940742945,
25.9851405640093));
#54411=CARTESIAN_POINT('Origin',(0.,0.,-3.23514056400933));
#54412=CARTESIAN_POINT('',(-4.91860118447858,6.69814320594633E-5,22.1398594359908));
#54413=CARTESIAN_POINT('',(-4.91808775011422,-0.000121504406732365,22.4851405640093));
#54414=CARTESIAN_POINT('',(-4.91825,1.47989506776076E-12,-3.23514056400933));
#54415=CARTESIAN_POINT('Ctrl Pts',(-4.91860118447858,6.69814320593525E-5,
22.1398594359908));
#54416=CARTESIAN_POINT('Ctrl Pts',(-4.91809758575849,-0.752564123265761,
22.182490686498));
#54417=CARTESIAN_POINT('Ctrl Pts',(-4.55189348730661,-2.32467849421272,
22.2715130894791));
#54418=CARTESIAN_POINT('Ctrl Pts',(-2.94553417198737,-4.19722526992435,
22.4069266449343));
#54419=CARTESIAN_POINT('Ctrl Pts',(-0.57428624079235,-5.09539663210565,
22.5461001023563));
#54420=CARTESIAN_POINT('Ctrl Pts',(1.93739480269542,-4.74756494461378,22.6852735597782));
#54421=CARTESIAN_POINT('Ctrl Pts',(3.97531491904182,-3.23878724513983,22.8244470172002));
#54422=CARTESIAN_POINT('Ctrl Pts',(5.04113121891057,-0.938012557784862,
22.9636204746221));
#54423=CARTESIAN_POINT('Ctrl Pts',(4.87421426441648,1.59213907350953,23.1027939320441));
#54424=CARTESIAN_POINT('Ctrl Pts',(3.51538110070013,3.73295690327082,23.241967389466));
#54425=CARTESIAN_POINT('Ctrl Pts',(1.29691405791799,4.9609359450825,23.381140846888));
#54426=CARTESIAN_POINT('Ctrl Pts',(-1.23869392363774,4.97579228750355,23.52031430431));
#54427=CARTESIAN_POINT('Ctrl Pts',(-3.47139782963254,3.77389303415709,23.6594877617318));
#54428=CARTESIAN_POINT('Ctrl Pts',(-4.69621463502052,1.89328920109618,23.7826694722922));
#54429=CARTESIAN_POINT('Ctrl Pts',(-4.91757515762881,0.536775400570982,
23.8594600303784));
#54430=CARTESIAN_POINT('Ctrl Pts',(-4.91798336942312,-0.000103487961194554,
23.8898594359907));
#54431=CARTESIAN_POINT('Ctrl Pts',(-4.91808775011422,-0.000121504406732746,
22.4851405640093));
#54432=CARTESIAN_POINT('Ctrl Pts',(-4.91831091521774,-0.242467126595803,
22.4988636054256));
#54433=CARTESIAN_POINT('Ctrl Pts',(-4.84124936173334,-1.30392870955655,
22.5589777993159));
#54434=CARTESIAN_POINT('Ctrl Pts',(-4.089788760808,-3.09297583065489,22.6654831456802));
#54435=CARTESIAN_POINT('Ctrl Pts',(-2.10773789918185,-4.67443178850642,
22.8046566031021));
#54436=CARTESIAN_POINT('Ctrl Pts',(0.389728746515864,-5.11282535406657,
22.9438300605241));
#54437=CARTESIAN_POINT('Ctrl Pts',(2.79189305526804,-4.30095393662765,23.083003517946));
#54438=CARTESIAN_POINT('Ctrl Pts',(4.51134166740374,-2.43734855057574,23.222176975368));
#54439=CARTESIAN_POINT('Ctrl Pts',(5.12760913750936,0.0222739753389076,
23.3613504327899));
#54440=CARTESIAN_POINT('Ctrl Pts',(4.48999647145208,2.47644973367009,23.5005238902119));
#54441=CARTESIAN_POINT('Ctrl Pts',(2.75442231183803,4.32504674253304,23.6396973476338));
#54442=CARTESIAN_POINT('Ctrl Pts',(0.345295365574717,5.11601824738336,23.7788708050558));
#54443=CARTESIAN_POINT('Ctrl Pts',(-2.14826839878302,4.65594399492059,23.9180442624777));
#54444=CARTESIAN_POINT('Ctrl Pts',(-4.11650525148601,3.05732826362086,24.0572177198997));
#54445=CARTESIAN_POINT('Ctrl Pts',(-4.8468218058486,1.27541781951381,24.1629164870769));
#54446=CARTESIAN_POINT('Ctrl Pts',(-4.91834882348122,0.228221530761836,
24.2222241017801));
#54447=CARTESIAN_POINT('Ctrl Pts',(-4.91812910911164,0.000125410111702882,
24.2351405640093));
#54448=CARTESIAN_POINT('Origin',(0.,0.,-3.23514056400933));
#54449=CARTESIAN_POINT('',(-4.91782637975552,-5.24142894187958E-6,20.3898594359907));
#54450=CARTESIAN_POINT('',(-4.91850368862107,9.83542250791031E-5,20.7351405640093));
#54451=CARTESIAN_POINT('',(-4.91825,1.47989506776076E-12,-3.23514056400933));
#54452=CARTESIAN_POINT('Ctrl Pts',(-4.91782637975553,-5.24142894198221E-6,
20.3898594359907));
#54453=CARTESIAN_POINT('Ctrl Pts',(-4.91784131778503,-0.404115038784516,
20.4127390376695));
#54454=CARTESIAN_POINT('Ctrl Pts',(-4.76876465270878,-1.627595371266,20.4820097918222));
#54455=CARTESIAN_POINT('Ctrl Pts',(-3.76535729773513,-3.48065452827909,
20.5976716984489));
#54456=CARTESIAN_POINT('Ctrl Pts',(-1.63721722455307,-4.85925830600346,
20.7368451558709));
#54457=CARTESIAN_POINT('Ctrl Pts',(0.891279837899838,-5.04960313048365,
20.8760186132929));
#54458=CARTESIAN_POINT('Ctrl Pts',(3.20182774421876,-4.00514302131496,21.0151920707148));
#54459=CARTESIAN_POINT('Ctrl Pts',(4.72941655591346,-1.98128507930803,21.1543655281368));
#54460=CARTESIAN_POINT('Ctrl Pts',(5.10049727269117,0.527066500649415,21.2935389855586));
#54461=CARTESIAN_POINT('Ctrl Pts',(4.22432765441569,2.9065318496407,21.4327124429807));
#54462=CARTESIAN_POINT('Ctrl Pts',(2.3151618789705,4.57524829916352,21.5718859004026));
#54463=CARTESIAN_POINT('Ctrl Pts',(-0.160142112979361,5.12515619552101,
21.7110593578246));
#54464=CARTESIAN_POINT('Ctrl Pts',(-2.5962857459699,4.4217837859975,21.8502328152465));
#54465=CARTESIAN_POINT('Ctrl Pts',(-4.39754652471548,2.63713027509066,21.9894062726684));
#54466=CARTESIAN_POINT('Ctrl Pts',(-4.90109526461051,0.951811533492146,
22.0859484795832));
#54467=CARTESIAN_POINT('Ctrl Pts',(-4.91864559982637,0.0664459672029366,
22.136099534024));
#54468=CARTESIAN_POINT('Ctrl Pts',(-4.91860118447858,6.69814320593525E-5,
22.1398594359908));
#54469=CARTESIAN_POINT('Ctrl Pts',(-4.91850368862107,9.83542250790163E-5,
20.7351405640093));
#54470=CARTESIAN_POINT('Ctrl Pts',(-4.91786254178827,-0.712520933069854,
20.7755031090711));
#54471=CARTESIAN_POINT('Ctrl Pts',(-4.5811979304639,-2.24478329879145,20.8622568066069));
#54472=CARTESIAN_POINT('Ctrl Pts',(-3.04721056302127,-4.12400040999737,
20.9954016566167));
#54473=CARTESIAN_POINT('Ctrl Pts',(-0.698616677582171,-5.07984314077225,
21.1345751140387));
#54474=CARTESIAN_POINT('Ctrl Pts',(1.82081346922569,-4.79348619559222,21.2737485714606));
#54475=CARTESIAN_POINT('Ctrl Pts',(3.89499091063157,-3.33495388321102,21.4129220288826));
#54476=CARTESIAN_POINT('Ctrl Pts',(5.01670657064901,-1.06090846968716,21.5520954863046));
#54477=CARTESIAN_POINT('Ctrl Pts',(4.91166165878904,1.47256624524283,21.6912689437265));
#54478=CARTESIAN_POINT('Ctrl Pts',(3.6055433374024,3.6459469056968,21.8304424011485));
#54479=CARTESIAN_POINT('Ctrl Pts',(1.41774331025312,4.92776577195785,21.9696158585704));
#54480=CARTESIAN_POINT('Ctrl Pts',(-1.11674464244417,5.00457320863818,22.1087893159924));
#54481=CARTESIAN_POINT('Ctrl Pts',(-3.37814939266335,3.85758710567824,22.2479627734143));
#54482=CARTESIAN_POINT('Ctrl Pts',(-4.67194924907029,1.97339756309458,22.3734131894199));
#54483=CARTESIAN_POINT('Ctrl Pts',(-4.91755649890211,0.576789506777712,
22.4524724529516));
#54484=CARTESIAN_POINT('Ctrl Pts',(-4.91808775011422,-0.000121504406732746,
22.4851405640093));
#54485=CARTESIAN_POINT('Origin',(0.,0.,-3.23514056400933));
#54486=CARTESIAN_POINT('',(-4.91862258429063,-5.67213663493321E-5,18.6398594359907));
#54487=CARTESIAN_POINT('',(-4.91784723885709,-4.2125959418271E-5,18.9851405640093));
#54488=CARTESIAN_POINT('',(-4.91825,1.47989506776076E-12,-3.23514056400933));
#54489=CARTESIAN_POINT('Ctrl Pts',(-4.91862258429063,-5.67213663495159E-5,
18.6398594359907));
#54490=CARTESIAN_POINT('Ctrl Pts',(-4.91865476642852,-0.0552782982130806,
18.642987388841));
#54491=CARTESIAN_POINT('Ctrl Pts',(-4.90423951910381,-0.929482791963975,
18.6925064941653));
#54492=CARTESIAN_POINT('Ctrl Pts',(-4.41539501983301,-2.60713604241717,
18.7884167519636));
#54493=CARTESIAN_POINT('Ctrl Pts',(-2.62632371694331,-4.40400899847605,
18.9275902093855));
#54494=CARTESIAN_POINT('Ctrl Pts',(-0.195024223195767,-5.12394741163527,
19.0667636668075));
#54495=CARTESIAN_POINT('Ctrl Pts',(2.28396552793643,-4.59090110893657,19.2059371242294));
#54496=CARTESIAN_POINT('Ctrl Pts',(4.2044456636982,-2.9352185925151,19.3451105816514));
#54497=CARTESIAN_POINT('Ctrl Pts',(5.09679148580437,-0.561772262637615,
19.4842840390733));
#54498=CARTESIAN_POINT('Ctrl Pts',(4.74279316762406,1.94904707330927,19.6234574964953));
#54499=CARTESIAN_POINT('Ctrl Pts',(3.22901570416719,3.98325609358456,19.7626309539172));
#54500=CARTESIAN_POINT('Ctrl Pts',(0.925630737050274,5.04341940190033,19.9018044113392));
#54501=CARTESIAN_POINT('Ctrl Pts',(-1.60410338490353,4.87028991492066,20.0409778687611));
#54502=CARTESIAN_POINT('Ctrl Pts',(-3.7415780118875,3.5062038597031,20.1801513261831));
#54503=CARTESIAN_POINT('Ctrl Pts',(-4.76312665923809,1.64993048430327,20.2964451819263));
#54504=CARTESIAN_POINT('Ctrl Pts',(-4.91781102912816,0.415266324955308,
20.3663478851955));
#54505=CARTESIAN_POINT('Ctrl Pts',(-4.91782637975553,-5.24142894198221E-6,
20.3898594359907));
#54506=CARTESIAN_POINT('Ctrl Pts',(-4.91784723885709,-4.21259594185139E-5,
18.9851405640093));
#54507=CARTESIAN_POINT('Ctrl Pts',(-4.91795594482061,-0.364076614836121,
19.0057514602427));
#54508=CARTESIAN_POINT('Ctrl Pts',(-4.78832206838964,-1.54740630006116,
19.07275350895));
#54509=CARTESIAN_POINT('Ctrl Pts',(-3.84928009761185,-3.3876118914622,19.1861467101313));
#54510=CARTESIAN_POINT('Ctrl Pts',(-1.75546046578727,-4.8178034569817,19.3253201675533));
#54511=CARTESIAN_POINT('Ctrl Pts',(0.767630771739118,-5.06987323266825,
19.4644936249752));
#54512=CARTESIAN_POINT('Ctrl Pts',(3.10300938320942,-4.08218132433643,19.6036670823972));
#54513=CARTESIAN_POINT('Ctrl Pts',(4.67959345250773,-2.09625301819547,19.7428405398192));
#54514=CARTESIAN_POINT('Ctrl Pts',(5.11185292177081,0.402282616117053,19.8820139972411));
#54515=CARTESIAN_POINT('Ctrl Pts',(4.29408520181098,2.80244605240401,20.0211874546631));
#54516=CARTESIAN_POINT('Ctrl Pts',(2.4262631596223,4.5173132144347,20.160360912085));
#54517=CARTESIAN_POINT('Ctrl Pts',(-0.0348652558426957,5.12753898190759,
20.299534369507));
#54518=CARTESIAN_POINT('Ctrl Pts',(-2.4874678943674,4.48390176872088,20.4387078269289));
#54519=CARTESIAN_POINT('Ctrl Pts',(-4.33179745699125,2.74379343038994,20.5778812843509));
#54520=CARTESIAN_POINT('Ctrl Pts',(-4.88917263131133,1.03197826464391,20.676692196711));
#54521=CARTESIAN_POINT('Ctrl Pts',(-4.91859945122828,0.106536189372549,
20.7291119565971));
#54522=CARTESIAN_POINT('Ctrl Pts',(-4.91850368862107,9.83542250790163E-5,
20.7351405640093));
#54523=CARTESIAN_POINT('Origin',(0.,0.,-3.23514056400933));
#54524=CARTESIAN_POINT('',(-4.91795812443448,9.68028131021826E-5,16.8898594359907));
#54525=CARTESIAN_POINT('',(-4.91867111326921,-1.61887755736889E-5,17.2351405640093));
#54526=CARTESIAN_POINT('',(-4.91825,1.47989506776076E-12,-3.23514056400933));
#54527=CARTESIAN_POINT('Ctrl Pts',(-4.91795812443448,9.68028131020232E-5,
16.8898594359907));
#54528=CARTESIAN_POINT('Ctrl Pts',(-4.91758682380195,-0.525629068321328,
16.9196268924865));
#54529=CARTESIAN_POINT('Ctrl Pts',(-4.70277528584012,-1.87096968829015,
16.9957855014563));
#54530=CARTESIAN_POINT('Ctrl Pts',(-3.4970054763967,-3.75017655889538,17.1183352629001));
#54531=CARTESIAN_POINT('Ctrl Pts',(-1.27253436014598,-4.96724549696155,
17.2575087203221));
#54532=CARTESIAN_POINT('Ctrl Pts',(1.2631160043629,-4.96964882907829,17.3966821777441));
#54533=CARTESIAN_POINT('Ctrl Pts',(3.48989023867801,-3.75679885631596,17.535855635166));
#54534=CARTESIAN_POINT('Ctrl Pts',(4.86326400304377,-1.62527990252007,17.675029092588));
#54535=CARTESIAN_POINT('Ctrl Pts',(5.04739928085542,0.903676946954519,17.8142025500099));
#54536=CARTESIAN_POINT('Ctrl Pts',(3.9972685434884,3.21165311266256,17.9533760074318));
#54537=CARTESIAN_POINT('Ctrl Pts',(1.96966555908043,4.73426753682229,18.0925494648538));
#54538=CARTESIAN_POINT('Ctrl Pts',(-0.539589683365057,5.09918763122548,
18.2317229222758));
#54539=CARTESIAN_POINT('Ctrl Pts',(-2.91689633778329,4.21717764381148,18.3708963796977));
#54540=CARTESIAN_POINT('Ctrl Pts',(-4.5435203376001,2.34692079867374,18.5069418842694));
#54541=CARTESIAN_POINT('Ctrl Pts',(-4.91817746816439,0.763721448255779,
18.596596236367));
#54542=CARTESIAN_POINT('Ctrl Pts',(-4.91862258429063,-5.67213663495159E-5,
18.6398594359907));
#54543=CARTESIAN_POINT('Ctrl Pts',(-4.91867111326921,-1.61887755739448E-5,
17.2351405640093));
#54544=CARTESIAN_POINT('Ctrl Pts',(-4.91867394862149,-0.0151850987544867,
17.2359998114142));
#54545=CARTESIAN_POINT('Ctrl Pts',(-4.91489622429265,-0.849328838714203,
17.2832502112931));
#54546=CARTESIAN_POINT('Ctrl Pts',(-4.47778002818978,-2.49847105570419,
17.376891763646));
#54547=CARTESIAN_POINT('Ctrl Pts',(-2.73314800394566,-4.33852205083421,
17.5160652210679));
#54548=CARTESIAN_POINT('Ctrl Pts',(-0.320165506910762,-5.11765235681669,
17.6552386784899));
#54549=CARTESIAN_POINT('Ctrl Pts',(2.17110867707493,-4.64533730846069,17.7944121359119));
#54550=CARTESIAN_POINT('Ctrl Pts',(4.13147070090376,-3.0370744878288,17.9335855933338));
#54551=CARTESIAN_POINT('Ctrl Pts',(5.08154334695868,-0.686140517697928,
18.0727590507557));
#54552=CARTESIAN_POINT('Ctrl Pts',(4.78900055706072,1.83257885547087,18.2119325081777));
#54553=CARTESIAN_POINT('Ctrl Pts',(3.3253792957861,3.90316847397136,18.3511059655996));
#54554=CARTESIAN_POINT('Ctrl Pts',(1.04858625554496,5.01929661025616,18.4902794230216));
#54555=CARTESIAN_POINT('Ctrl Pts',(-1.4846228729006,4.90803081920919,18.6294528804436));
#54556=CARTESIAN_POINT('Ctrl Pts',(-3.6547896788716,3.5965794861591,18.7686263378655));
#54557=CARTESIAN_POINT('Ctrl Pts',(-4.74219752133363,1.7301058879693,18.8871888990541));
#54558=CARTESIAN_POINT('Ctrl Pts',(-4.91771126866139,0.455294813171815,
18.9593603077687));
#54559=CARTESIAN_POINT('Ctrl Pts',(-4.91784723885709,-4.21259594185139E-5,
18.9851405640093));
#54560=CARTESIAN_POINT('Origin',(0.,0.,-3.23514056400933));
#54561=CARTESIAN_POINT('',(-4.91828854462098,-0.000127404755611427,15.1398594359907));
#54562=CARTESIAN_POINT('',(-4.91788408102176,6.79148635503168E-5,15.4851405640093));
#54563=CARTESIAN_POINT('',(-4.91825,1.47989506776076E-12,-3.23514056400933));
#54564=CARTESIAN_POINT('Ctrl Pts',(-4.91828854462098,-0.000127404755611727,
15.1398594359907));
#54565=CARTESIAN_POINT('Ctrl Pts',(-4.91847218829568,-0.176983412021483,
15.1498752436581));
#54566=CARTESIAN_POINT('Ctrl Pts',(-4.86579387478643,-1.17289109012218,
15.2062822037994));
#54567=CARTESIAN_POINT('Ctrl Pts',(-4.21000220374625,-2.92724323712408,
15.3090803164148));
#54568=CARTESIAN_POINT('Ctrl Pts',(-2.29266408325714,-4.58656330231903,
15.4482537738367));
#54569=CARTESIAN_POINT('Ctrl Pts',(0.185310754227624,-5.12430789953185,
15.5874272312587));
#54570=CARTESIAN_POINT('Ctrl Pts',(2.6179706179084,-4.40897962896238,15.7266006886806));
#54571=CARTESIAN_POINT('Ctrl Pts',(4.41044491618784,-2.61550132213878,15.8657741461026));
#54572=CARTESIAN_POINT('Ctrl Pts',(5.12441086413413,-0.182441279268398,
16.0049476035245));
#54573=CARTESIAN_POINT('Ctrl Pts',(4.58527876584435,2.29523205021492,16.1441210609465));
#54574=CARTESIAN_POINT('Ctrl Pts',(2.92488531375835,4.21164070478449,16.2832945183684));
#54575=CARTESIAN_POINT('Ctrl Pts',(0.549254897012139,5.09815560599567,16.4224679757903));
#54576=CARTESIAN_POINT('Ctrl Pts',(-1.96068759122481,4.73799279172668,16.5616414332123));
#54577=CARTESIAN_POINT('Ctrl Pts',(-3.99117324920656,3.21922469232187,16.7008148906343));
#54578=CARTESIAN_POINT('Ctrl Pts',(-4.82013201349797,1.40646381671154,16.8102208915604));
#54579=CARTESIAN_POINT('Ctrl Pts',(-4.91816547801985,0.293689473413913,
16.8732357400126));
#54580=CARTESIAN_POINT('Ctrl Pts',(-4.91795812443448,9.68028131020232E-5,
16.8898594359907));
#54581=CARTESIAN_POINT('Ctrl Pts',(-4.91788408102176,6.79148635503515E-5,
15.4851405640093));
#54582=CARTESIAN_POINT('Ctrl Pts',(-4.91764809163557,-0.485611072828922,
15.5126393150597));
#54583=CARTESIAN_POINT('Ctrl Pts',(-4.72562172430427,-1.7908264783202,15.5865292185841));
#54584=CARTESIAN_POINT('Ctrl Pts',(-3.587593947644,-3.66361041376876,15.7068102745826));
#54585=CARTESIAN_POINT('Ctrl Pts',(-1.39352506003175,-4.93466913826148,
15.8459837320045));
#54586=CARTESIAN_POINT('Ctrl Pts',(1.1413095421973,-4.99902831817707,15.9851571894265));
#54587=CARTESIAN_POINT('Ctrl Pts',(3.39705396305783,-3.8409498784962,16.1243306468484));
#54588=CARTESIAN_POINT('Ctrl Pts',(4.82209963689558,-1.74362458370441,16.2635041042704));
#54589=CARTESIAN_POINT('Ctrl Pts',(5.06797295434764,0.780078028819932,16.4026775616923));
#54590=CARTESIAN_POINT('Ctrl Pts',(4.07454927242783,3.11302422470575,16.5418510191143));
#54591=CARTESIAN_POINT('Ctrl Pts',(2.08475549686315,4.68472689869385,16.6810244765362));
#54592=CARTESIAN_POINT('Ctrl Pts',(-0.414834059965531,5.1108496651476,16.8201979339582));
#54593=CARTESIAN_POINT('Ctrl Pts',(-2.81298215087013,4.28719057378289,16.9593713913801));
#54594=CARTESIAN_POINT('Ctrl Pts',(-4.51269839905733,2.42672090768734,17.0976856013972));
#54595=CARTESIAN_POINT('Ctrl Pts',(-4.91852086668098,0.803791149140066,
17.1896086589402));
#54596=CARTESIAN_POINT('Ctrl Pts',(-4.91867111326921,-1.61887755739448E-5,
17.2351405640093));
#54597=CARTESIAN_POINT('Origin',(0.,0.,-3.23514056400933));
#54598=CARTESIAN_POINT('',(-4.91830432977965,0.000126561679052736,13.3898594359907));
#54599=CARTESIAN_POINT('',(-4.91841486112574,-0.000115290859867556,13.7351405640093));
#54600=CARTESIAN_POINT('',(-4.91825,1.47989506776076E-12,-3.23514056400933));
#54601=CARTESIAN_POINT('Ctrl Pts',(-4.91830432977965,0.000126561679052607,
13.3898594359907));
#54602=CARTESIAN_POINT('Ctrl Pts',(-4.91763218604279,-0.64711550896179,
13.4265147473036));
#54603=CARTESIAN_POINT('Ctrl Pts',(-4.62657036081707,-2.11409703197736,
13.5095612110905));
#54604=CARTESIAN_POINT('Ctrl Pts',(-3.20941426864339,-3.99906633816759,
13.6389988273513));
#54605=CARTESIAN_POINT('Ctrl Pts',(-0.900850425695856,-5.04790451923969,
13.7781722847733));
#54606=CARTESIAN_POINT('Ctrl Pts',(1.62800291751233,-4.86235313664159,13.9173457421952));
#54607=CARTESIAN_POINT('Ctrl Pts',(3.75875249244549,-3.4877860062469,14.0565191996172));
#54608=CARTESIAN_POINT('Ctrl Pts',(4.97035535384435,-1.26033296447714,14.1956926570391));
#54609=CARTESIAN_POINT('Ctrl Pts',(4.96653214029797,1.27531565669998,14.3348661144611));
#54610=CARTESIAN_POINT('Ctrl Pts',(3.7482177615067,3.49910490513827,14.474039571883));
#54611=CARTESIAN_POINT('Ctrl Pts',(1.61333278009552,4.86724037474072,14.613213029305));
#54612=CARTESIAN_POINT('Ctrl Pts',(-0.916068606863061,5.04516499555335,
14.7523864867269));
#54613=CARTESIAN_POINT('Ctrl Pts',(-3.22145911492965,3.98936996224636,14.8915599441489));
#54614=CARTESIAN_POINT('Ctrl Pts',(-4.62987159599441,2.10422201302728,15.0207175939035));
#54615=CARTESIAN_POINT('Ctrl Pts',(-4.91762158872381,0.642177086213023,
15.1034840911841));
#54616=CARTESIAN_POINT('Ctrl Pts',(-4.91828854462098,-0.000127404755611727,
15.1398594359907));
#54617=CARTESIAN_POINT('Ctrl Pts',(-4.91841486112574,-0.000115290859867678,
13.7351405640093));
#54618=CARTESIAN_POINT('Ctrl Pts',(-4.9185513730654,-0.136901079078092,
13.7428876662313));
#54619=CARTESIAN_POINT('Ctrl Pts',(-4.87947714473731,-1.09270897128707,
13.7970259209272));
#54620=CARTESIAN_POINT('Ctrl Pts',(-4.28027009411781,-2.82350128713404,
13.8975553280972));
#54621=CARTESIAN_POINT('Ctrl Pts',(-2.40404855375509,-4.52917455484274,
14.0367287855191));
#54622=CARTESIAN_POINT('Ctrl Pts',(0.06004711021698,-5.12730591457165,14.1759022429411));
#54623=CARTESIAN_POINT('Ctrl Pts',(2.5094591513317,-4.47163128677269,14.315075700363));
#54624=CARTESIAN_POINT('Ctrl Pts',(4.34522048351284,-2.72248609669679,14.454249157785));
#54625=CARTESIAN_POINT('Ctrl Pts',(5.11842312500342,-0.307597643809348,
14.5934226152069));
#54626=CARTESIAN_POINT('Ctrl Pts',(4.63999193232155,2.18250921304762,14.7325960726289));
#54627=CARTESIAN_POINT('Ctrl Pts',(3.02692009916372,4.13891607915956,14.8717695300508));
#54628=CARTESIAN_POINT('Ctrl Pts',(0.673660220405915,5.08321291158352,15.0109429874728));
#54629=CARTESIAN_POINT('Ctrl Pts',(-1.84433319131777,4.78448604099233,15.1501164448947));
#54630=CARTESIAN_POINT('Ctrl Pts',(-3.91132250131647,3.31578465641879,15.2892899023167));
#54631=CARTESIAN_POINT('Ctrl Pts',(-4.80243024213341,1.4866607259055,15.4009646086882));
#54632=CARTESIAN_POINT('Ctrl Pts',(-4.91804621224755,0.333742792738227,
15.4662481625857));
#54633=CARTESIAN_POINT('Ctrl Pts',(-4.91788408102176,6.79148635503515E-5,
15.4851405640093));
#54634=CARTESIAN_POINT('Origin',(0.,0.,-3.23514056400933));
#54635=CARTESIAN_POINT('',(-4.91794754609162,-9.36338042964645E-5,11.6398594359907));
#54636=CARTESIAN_POINT('',(-4.91817784002761,0.000128112752882797,11.9851405640093));
#54637=CARTESIAN_POINT('',(-4.91825,1.47989506776076E-12,-3.23514056400933));
#54638=CARTESIAN_POINT('Ctrl Pts',(-4.91794754609163,-9.36338042967569E-5,
11.6398594359907));
#54639=CARTESIAN_POINT('Ctrl Pts',(-4.91815090375448,-0.298632658744152,
11.6567630984751));
#54640=CARTESIAN_POINT('Ctrl Pts',(-4.81800407439185,-1.41636045649421,
11.7200579134335));
#54641=CARTESIAN_POINT('Ctrl Pts',(-3.98144732521719,-3.23124569189002,
11.829743880866));
#54642=CARTESIAN_POINT('Ctrl Pts',(-1.94639095768057,-4.74388382706577,
11.9689173382879));
#54643=CARTESIAN_POINT('Ctrl Pts',(0.564626212170274,-5.09647611250825,
12.1080907957099));
#54644=CARTESIAN_POINT('Ctrl Pts',(2.93757248527155,-4.20280137748769,12.2472642531318));
#54645=CARTESIAN_POINT('Ctrl Pts',(4.59217933564339,-2.28139441441562,12.3864377105538));
#54646=CARTESIAN_POINT('Ctrl Pts',(5.12383740106595,0.197893436663885,12.5256111679757));
#54647=CARTESIAN_POINT('Ctrl Pts',(4.40253765207021,2.62878940711139,12.6647846253977));
#54648=CARTESIAN_POINT('Ctrl Pts',(2.60466315593581,4.41685423904247,12.8039580828196));
#54649=CARTESIAN_POINT('Ctrl Pts',(0.169857235225308,5.12484341658148,12.9431315402416));
#54650=CARTESIAN_POINT('Ctrl Pts',(-2.30648473230954,4.57962877365185,13.0823049976635));
#54651=CARTESIAN_POINT('Ctrl Pts',(-4.21881034979734,2.9145343980265,13.2214784550854));
#54652=CARTESIAN_POINT('Ctrl Pts',(-4.86753707266041,1.16299591758168,13.3239966011945));
#54653=CARTESIAN_POINT('Ctrl Pts',(-4.9184828546489,0.172037418983138,13.3801235948296));
#54654=CARTESIAN_POINT('Ctrl Pts',(-4.91830432977965,0.000126561679052607,
13.3898594359907));
#54655=CARTESIAN_POINT('Ctrl Pts',(-4.91817784002761,0.000128112752882659,
11.9851405640093));
#54656=CARTESIAN_POINT('Ctrl Pts',(-4.91757026063081,-0.607099161997894,
12.0195271698768));
#54657=CARTESIAN_POINT('Ctrl Pts',(-4.65282093162953,-2.03405502531225,
12.1003049282183));
#54658=CARTESIAN_POINT('Ctrl Pts',(-3.30617002296448,-3.91945294349836,
12.2274738390338));
#54659=CARTESIAN_POINT('Ctrl Pts',(-1.02392293276547,-5.02438587538853,
12.3666472964557));
#54660=CARTESIAN_POINT('Ctrl Pts',(1.50870919886821,-4.90068037626382,12.5058207538777));
#54661=CARTESIAN_POINT('Ctrl Pts',(3.67240905719958,-3.57858677603957,12.6449942112996));
#54662=CARTESIAN_POINT('Ctrl Pts',(4.93807619790383,-1.38140329402478,12.7841676687216));
#54663=CARTESIAN_POINT('Ctrl Pts',(4.99621064854467,1.15358170599905,12.9233411261435));
#54664=CARTESIAN_POINT('Ctrl Pts',(3.83259649856215,3.40647555051493,13.0625145835655));
#54665=CARTESIAN_POINT('Ctrl Pts',(1.7317781876149,4.82636673968609,13.2016880409874));
#54666=CARTESIAN_POINT('Ctrl Pts',(-0.792520582052584,5.06604211629452,
13.3408614984094));
#54667=CARTESIAN_POINT('Ctrl Pts',(-3.12302029475477,4.06689265110314,13.4800349558313));
#54668=CARTESIAN_POINT('Ctrl Pts',(-4.60261538530517,2.18422194630641,13.6114613110313));
#54669=CARTESIAN_POINT('Ctrl Pts',(-4.91773391306217,0.68219878247996,13.6964965137573));
#54670=CARTESIAN_POINT('Ctrl Pts',(-4.91841486112574,-0.000115290859867678,
13.7351405640093));
#54671=CARTESIAN_POINT('Origin',(0.,0.,-3.23514056400933));
#54672=CARTESIAN_POINT('',(-4.91863108450388,5.20022792591365E-5,9.88985943599073));
#54673=CARTESIAN_POINT('',(-4.91804344864283,-0.000115457371072658,10.2351405640093));
#54674=CARTESIAN_POINT('',(-4.91825,1.47989506776076E-12,-3.23514056400933));
#54675=CARTESIAN_POINT('Ctrl Pts',(-4.91863108450388,5.20022792590506E-5,
9.88985943599073));
#54676=CARTESIAN_POINT('Ctrl Pts',(-4.91821498045426,-0.768664899305898,
9.93340260212068));
#54677=CARTESIAN_POINT('Ctrl Pts',(-4.53978139223194,-2.35677273363979,
10.0233369207246));
#54678=CARTESIAN_POINT('Ctrl Pts',(-2.90416590773529,-4.225954555504,10.1596623918025));
#54679=CARTESIAN_POINT('Ctrl Pts',(-0.524210305286386,-5.10079161313893,
10.2988358492245));
#54680=CARTESIAN_POINT('Ctrl Pts',(1.98393308826428,-4.72830635916573,10.4380093066464));
#54681=CARTESIAN_POINT('Ctrl Pts',(4.00693531287256,-3.1995844922883,10.5771827640684));
#54682=CARTESIAN_POINT('Ctrl Pts',(5.05010142654417,-0.888452084500591,
10.7163562214903));
#54683=CARTESIAN_POINT('Ctrl Pts',(4.85834075571687,1.63993799461361,10.8555296789123));
#54684=CARTESIAN_POINT('Ctrl Pts',(3.47854550484689,3.76730576082515,10.9947031363342));
#54685=CARTESIAN_POINT('Ctrl Pts',(1.24812396903648,4.97343523962598,11.1338765937562));
#54686=CARTESIAN_POINT('Ctrl Pts',(-1.28750761891996,4.96338550347039,11.2730500511781));
#54687=CARTESIAN_POINT('Ctrl Pts',(-3.5082984720956,3.73961406505117,11.4122235086001));
#54688=CARTESIAN_POINT('Ctrl Pts',(-4.70565429318266,1.86108102271416,11.5344933035376));
#54689=CARTESIAN_POINT('Ctrl Pts',(-4.9175928000682,0.520690930932643,11.6103719460012));
#54690=CARTESIAN_POINT('Ctrl Pts',(-4.91794754609163,-9.36338042967569E-5,
11.6398594359907));
#54691=CARTESIAN_POINT('Ctrl Pts',(-4.91804344864283,-0.000115457371073178,
10.2351405640093));
#54692=CARTESIAN_POINT('Ctrl Pts',(-4.91826654662029,-0.258571969827967,
10.2497755210483));
#54693=CARTESIAN_POINT('Ctrl Pts',(-4.83479258826795,-1.33616357645592,
10.3108016305613));
#54694=CARTESIAN_POINT('Ctrl Pts',(-4.05921150653168,-3.13299753308037,
10.4182188925484));
#54695=CARTESIAN_POINT('Ctrl Pts',(-2.06172281055525,-4.69490901397279,
10.5573923499703));
#54696=CARTESIAN_POINT('Ctrl Pts',(0.439929367680037,-5.10875070330306,
10.6965658073923));
#54697=CARTESIAN_POINT('Ctrl Pts',(2.83400339776564,-4.27332380454602,10.8357392648142));
#54698=CARTESIAN_POINT('Ctrl Pts',(4.53506427669625,-2.39291947279475,10.9749127222362));
#54699=CARTESIAN_POINT('Ctrl Pts',(5.12714300424288,0.0726375322416105,
11.1140861796581));
#54700=CARTESIAN_POINT('Ctrl Pts',(4.46545558154636,2.52043211499204,11.2532596370801));
#54701=CARTESIAN_POINT('Ctrl Pts',(2.71180777293433,4.35189271463576,11.392433094502));
#54702=CARTESIAN_POINT('Ctrl Pts',(0.295027925902909,5.11916302924455,11.531606551924));
#54703=CARTESIAN_POINT('Ctrl Pts',(-2.19389658855195,4.63461857716327,11.6707800093459));
#54704=CARTESIAN_POINT('Ctrl Pts',(-4.14633649986933,3.01674745825668,11.8099534667679));
#54705=CARTESIAN_POINT('Ctrl Pts',(-4.85296596667775,1.24318419508919,11.9147403183223));
#54706=CARTESIAN_POINT('Ctrl Pts',(-4.91838994921961,0.212114377071997,
11.9731360174028));
#54707=CARTESIAN_POINT('Ctrl Pts',(-4.91817784002761,0.000128112752882659,
11.9851405640093));
#54708=CARTESIAN_POINT('Origin',(0.,0.,-3.23514056400933));
#54709=CARTESIAN_POINT('',(-4.91782719367126,9.87882777895753E-6,8.13985943599073));
#54710=CARTESIAN_POINT('',(-4.91854624166208,8.68734550606501E-5,8.48514056400926));
#54711=CARTESIAN_POINT('',(-4.91825,1.47989506776076E-12,-3.23514056400933));
#54712=CARTESIAN_POINT('Ctrl Pts',(-4.91782719367126,9.87882777886417E-6,
8.13985943599073));
#54713=CARTESIAN_POINT('Ctrl Pts',(-4.91779791116503,-0.420206382800527,
8.16365095329221));
#54714=CARTESIAN_POINT('Ctrl Pts',(-4.76060227876805,-1.65982512688071,
8.23383362306768));
#54715=CARTESIAN_POINT('Ctrl Pts',(-3.73098781882938,-3.51747088411314,
8.35040744531713));
#54716=CARTESIAN_POINT('Ctrl Pts',(-1.58940942229392,-4.87510504637185,
8.48958090273909));
#54717=CARTESIAN_POINT('Ctrl Pts',(0.940835280389158,-5.04060517200187,
8.62875436016105));
#54718=CARTESIAN_POINT('Ctrl Pts',(3.24101278453099,-3.97350068017404,8.76792781758299));
#54719=CARTESIAN_POINT('Ctrl Pts',(4.74864907841449,-1.93473601685351,8.90710127500494));
#54720=CARTESIAN_POINT('Ctrl Pts',(5.09507425160708,0.577139407290319,9.04627473242689));
#54721=CARTESIAN_POINT('Ctrl Pts',(4.19557520845658,2.94788401994064,9.18544818984885));
#54722=CARTESIAN_POINT('Ctrl Pts',(2.27011098883077,4.59776767825721,9.3246216472708));
#54723=CARTESIAN_POINT('Ctrl Pts',(-0.210474925808355,5.12333600600652,
9.46379510469275));
#54724=CARTESIAN_POINT('Ctrl Pts',(-2.63959234478916,4.39606912800144,9.60296856211471));
#54725=CARTESIAN_POINT('Ctrl Pts',(-4.42323692839189,2.59380928368822,9.74214201953665));
#54726=CARTESIAN_POINT('Ctrl Pts',(-4.90560794918632,0.919590948282322,
9.83777231082867));
#54727=CARTESIAN_POINT('Ctrl Pts',(-4.91865830022465,0.0503307356082542,
9.88701144964669));
#54728=CARTESIAN_POINT('Ctrl Pts',(-4.91863108450388,5.20022792590506E-5,
9.88985943599073));
#54729=CARTESIAN_POINT('Ctrl Pts',(-4.91854624166208,8.68734550606501E-5,
8.48514056400926));
#54730=CARTESIAN_POINT('Ctrl Pts',(-4.91794764432125,-0.728614457117709,
8.52641502469384));
#54731=CARTESIAN_POINT('Ctrl Pts',(-4.56956039415971,-2.27690562510606,
8.6140806378524));
#54732=CARTESIAN_POINT('Ctrl Pts',(-3.00655662644843,-4.15373191828816,
8.74813740348495));
#54733=CARTESIAN_POINT('Ctrl Pts',(-0.648687514646424,-5.08646007606358,
8.88731086090689));
#54734=CARTESIAN_POINT('Ctrl Pts',(1.86780842837057,-4.77537048530841,9.02648431832885));
#54735=CARTESIAN_POINT('Ctrl Pts',(3.92755975149067,-3.29653545339913,9.1656577757508));
#54736=CARTESIAN_POINT('Ctrl Pts',(5.0268850702256,-1.01158197284738,9.30483123317275));
#54737=CARTESIAN_POINT('Ctrl Pts',(4.89696081722127,1.52073875193816,9.44400469059471));
#54738=CARTESIAN_POINT('Ctrl Pts',(3.56955802565887,3.68118555610841,9.58317814801665));
#54739=CARTESIAN_POINT('Ctrl Pts',(1.36927319819533,4.9414534810874,9.72235160543861));
#54740=CARTESIAN_POINT('Ctrl Pts',(-1.16584691373595,4.99336285190443,9.86152506286056));
#54741=CARTESIAN_POINT('Ctrl Pts',(-3.41587659702151,3.82422000818044,10.0006985202825));
#54742=CARTESIAN_POINT('Ctrl Pts',(-4.68183725211151,1.94120147697101,10.1252370206654));
#54743=CARTESIAN_POINT('Ctrl Pts',(-4.91755935135749,0.560705835039386,
10.2033843685743));
#54744=CARTESIAN_POINT('Ctrl Pts',(-4.91804344864283,-0.000115457371073178,
10.2351405640093));
#54745=CARTESIAN_POINT('Origin',(0.,0.,-3.23514056400933));
#54746=CARTESIAN_POINT('',(-4.91859079181753,-7.13374654231665E-5,6.38985943599073));
#54747=CARTESIAN_POINT('',(-4.91783496857819,-2.75488291934245E-5,6.73514056400926));
#54748=CARTESIAN_POINT('',(-4.91825,1.47989506776076E-12,-3.23514056400933));
#54749=CARTESIAN_POINT('Ctrl Pts',(-4.91859079181753,-7.13374654238812E-5,
6.38985943599073));
#54750=CARTESIAN_POINT('Ctrl Pts',(-4.91864101597956,-0.0713934139407059,
6.39389930446375));
#54751=CARTESIAN_POINT('Ctrl Pts',(-4.89967772397134,-0.96170387456932,
6.44433032541076));
#54752=CARTESIAN_POINT('Ctrl Pts',(-4.3895740957611,-2.65037936580031,6.54115249883176));
#54753=CARTESIAN_POINT('Ctrl Pts',(-2.58293977084456,-4.42959294574867,
6.68032595625371));
#54754=CARTESIAN_POINT('Ctrl Pts',(-0.14468615032387,-5.12561581107493,
6.81949941367566));
#54755=CARTESIAN_POINT('Ctrl Pts',(2.32894830461766,-4.5682459784096,6.95867287109761));
#54756=CARTESIAN_POINT('Ctrl Pts',(4.2330732788251,-2.89377990540639,7.09784632851956));
#54757=CARTESIAN_POINT('Ctrl Pts',(5.10206348419584,-0.51168323020428,7.23701978594152));
#54758=CARTESIAN_POINT('Ctrl Pts',(4.72342036091109,1.9955379272185,7.37619324336347));
#54759=CARTESIAN_POINT('Ctrl Pts',(3.18973542252992,4.01478012587175,7.51536670078542));
#54760=CARTESIAN_POINT('Ctrl Pts',(0.876048385964622,5.05226788188094,7.65454015820737));
#54761=CARTESIAN_POINT('Ctrl Pts',(-1.65186318293549,4.85429907913586,7.79371361562932));
#54762=CARTESIAN_POINT('Ctrl Pts',(-3.77583631245843,3.46928402791661,7.93288707305128));
#54763=CARTESIAN_POINT('Ctrl Pts',(-4.77123581750181,1.61770020117239,8.04826901317175));
#54764=CARTESIAN_POINT('Ctrl Pts',(-4.91785500921365,0.39917459312526,8.11725980081823));
#54765=CARTESIAN_POINT('Ctrl Pts',(-4.91782719367126,9.87882777886417E-6,
8.13985943599073));
#54766=CARTESIAN_POINT('Ctrl Pts',(-4.91783496857819,-2.75488291934939E-5,
6.73514056400926));
#54767=CARTESIAN_POINT('Ctrl Pts',(-4.91790898066783,-0.380171218459799,
6.75666337586538));
#54768=CARTESIAN_POINT('Ctrl Pts',(-4.78058891259536,-1.5796395597185,6.82457734019548));
#54769=CARTESIAN_POINT('Ctrl Pts',(-3.81582045786105,-3.42525704588953,
6.93888245699957));
#54770=CARTESIAN_POINT('Ctrl Pts',(-1.70805413921296,-4.83481361115031,
7.07805591442152));
#54771=CARTESIAN_POINT('Ctrl Pts',(0.817391276888771,-5.06208880774656,
7.21722937184347));
#54772=CARTESIAN_POINT('Ctrl Pts',(3.1429558795201,-4.05150588503051,7.35640282926542));
#54773=CARTESIAN_POINT('Ctrl Pts',(4.69995762166771,-2.05018778446619,7.49557628668737));
#54774=CARTESIAN_POINT('Ctrl Pts',(5.10765501073841,0.452473080222043,7.63474974410933));
#54775=CARTESIAN_POINT('Ctrl Pts',(4.26635174695346,2.84448841943749,7.77392320153127));
#54776=CARTESIAN_POINT('Ctrl Pts',(2.3817759625982,4.5409266522414,7.91309665895324));
#54777=CARTESIAN_POINT('Ctrl Pts',(-0.085227516263993,5.12694917738788,
8.05227011637518));
#54778=CARTESIAN_POINT('Ctrl Pts',(-2.53138988051854,4.45925294975012,8.19144357379713));
#54779=CARTESIAN_POINT('Ctrl Pts',(-4.35853870396961,2.70111309704827,8.33061703121909));
#54780=CARTESIAN_POINT('Ctrl Pts',(-4.89408458761665,0.999753759990778,
8.42851602795646));
#54781=CARTESIAN_POINT('Ctrl Pts',(-4.91862044827915,0.0904221571445439,
8.48002387221985));
#54782=CARTESIAN_POINT('Ctrl Pts',(-4.91854624166208,8.68734550606501E-5,
8.48514056400926));
#54783=CARTESIAN_POINT('Origin',(0.,0.,-3.23514056400933));
#54784=CARTESIAN_POINT('',(-4.91799513380959,0.000106232428033744,4.63985943599073));
#54785=CARTESIAN_POINT('',(-4.9186575077129,-3.3023661052678E-5,4.98514056400926));
#54786=CARTESIAN_POINT('',(-4.91825,1.47989506776076E-12,-3.23514056400933));
#54787=CARTESIAN_POINT('Ctrl Pts',(-4.91799513380959,0.000106232428033724,
4.63985943599073));
#54788=CARTESIAN_POINT('Ctrl Pts',(-4.91757083151256,-0.541713384096372,
4.67053880810928));
#54789=CARTESIAN_POINT('Ctrl Pts',(-4.69328057951372,-1.90317651775494,
4.74760933270181));
#54790=CARTESIAN_POINT('Ctrl Pts',(-3.46000163130249,-3.78434409590636,
4.87107100976833));
#54791=CARTESIAN_POINT('Ctrl Pts',(-1.22368347336451,-4.9795050237801,5.01024446719028));
#54792=CARTESIAN_POINT('Ctrl Pts',(1.31186817898678,-4.95700246175034,5.14941792461223));
#54793=CARTESIAN_POINT('Ctrl Pts',(3.52662208588147,-3.72233907485736,5.28859138203419));
#54794=CARTESIAN_POINT('Ctrl Pts',(4.87899329888229,-1.57743333117398,5.42776483945614));
#54795=CARTESIAN_POINT('Ctrl Pts',(5.03827966124805,0.953210144664441,5.56693829687808));
#54796=CARTESIAN_POINT('Ctrl Pts',(3.96553007503505,3.25076033395718,5.70611175430005));
#54797=CARTESIAN_POINT('Ctrl Pts',(1.92306940962342,4.75338569554455,5.84528521172199));
#54798=CARTESIAN_POINT('Ctrl Pts',(-0.589649122276164,5.09364166755337,
5.98445866914395));
#54799=CARTESIAN_POINT('Ctrl Pts',(-2.9581777789531,4.18832374022651,6.1236321265659));
#54800=CARTESIAN_POINT('Ctrl Pts',(-4.55557356052274,2.31482287380865,6.25876571551483));
#54801=CARTESIAN_POINT('Ctrl Pts',(-4.91806427523321,0.747621696728937,
6.34750815198977));
#54802=CARTESIAN_POINT('Ctrl Pts',(-4.91859079181753,-7.13374654238812E-5,
6.38985943599073));
#54803=CARTESIAN_POINT('Ctrl Pts',(-4.9186575077129,-3.30236610529425E-5,
4.98514056400926));
#54804=CARTESIAN_POINT('Ctrl Pts',(-4.91866884723753,-0.0313008852961278,
4.98691172703692));
#54805=CARTESIAN_POINT('Ctrl Pts',(-4.91073115346834,-0.881545817767002,
5.03507404253856));
#54806=CARTESIAN_POINT('Ctrl Pts',(-4.45302342878565,-2.54233238183619,
5.12962751051419));
#54807=CARTESIAN_POINT('Ctrl Pts',(-2.69040213352721,-4.36515841143928,
5.26880096793613));
#54808=CARTESIAN_POINT('Ctrl Pts',(-0.269883228865836,-5.12055022822975,
5.40797442535809));
#54809=CARTESIAN_POINT('Ctrl Pts',(2.21663158357308,-4.62378805956254,5.54714788278004));
#54810=CARTESIAN_POINT('Ctrl Pts',(4.16110228982188,-2.99634766518939,5.686321340202));
#54811=CARTESIAN_POINT('Ctrl Pts',(5.08803765633847,-0.636195256763649,
5.82549479762394));
#54812=CARTESIAN_POINT('Ctrl Pts',(4.77076950065945,1.87952918802142,5.9646682550459));
#54813=CARTESIAN_POINT('Ctrl Pts',(3.28688100581895,3.93564287640957,6.10384171246786));
#54814=CARTESIAN_POINT('Ctrl Pts',(0.999234913118859,5.02935395308892,6.2430151698898));
#54815=CARTESIAN_POINT('Ctrl Pts',(-1.53275913499672,4.89321172964454,6.38218862731175));
#54816=CARTESIAN_POINT('Ctrl Pts',(-3.68993985757321,3.56050775094501,6.52136208473371));
#54817=CARTESIAN_POINT('Ctrl Pts',(-4.75073997281743,1.69788071323429,6.63901273029954));
#54818=CARTESIAN_POINT('Ctrl Pts',(-4.91774945197063,0.439206057044297,
6.71027222339139));
#54819=CARTESIAN_POINT('Ctrl Pts',(-4.91783496857819,-2.75488291934939E-5,
6.73514056400926));
#54820=CARTESIAN_POINT('Origin',(0.,0.,-3.23514056400933));
#54821=CARTESIAN_POINT('',(-4.91823729647676,-0.000128872636838075,2.88985943599072));
#54822=CARTESIAN_POINT('',(-4.91791055468647,8.03577796647248E-5,3.23514056400926));
#54823=CARTESIAN_POINT('',(-4.91825,1.47989506776076E-12,-3.23514056400933));
#54824=CARTESIAN_POINT('Ctrl Pts',(-4.91823729647676,-0.000128872636838643,
2.88985943599072));
#54825=CARTESIAN_POINT('Ctrl Pts',(-4.91843583389124,-0.193092987687688,
2.90078715928082));
#54826=CARTESIAN_POINT('Ctrl Pts',(-4.86000879587966,-1.20512267208922,
2.95810603504489));
#54827=CARTESIAN_POINT('Ctrl Pts',(-4.18104701653603,-2.96845369999834,
3.06181606328295));
#54828=CARTESIAN_POINT('Ctrl Pts',(-2.24750313966228,-4.60886115685302,
3.2009895207049));
#54829=CARTESIAN_POINT('Ctrl Pts',(0.235634020762259,-5.12224053832399,
3.34016297812685));
#54830=CARTESIAN_POINT('Ctrl Pts',(2.66115040510108,-4.38305259454633,3.47933643554881));
#54831=CARTESIAN_POINT('Ctrl Pts',(4.43592225278534,-2.57205468293112,3.61850989297076));
#54832=CARTESIAN_POINT('Ctrl Pts',(5.12595564846396,-0.132099261254929,
3.75768335039271));
#54833=CARTESIAN_POINT('Ctrl Pts',(4.56251324399756,2.34015905938081,3.89685680781466));
#54834=CARTESIAN_POINT('Ctrl Pts',(2.88337645366723,4.24016647683272,4.03603026523662));
#54835=CARTESIAN_POINT('Ctrl Pts',(0.499153069686797,5.10330458995647,4.17520372265857));
#54836=CARTESIAN_POINT('Ctrl Pts',(-2.00713073313589,4.71850588056565,4.31437718008052));
#54837=CARTESIAN_POINT('Ctrl Pts',(-4.02260072986122,3.17986711875809,4.45355063750247));
#54838=CARTESIAN_POINT('Ctrl Pts',(-4.82695337161777,1.37422822879704,4.56204472280588));
#54839=CARTESIAN_POINT('Ctrl Pts',(-4.91821243110203,0.277587491633778,
4.62414765563529));
#54840=CARTESIAN_POINT('Ctrl Pts',(-4.91799513380959,0.000106232428033724,
4.63985943599073));
#54841=CARTESIAN_POINT('Ctrl Pts',(-4.91791055468647,8.03577796646554E-5,
3.23514056400926));
#54842=CARTESIAN_POINT('Ctrl Pts',(-4.91762009358936,-0.501697021057008,
3.26355123068244));
#54843=CARTESIAN_POINT('Ctrl Pts',(-4.71657087607217,-1.8230431477797,3.33835304982961));
#54844=CARTESIAN_POINT('Ctrl Pts',(-3.55143600647059,-3.69867190880361,
3.45954602145075));
#54845=CARTESIAN_POINT('Ctrl Pts',(-1.34498830969541,-4.94811863679935,
3.59871947887272));
#54846=CARTESIAN_POINT('Ctrl Pts',(1.19035616522235,-4.98757694646994,3.73789293629466));
#54847=CARTESIAN_POINT('Ctrl Pts',(3.43461684055513,-3.80739789825333,3.87706639371662));
#54848=CARTESIAN_POINT('Ctrl Pts',(4.83899332888966,-1.69617662995569,4.01623985113857));
#54849=CARTESIAN_POINT('Ctrl Pts',(5.06006636109004,0.829819268522708,4.15541330856052));
#54850=CARTESIAN_POINT('Ctrl Pts',(4.04377583306429,3.15289527402549,4.29458676598247));
#54851=CARTESIAN_POINT('Ctrl Pts',(2.03864039580317,4.7049778887521,4.43376022340442));
#54852=CARTESIAN_POINT('Ctrl Pts',(-0.4650140643643,5.1065285191596,4.57293368082638));
#54853=CARTESIAN_POINT('Ctrl Pts',(-2.85495628892523,4.25935396338143,4.71210713824833));
#54854=CARTESIAN_POINT('Ctrl Pts',(-4.52523122535563,2.3946547077534,4.84950943264262));
#54855=CARTESIAN_POINT('Ctrl Pts',(-4.91837183696364,0.787681960436565,
4.94052057456294));
#54856=CARTESIAN_POINT('Ctrl Pts',(-4.9186575077129,-3.30236610529425E-5,
4.98514056400926));
#54857=CARTESIAN_POINT('Origin',(0.,0.,-3.23514056400933));
#54858=CARTESIAN_POINT('',(-4.91835559909507,0.00012341875379533,1.13985943599073));
#54859=CARTESIAN_POINT('',(-4.91836475234218,-0.000121599733085009,1.48514056400926));
#54860=CARTESIAN_POINT('',(-4.91825,1.47989506776076E-12,-3.23514056400933));
#54861=CARTESIAN_POINT('Ctrl Pts',(-4.91835559909507,0.00012341875379537,
1.13985943599073));
#54862=CARTESIAN_POINT('Ctrl Pts',(-4.917672964651,-0.663200925352557,1.17742666292634));
#54863=CARTESIAN_POINT('Ctrl Pts',(-4.6156960583571,-2.14625832956755,1.26138504233594));
#54864=CARTESIAN_POINT('Ctrl Pts',(-3.16997967797153,-4.03039635294118,
1.39173457421952));
#54865=CARTESIAN_POINT('Ctrl Pts',(-0.85122519685208,-5.05650975620884,
1.53090803164147));
#54866=CARTESIAN_POINT('Ctrl Pts',(1.67568359580848,-4.84612774610485,1.67008148906343));
#54867=CARTESIAN_POINT('Ctrl Pts',(3.79282906492235,-3.45069846869191,1.80925494648538));
#54868=CARTESIAN_POINT('Ctrl Pts',(4.98249488295983,-1.21145207040314,1.94842840390733));
#54869=CARTESIAN_POINT('Ctrl Pts',(4.95376609667662,1.32403660424732,2.08760186132928));
#54870=CARTESIAN_POINT('Ctrl Pts',(3.71366788460521,3.5357520353937,2.22677531875123));
#54871=CARTESIAN_POINT('Ctrl Pts',(1.56544772852549,4.88285212444658,2.36594877617319));
#54872=CARTESIAN_POINT('Ctrl Pts',(-0.965579261288932,5.03592377327551,
2.50512223359514));
#54873=CARTESIAN_POINT('Ctrl Pts',(-3.26048828129931,3.9575355560864,2.6442956910171));
#54874=CARTESIAN_POINT('Ctrl Pts',(-4.64050357659391,2.07205186532311,2.77254142514895));
#54875=CARTESIAN_POINT('Ctrl Pts',(-4.91759298865968,0.62609207453369,2.85439600680683));
#54876=CARTESIAN_POINT('Ctrl Pts',(-4.91823729647676,-0.000128872636838643,
2.88985943599072));
#54877=CARTESIAN_POINT('Ctrl Pts',(-4.91836475234218,-0.000121599733084975,
1.48514056400926));
#54878=CARTESIAN_POINT('Ctrl Pts',(-4.91852158624276,-0.153013008821408,
1.49379958185398));
#54879=CARTESIAN_POINT('Ctrl Pts',(-4.87409834135891,-1.12493756164979,
1.54884975217269));
#54880=CARTESIAN_POINT('Ctrl Pts',(-4.25233049755791,-2.86540695615602,
1.65029107496538));
#54881=CARTESIAN_POINT('Ctrl Pts',(-2.35944592257799,-4.55256921648261,
1.78946453238733));
#54882=CARTESIAN_POINT('Ctrl Pts',(0.110405866233583,-5.12646878239007,
1.92863798980928));
#54883=CARTESIAN_POINT('Ctrl Pts',(2.55325955316838,-4.44676705445871,2.06781144723124));
#54884=CARTESIAN_POINT('Ctrl Pts',(4.37175179702231,-2.67967494785925,2.20698490465319));
#54885=CARTESIAN_POINT('Ctrl Pts',(5.12119751466329,-0.257308400894945,
2.34615836207514));
#54886=CARTESIAN_POINT('Ctrl Pts',(4.61833096239999,2.22797906576163,2.48533181949709));
#54887=CARTESIAN_POINT('Ctrl Pts',(2.98612063605357,4.1684475701488,2.62450527691905));
#54888=CARTESIAN_POINT('Ctrl Pts',(0.623699162634292,5.08958455582901,2.763678734341));
#54889=CARTESIAN_POINT('Ctrl Pts',(-1.8912386141611,4.76613974843824,2.90285219176295));
#54890=CARTESIAN_POINT('Ctrl Pts',(-3.94370226951601,3.27720673842359,3.04202564918491));
#54891=CARTESIAN_POINT('Ctrl Pts',(-4.80967135409758,1.45442541578736,3.15278843993367));
#54892=CARTESIAN_POINT('Ctrl Pts',(-4.91809438112364,0.317644219941786,
3.21716007820846));
#54893=CARTESIAN_POINT('Ctrl Pts',(-4.91791055468647,8.03577796646554E-5,
3.23514056400926));
#54894=CARTESIAN_POINT('Origin',(2.3094010767585,4.,91.));
#54895=CARTESIAN_POINT('',(2.3094010767585,4.,91.));
#54896=CARTESIAN_POINT('',(4.61880215351701,0.,91.));
#54897=CARTESIAN_POINT('',(2.88675134594813,3.,91.));
#54898=CARTESIAN_POINT('',(2.3094010767585,4.,86.));
#54899=CARTESIAN_POINT('',(2.3094010767585,4.,91.));
#54900=CARTESIAN_POINT('',(4.61880215351701,0.,86.));
#54901=CARTESIAN_POINT('',(4.61880215351701,0.,86.));
#54902=CARTESIAN_POINT('',(4.61880215351701,0.,91.));
#54903=CARTESIAN_POINT('Origin',(-2.3094010767585,4.,91.));
#54904=CARTESIAN_POINT('',(-2.3094010767585,4.,91.));
#54905=CARTESIAN_POINT('',(-1.15470053837925,4.,91.));
#54906=CARTESIAN_POINT('',(-2.3094010767585,4.,86.));
#54907=CARTESIAN_POINT('',(-2.3094010767585,4.,91.));
#54908=CARTESIAN_POINT('',(2.3094010767585,4.,86.));
#54909=CARTESIAN_POINT('Origin',(-4.61880215351701,5.55111512312578E-16,
91.));
#54910=CARTESIAN_POINT('',(-4.61880215351701,5.6564012731995E-16,91.));
#54911=CARTESIAN_POINT('',(-4.04145188432738,1.,91.));
#54912=CARTESIAN_POINT('',(-4.61880215351701,5.55111512312578E-16,86.));
#54913=CARTESIAN_POINT('',(-4.61880215351701,5.6564012731995E-16,91.));
#54914=CARTESIAN_POINT('',(-2.3094010767585,4.,86.));
#54915=CARTESIAN_POINT('Origin',(-2.30940107675851,-4.,91.));
#54916=CARTESIAN_POINT('',(-2.30940107675851,-4.,91.));
#54917=CARTESIAN_POINT('',(-2.88675134594813,-3.,91.));
#54918=CARTESIAN_POINT('',(-2.30940107675851,-4.,86.));
#54919=CARTESIAN_POINT('',(-2.30940107675851,-4.,91.));
#54920=CARTESIAN_POINT('',(-4.61880215351701,5.6564012731995E-16,86.));
#54921=CARTESIAN_POINT('Origin',(2.3094010767585,-4.,91.));
#54922=CARTESIAN_POINT('',(2.3094010767585,-4.,91.));
#54923=CARTESIAN_POINT('',(1.15470053837925,-4.,91.));
#54924=CARTESIAN_POINT('',(2.3094010767585,-4.,86.));
#54925=CARTESIAN_POINT('',(2.3094010767585,-4.,91.));
#54926=CARTESIAN_POINT('',(-2.30940107675851,-4.,86.));
#54927=CARTESIAN_POINT('Origin',(4.61880215351701,0.,91.));
#54928=CARTESIAN_POINT('',(4.04145188432738,-1.,91.));
#54929=CARTESIAN_POINT('',(2.3094010767585,-4.,86.));
#54930=CARTESIAN_POINT('Origin',(0.,0.,86.));
#54931=CARTESIAN_POINT('Origin',(0.,0.,66.5));
#54932=CARTESIAN_POINT('',(-5.,-6.12323399573677E-16,66.));
#54933=CARTESIAN_POINT('Origin',(0.,0.,66.));
#54934=CARTESIAN_POINT('',(-5.,-6.12323399573677E-16,67.));
#54935=CARTESIAN_POINT('',(-5.,-6.12323399573677E-16,66.5));
#54936=CARTESIAN_POINT('Origin',(0.,0.,67.));
#54937=CARTESIAN_POINT('Origin',(9.,0.,66.));
#54938=CARTESIAN_POINT('Origin',(5.,0.,67.));
#54939=CARTESIAN_POINT('',(-5.91675,-7.2459289488551E-16,67.));
#54940=CARTESIAN_POINT('Origin',(0.,0.,67.));
#54941=CARTESIAN_POINT('Origin',(0.,0.,0.));
#54942=CARTESIAN_POINT('',(-5.91675,7.2459289488551E-16,79.));
#54943=CARTESIAN_POINT('Origin',(0.,0.,79.));
#54944=CARTESIAN_POINT('',(-5.91675,-7.2459289488551E-16,0.));
#54945=CARTESIAN_POINT('Origin',(7.01450167938425E-16,2.84304068604708E-16,
64.));
#54946=CARTESIAN_POINT('Ctrl Pts',(-4.31134524531358,2.36723698448015,64.));
#54947=CARTESIAN_POINT('Ctrl Pts',(-4.37780531290395,2.27027384935843,64.));
#54948=CARTESIAN_POINT('Ctrl Pts',(-4.44067228193355,2.17102449251108,64.));
#54949=CARTESIAN_POINT('Ctrl Pts',(-4.49981011185718,2.0696792768666,64.));
#54950=CARTESIAN_POINT('Ctrl Pts',(-4.57274167435655,1.94469557458442,64.));
#54951=CARTESIAN_POINT('Ctrl Pts',(-4.64000323337925,1.81652518433702,64.));
#54952=CARTESIAN_POINT('Ctrl Pts',(-4.70155965673999,1.68560383988636,64.));
#54953=CARTESIAN_POINT('Ctrl Pts',(-4.7408839899757,1.60196683994773,64.));
#54954=CARTESIAN_POINT('Ctrl Pts',(-4.77787928239261,1.51720632798493,64.));
#54955=CARTESIAN_POINT('Ctrl Pts',(-4.81252800330284,1.4314287333935,64.));
#54956=CARTESIAN_POINT('Ctrl Pts',(-4.83227826388887,1.38253429223898,64.));
#54957=CARTESIAN_POINT('Ctrl Pts',(-4.85126596242407,1.33330929126607,64.));
#54958=CARTESIAN_POINT('Ctrl Pts',(-4.86948683348219,1.28377278855725,64.));
#54959=CARTESIAN_POINT('Ctrl Pts',(-4.87821226202323,1.26005124345768,64.));
#54960=CARTESIAN_POINT('Ctrl Pts',(-4.88676183322489,1.23625825950357,64.));
#54961=CARTESIAN_POINT('Ctrl Pts',(-4.89513501616439,1.2123958965766,64.));
#54962=CARTESIAN_POINT('Ctrl Pts',(-4.90245405282655,1.19153769840151,64.));
#54963=CARTESIAN_POINT('Ctrl Pts',(-4.90963706645259,1.17062994477078,64.));
#54964=CARTESIAN_POINT('Ctrl Pts',(-4.91668120130263,1.1496821616254,64.));
#54965=CARTESIAN_POINT('Ctrl Pts',(-4.96416649792232,1.00847082519322,64.));
#54966=CARTESIAN_POINT('Ctrl Pts',(-5.00538204512764,0.865335696509366,
64.));
#54967=CARTESIAN_POINT('Ctrl Pts',(-5.04029027971585,0.720733498032987,
64.));
#54968=CARTESIAN_POINT('Ctrl Pts',(-5.07541418696244,0.575237907469583,
64.));
#54969=CARTESIAN_POINT('Ctrl Pts',(-5.10415294561491,0.428256357527027,
64.));
#54970=CARTESIAN_POINT('Ctrl Pts',(-5.12642409992174,0.280225006492737,
64.));
#54971=CARTESIAN_POINT('Ctrl Pts',(-5.1422597967598,0.17496869309234,64.));
#54972=CARTESIAN_POINT('Ctrl Pts',(-5.15482469765586,0.069180988940228,
64.));
#54973=CARTESIAN_POINT('Ctrl Pts',(-5.16407425049376,-0.0369871404655844,
64.));
#54974=CARTESIAN_POINT('Ctrl Pts',(-5.16596772707835,-0.0587208253888005,
64.));
#54975=CARTESIAN_POINT('Ctrl Pts',(-5.16772222652803,-0.080470463857156,
64.));
#54976=CARTESIAN_POINT('Ctrl Pts',(-5.16933729871037,-0.10223477637485,
64.));
#54977=CARTESIAN_POINT('Ctrl Pts',(-5.17106601869474,-0.125530578511035,
64.));
#54978=CARTESIAN_POINT('Ctrl Pts',(-5.17263441131894,-0.148835747470043,
64.));
#54979=CARTESIAN_POINT('Ctrl Pts',(-5.17404184458105,-0.172141022243276,
64.));
#54980=CARTESIAN_POINT('Ctrl Pts',(-5.17774276994364,-0.233423560330576,
64.));
#54981=CARTESIAN_POINT('Ctrl Pts',(-5.18033204032176,-0.294723109481203,
64.));
#54982=CARTESIAN_POINT('Ctrl Pts',(-5.18180770735793,-0.356009398655015,
64.));
#54983=CARTESIAN_POINT('Ctrl Pts',(-5.18539797672768,-0.505117755359866,
64.));
#54984=CARTESIAN_POINT('Ctrl Pts',(-5.18239996117048,-0.654146301806263,
64.));
#54985=CARTESIAN_POINT('Ctrl Pts',(-5.17302423201139,-0.802695070252512,
64.));
#54986=CARTESIAN_POINT('Ctrl Pts',(-5.16350202633312,-0.953564608226403,
64.));
#54987=CARTESIAN_POINT('Ctrl Pts',(-5.14740132458846,-1.10393992393194,
64.));
#54988=CARTESIAN_POINT('Ctrl Pts',(-5.12489097487864,-1.25341711880026,
64.));
#54989=CARTESIAN_POINT('Ctrl Pts',(-5.10217125158059,-1.40428463310164,
64.));
#54990=CARTESIAN_POINT('Ctrl Pts',(-5.07292209013945,-1.55423798988641,
64.));
#54991=CARTESIAN_POINT('Ctrl Pts',(-5.03726447997022,-1.70286643658769,
64.));
#54992=CARTESIAN_POINT('Ctrl Pts',(-5.01186088094471,-1.8087540001643,64.));
#54993=CARTESIAN_POINT('Ctrl Pts',(-4.98320351689797,-1.91396921865827,
64.));
#54994=CARTESIAN_POINT('Ctrl Pts',(-4.95132011278482,-2.01836169389923,
64.));
#54995=CARTESIAN_POINT('Ctrl Pts',(-4.94086691439713,-2.05258750146991,
64.));
#54996=CARTESIAN_POINT('Ctrl Pts',(-4.93006684271935,-2.08672484833539,
64.));
#54997=CARTESIAN_POINT('Ctrl Pts',(-4.91892056737488,-2.12076835091139,
64.));
#54998=CARTESIAN_POINT('Ctrl Pts',(-4.91265900654528,-2.13989271807844,
64.));
#54999=CARTESIAN_POINT('Ctrl Pts',(-4.90629102097233,-2.15897878249012,
64.));
#55000=CARTESIAN_POINT('Ctrl Pts',(-4.89981802721649,-2.1780227675418,64.));
#55001=CARTESIAN_POINT('Ctrl Pts',(-4.84938469026562,-2.32640105295769,
64.));
#55002=CARTESIAN_POINT('Ctrl Pts',(-4.79256264059072,-2.47228090596256,
64.));
#55003=CARTESIAN_POINT('Ctrl Pts',(-4.72954803993235,-2.61523817290472,
64.));
#55004=CARTESIAN_POINT('Ctrl Pts',(-4.68330907578958,-2.72013760686169,
64.));
#55005=CARTESIAN_POINT('Ctrl Pts',(-4.63373470382308,-2.82346372059285,
64.));
#55006=CARTESIAN_POINT('Ctrl Pts',(-4.58088461958618,-2.92504945063106,
64.));
#55007=CARTESIAN_POINT('Ctrl Pts',(-4.50929622970348,-3.06265299381362,
64.));
#55008=CARTESIAN_POINT('Ctrl Pts',(-4.43169950814481,-3.19706421366866,
64.));
#55009=CARTESIAN_POINT('Ctrl Pts',(-4.34843690979793,-3.3280078311807,64.));
#55010=CARTESIAN_POINT('Ctrl Pts',(-4.26448354412519,-3.46003778967061,
64.));
#55011=CARTESIAN_POINT('Ctrl Pts',(-4.17476954614258,-3.58854300641687,
64.));
#55012=CARTESIAN_POINT('Ctrl Pts',(-4.07959689883012,-3.71322134423231,
64.));
#55013=CARTESIAN_POINT('Ctrl Pts',(-4.03277217929074,-3.77456279438319,
64.));
#55014=CARTESIAN_POINT('Ctrl Pts',(-3.98462541634808,-3.83497754023627,
64.));
#55015=CARTESIAN_POINT('Ctrl Pts',(-3.93518868011867,-3.89442711707548,
64.));
#55016=CARTESIAN_POINT('Ctrl Pts',(-3.92030576236725,-3.91232439812471,
64.));
#55017=CARTESIAN_POINT('Ctrl Pts',(-3.90530591656096,-3.93013419211438,
64.));
#55018=CARTESIAN_POINT('Ctrl Pts',(-3.89018997578744,-3.94785541510478,
64.));
#55019=CARTESIAN_POINT('Ctrl Pts',(-3.87616481471958,-3.96429785891188,
64.));
#55020=CARTESIAN_POINT('Ctrl Pts',(-3.86204436309214,-3.98065855108264,
64.));
#55021=CARTESIAN_POINT('Ctrl Pts',(-3.84783458724206,-3.99693104286356,
64.));
#55022=CARTESIAN_POINT('Ctrl Pts',(-3.74279515441396,-4.11721818358982,
64.));
#55023=CARTESIAN_POINT('Ctrl Pts',(-3.63279501364812,-4.23278568191491,
64.));
#55024=CARTESIAN_POINT('Ctrl Pts',(-3.51822087870055,-4.34336190163689,
64.));
#55025=CARTESIAN_POINT('Ctrl Pts',(-3.39739720559283,-4.45996959002389,
64.));
#55026=CARTESIAN_POINT('Ctrl Pts',(-3.2714868962383,-4.57102756026343,64.));
#55027=CARTESIAN_POINT('Ctrl Pts',(-3.14088626174176,-4.67619358286374,
64.));
#55028=CARTESIAN_POINT('Ctrl Pts',(-3.01028562724523,-4.78135960546406,
64.));
#55029=CARTESIAN_POINT('Ctrl Pts',(-2.87499408109108,-4.88063446711579,
64.));
#55030=CARTESIAN_POINT('Ctrl Pts',(-2.73535787325043,-4.97364013837371,
64.));
#55031=CARTESIAN_POINT('Ctrl Pts',(-2.63476045962855,-5.04064374814942,
64.));
#55032=CARTESIAN_POINT('Ctrl Pts',(-2.5319070344886,-5.10439284622974,64.));
#55033=CARTESIAN_POINT('Ctrl Pts',(-2.42697062082297,-5.16484032452088,
64.));
#55034=CARTESIAN_POINT('Ctrl Pts',(-2.38106093984425,-5.19128609627326,
64.));
#55035=CARTESIAN_POINT('Ctrl Pts',(-2.33475243107453,-5.21709974137731,
64.));
#55036=CARTESIAN_POINT('Ctrl Pts',(-2.28805902581717,-5.24227646698602,
64.));
#55037=CARTESIAN_POINT('Ctrl Pts',(-2.25858405339635,-5.25816914581022,
64.));
#55038=CARTESIAN_POINT('Ctrl Pts',(-2.2289557048792,-5.27380802074749,64.));
#55039=CARTESIAN_POINT('Ctrl Pts',(-2.19917742481413,-5.28919177522327,
64.));
#55040=CARTESIAN_POINT('Ctrl Pts',(-2.18038129925631,-5.2989020398875,64.));
#55041=CARTESIAN_POINT('Ctrl Pts',(-2.16152483404981,-5.30851090345271,
64.));
#55042=CARTESIAN_POINT('Ctrl Pts',(-2.14262330943649,-5.31801094329774,
64.));
#55043=CARTESIAN_POINT('Ctrl Pts',(-1.99828519502283,-5.39055629961888,
64.));
#55044=CARTESIAN_POINT('Ctrl Pts',(-1.85112559185448,-5.45686153661499,
64.));
#55045=CARTESIAN_POINT('Ctrl Pts',(-1.70160748689977,-5.51689175397447,
64.));
#55046=CARTESIAN_POINT('Ctrl Pts',(-1.54897259072225,-5.57817333587356,
64.));
#55047=CARTESIAN_POINT('Ctrl Pts',(-1.3938793092164,-5.63291598043752,64.));
#55048=CARTESIAN_POINT('Ctrl Pts',(-1.23678212836632,-5.6810439753599,64.));
#55049=CARTESIAN_POINT('Ctrl Pts',(-1.07907796720142,-5.72935792362245,
64.));
#55050=CARTESIAN_POINT('Ctrl Pts',(-0.919353717236846,-5.77100635051268,
64.));
#55051=CARTESIAN_POINT('Ctrl Pts',(-0.758040484974843,-5.80586855253193,
64.));
#55052=CARTESIAN_POINT('Ctrl Pts',(-0.597977648513776,-5.84046052531825,
64.));
#55053=CARTESIAN_POINT('Ctrl Pts',(-0.436349656242937,-5.86837132847252,
64.));
#55054=CARTESIAN_POINT('Ctrl Pts',(-0.273559922641045,-5.88943535634351,
64.));
#55055=CARTESIAN_POINT('Ctrl Pts',(-0.18886669624301,-5.90039415848576,
64.));
#55056=CARTESIAN_POINT('Ctrl Pts',(-0.10385879111916,-5.9094989197477,64.));
#55057=CARTESIAN_POINT('Ctrl Pts',(-0.018592070832216,-5.91672078920428,
64.));
#55058=CARTESIAN_POINT('Ctrl Pts',(4.63776713187094,-3.67456288307058,64.));
#55059=CARTESIAN_POINT('Ctrl Pts',(4.71578553900881,-3.55794368649718,64.));
#55060=CARTESIAN_POINT('Ctrl Pts',(4.78951444896037,-3.43867724387658,64.));
#55061=CARTESIAN_POINT('Ctrl Pts',(4.85875509456031,-3.31693895956287,64.));
#55062=CARTESIAN_POINT('Ctrl Pts',(4.94085947644668,-3.17258376906917,64.));
#55063=CARTESIAN_POINT('Ctrl Pts',(5.01665430968009,-3.02475279858741,64.));
#55064=CARTESIAN_POINT('Ctrl Pts',(5.08600617178006,-2.87388851250663,64.));
#55065=CARTESIAN_POINT('Ctrl Pts',(5.15507978373619,-2.72362951672421,64.));
#55066=CARTESIAN_POINT('Ctrl Pts',(5.21776212770692,-2.57036072742675,64.));
#55067=CARTESIAN_POINT('Ctrl Pts',(5.2738704289044,-2.41451223998073,64.));
#55068=CARTESIAN_POINT('Ctrl Pts',(5.28458676255205,-2.3847461562764,64.));
#55069=CARTESIAN_POINT('Ctrl Pts',(5.29506313174358,-2.35488596754356,64.));
#55070=CARTESIAN_POINT('Ctrl Pts',(5.30529804539234,-2.3249346767927,64.));
#55071=CARTESIAN_POINT('Ctrl Pts',(5.31418295674338,-2.29893401158895,64.));
#55072=CARTESIAN_POINT('Ctrl Pts',(5.32288630842342,-2.27286324727078,64.));
#55073=CARTESIAN_POINT('Ctrl Pts',(5.33140150285065,-2.24674211170248,64.));
#55074=CARTESIAN_POINT('Ctrl Pts',(5.38204436598286,-2.09139050995696,64.));
#55075=CARTESIAN_POINT('Ctrl Pts',(5.42608483565498,-1.93411836332475,64.));
#55076=CARTESIAN_POINT('Ctrl Pts',(5.46339533915538,-1.77535137306523,64.));
#55077=CARTESIAN_POINT('Ctrl Pts',(5.50043436992127,-1.61773957785674,64.));
#55078=CARTESIAN_POINT('Ctrl Pts',(5.53084106778903,-1.45865387817275,64.));
#55079=CARTESIAN_POINT('Ctrl Pts',(5.55443968683482,-1.29850913579728,64.));
#55080=CARTESIAN_POINT('Ctrl Pts',(5.5724596467274,-1.17622224142378,64.));
#55081=CARTESIAN_POINT('Ctrl Pts',(5.58650888091475,-1.05331771709944,64.));
#55082=CARTESIAN_POINT('Ctrl Pts',(5.59648856647768,-0.929983589607728,
64.));
#55083=CARTESIAN_POINT('Ctrl Pts',(5.59871377260605,-0.902483338763021,
64.));
#55084=CARTESIAN_POINT('Ctrl Pts',(5.60073658073746,-0.8749617478155,64.));
#55085=CARTESIAN_POINT('Ctrl Pts',(5.60255577183255,-0.847420936734302,
64.));
#55086=CARTESIAN_POINT('Ctrl Pts',(5.60426136527795,-0.821599885285683,
64.));
#55087=CARTESIAN_POINT('Ctrl Pts',(5.60578799465812,-0.795760150203196,
64.));
#55088=CARTESIAN_POINT('Ctrl Pts',(5.60713372452998,-0.769924994464162,
64.));
#55089=CARTESIAN_POINT('Ctrl Pts',(5.6107899878593,-0.699732503006053,64.));
#55090=CARTESIAN_POINT('Ctrl Pts',(5.61311362363577,-0.629538426216335,
64.));
#55091=CARTESIAN_POINT('Ctrl Pts',(5.61409507354281,-0.559376451480223,
64.));
#55092=CARTESIAN_POINT('Ctrl Pts',(5.6163226971518,-0.400127904759795,64.));
#55093=CARTESIAN_POINT('Ctrl Pts',(5.61163937877799,-0.241044294874839,
64.));
#55094=CARTESIAN_POINT('Ctrl Pts',(5.60017586715559,-0.0825479907627651,
64.));
#55095=CARTESIAN_POINT('Ctrl Pts',(5.5886705938214,0.0765257173061029,64.));
#55096=CARTESIAN_POINT('Ctrl Pts',(5.57033540063889,0.235008590310874,64.));
#55097=CARTESIAN_POINT('Ctrl Pts',(5.54525152574663,0.392461691483428,64.));
#55098=CARTESIAN_POINT('Ctrl Pts',(5.52050581985309,0.547792084031498,64.));
#55099=CARTESIAN_POINT('Ctrl Pts',(5.48919182491573,0.702120940243903,64.));
#55100=CARTESIAN_POINT('Ctrl Pts',(5.45134258839387,0.855004798823976,64.));
#55101=CARTESIAN_POINT('Ctrl Pts',(5.42448368941834,0.96349555028783,64.));
#55102=CARTESIAN_POINT('Ctrl Pts',(5.39433288585167,1.07125820303177,64.));
#55103=CARTESIAN_POINT('Ctrl Pts',(5.36088933597902,1.17812470068103,64.));
#55104=CARTESIAN_POINT('Ctrl Pts',(5.34772509504774,1.22019010127083,64.));
#55105=CARTESIAN_POINT('Ctrl Pts',(5.33405056167791,1.26211655112641,64.));
#55106=CARTESIAN_POINT('Ctrl Pts',(5.31986526294901,1.30389338831185,64.));
#55107=CARTESIAN_POINT('Ctrl Pts',(5.31288626186537,1.32444710364491,64.));
#55108=CARTESIAN_POINT('Ctrl Pts',(5.30578589639194,1.34495781344142,64.));
#55109=CARTESIAN_POINT('Ctrl Pts',(5.29856707862928,1.36541680688513,64.));
#55110=CARTESIAN_POINT('Ctrl Pts',(5.24687903771558,1.51190690054584,64.));
#55111=CARTESIAN_POINT('Ctrl Pts',(5.1890807996147,1.65586906246907,64.));
#55112=CARTESIAN_POINT('Ctrl Pts',(5.12526319108892,1.79690248233301,64.));
#55113=CARTESIAN_POINT('Ctrl Pts',(5.07803955192826,1.90126413867048,64.));
#55114=CARTESIAN_POINT('Ctrl Pts',(5.02751886787974,2.00402182099969,64.));
#55115=CARTESIAN_POINT('Ctrl Pts',(4.97372199207057,2.10500394192546,64.));
#55116=CARTESIAN_POINT('Ctrl Pts',(4.90071000480305,2.24205475047863,64.));
#55117=CARTESIAN_POINT('Ctrl Pts',(4.82166453854399,2.37583674945006,64.));
#55118=CARTESIAN_POINT('Ctrl Pts',(4.73686704330111,2.50599898911507,64.));
#55119=CARTESIAN_POINT('Ctrl Pts',(4.6526636823959,2.63524924599295,64.));
#55120=CARTESIAN_POINT('Ctrl Pts',(4.56278799724779,2.76093077356813,64.));
#55121=CARTESIAN_POINT('Ctrl Pts',(4.4674852282392,2.88265881474064,64.));
#55122=CARTESIAN_POINT('Ctrl Pts',(4.42323218722205,2.93918220912867,64.));
#55123=CARTESIAN_POINT('Ctrl Pts',(4.37780862316338,2.99485255318148,64.));
#55124=CARTESIAN_POINT('Ctrl Pts',(4.33123740110862,3.04962783433613,64.));
#55125=CARTESIAN_POINT('Ctrl Pts',(4.31630796020963,3.06718726882472,64.));
#55126=CARTESIAN_POINT('Ctrl Pts',(4.30126057146792,3.08465470260554,64.));
#55127=CARTESIAN_POINT('Ctrl Pts',(4.28609596941756,3.1020286992127,64.));
#55128=CARTESIAN_POINT('Ctrl Pts',(4.27208612364491,3.11807969825063,64.));
#55129=CARTESIAN_POINT('Ctrl Pts',(4.25798072796444,3.13404575090414,64.));
#55130=CARTESIAN_POINT('Ctrl Pts',(4.24378617175793,3.14991972152872,64.));
#55131=CARTESIAN_POINT('Ctrl Pts',(4.14263165658703,3.26304222983437,64.));
#55132=CARTESIAN_POINT('Ctrl Pts',(4.0368652620674,3.37159127598299,64.));
#55133=CARTESIAN_POINT('Ctrl Pts',(3.92677488831619,3.47526252928417,64.));
#55134=CARTESIAN_POINT('Ctrl Pts',(3.81533679383097,3.58020292077459,64.));
#55135=CARTESIAN_POINT('Ctrl Pts',(3.69946764495016,3.68014597296354,64.));
#55136=CARTESIAN_POINT('Ctrl Pts',(3.57943412821498,3.77473182718883,64.));
#55137=CARTESIAN_POINT('Ctrl Pts',(3.4594006114798,3.86931768141412,64.));
#55138=CARTESIAN_POINT('Ctrl Pts',(3.33520211173227,3.9585468624312,64.));
#55139=CARTESIAN_POINT('Ctrl Pts',(3.20708253874238,4.04200713373791,64.));
#55140=CARTESIAN_POINT('Ctrl Pts',(3.11885047720282,4.09948368960047,64.));
#55141=CARTESIAN_POINT('Ctrl Pts',(3.02875820280347,4.15422301877539,64.));
#55142=CARTESIAN_POINT('Ctrl Pts',(2.93694146408057,4.20615325321952,64.));
#55143=CARTESIAN_POINT('Ctrl Pts',(2.88917182567783,4.23317107759523,64.));
#55144=CARTESIAN_POINT('Ctrl Pts',(2.84093538421679,4.2594283266899,64.));
#55145=CARTESIAN_POINT('Ctrl Pts',(2.79225122260655,4.28491353726207,64.));
#55146=CARTESIAN_POINT('Ctrl Pts',(2.76158313515809,4.30096768383909,64.));
#55147=CARTESIAN_POINT('Ctrl Pts',(2.73073738177846,4.31671544847069,64.));
#55148=CARTESIAN_POINT('Ctrl Pts',(2.69971874557491,4.33215377415929,64.));
#55149=CARTESIAN_POINT('Ctrl Pts',(2.6819646151136,4.34099020547693,64.));
#55150=CARTESIAN_POINT('Ctrl Pts',(2.6641624621708,4.34972096085384,64.));
#55151=CARTESIAN_POINT('Ctrl Pts',(2.6463156374621,4.35834466861521,64.));
#55152=CARTESIAN_POINT('Ctrl Pts',(2.51371120616726,4.42242003675576,64.));
#55153=CARTESIAN_POINT('Ctrl Pts',(2.37859978023243,4.48061070952557,64.));
#55154=CARTESIAN_POINT('Ctrl Pts',(2.24138104291238,4.53280614111679,64.));
#55155=CARTESIAN_POINT('Ctrl Pts',(2.10421785117505,4.58498044421114,64.));
#55156=CARTESIAN_POINT('Ctrl Pts',(1.96494827442017,4.63116450492661,64.));
#55157=CARTESIAN_POINT('Ctrl Pts',(1.82395999692009,4.67119766109615,64.));
#55158=CARTESIAN_POINT('Ctrl Pts',(1.68432383228183,4.71084688928022,64.));
#55159=CARTESIAN_POINT('Ctrl Pts',(1.54300104255641,4.74446268902098,64.));
#55160=CARTESIAN_POINT('Ctrl Pts',(1.40036822577045,4.77183822748119,64.));
#55161=CARTESIAN_POINT('Ctrl Pts',(1.26083360159048,4.79861912935809,64.));
#55162=CARTESIAN_POINT('Ctrl Pts',(1.12004462305474,4.81942787543702,64.));
#55163=CARTESIAN_POINT('Ctrl Pts',(0.978363735010218,4.83402204168757,64.));
#55164=CARTESIAN_POINT('Ctrl Pts',(0.931389872203962,4.8388606926354,64.));
#55165=CARTESIAN_POINT('Ctrl Pts',(0.884318089179114,4.84301581405944,64.));
#55166=CARTESIAN_POINT('Ctrl Pts',(0.837162017642518,4.84647736182856,64.));
#55167=CARTESIAN_POINT('Ctrl Pts',(-2.14786219406452,4.42446279878228,-0.576484243785856));
#55168=CARTESIAN_POINT('Ctrl Pts',(-2.8848113557746,4.06670970753236,-0.530093091311872));
#55169=CARTESIAN_POINT('Ctrl Pts',(-4.17573600431334,2.97619823210191,-0.437310786363904));
#55170=CARTESIAN_POINT('Ctrl Pts',(-5.09111818072895,0.611045927560412,
-0.298137328941951));
#55171=CARTESIAN_POINT('Ctrl Pts',(-4.76147221760645,-1.90285915103548,
-0.15896387152));
#55172=CARTESIAN_POINT('Ctrl Pts',(-3.26751735403169,-3.9517774964877,-0.0197904140980472));
#55173=CARTESIAN_POINT('Ctrl Pts',(-0.97452041004599,-5.03418042523659,
0.119383043323905));
#55174=CARTESIAN_POINT('Ctrl Pts',(1.5567708799336,-4.88563546465558,0.258556500745857));
#55175=CARTESIAN_POINT('Ctrl Pts',(3.70738228326065,-3.54233751270576,0.39772995816781));
#55176=CARTESIAN_POINT('Ctrl Pts',(4.95140614815209,-1.33283639810976,0.536903415589762));
#55177=CARTESIAN_POINT('Ctrl Pts',(4.98463903712129,1.20260146313003,0.676076873011714));
#55178=CARTESIAN_POINT('Ctrl Pts',(3.79895229578282,3.44395520585394,0.815250330433666));
#55179=CARTESIAN_POINT('Ctrl Pts',(1.68428893605082,4.84314423609996,0.954423787855619));
#55180=CARTESIAN_POINT('Ctrl Pts',(-0.842242278542283,5.05801321348077,
1.09359724527757));
#55181=CARTESIAN_POINT('Ctrl Pts',(-3.16281564529539,4.03602149408518,1.23277070269952));
#55182=CARTESIAN_POINT('Ctrl Pts',(-4.70996979078121,2.02708066455042,1.37194416012147));
#55183=CARTESIAN_POINT('Ctrl Pts',(-5.10537123237187,-0.477552219033277,
1.51111761754343));
#55184=CARTESIAN_POINT('Ctrl Pts',(-4.25233049755791,-2.86540695615602,
1.65029107496538));
#55185=CARTESIAN_POINT('Ctrl Pts',(-2.35944592257799,-4.55256921648261,
1.78946453238733));
#55186=CARTESIAN_POINT('Ctrl Pts',(0.110405866233583,-5.12646878239007,
1.92863798980928));
#55187=CARTESIAN_POINT('Ctrl Pts',(2.55325955316838,-4.44676705445871,2.06781144723124));
#55188=CARTESIAN_POINT('Ctrl Pts',(4.37175179702231,-2.67967494785925,2.20698490465319));
#55189=CARTESIAN_POINT('Ctrl Pts',(5.12119751466329,-0.257308400894945,
2.34615836207514));
#55190=CARTESIAN_POINT('Ctrl Pts',(4.61833096239999,2.22797906576163,2.48533181949709));
#55191=CARTESIAN_POINT('Ctrl Pts',(2.98612063605357,4.1684475701488,2.62450527691905));
#55192=CARTESIAN_POINT('Ctrl Pts',(0.623699162634292,5.08958455582901,2.763678734341));
#55193=CARTESIAN_POINT('Ctrl Pts',(-1.8912386141611,4.76613974843824,2.90285219176295));
#55194=CARTESIAN_POINT('Ctrl Pts',(-3.94370226951601,3.27720673842359,3.04202564918491));
#55195=CARTESIAN_POINT('Ctrl Pts',(-5.03179250909024,0.986881828040634,
3.18119910660685));
#55196=CARTESIAN_POINT('Ctrl Pts',(-4.88943313614101,-1.54477027556571,
3.32037256402881));
#55197=CARTESIAN_POINT('Ctrl Pts',(-3.55143600647059,-3.69867190880361,
3.45954602145075));
#55198=CARTESIAN_POINT('Ctrl Pts',(-1.34498830969541,-4.94811863679935,
3.59871947887272));
#55199=CARTESIAN_POINT('Ctrl Pts',(1.19035616522235,-4.98757694646994,3.73789293629466));
#55200=CARTESIAN_POINT('Ctrl Pts',(3.43461684055513,-3.80739789825333,3.87706639371662));
#55201=CARTESIAN_POINT('Ctrl Pts',(4.83899332888966,-1.69617662995569,4.01623985113857));
#55202=CARTESIAN_POINT('Ctrl Pts',(5.06006636109004,0.829819268522708,4.15541330856052));
#55203=CARTESIAN_POINT('Ctrl Pts',(4.04377583306429,3.15289527402549,4.29458676598247));
#55204=CARTESIAN_POINT('Ctrl Pts',(2.03864039580317,4.7049778887521,4.43376022340442));
#55205=CARTESIAN_POINT('Ctrl Pts',(-0.4650140643643,5.1065285191596,4.57293368082638));
#55206=CARTESIAN_POINT('Ctrl Pts',(-2.85495628892523,4.25935396338143,4.71210713824833));
#55207=CARTESIAN_POINT('Ctrl Pts',(-4.54676164612823,2.37061809036044,4.85128059567028));
#55208=CARTESIAN_POINT('Ctrl Pts',(-5.12672443517544,-0.0978169863668739,
4.99045405309224));
#55209=CARTESIAN_POINT('Ctrl Pts',(-4.45302342878565,-2.54233238183619,
5.12962751051419));
#55210=CARTESIAN_POINT('Ctrl Pts',(-2.69040213352721,-4.36515841143928,
5.26880096793613));
#55211=CARTESIAN_POINT('Ctrl Pts',(-0.269883228865836,-5.12055022822975,
5.40797442535809));
#55212=CARTESIAN_POINT('Ctrl Pts',(2.21663158357308,-4.62378805956254,5.54714788278004));
#55213=CARTESIAN_POINT('Ctrl Pts',(4.16110228982188,-2.99634766518939,5.686321340202));
#55214=CARTESIAN_POINT('Ctrl Pts',(5.08803765633847,-0.636195256763649,
5.82549479762394));
#55215=CARTESIAN_POINT('Ctrl Pts',(4.77076950065945,1.87952918802142,5.9646682550459));
#55216=CARTESIAN_POINT('Ctrl Pts',(3.28688100581895,3.93564287640957,6.10384171246786));
#55217=CARTESIAN_POINT('Ctrl Pts',(0.999234913118859,5.02935395308892,6.2430151698898));
#55218=CARTESIAN_POINT('Ctrl Pts',(-1.53275913499672,4.89321172964454,6.38218862731175));
#55219=CARTESIAN_POINT('Ctrl Pts',(-3.68993985757321,3.56050775094501,6.52136208473371));
#55220=CARTESIAN_POINT('Ctrl Pts',(-4.94480096744728,1.35713484568753,6.66053554215565));
#55221=CARTESIAN_POINT('Ctrl Pts',(-4.99048494542848,-1.17810509144919,
6.79970899957761));
#55222=CARTESIAN_POINT('Ctrl Pts',(-3.81582045786105,-3.42525704588953,
6.93888245699957));
#55223=CARTESIAN_POINT('Ctrl Pts',(-1.70805413921296,-4.83481361115031,
7.07805591442152));
#55224=CARTESIAN_POINT('Ctrl Pts',(0.817391276888771,-5.06208880774656,
7.21722937184347));
#55225=CARTESIAN_POINT('Ctrl Pts',(3.1429558795201,-4.05150588503051,7.35640282926542));
#55226=CARTESIAN_POINT('Ctrl Pts',(4.69995762166771,-2.05018778446619,7.49557628668737));
#55227=CARTESIAN_POINT('Ctrl Pts',(5.10765501073841,0.452473080222043,7.63474974410933));
#55228=CARTESIAN_POINT('Ctrl Pts',(4.26635174695346,2.84448841943749,7.77392320153127));
#55229=CARTESIAN_POINT('Ctrl Pts',(2.3817759625982,4.5409266522414,7.91309665895324));
#55230=CARTESIAN_POINT('Ctrl Pts',(-0.085227516263993,5.12694917738788,
8.05227011637518));
#55231=CARTESIAN_POINT('Ctrl Pts',(-2.53138988051854,4.45925294975012,8.19144357379713));
#55232=CARTESIAN_POINT('Ctrl Pts',(-4.35853870396961,2.70111309704827,8.33061703121909));
#55233=CARTESIAN_POINT('Ctrl Pts',(-5.11987206507848,0.282456428986481,
8.46979048864104));
#55234=CARTESIAN_POINT('Ctrl Pts',(-4.62921727538704,-2.20527073492236,
8.60896394606299));
#55235=CARTESIAN_POINT('Ctrl Pts',(-3.00655662644843,-4.15373191828816,
8.74813740348495));
#55236=CARTESIAN_POINT('Ctrl Pts',(-0.648687514646424,-5.08646007606358,
8.88731086090689));
#55237=CARTESIAN_POINT('Ctrl Pts',(1.86780842837057,-4.77537048530841,9.02648431832885));
#55238=CARTESIAN_POINT('Ctrl Pts',(3.92755975149067,-3.29653545339913,9.1656577757508));
#55239=CARTESIAN_POINT('Ctrl Pts',(5.0268850702256,-1.01158197284738,9.30483123317275));
#55240=CARTESIAN_POINT('Ctrl Pts',(4.89696081722127,1.52073875193816,9.44400469059471));
#55241=CARTESIAN_POINT('Ctrl Pts',(3.56955802565887,3.68118555610841,9.58317814801665));
#55242=CARTESIAN_POINT('Ctrl Pts',(1.36927319819533,4.9414534810874,9.72235160543861));
#55243=CARTESIAN_POINT('Ctrl Pts',(-1.16584691373595,4.99336285190443,9.86152506286056));
#55244=CARTESIAN_POINT('Ctrl Pts',(-3.41587659702151,3.82422000818044,10.0006985202825));
#55245=CARTESIAN_POINT('Ctrl Pts',(-4.83060473962267,1.71992134895229,10.1398719777045));
#55246=CARTESIAN_POINT('Ctrl Pts',(-5.06408073015179,-0.804958356408661,
10.2790454351264));
#55247=CARTESIAN_POINT('Ctrl Pts',(-4.05921150653168,-3.13299753308037,
10.4182188925484));
#55248=CARTESIAN_POINT('Ctrl Pts',(-2.06172281055525,-4.69490901397279,
10.5573923499703));
#55249=CARTESIAN_POINT('Ctrl Pts',(0.439929367680037,-5.10875070330306,
10.6965658073923));
#55250=CARTESIAN_POINT('Ctrl Pts',(2.83400339776564,-4.27332380454602,10.8357392648142));
#55251=CARTESIAN_POINT('Ctrl Pts',(4.53506427669625,-2.39291947279475,10.9749127222362));
#55252=CARTESIAN_POINT('Ctrl Pts',(5.12714300424288,0.0726375322416105,
11.1140861796581));
#55253=CARTESIAN_POINT('Ctrl Pts',(4.46545558154636,2.52043211499204,11.2532596370801));
#55254=CARTESIAN_POINT('Ctrl Pts',(2.71180777293433,4.35189271463576,11.392433094502));
#55255=CARTESIAN_POINT('Ctrl Pts',(0.295027925902909,5.11916302924455,11.531606551924));
#55256=CARTESIAN_POINT('Ctrl Pts',(-2.19389658855195,4.63461857716327,11.6707800093459));
#55257=CARTESIAN_POINT('Ctrl Pts',(-4.14633649986933,3.01674745825668,11.8099534667679));
#55258=CARTESIAN_POINT('Ctrl Pts',(-5.08485182457936,0.661175860961971,
11.9491269241898));
#55259=CARTESIAN_POINT('Ctrl Pts',(-4.77994267460943,-1.8560764058881,12.0883003816118));
#55260=CARTESIAN_POINT('Ctrl Pts',(-3.30617002296448,-3.91945294349836,
12.2274738390338));
#55261=CARTESIAN_POINT('Ctrl Pts',(-1.02392293276547,-5.02438587538853,
12.3666472964557));
#55262=CARTESIAN_POINT('Ctrl Pts',(1.50870919886821,-4.90068037626382,12.5058207538777));
#55263=CARTESIAN_POINT('Ctrl Pts',(3.67240905719958,-3.57858677603957,12.6449942112996));
#55264=CARTESIAN_POINT('Ctrl Pts',(4.93807619790383,-1.38140329402478,12.7841676687216));
#55265=CARTESIAN_POINT('Ctrl Pts',(4.99621064854467,1.15358170599905,12.9233411261435));
#55266=CARTESIAN_POINT('Ctrl Pts',(3.83259649856215,3.40647555051493,13.0625145835655));
#55267=CARTESIAN_POINT('Ctrl Pts',(1.7317781876149,4.82636673968609,13.2016880409874));
#55268=CARTESIAN_POINT('Ctrl Pts',(-0.792520582052584,5.06604211629452,
13.3408614984094));
#55269=CARTESIAN_POINT('Ctrl Pts',(-3.12302029475477,4.06689265110314,13.4800349558313));
#55270=CARTESIAN_POINT('Ctrl Pts',(-4.68983209611028,2.07324540451455,13.6192084132533));
#55271=CARTESIAN_POINT('Ctrl Pts',(-5.10981559024654,-0.427383002376447,
13.7583818706752));
#55272=CARTESIAN_POINT('Ctrl Pts',(-4.28027009411781,-2.82350128713404,
13.8975553280972));
#55273=CARTESIAN_POINT('Ctrl Pts',(-2.40404855375509,-4.52917455484274,
14.0367287855191));
#55274=CARTESIAN_POINT('Ctrl Pts',(0.06004711021698,-5.12730591457165,14.1759022429411));
#55275=CARTESIAN_POINT('Ctrl Pts',(2.5094591513317,-4.47163128677269,14.315075700363));
#55276=CARTESIAN_POINT('Ctrl Pts',(4.34522048351284,-2.72248609669679,14.454249157785));
#55277=CARTESIAN_POINT('Ctrl Pts',(5.11842312500342,-0.307597643809348,
14.5934226152069));
#55278=CARTESIAN_POINT('Ctrl Pts',(4.63999193232155,2.18250921304762,14.7325960726289));
#55279=CARTESIAN_POINT('Ctrl Pts',(3.02692009916372,4.13891607915956,14.8717695300508));
#55280=CARTESIAN_POINT('Ctrl Pts',(0.673660220405915,5.08321291158352,15.0109429874728));
#55281=CARTESIAN_POINT('Ctrl Pts',(-1.84433319131777,4.78448604099233,15.1501164448947));
#55282=CARTESIAN_POINT('Ctrl Pts',(-3.91132250131647,3.31578465641879,15.2892899023167));
#55283=CARTESIAN_POINT('Ctrl Pts',(-5.02185638364779,1.0362577184575,15.4284633597386));
#55284=CARTESIAN_POINT('Ctrl Pts',(-4.90437038434335,-1.49667054832476,
15.5676368171606));
#55285=CARTESIAN_POINT('Ctrl Pts',(-3.587593947644,-3.66361041376876,15.7068102745826));
#55286=CARTESIAN_POINT('Ctrl Pts',(-1.39352506003175,-4.93466913826148,
15.8459837320045));
#55287=CARTESIAN_POINT('Ctrl Pts',(1.1413095421973,-4.99902831817707,15.9851571894265));
#55288=CARTESIAN_POINT('Ctrl Pts',(3.39705396305783,-3.8409498784962,16.1243306468484));
#55289=CARTESIAN_POINT('Ctrl Pts',(4.82209963689558,-1.74362458370441,16.2635041042704));
#55290=CARTESIAN_POINT('Ctrl Pts',(5.06797295434764,0.780078028819932,16.4026775616923));
#55291=CARTESIAN_POINT('Ctrl Pts',(4.07454927242783,3.11302422470575,16.5418510191143));
#55292=CARTESIAN_POINT('Ctrl Pts',(2.08475549686315,4.68472689869385,16.6810244765362));
#55293=CARTESIAN_POINT('Ctrl Pts',(-0.414834059965531,5.1108496651476,16.8201979339582));
#55294=CARTESIAN_POINT('Ctrl Pts',(-2.81298215087013,4.28719057378289,16.9593713913801));
#55295=CARTESIAN_POINT('Ctrl Pts',(-4.52325752219571,2.41516313837115,17.0985448488021));
#55296=CARTESIAN_POINT('Ctrl Pts',(-5.12743790739186,-0.0474563261099836,
17.237718306224));
#55297=CARTESIAN_POINT('Ctrl Pts',(-4.47778002818978,-2.49847105570419,
17.376891763646));
#55298=CARTESIAN_POINT('Ctrl Pts',(-2.73314800394566,-4.33852205083421,
17.5160652210679));
#55299=CARTESIAN_POINT('Ctrl Pts',(-0.320165506910762,-5.11765235681669,
17.6552386784899));
#55300=CARTESIAN_POINT('Ctrl Pts',(2.17110867707493,-4.64533730846069,17.7944121359119));
#55301=CARTESIAN_POINT('Ctrl Pts',(4.13147070090376,-3.0370744878288,17.9335855933338));
#55302=CARTESIAN_POINT('Ctrl Pts',(5.08154334695868,-0.686140517697928,
18.0727590507557));
#55303=CARTESIAN_POINT('Ctrl Pts',(4.78900055706072,1.83257885547087,18.2119325081777));
#55304=CARTESIAN_POINT('Ctrl Pts',(3.3253792957861,3.90316847397136,18.3511059655996));
#55305=CARTESIAN_POINT('Ctrl Pts',(1.04858625554496,5.01929661025616,18.4902794230216));
#55306=CARTESIAN_POINT('Ctrl Pts',(-1.4846228729006,4.90803081920919,18.6294528804436));
#55307=CARTESIAN_POINT('Ctrl Pts',(-3.6547896788716,3.5965794861591,18.7686263378655));
#55308=CARTESIAN_POINT('Ctrl Pts',(-4.93123232270488,1.40563842312223,18.9077997952874));
#55309=CARTESIAN_POINT('Ctrl Pts',(-5.00181584381112,-1.12903049633163,
19.0469732527094));
#55310=CARTESIAN_POINT('Ctrl Pts',(-3.84928009761185,-3.3876118914622,19.1861467101313));
#55311=CARTESIAN_POINT('Ctrl Pts',(-1.75546046578727,-4.8178034569817,19.3253201675533));
#55312=CARTESIAN_POINT('Ctrl Pts',(0.767630771739118,-5.06987323266825,
19.4644936249752));
#55313=CARTESIAN_POINT('Ctrl Pts',(3.10300938320942,-4.08218132433643,19.6036670823972));
#55314=CARTESIAN_POINT('Ctrl Pts',(4.67959345250773,-2.09625301819547,19.7428405398192));
#55315=CARTESIAN_POINT('Ctrl Pts',(5.11185292177081,0.402282616117053,19.8820139972411));
#55316=CARTESIAN_POINT('Ctrl Pts',(4.29408520181098,2.80244605240401,20.0211874546631));
#55317=CARTESIAN_POINT('Ctrl Pts',(2.4262631596223,4.5173132144347,20.160360912085));
#55318=CARTESIAN_POINT('Ctrl Pts',(-0.0348652558426957,5.12753898190759,
20.299534369507));
#55319=CARTESIAN_POINT('Ctrl Pts',(-2.4874678943674,4.48390176872088,20.4387078269289));
#55320=CARTESIAN_POINT('Ctrl Pts',(-4.33179745699125,2.74379343038994,20.5778812843509));
#55321=CARTESIAN_POINT('Ctrl Pts',(-5.11685072933207,0.33273143942329,20.7170547417728));
#55322=CARTESIAN_POINT('Ctrl Pts',(-4.65065467334822,-2.15969504937878,
20.8562281991948));
#55323=CARTESIAN_POINT('Ctrl Pts',(-3.04721056302127,-4.12400040999737,
20.9954016566167));
#55324=CARTESIAN_POINT('Ctrl Pts',(-0.698616677582171,-5.07984314077225,
21.1345751140387));
#55325=CARTESIAN_POINT('Ctrl Pts',(1.82081346922569,-4.79348619559222,21.2737485714606));
#55326=CARTESIAN_POINT('Ctrl Pts',(3.89499091063157,-3.33495388321102,21.4129220288826));
#55327=CARTESIAN_POINT('Ctrl Pts',(5.01670657064901,-1.06090846968716,21.5520954863046));
#55328=CARTESIAN_POINT('Ctrl Pts',(4.91166165878904,1.47256624524283,21.6912689437265));
#55329=CARTESIAN_POINT('Ctrl Pts',(3.6055433374024,3.6459469056968,21.8304424011485));
#55330=CARTESIAN_POINT('Ctrl Pts',(1.41774331025312,4.92776577195785,21.9696158585704));
#55331=CARTESIAN_POINT('Ctrl Pts',(-1.11674464244417,5.00457320863818,22.1087893159924));
#55332=CARTESIAN_POINT('Ctrl Pts',(-3.37814939266335,3.85758710567824,22.2479627734143));
#55333=CARTESIAN_POINT('Ctrl Pts',(-4.81347822585022,1.76728576249361,22.3871362308363));
#55334=CARTESIAN_POINT('Ctrl Pts',(-5.07174293979774,-0.755178885866551,
22.5263096882582));
#55335=CARTESIAN_POINT('Ctrl Pts',(-4.089788760808,-3.09297583065489,22.6654831456802));
#55336=CARTESIAN_POINT('Ctrl Pts',(-2.10773789918185,-4.67443178850642,
22.8046566031021));
#55337=CARTESIAN_POINT('Ctrl Pts',(0.389728746515864,-5.11282535406657,
22.9438300605241));
#55338=CARTESIAN_POINT('Ctrl Pts',(2.79189305526804,-4.30095393662765,23.083003517946));
#55339=CARTESIAN_POINT('Ctrl Pts',(4.51134166740374,-2.43734855057574,23.222176975368));
#55340=CARTESIAN_POINT('Ctrl Pts',(5.12760913750936,0.0222739753389076,
23.3613504327899));
#55341=CARTESIAN_POINT('Ctrl Pts',(4.48999647145208,2.47644973367009,23.5005238902119));
#55342=CARTESIAN_POINT('Ctrl Pts',(2.75442231183803,4.32504674253304,23.6396973476338));
#55343=CARTESIAN_POINT('Ctrl Pts',(0.345295365574717,5.11601824738336,23.7788708050558));
#55344=CARTESIAN_POINT('Ctrl Pts',(-2.14826839878302,4.65594399492059,23.9180442624777));
#55345=CARTESIAN_POINT('Ctrl Pts',(-4.11650525148601,3.05732826362086,24.0572177198997));
#55346=CARTESIAN_POINT('Ctrl Pts',(-5.07811230327642,0.711088624827749,
24.1963911773216));
#55347=CARTESIAN_POINT('Ctrl Pts',(-4.79794292953853,-1.80903710352717,
24.3355646347436));
#55348=CARTESIAN_POINT('Ctrl Pts',(-3.34450836095903,-3.8867898606076,24.4747380921655));
#55349=CARTESIAN_POINT('Ctrl Pts',(-1.07322428658152,-5.01408628044417,
24.6139115495875));
#55350=CARTESIAN_POINT('Ctrl Pts',(1.46050073805254,-4.91526288118904,24.7530850070094));
#55351=CARTESIAN_POINT('Ctrl Pts',(3.63708214756602,-3.61448544732211,24.8922584644314));
#55352=CARTESIAN_POINT('Ctrl Pts',(4.92426950692363,-1.42983964843226,25.0314319218533));
#55353=CARTESIAN_POINT('Ctrl Pts',(5.0073003960314,1.10445205461833,25.1706053792753));
#55354=CARTESIAN_POINT('Ctrl Pts',(3.86587085260431,3.36866652371991,25.3097788366973));
#55355=CARTESIAN_POINT('Ctrl Pts',(1.77910040251715,4.80912396958221,25.4489522941192));
#55356=CARTESIAN_POINT('Ctrl Pts',(-0.742722446286816,5.07358206446181,
25.5881257515412));
#55357=CARTESIAN_POINT('Ctrl Pts',(-3.08292362754424,4.0973715359699,25.7272992089631));
#55358=CARTESIAN_POINT('Ctrl Pts',(-4.66924193781462,2.11921007056874,25.8664726663851));
#55359=CARTESIAN_POINT('Ctrl Pts',(-5.11376695617113,-0.377172526861437,
26.005646123807));
#55360=CARTESIAN_POINT('Ctrl Pts',(-4.30779673681465,-2.7813232230965,26.144819581229));
#55361=CARTESIAN_POINT('Ctrl Pts',(-2.44841924438686,-4.50534291711108,
26.2839930386509));
#55362=CARTESIAN_POINT('Ctrl Pts',(0.00968256052368256,-5.12764837377413,
26.4231664960729));
#55363=CARTESIAN_POINT('Ctrl Pts',(2.46541664005145,-4.49606409963251,26.5623399534948));
#55364=CARTESIAN_POINT('Ctrl Pts',(4.31826994816623,-2.76503458419805,26.7015134109168));
#55365=CARTESIAN_POINT('Ctrl Pts',(5.11515491599038,-0.357857209604937,
26.8406868683387));
#55366=CARTESIAN_POINT('Ctrl Pts',(4.66120524128334,2.13682879419003,26.9798603257607));
#55367=CARTESIAN_POINT('Ctrl Pts',(3.06742752861815,4.10898527056527,27.1190337831826));
#55368=CARTESIAN_POINT('Ctrl Pts',(0.723556284229189,5.07635084490811,27.2582072406046));
#55369=CARTESIAN_POINT('Ctrl Pts',(-1.79724982938647,4.80237073202571,27.3973806980266));
#55370=CARTESIAN_POINT('Ctrl Pts',(-3.87856537335147,3.35404267141695,27.5365541554485));
#55371=CARTESIAN_POINT('Ctrl Pts',(-5.01143575544194,1.08553363196406,27.6757276128705));
#55372=CARTESIAN_POINT('Ctrl Pts',(-4.91883446469394,-1.44842642408439,
27.8149010702924));
#55373=CARTESIAN_POINT('Ctrl Pts',(-3.62340576199759,-3.62819545793354,
27.9540745277144));
#55374=CARTESIAN_POINT('Ctrl Pts',(-1.44192736471906,-4.92074354868461,
28.0932479851363));
#55375=CARTESIAN_POINT('Ctrl Pts',(1.09215280697808,-5.0099973895459,28.2324214425583));
#55376=CARTESIAN_POINT('Ctrl Pts',(3.35916334181333,-3.8741312884393,28.3715948999802));
#55377=CARTESIAN_POINT('Ctrl Pts',(4.80474071443369,-1.79090431461596,28.5107683574022));
#55378=CARTESIAN_POINT('Ctrl Pts',(5.0753905955706,0.730261528111896,28.6499418148241));
#55379=CARTESIAN_POINT('Ctrl Pts',(4.10492960409817,3.07285283449196,28.7891152722461));
#55380=CARTESIAN_POINT('Ctrl Pts',(2.1306694631793,4.66402393172698,28.928288729668));
#55381=CARTESIAN_POINT('Ctrl Pts',(-0.36461403286742,5.11467772240667,29.06746218709));
#55382=CARTESIAN_POINT('Ctrl Pts',(-2.77073661962518,4.31461356111005,29.2066356445119));
#55383=CARTESIAN_POINT('Ctrl Pts',(-4.49931699972899,2.45947517429971,29.3458091019339));
#55384=CARTESIAN_POINT('Ctrl Pts',(-5.12765669046533,0.00290891267710508,
29.4849825593558));
#55385=CARTESIAN_POINT('Ctrl Pts',(-4.50210461667452,-2.45436868004072,
29.6241560167778));
#55386=CARTESIAN_POINT('Ctrl Pts',(-2.77563018347832,-4.31146711475466,
29.7633294741997));
#55387=CARTESIAN_POINT('Ctrl Pts',(-0.370416895766376,-5.11426074035902,
29.9025029316217));
#55388=CARTESIAN_POINT('Ctrl Pts',(2.1253763045803,-4.66643838071129,30.0416763890436));
#55389=CARTESIAN_POINT('Ctrl Pts',(4.10144051258044,-3.07750829711484,30.1808498464656));
#55390=CARTESIAN_POINT('Ctrl Pts',(5.07455877628885,-0.736019580606846,
30.3200233038876));
#55391=CARTESIAN_POINT('Ctrl Pts',(4.8067695763542,1.7854517178805,30.4591967613095));
#55392=CARTESIAN_POINT('Ctrl Pts',(3.36355675709311,3.87031749845671,30.5983702187315));
#55393=CARTESIAN_POINT('Ctrl Pts',(1.09783643160968,5.00875501162488,30.7375436761534));
#55394=CARTESIAN_POINT('Ctrl Pts',(-1.43634337614621,4.92237638776717,30.8767171335754));
#55395=CARTESIAN_POINT('Ctrl Pts',(-3.61928689038582,3.63230422763955,31.0158905909973));
#55396=CARTESIAN_POINT('Ctrl Pts',(-4.91718791850219,1.45400638622494,31.1550640484193));
#55397=CARTESIAN_POINT('Ctrl Pts',(-5.0126641729189,-1.07984697368752,31.2942375058412));
#55398=CARTESIAN_POINT('Ctrl Pts',(-3.882368363373,-3.34963990424751,31.4334109632632));
#55399=CARTESIAN_POINT('Ctrl Pts',(-1.80269742761279,-4.80032848683557,
31.5725844206851));
#55400=CARTESIAN_POINT('Ctrl Pts',(0.717796206480772,-5.07716852221872,
31.7117578781071));
#55401=CARTESIAN_POINT('Ctrl Pts',(3.06276351222464,-4.1124629196179,31.850931335529));
#55402=CARTESIAN_POINT('Ctrl Pts',(4.65877780170794,-2.14211600791371,31.990104792951));
#55403=CARTESIAN_POINT('Ctrl Pts',(5.11555764728126,0.352053340261175,32.1292782503729));
#55404=CARTESIAN_POINT('Ctrl Pts',(4.32140436840864,2.760133308691,32.2684517077949));
#55405=CARTESIAN_POINT('Ctrl Pts',(2.47051627364734,4.49326395159359,32.4076251652168));
#55406=CARTESIAN_POINT('Ctrl Pts',(0.0155003683372346,5.12763408753279,
32.5467986226388));
#55407=CARTESIAN_POINT('Ctrl Pts',(-2.44330592025679,4.50811798615397,32.6859720800608));
#55408=CARTESIAN_POINT('Ctrl Pts',(-4.30463828331925,2.78620904578768,32.8251455374827));
#55409=CARTESIAN_POINT('Ctrl Pts',(-5.11333572588113,0.382974348324482,
32.9643189949047));
#55410=CARTESIAN_POINT('Ctrl Pts',(-4.67164338164879,-2.113910999012,33.1034924523266));
#55411=CARTESIAN_POINT('Ctrl Pts',(-3.0875705083242,-4.0938710230262,33.2426659097486));
#55412=CARTESIAN_POINT('Ctrl Pts',(-0.748478438807404,-5.07273610822475,
33.3818393671704));
#55413=CARTESIAN_POINT('Ctrl Pts',(1.77364284015155,-4.81113943599913,33.5210128245925));
#55414=CARTESIAN_POINT('Ctrl Pts',(3.86204628565767,-3.37305056061788,33.6601862820144));
#55415=CARTESIAN_POINT('Ctrl Pts',(5.00604406515782,-1.11013261133297,33.7993597394364));
#55416=CARTESIAN_POINT('Ctrl Pts',(4.92588862905106,1.42425166709831,33.9385331968583));
#55417=CARTESIAN_POINT('Ctrl Pts',(3.64118079059058,3.61035649864124,34.0777066542803));
#55418=CARTESIAN_POINT('Ctrl Pts',(1.4660766401138,4.91360263781672,34.2168801117022));
#55419=CARTESIAN_POINT('Ctrl Pts',(-1.06753462895041,5.01530073006979,34.3560535691242));
#55420=CARTESIAN_POINT('Ctrl Pts',(-3.34009626844846,3.89058202773615,34.4952270265461));
#55421=CARTESIAN_POINT('Ctrl Pts',(-4.79588731339343,1.81447967039556,34.6344004839681));
#55422=CARTESIAN_POINT('Ctrl Pts',(-5.07891583368533,-0.705326556558901,
34.7735739413899));
#55423=CARTESIAN_POINT('Ctrl Pts',(-4.11997143710345,-3.05265572158056,
34.912747398812));
#55424=CARTESIAN_POINT('Ctrl Pts',(-2.15354963574969,-4.65350357939147,
35.0519208562339));
#55425=CARTESIAN_POINT('Ctrl Pts',(0.339490524783248,-5.11640672548902,
35.1910943136559));
#55426=CARTESIAN_POINT('Ctrl Pts',(2.74951335423154,-4.32816911776206,35.3302677710778));
#55427=CARTESIAN_POINT('Ctrl Pts',(4.48718380920458,-2.4815424758523,35.4694412284998));
#55428=CARTESIAN_POINT('Ctrl Pts',(5.12758056511281,-0.0280917305306554,
35.6086146859217));
#55429=CARTESIAN_POINT('Ctrl Pts',(4.51410417181047,2.43222842740771,35.7477881433437));
#55430=CARTESIAN_POINT('Ctrl Pts',(2.79677110733593,4.29778349503762,35.8869616007656));
#55431=CARTESIAN_POINT('Ctrl Pts',(0.395529491558261,5.1123798781345,36.0261350581876));
#55432=CARTESIAN_POINT('Ctrl Pts',(-2.10243294662056,4.67682021270983,36.1653085156095));
#55433=CARTESIAN_POINT('Ctrl Pts',(-4.08627684754628,3.09761410157141,36.3044819730315));
#55434=CARTESIAN_POINT('Ctrl Pts',(-5.07088285170647,0.760932783704383,
36.4436554304534));
#55435=CARTESIAN_POINT('Ctrl Pts',(-4.81548028461036,-1.76182326740675,
36.5828288878754));
#55436=CARTESIAN_POINT('Ctrl Pts',(-3.38252402474393,-3.85375178482954,
36.7220023452973));
#55437=CARTESIAN_POINT('Ctrl Pts',(-1.12242209698828,-5.0033029323877,36.8611758027193));
#55438=CARTESIAN_POINT('Ctrl Pts',(1.41215136985344,-4.92937116736687,37.0003492601412));
#55439=CARTESIAN_POINT('Ctrl Pts',(3.60140433654983,-3.6500353973252,37.1395227175632));
#55440=CARTESIAN_POINT('Ctrl Pts',(4.90998772824735,-1.47813805360231,37.2786961749851));
#55441=CARTESIAN_POINT('Ctrl Pts',(5.01790704510018,1.05521584700991,37.4178696324071));
#55442=CARTESIAN_POINT('Ctrl Pts',(3.89877223200052,3.33053249196408,37.5570430898291));
#55443=CARTESIAN_POINT('Ctrl Pts',(1.82625097191763,4.79141722088745,37.696216547251));
#55444=CARTESIAN_POINT('Ctrl Pts',(-0.692852653537991,5.08063251943419,
37.835390004673));
#55445=CARTESIAN_POINT('Ctrl Pts',(-3.04252952350951,4.12745511127861,37.9745634620949));
#55446=CARTESIAN_POINT('Ctrl Pts',(-4.64820129658106,2.16497027774265,38.1137369195169));
#55447=CARTESIAN_POINT('Ctrl Pts',(-5.11722495190999,-0.326925662187272,
38.2529103769388));
#55448=CARTESIAN_POINT('Ctrl Pts',(-4.33490776837895,-2.73887682028504,
38.3920838343608));
#55449=CARTESIAN_POINT('Ctrl Pts',(-2.4925537144267,-4.48107660922512,38.5312572917828));
#55450=CARTESIAN_POINT('Ctrl Pts',(-0.0406829233315988,-5.12749612352813,
38.6704307492046));
#55451=CARTESIAN_POINT('Ctrl Pts',(2.42113626829065,-4.52006313754736,38.8096042066267));
#55452=CARTESIAN_POINT('Ctrl Pts',(4.29090279124404,-2.80731630443399,38.9487776640485));
#55453=CARTESIAN_POINT('Ctrl Pts',(5.11139320288289,-0.408082249760327,
39.0879511214706));
#55454=CARTESIAN_POINT('Ctrl Pts',(4.6819688426782,2.09094221661848,39.2271245788925));
#55455=CARTESIAN_POINT('Ctrl Pts',(3.10763901629375,4.0786580319335,39.3662980363144));
#55456=CARTESIAN_POINT('Ctrl Pts',(0.773382540198208,5.06899901790909,39.5054714937364));
#55457=CARTESIAN_POINT('Ctrl Pts',(-1.74999307091798,4.81979209601264,39.6446449511584));
#55458=CARTESIAN_POINT('Ctrl Pts',(-3.84543404598807,3.39197709234639,39.7838184085803));
#55459=CARTESIAN_POINT('Ctrl Pts',(-5.00053162984347,1.13470481447017,39.9229918660022));
#55460=CARTESIAN_POINT('Ctrl Pts',(-4.93282398171498,-1.40004255737619,
40.0621653234243));
#55461=CARTESIAN_POINT('Ctrl Pts',(-3.65886799445027,-3.59243045809301,
40.2013387808461));
#55462=CARTESIAN_POINT('Ctrl Pts',(-1.49019055396033,-4.90634321159193,
40.3405122382681));
#55463=CARTESIAN_POINT('Ctrl Pts',(1.04289070214805,-5.02048310229404,40.4796856956901));
#55464=CARTESIAN_POINT('Ctrl Pts',(3.32094863246379,-3.90693892677934,40.618859153112));
#55465=CARTESIAN_POINT('Ctrl Pts',(4.7869182362722,-1.83801126119823,40.758032610534));
#55466=CARTESIAN_POINT('Ctrl Pts',(5.0823185691137,0.680374572635465,40.8972060679559));
#55467=CARTESIAN_POINT('Ctrl Pts',(4.13491389701701,3.03238497907216,41.0363795253779));
#55468=CARTESIAN_POINT('Ctrl Pts',(2.17637786502656,4.64287098524924,41.1755529827997));
#55469=CARTESIAN_POINT('Ctrl Pts',(-0.314358828238725,5.11801232161034,
41.3147264402218));
#55470=CARTESIAN_POINT('Ctrl Pts',(-2.72822377098922,4.34162027962559,41.4538998976437));
#55471=CARTESIAN_POINT('Ctrl Pts',(-4.47494238848132,2.50354992297337,41.5930733550657));
#55472=CARTESIAN_POINT('Ctrl Pts',(-5.12738076328793,0.0532738708158156,
41.7322468124876));
#55473=CARTESIAN_POINT('Ctrl Pts',(-4.5259948474324,-2.41002950979075,41.8714202699096));
#55474=CARTESIAN_POINT('Ctrl Pts',(-2.81784457349484,-4.28399621342882,
42.0105937273315));
#55475=CARTESIAN_POINT('Ctrl Pts',(-0.420632547238203,-5.1103757060759,
42.1497671847535));
#55476=CARTESIAN_POINT('Ctrl Pts',(2.07943887829429,-4.68708924050791,42.2889406421754));
#55477=CARTESIAN_POINT('Ctrl Pts',(4.07101462212891,-3.11764519204149,42.4281140995974));
#55478=CARTESIAN_POINT('Ctrl Pts',(5.06708461819206,-0.785827633217498,
42.5672875570193));
#55479=CARTESIAN_POINT('Ctrl Pts',(4.82407484420597,1.73815232202072,42.7064610144413));
#55480=CARTESIAN_POINT('Ctrl Pts',(3.40140970642374,3.83709311928876,42.8456344718632));
#55481=CARTESIAN_POINT('Ctrl Pts',(1.14698068971451,4.99773017423599,42.9848079292852));
#55482=CARTESIAN_POINT('Ctrl Pts',(-1.38792530268207,4.93624705127506,43.1239813867072));
#55483=CARTESIAN_POINT('Ctrl Pts',(-3.58343491738278,3.66767852870569,43.2631548441291));
#55484=CARTESIAN_POINT('Ctrl Pts',(-4.90266910982671,1.50223406851191,43.4023283015511));
#55485=CARTESIAN_POINT('Ctrl Pts',(-5.02302888611788,-1.03055926868484,
43.541501758973));
#55486=CARTESIAN_POINT('Ctrl Pts',(-3.91508206282783,-3.3113447477378,43.680675216395));
#55487=CARTESIAN_POINT('Ctrl Pts',(-1.84976046732335,-4.78239038667639,
43.8198486738169));
#55488=CARTESIAN_POINT('Ctrl Pts',(0.667892389093657,-5.08397397255705,
43.9590221312389));
#55489=CARTESIAN_POINT('Ctrl Pts',(3.02222214943982,-4.14234774934242,44.0981955886608));
#55490=CARTESIAN_POINT('Ctrl Pts',(4.63751267753772,-2.18777232881387,44.2373690460827));
#55491=CARTESIAN_POINT('Ctrl Pts',(5.1187688298422,0.301790098715543,44.3765425035047));
#55492=CARTESIAN_POINT('Ctrl Pts',(4.34830661102557,2.71755427058194,44.5157159609267));
#55493=CARTESIAN_POINT('Ctrl Pts',(2.51453103518521,4.46878118396249,44.6548894183486));
#55494=CARTESIAN_POINT('Ctrl Pts',(0.0658644970599633,5.12723448508783,
44.7940628757706));
#55495=CARTESIAN_POINT('Ctrl Pts',(-2.3989082188817,4.5318992656974,44.9332363331925));
#55496=CARTESIAN_POINT('Ctrl Pts',(-4.27706380323859,2.82835585103309,45.0724097906145));
#55497=CARTESIAN_POINT('Ctrl Pts',(-5.10932739384903,0.433180308313655,
45.2115832480364));
#55498=CARTESIAN_POINT('Ctrl Pts',(-4.692181375323,-2.06792300101305,45.3507567054584));
#55499=CARTESIAN_POINT('Ctrl Pts',(-3.12763256847743,-4.06334666422225,
45.4899301628804));
#55500=CARTESIAN_POINT('Ctrl Pts',(-0.798267987718407,-5.06513966409919,
45.6291036203023));
#55501=CARTESIAN_POINT('Ctrl Pts',(1.72630109211463,-4.82832850336539,45.7682770777242));
#55502=CARTESIAN_POINT('Ctrl Pts',(3.82872905502739,-3.41082181009738,45.9074505351462));
#55503=CARTESIAN_POINT('Ctrl Pts',(4.99489858245798,-1.15924964869784,46.0466239925681));
#55504=CARTESIAN_POINT('Ctrl Pts',(4.93964035540605,1.37579967883806,46.1857974499902));
#55505=CARTESIAN_POINT('Ctrl Pts',(3.67646694696398,3.57441776866221,46.3249709074119));
#55506=CARTESIAN_POINT('Ctrl Pts',(1.51426852463472,4.89896544510649,46.4641443648341));
#55507=CARTESIAN_POINT('Ctrl Pts',(-1.01822162097875,5.02554438122063,46.6033178222559));
#55508=CARTESIAN_POINT('Ctrl Pts',(-3.30172089569737,3.92320159104299,46.7424912796779));
#55509=CARTESIAN_POINT('Ctrl Pts',(-4.77783369940276,1.86149851944559,46.8816647370998));
#55510=CARTESIAN_POINT('Ctrl Pts',(-5.08559871978225,-0.655406178179629,
47.0208381945219));
#55511=CARTESIAN_POINT('Ctrl Pts',(-4.14975662342901,-3.01204109589393,
47.1600116519437));
#55512=CARTESIAN_POINT('Ctrl Pts',(-2.19915360039652,-4.63212640575685,
47.2991851093658));
#55513=CARTESIAN_POINT('Ctrl Pts',(0.289219549406528,-5.11949447204388,
47.4383585667875));
#55514=CARTESIAN_POINT('Ctrl Pts',(2.7068683833997,-4.35496672226068,47.5775320242097));
#55515=CARTESIAN_POINT('Ctrl Pts',(4.4625930328204,-2.52549698484668,47.7167054816315));
#55516=CARTESIAN_POINT('Ctrl Pts',(5.12705728980988,-0.0784547261432202,
47.8558789390536));
#55517=CARTESIAN_POINT('Ctrl Pts',(4.53777635673904,2.38777246262433,47.9950523964754));
#55518=CARTESIAN_POINT('Ctrl Pts',(2.83885007366626,4.27010560247541,48.1342258538975));
#55519=CARTESIAN_POINT('Ctrl Pts',(0.445725457324341,5.10824827252355,48.2733993113193));
#55520=CARTESIAN_POINT('Ctrl Pts',(-2.0563946542149,4.69724521641816,48.4125727687414));
#55521=CARTESIAN_POINT('Ctrl Pts',(-4.05565420445089,3.13760108537823,48.5517462261632));
#55522=CARTESIAN_POINT('Ctrl Pts',(-5.06316416735844,0.810703528686243,
48.6909196835853));
#55523=CARTESIAN_POINT('Ctrl Pts',(-4.83255304784156,-1.714439452662,48.8300931410071));
#55524=CARTESIAN_POINT('Ctrl Pts',(-3.4202133466128,-3.8203419036388,48.9692665984293));
#55525=CARTESIAN_POINT('Ctrl Pts',(-1.17151161743895,-4.99203687158382,
49.108440055851));
#55526=CARTESIAN_POINT('Ctrl Pts',(1.36366575896105,-4.94300387364647,49.2476135132731));
#55527=CARTESIAN_POINT('Ctrl Pts',(3.56537906630424,-3.68523319623146,49.386786970695));
#55528=CARTESIAN_POINT('Ctrl Pts',(4.89523223976419,-1.52629384976162,49.5259604281169));
#55529=CARTESIAN_POINT('Ctrl Pts',(5.02802957243399,1.00587783342514,49.6651338855389));
#55530=CARTESIAN_POINT('Ctrl Pts',(3.93129746246441,3.29207713437395,49.8043073429608));
#55531=CARTESIAN_POINT('Ctrl Pts',(1.87322534678482,4.77324820192809,49.9434808003828));
#55532=CARTESIAN_POINT('Ctrl Pts',(-0.642916015185119,5.08719280099207,
50.0826542578048));
#55533=CARTESIAN_POINT('Ctrl Pts',(-3.00184187982617,4.15714047460132,50.2218277152267));
#55534=CARTESIAN_POINT('Ctrl Pts',(-4.62671220238579,2.21052161114549,50.3610011726486));
#55535=CARTESIAN_POINT('Ctrl Pts',(-5.12018924383978,-0.276647256112013,
50.5001746300706));
#55536=CARTESIAN_POINT('Ctrl Pts',(-4.36160057317046,-2.69616617387836,
50.6393480874925));
#55537=CARTESIAN_POINT('Ctrl Pts',(-2.53644770583317,-4.45637797236955,
50.7785215449146));
#55538=CARTESIAN_POINT('Ctrl Pts',(-0.0910444821465626,-5.12684917852256,
50.9176950023364));
#55539=CARTESIAN_POINT('Ctrl Pts',(2.37662230816716,-4.54362608511847,51.0568684597585));
#55540=CARTESIAN_POINT('Ctrl Pts',(4.26312165309721,-2.84932717811426,51.1960419171803));
#55541=CARTESIAN_POINT('Ctrl Pts',(5.10713834860655,-0.458267918623071,
51.3352153746024));
#55542=CARTESIAN_POINT('Ctrl Pts',(4.70228073325844,2.04485390741571,51.4743888320243));
#55543=CARTESIAN_POINT('Ctrl Pts',(3.14755068263376,4.04793728920033,51.6135622894463));
#55544=CARTESIAN_POINT('Ctrl Pts',(0.823134181134756,5.06115813988206,51.7527357468682));
#55545=CARTESIAN_POINT('Ctrl Pts',(-1.70256747518846,4.83674845216052,51.8919092042902));
#55546=CARTESIAN_POINT('Ctrl Pts',(-3.8119317156975,3.42958425933908,52.0310826617121));
#55547=CARTESIAN_POINT('Ctrl Pts',(-4.98914505886961,1.18376652199825,52.1702561191341));
#55548=CARTESIAN_POINT('Ctrl Pts',(-4.94633758571435,-1.35152361621851,
52.3094295765559));
#55549=CARTESIAN_POINT('Ctrl Pts',(-3.69397722364766,-3.5563188648122,52.448603033978));
#55550=CARTESIAN_POINT('Ctrl Pts',(-1.53830997137995,-4.891469516311,52.5877764913998));
#55551=CARTESIAN_POINT('Ctrl Pts',(0.993527980457018,-5.03048444477228,
52.7269499488219));
#55552=CARTESIAN_POINT('Ctrl Pts',(3.28241352191931,-3.93936962827405,52.8661234062438));
#55553=CARTESIAN_POINT('Ctrl Pts',(4.76863392190279,-1.88494087862853,53.0052968636658));
#55554=CARTESIAN_POINT('Ctrl Pts',(5.08875620657422,0.630421975425304,53.1444703210877));
#55555=CARTESIAN_POINT('Ctrl Pts',(4.16449925833512,2.9916245627373,53.2836437785097));
#55556=CARTESIAN_POINT('Ctrl Pts',(2.22187629251225,4.62127010007193,53.4228172359315));
#55557=CARTESIAN_POINT('Ctrl Pts',(-0.264073294642276,5.12085314104043,
53.5619906933537));
#55558=CARTESIAN_POINT('Ctrl Pts',(-2.68544770655171,4.36820812375314,53.7011641507754));
#55559=CARTESIAN_POINT('Ctrl Pts',(-4.45013604008643,2.54738313211239,53.8403376081976));
#55560=CARTESIAN_POINT('Ctrl Pts',(-5.12661015248078,0.103633689154421,
53.9795110656193));
#55561=CARTESIAN_POINT('Ctrl Pts',(-4.54944841556215,-2.36545782274508,
54.1186845230415));
#55562=CARTESIAN_POINT('Ctrl Pts',(-2.8597871012007,-4.25611199721682,54.2578579804633));
#55563=CARTESIAN_POINT('Ctrl Pts',(-0.470807616579455,-5.10599762879083,
54.3970314378853));
#55564=CARTESIAN_POINT('Ctrl Pts',(2.0333008302056,-4.70728789547995,54.5362048953072));
#55565=CARTESIAN_POINT('Ctrl Pts',(4.04019596500318,-3.15748130024849,54.6753783527292));
#55566=CARTESIAN_POINT('Ctrl Pts',(5.05912159376628,-0.835559870107751,
54.8145518101511));
#55567=CARTESIAN_POINT('Ctrl Pts',(4.84091469102418,1.69068523128142,54.9537252675731));
#55568=CARTESIAN_POINT('Ctrl Pts',(3.4389344917701,3.80349854191647,55.092898724995));
#55569=CARTESIAN_POINT('Ctrl Pts',(1.1960142884793,4.98622316175281,55.232072182417));
#55570=CARTESIAN_POINT('Ctrl Pts',(-1.33937332382694,4.94964147150757,55.3712456398389));
#55571=CARTESIAN_POINT('Ctrl Pts',(-3.54723721881863,3.70269897648656,55.5104190972609));
#55572=CARTESIAN_POINT('Ctrl Pts',(-4.88767729743601,1.55031681703309,55.6495925546829));
#55573=CARTESIAN_POINT('Ctrl Pts',(-5.03290898343272,-0.981172136543431,
55.7887660121048));
#55574=CARTESIAN_POINT('Ctrl Pts',(-3.94741803979709,-3.27273011660468,
55.9279394695267));
#55575=CARTESIAN_POINT('Ctrl Pts',(-1.89664504433241,-4.76399088715083,
56.0671129269487));
#55576=CARTESIAN_POINT('Ctrl Pts',(0.617924134239044,-5.09028892710146,
56.2062863843707));
#55577=CARTESIAN_POINT('Ctrl Pts',(2.98138920623766,-4.17183293025696,56.3454598417926));
#55578=CARTESIAN_POINT('Ctrl Pts',(4.61580013163112,-2.23321757602816,56.4846332992146));
#55579=CARTESIAN_POINT('Ctrl Pts',(5.12148615964254,0.251497740818248,56.6238067566365));
#55580=CARTESIAN_POINT('Ctrl Pts',(4.37478933416524,2.67471304605202,56.7629802140585));
#55581=CARTESIAN_POINT('Ctrl Pts',(2.55830319774378,4.44386727360986,56.9021536714803));
#55582=CARTESIAN_POINT('Ctrl Pts',(0.116222271253945,5.12634021312587,57.0413271289025));
#55583=CARTESIAN_POINT('Ctrl Pts',(-2.35427907367985,4.55524331296145,57.1805005863242));
#55584=CARTESIAN_POINT('Ctrl Pts',(-4.24907667710245,2.87022977985227,57.3196740437464));
#55585=CARTESIAN_POINT('Ctrl Pts',(-5.10482611995491,0.483344475579185,
57.4588475011681));
#55586=CARTESIAN_POINT('Ctrl Pts',(-4.71226667288952,-2.02173549224955,
57.5980209585902));
#55587=CARTESIAN_POINT('Ctrl Pts',(-3.16739287834083,-4.03243027853956,
57.7371944160121));
#55588=CARTESIAN_POINT('Ctrl Pts',(-0.847980520678397,-5.05705454129148,
57.8763678734341));
#55589=CARTESIAN_POINT('Ctrl Pts',(1.67879279259075,-4.84505173931014,58.0155413308561));
#55590=CARTESIAN_POINT('Ctrl Pts',(3.79504243314771,-3.44826398752403,58.1547147882779));
#55591=CARTESIAN_POINT('Ctrl Pts',(4.98327119785246,-1.20825484302812,58.2938882457));
#55592=CARTESIAN_POINT('Ctrl Pts',(4.95291551110372,1.32721495505253,58.4330617031219));
#55593=CARTESIAN_POINT('Ctrl Pts',(3.71139840215604,3.53813418308582,58.5722351605439));
#55594=CARTESIAN_POINT('Ctrl Pts',(1.56231431431994,4.88385560600616,58.7114086179658));
#55595=CARTESIAN_POINT('Ctrl Pts',(-0.968810376189768,5.0353031737954,58.8505820753878));
#55596=CARTESIAN_POINT('Ctrl Pts',(-3.26302697682058,3.95544264850191,58.9897555328096));
#55597=CARTESIAN_POINT('Ctrl Pts',(-4.75931912566953,1.90833777332089,59.1289289902317));
#55598=CARTESIAN_POINT('Ctrl Pts',(-5.0917909533315,-0.605422566987785,
59.2681024476536));
#55599=CARTESIAN_POINT('Ctrl Pts',(-4.17914144614525,-2.97113587204582,
59.4072759050756));
#55600=CARTESIAN_POINT('Ctrl Pts',(-2.24454539330572,-4.61030233004723,
59.5464493624975));
#55601=CARTESIAN_POINT('Ctrl Pts',(0.238920670469636,-5.12208829582852,
59.6856228199195));
#55602=CARTESIAN_POINT('Ctrl Pts',(2.6639622571092,-4.38134416472343,59.8247962773414));
#55603=CARTESIAN_POINT('Ctrl Pts',(4.43757171073933,-2.56920783687788,59.9639697347634));
#55604=CARTESIAN_POINT('Ctrl Pts',(5.12603936208722,-0.128810152540617,
60.1031431921853));
#55605=CARTESIAN_POINT('Ctrl Pts',(4.56101074237015,2.34308612838655,60.2423166496072));
#55606=CARTESIAN_POINT('Ctrl Pts',(2.88065515110656,4.24201573516153,60.3814901070293));
#55607=CARTESIAN_POINT('Ctrl Pts',(0.495878420013193,5.10362382919256,60.5206635644512));
#55608=CARTESIAN_POINT('Ctrl Pts',(-2.01015796326168,4.7172170354076,60.6598370218731));
#55609=CARTESIAN_POINT('Ctrl Pts',(-4.02464027668354,3.1772853572572,60.7990104792952));
#55610=CARTESIAN_POINT('Ctrl Pts',(-5.05495699482949,0.860396057730921,
60.9381839367169));
#55611=CARTESIAN_POINT('Ctrl Pts',(-4.84915957225241,-1.66689023039832,
61.0773573941391));
#55612=CARTESIAN_POINT('Ctrl Pts',(-3.45757268999299,-3.78656344121777,
61.2165308515608));
#55613=CARTESIAN_POINT('Ctrl Pts',(-1.22048811252045,-4.98028918333677,
61.355704308983));
#55614=CARTESIAN_POINT('Ctrl Pts',(1.31504858454702,-4.95615968794384,61.4948777664048));
#55615=CARTESIAN_POINT('Ctrl Pts',(3.52900980989584,-3.72007544198956,61.6340512238268));
#55616=CARTESIAN_POINT('Ctrl Pts',(4.8800044701548,-1.57430240300827,61.7732246812487));
#55617=CARTESIAN_POINT('Ctrl Pts',(5.0376669914975,0.956442797563212,61.9123981386707));
#55618=CARTESIAN_POINT('Ctrl Pts',(3.96344342536178,3.25330411499177,62.0515715960926));
#55619=CARTESIAN_POINT('Ctrl Pts',(1.92001895732006,4.75461875552336,62.1907450535146));
#55620=CARTESIAN_POINT('Ctrl Pts',(-0.592917275387842,5.09326210086,62.3299185109366));
#55621=CARTESIAN_POINT('Ctrl Pts',(-2.96086476568654,4.18642510396251,62.4690919683585));
#55622=CARTESIAN_POINT('Ctrl Pts',(-4.60477644817559,2.25585900886765,62.6082654257805));
#55623=CARTESIAN_POINT('Ctrl Pts',(-5.12266009271483,-0.226340858050212,
62.7474388832024));
#55624=CARTESIAN_POINT('Ctrl Pts',(-4.38787150941422,-2.6531979430407,62.8866123406244));
#55625=CARTESIAN_POINT('Ctrl Pts',(-2.5800990640586,-4.43124443783022,63.0257857980463));
#55626=CARTESIAN_POINT('Ctrl Pts',(-0.141393199236074,-5.12571725998609,
63.1649592554683));
#55627=CARTESIAN_POINT('Ctrl Pts',(2.33187113869595,-4.56673182658543,63.3041327128902));
#55628=CARTESIAN_POINT('Ctrl Pts',(4.23494465804981,-2.89109992630838,63.4433061703121));
#55629=CARTESIAN_POINT('Ctrl Pts',(5.10236059910481,-0.508337431653702,
63.5824796277342));
#55630=CARTESIAN_POINT('Ctrl Pts',(4.72219820521398,1.9984257720543,63.721653085156));
#55631=CARTESIAN_POINT('Ctrl Pts',(3.18703877163087,4.01712720269185,63.8608265425781));
#55632=CARTESIAN_POINT('Ctrl Pts',(1.64440293964314,4.70703764334184,63.953608847526));
#55633=CARTESIAN_POINT('Ctrl Pts',(0.837162017642518,4.84647736182856,64.));
#55634=CARTESIAN_POINT('Ctrl Pts',(-2.29321473482425,4.72388001049942,-0.384322829190576));
#55635=CARTESIAN_POINT('Ctrl Pts',(-3.08003554722089,4.34191665058258,-0.337931676716592));
#55636=CARTESIAN_POINT('Ctrl Pts',(-4.45832109727037,3.17760685879857,-0.245149371768623));
#55637=CARTESIAN_POINT('Ctrl Pts',(-5.43565004358383,0.652397313295008,
-0.105975914346671));
#55638=CARTESIAN_POINT('Ctrl Pts',(-5.08369590891124,-2.0316315709213,0.0331975430752808));
#55639=CARTESIAN_POINT('Ctrl Pts',(-3.48864045527025,-4.2192066179736,0.172371000497233));
#55640=CARTESIAN_POINT('Ctrl Pts',(-1.04046924885582,-5.3748591324054,0.311544457919186));
#55641=CARTESIAN_POINT('Ctrl Pts',(1.66212242595201,-5.21626167055254,0.450717915341138));
#55642=CARTESIAN_POINT('Ctrl Pts',(3.9582724176131,-3.78205855212937,0.58989137276309));
#55643=CARTESIAN_POINT('Ctrl Pts',(5.28648326155152,-1.42303359857138,0.729064830185042));
#55644=CARTESIAN_POINT('Ctrl Pts',(5.32196512387744,1.28398525892032,0.868238287606994));
#55645=CARTESIAN_POINT('Ctrl Pts',(4.05603925878376,3.67701840740235,1.00741174502895));
#55646=CARTESIAN_POINT('Ctrl Pts',(1.79827002706525,5.17089492789387,1.1465852024509));
#55647=CARTESIAN_POINT('Ctrl Pts',(-0.899239443192715,5.40030475984112,
1.28575865987285));
#55648=CARTESIAN_POINT('Ctrl Pts',(-3.37685325500269,4.30915166991622,1.4249321172948));
#55649=CARTESIAN_POINT('Ctrl Pts',(-5.02870815206118,2.16425954210186,1.56410557471676));
#55650=CARTESIAN_POINT('Ctrl Pts',(-5.4508676437325,-0.509869668716006,
1.70327903213871));
#55651=CARTESIAN_POINT('Ctrl Pts',(-4.54009897901715,-3.05931799129542,
1.84245248956066));
#55652=CARTESIAN_POINT('Ctrl Pts',(-2.51911699485592,-4.86065578946139,
1.98162594698261));
#55653=CARTESIAN_POINT('Ctrl Pts',(0.117877375912552,-5.47339293083152,
2.12079940440456));
#55654=CARTESIAN_POINT('Ctrl Pts',(2.72604659895634,-4.74769366479615,2.25997286182652));
#55655=CARTESIAN_POINT('Ctrl Pts',(4.66760189067538,-2.86101691810178,2.39914631924847));
#55656=CARTESIAN_POINT('Ctrl Pts',(5.46776493995964,-0.274721263755522,
2.53831977667042));
#55657=CARTESIAN_POINT('Ctrl Pts',(4.9308678380472,2.37875336537121,2.67749323409237));
#55658=CARTESIAN_POINT('Ctrl Pts',(3.18820074280552,4.45053943200986,2.81666669151433));
#55659=CARTESIAN_POINT('Ctrl Pts',(0.665906832292452,5.43401263349861,2.95584014893628));
#55660=CARTESIAN_POINT('Ctrl Pts',(-2.01922463603481,5.08867930612745,3.09501360635823));
#55661=CARTESIAN_POINT('Ctrl Pts',(-4.21058491518014,3.49898555055628,3.23418706378019));
#55662=CARTESIAN_POINT('Ctrl Pts',(-5.37230961851784,1.05366720260117,3.37336052120213));
#55663=CARTESIAN_POINT('Ctrl Pts',(-5.22031634232453,-1.64930970321809,
3.51253397862409));
#55664=CARTESIAN_POINT('Ctrl Pts',(-3.79177276937472,-3.94897258492089,
3.65170743604604));
#55665=CARTESIAN_POINT('Ctrl Pts',(-1.43600786795491,-5.28297327404123,
3.79088089346799));
#55666=CARTESIAN_POINT('Ctrl Pts',(1.27091128347078,-5.32510185072449,3.93005435088995));
#55667=CARTESIAN_POINT('Ctrl Pts',(3.66704808576738,-4.06505640154244,4.06922780831189));
#55668=CARTESIAN_POINT('Ctrl Pts',(5.16646311583264,-1.8109621983326,4.20840126573385));
#55669=CARTESIAN_POINT('Ctrl Pts',(5.40249685035948,0.885975729297808,4.34757472315579));
#55670=CARTESIAN_POINT('Ctrl Pts',(4.31743076922477,3.36626154123542,4.48674818057776));
#55671=CARTESIAN_POINT('Ctrl Pts',(2.17660155646045,5.02337843243596,4.62592163799969));
#55672=CARTESIAN_POINT('Ctrl Pts',(-0.49648301797377,5.45210324773045,4.76509509542167));
#55673=CARTESIAN_POINT('Ctrl Pts',(-3.04816009478389,4.54759774470171,4.9042685528436));
#55674=CARTESIAN_POINT('Ctrl Pts',(-4.85445520268865,2.53104521811412,5.04344201026558));
#55675=CARTESIAN_POINT('Ctrl Pts',(-5.47366588443908,-0.104436567240076,
5.1826154676875));
#55676=CARTESIAN_POINT('Ctrl Pts',(-4.75437342750754,-2.71437995182313,
5.32178892510947));
#55677=CARTESIAN_POINT('Ctrl Pts',(-2.87247004591648,-4.66056231010398,
5.46096238253142));
#55678=CARTESIAN_POINT('Ctrl Pts',(-0.288147069596518,-5.46707384963218,
5.60013583995337));
#55679=CARTESIAN_POINT('Ctrl Pts',(2.36663796363368,-4.93669423401298,5.73930929737533));
#55680=CARTESIAN_POINT('Ctrl Pts',(4.44269707362967,-3.19911986693394,5.87848275479727));
#55681=CARTESIAN_POINT('Ctrl Pts',(5.43236105048979,-0.679248576127037,
6.01765621221923));
#55682=CARTESIAN_POINT('Ctrl Pts',(5.09362236813656,2.00672279646893,6.15682966964118));
#55683=CARTESIAN_POINT('Ctrl Pts',(3.50931450583143,4.20198011777903,6.29600312706314));
#55684=CARTESIAN_POINT('Ctrl Pts',(1.06685625951563,5.36970603781822,6.43517658448508));
#55685=CARTESIAN_POINT('Ctrl Pts',(-1.63648573126543,5.22435064504803,6.57435004190704));
#55686=CARTESIAN_POINT('Ctrl Pts',(-3.93964960852039,3.80145842712166,6.71352349932899));
#55687=CARTESIAN_POINT('Ctrl Pts',(-5.27943108764563,1.44897639796171,6.85269695675095));
#55688=CARTESIAN_POINT('Ctrl Pts',(-5.32820664305195,-1.2578311412849,6.99187041417289));
#55689=CARTESIAN_POINT('Ctrl Pts',(-4.07404894205586,-3.65705488457347,
7.13104387159485));
#55690=CARTESIAN_POINT('Ctrl Pts',(-1.82364349572545,-5.16200054354388,
7.27021732901679));
#55691=CARTESIAN_POINT('Ctrl Pts',(0.872706696667147,-5.40465616229575,
7.40939078643876));
#55692=CARTESIAN_POINT('Ctrl Pts',(3.35564951687092,-4.32568393794243,7.5485642438607));
#55693=CARTESIAN_POINT('Ctrl Pts',(5.01801842820364,-2.18893039296773,7.68773770128266));
#55694=CARTESIAN_POINT('Ctrl Pts',(5.45330597251155,0.483093346278957,7.82691115870461));
#55695=CARTESIAN_POINT('Ctrl Pts',(4.55506909013666,3.03698383188497,7.96608461612655));
#55696=CARTESIAN_POINT('Ctrl Pts',(2.54295817840347,4.84822533654739,8.10525807354852));
#55697=CARTESIAN_POINT('Ctrl Pts',(-0.0909951283882992,5.47390583565873,
8.24443153097046));
#55698=CARTESIAN_POINT('Ctrl Pts',(-2.70269693727647,4.76102451960558,8.38360498839242));
#55699=CARTESIAN_POINT('Ctrl Pts',(-4.65349462636169,2.88390585378095,8.52277844581437));
#55700=CARTESIAN_POINT('Ctrl Pts',(-5.46634979306309,0.301571137425558,
8.66195190323632));
#55701=CARTESIAN_POINT('Ctrl Pts',(-4.9424908618235,-2.35450829088376,8.80112536065827));
#55702=CARTESIAN_POINT('Ctrl Pts',(-3.21001970047595,-4.43482792604239,
8.94029881808022));
#55703=CARTESIAN_POINT('Ctrl Pts',(-0.692586224104254,-5.43067671043215,
9.07947227550218));
#55704=CARTESIAN_POINT('Ctrl Pts',(1.99420885641777,-5.09853471578198,9.21864573292412));
#55705=CARTESIAN_POINT('Ctrl Pts',(4.19334998255961,-3.51962230002261,9.35781919034609));
#55706=CARTESIAN_POINT('Ctrl Pts',(5.36707007794315,-1.08003888332615,9.49699264776802));
#55707=CARTESIAN_POINT('Ctrl Pts',(5.22835344508653,1.62365189135507,9.63616610519));
#55708=CARTESIAN_POINT('Ctrl Pts',(3.81112116218231,3.93030287614265,9.77533956261193));
#55709=CARTESIAN_POINT('Ctrl Pts',(1.46193619068226,5.2758570664322,9.9145130200339));
#55710=CARTESIAN_POINT('Ctrl Pts',(-1.24474341441315,5.33127930644458,10.0536864774558));
#55711=CARTESIAN_POINT('Ctrl Pts',(-3.64703963144277,4.08301691617056,10.1928599348778));
#55712=CARTESIAN_POINT('Ctrl Pts',(-5.15750684453896,1.83631379659982,10.3320333922997));
#55713=CARTESIAN_POINT('Ctrl Pts',(-5.40678288430936,-0.859432401639897,
10.4712068497217));
#55714=CARTESIAN_POINT('Ctrl Pts',(-4.33391102290919,-3.34501725803552,
10.6103803071437));
#55715=CARTESIAN_POINT('Ctrl Pts',(-2.20124603028706,-5.01262816546316,
10.7495537645656));
#55716=CARTESIAN_POINT('Ctrl Pts',(0.469700761545068,-5.45447581401303,
10.8887272219876));
#55717=CARTESIAN_POINT('Ctrl Pts',(3.02578925606011,-4.56251296863476,11.0279006794095));
#55718=CARTESIAN_POINT('Ctrl Pts',(4.8419662357455,-2.55485580472747,11.1670741368315));
#55719=CARTESIAN_POINT('Ctrl Pts',(5.47411277938217,0.0775531408384875,
11.3062475942534));
#55720=CARTESIAN_POINT('Ctrl Pts',(4.76764690286142,2.6909976255443,11.4454210516754));
#55721=CARTESIAN_POINT('Ctrl Pts',(2.89532427177529,4.6463988821794,11.5845945090973));
#55722=CARTESIAN_POINT('Ctrl Pts',(0.314993386789232,5.46559277456052,11.7237679665193));
#55723=CARTESIAN_POINT('Ctrl Pts',(-2.34236442051593,4.94825768655495,11.8629414239412));
#55724=CARTESIAN_POINT('Ctrl Pts',(-4.42693203656908,3.22090017769063,12.0021148813632));
#55725=CARTESIAN_POINT('Ctrl Pts',(-5.42895962354868,0.705919695806274,
12.1412883387851));
#55726=CARTESIAN_POINT('Ctrl Pts',(-5.10341631940836,-1.98168289134401,
12.2804617962071));
#55727=CARTESIAN_POINT('Ctrl Pts',(-3.52990887099163,-4.18469456155927,
12.419635253629));
#55728=CARTESIAN_POINT('Ctrl Pts',(-1.09321499453303,-5.36440175478844,
12.558808711051));
#55729=CARTESIAN_POINT('Ctrl Pts',(1.61080826087004,-5.23232471830275,12.6979821684729));
#55730=CARTESIAN_POINT('Ctrl Pts',(3.92093244415056,-3.82076091629097,12.8371556258949));
#55731=CARTESIAN_POINT('Ctrl Pts',(5.27225123195099,-1.47488716796925,12.9763290833168));
#55732=CARTESIAN_POINT('Ctrl Pts',(5.33431982237489,1.23164818177408,13.1155025407388));
#55733=CARTESIAN_POINT('Ctrl Pts',(4.09196026980959,3.63700238676701,13.2546759981608));
#55734=CARTESIAN_POINT('Ctrl Pts',(1.84897302455433,5.15298204591473,13.3938494555827));
#55735=CARTESIAN_POINT('Ctrl Pts',(-0.846152924259742,5.40887700357624,
13.5330229130046));
#55736=CARTESIAN_POINT('Ctrl Pts',(-3.33436482884134,4.34211197451597,13.6721963704266));
#55737=CARTESIAN_POINT('Ctrl Pts',(-5.00720767671766,2.21354839415561,13.8113698278485));
#55738=CARTESIAN_POINT('Ctrl Pts',(-5.45561276518078,-0.456305344528939,
13.9505432852705));
#55739=CARTESIAN_POINT('Ctrl Pts',(-4.56992933530968,-3.01457643481222,
14.0897167426925));
#55740=CARTESIAN_POINT('Ctrl Pts',(-2.56673802534377,-4.83567793802519,
14.2288902001144));
#55741=CARTESIAN_POINT('Ctrl Pts',(0.0641106856454472,-5.47428671436153,
14.3680636575364));
#55742=CARTESIAN_POINT('Ctrl Pts',(2.67928208717311,-4.77424053734229,14.5072371149583));
#55743=CARTESIAN_POINT('Ctrl Pts',(4.63927512034426,-2.90672523104677,14.6464105723803));
#55744=CARTESIAN_POINT('Ctrl Pts',(5.46480279868925,-0.328413736751764,
14.7855840298022));
#55745=CARTESIAN_POINT('Ctrl Pts',(4.95399467343356,2.33020642575739,14.9247574872242));
#55746=CARTESIAN_POINT('Ctrl Pts',(3.23176123296902,4.41900945282172,15.0639309446461));
#55747=CARTESIAN_POINT('Ctrl Pts',(0.719248910832644,5.42720980019339,15.2031044020681));
#55748=CARTESIAN_POINT('Ctrl Pts',(-1.96914497677888,5.10826714957975,15.34227785949));
#55749=CARTESIAN_POINT('Ctrl Pts',(-4.17601390696993,3.54017415671077,15.481451316912));
#55750=CARTESIAN_POINT('Ctrl Pts',(-5.36170108444399,1.10638451368468,15.6206247743339));
#55751=CARTESIAN_POINT('Ctrl Pts',(-5.23626444075002,-1.59795491725705,
15.7597982317559));
#55752=CARTESIAN_POINT('Ctrl Pts',(-3.8303776313202,-3.91153836904752,15.8989716891778));
#55753=CARTESIAN_POINT('Ctrl Pts',(-1.48782925172868,-5.26861360594508,
16.0381451465998));
#55754=CARTESIAN_POINT('Ctrl Pts',(1.21854552233153,-5.33732817250869,16.1773186040217));
#55755=CARTESIAN_POINT('Ctrl Pts',(3.62694321107045,-4.10087894904483,16.3164920614437));
#55756=CARTESIAN_POINT('Ctrl Pts',(5.14842617495558,-1.86162110325421,16.4556655188657));
#55757=CARTESIAN_POINT('Ctrl Pts',(5.4109385074689,0.832868344601511,16.5948389762876));
#55758=CARTESIAN_POINT('Ctrl Pts',(4.35028674331132,3.32369229352223,16.7340124337096));
#55759=CARTESIAN_POINT('Ctrl Pts',(2.22583741039042,5.00175699465254,16.8731858911315));
#55760=CARTESIAN_POINT('Ctrl Pts',(-0.442907176004575,5.45671681915901,
17.0123593485535));
#55761=CARTESIAN_POINT('Ctrl Pts',(-3.00334543575433,4.57731814544092,17.1515328059754));
#55762=CARTESIAN_POINT('Ctrl Pts',(-4.82936048130468,2.57860476860292,17.2907062633974));
#55763=CARTESIAN_POINT('Ctrl Pts',(-5.474427639548,-0.0506678438667996,
17.4298797208193));
#55764=CARTESIAN_POINT('Ctrl Pts',(-4.78080538328875,-2.66755039280729,
17.5690531782413));
#55765=CARTESIAN_POINT('Ctrl Pts',(-2.91810866284794,-4.63212338381232,
17.7082266356632));
#55766=CARTESIAN_POINT('Ctrl Pts',(-0.341832106388815,-5.46397987021282,
17.8474000930852));
#55767=CARTESIAN_POINT('Ctrl Pts',(2.3180343799205,-4.95970178786544,17.9865735505071));
#55768=CARTESIAN_POINT('Ctrl Pts',(4.41106022257329,-3.24260280081925,18.1257470079291));
#55769=CARTESIAN_POINT('Ctrl Pts',(5.42542725091764,-0.732573788808574,
18.264920465351));
#55770=CARTESIAN_POINT('Ctrl Pts',(5.11308717704579,1.95659518832565,18.404093922773));
#55771=CARTESIAN_POINT('Ctrl Pts',(3.55041809528059,4.16730807113576,18.5432673801949));
#55772=CARTESIAN_POINT('Ctrl Pts',(1.1195473613692,5.35896808319478,18.6824408376169));
#55773=CARTESIAN_POINT('Ctrl Pts',(-1.58509193802151,5.24017258867191,18.8216142950388));
#55774=CARTESIAN_POINT('Ctrl Pts',(-3.90212070747964,3.8399712492814,18.9607877524608));
#55775=CARTESIAN_POINT('Ctrl Pts',(-5.26494421034928,1.50076236392,19.0999612098827));
#55776=CARTESIAN_POINT('Ctrl Pts',(-5.34030433870565,-1.20543551509431,
19.2391346673047));
#55777=CARTESIAN_POINT('Ctrl Pts',(-4.10977290009678,-3.61686216500979,
19.3783081247266));
#55778=CARTESIAN_POINT('Ctrl Pts',(-1.87425795643178,-5.14383925913332,
19.5174815821486));
#55779=CARTESIAN_POINT('Ctrl Pts',(0.819578742771026,-5.41296738355655,
19.6566550395706));
#55780=CARTESIAN_POINT('Ctrl Pts',(3.31299971643335,-4.35843528000149,19.7958284969925));
#55781=CARTESIAN_POINT('Ctrl Pts',(4.99627615213528,-2.23811300488903,19.9350019544145));
#55782=CARTESIAN_POINT('Ctrl Pts',(5.45778796929029,0.429506336762568,20.0741754118364));
#55783=CARTESIAN_POINT('Ctrl Pts',(4.58467935447419,2.99209632660904,20.2133488692584));
#55784=CARTESIAN_POINT('Ctrl Pts',(2.59045596294879,4.82301390367809,20.3525223266803));
#55785=CARTESIAN_POINT('Ctrl Pts',(-0.0372246965624955,5.47453555409178,
20.4916957841023));
#55786=CARTESIAN_POINT('Ctrl Pts',(-2.65580261318861,4.78734140111499,20.6308692415242));
#55787=CARTESIAN_POINT('Ctrl Pts',(-4.62494371570838,2.92947449853702,20.7700426989462));
#55788=CARTESIAN_POINT('Ctrl Pts',(-5.46312399409346,0.35524841478801,20.9092161563681));
#55789=CARTESIAN_POINT('Ctrl Pts',(-4.96537899543687,-2.30584835640235,
21.0483896137901));
#55790=CARTESIAN_POINT('Ctrl Pts',(-3.25342481586699,-4.4030843937574,21.187563071212));
#55791=CARTESIAN_POINT('Ctrl Pts',(-0.745894249385438,-5.42361198647016,
21.326736528634));
#55792=CARTESIAN_POINT('Ctrl Pts',(1.9440336016592,-5.11787637274183,21.4659099860559));
#55793=CARTESIAN_POINT('Ctrl Pts',(4.15857710655266,-3.56064062493046,21.6050834434779));
#55794=CARTESIAN_POINT('Ctrl Pts',(5.35620276752075,-1.132703458215,21.7442569008998));
#55795=CARTESIAN_POINT('Ctrl Pts',(5.24404913850238,1.57221940072675,21.8834303583218));
#55796=CARTESIAN_POINT('Ctrl Pts',(3.8495417123254,3.89267951623505,22.0226038157437));
#55797=CARTESIAN_POINT('Ctrl Pts',(1.51368642655711,5.26124306728988,22.1617772731657));
#55798=CARTESIAN_POINT('Ctrl Pts',(-1.19231823911521,5.34324830301965,22.3009507305877));
#55799=CARTESIAN_POINT('Ctrl Pts',(-3.60675930937326,4.11864206933528,22.4401241880096));
#55800=CARTESIAN_POINT('Ctrl Pts',(-5.13922132610689,1.88688350788735,22.5792976454316));
#55801=CARTESIAN_POINT('Ctrl Pts',(-5.41496361960511,-0.806284198903995,
22.7184711028535));
#55802=CARTESIAN_POINT('Ctrl Pts',(-4.36655753545115,-3.30228716205056,
22.8576445602755));
#55803=CARTESIAN_POINT('Ctrl Pts',(-2.25037510363002,-4.99076518221518,
22.9968180176974));
#55804=CARTESIAN_POINT('Ctrl Pts',(0.41610290760959,-5.45882620911565,23.1359914751193));
#55805=CARTESIAN_POINT('Ctrl Pts',(2.98082917520816,-4.59201291802157,23.2751649325413));
#55806=CARTESIAN_POINT('Ctrl Pts',(4.81663824341509,-2.60229153691902,23.4143383899633));
#55807=CARTESIAN_POINT('Ctrl Pts',(5.47461045734216,0.0237813247943329,
23.5535118473852));
#55808=CARTESIAN_POINT('Ctrl Pts',(4.79384855140899,2.64403881915585,23.6926853048072));
#55809=CARTESIAN_POINT('Ctrl Pts',(2.94082266957834,4.61773615932561,23.8318587622291));
#55810=CARTESIAN_POINT('Ctrl Pts',(0.368662581049387,5.46223517549209,23.9710322196511));
#55811=CARTESIAN_POINT('Ctrl Pts',(-2.29364842868432,4.97102626191444,24.110205677073));
#55812=CARTESIAN_POINT('Ctrl Pts',(-4.39508201446807,3.26422721285581,24.249379134495));
#55813=CARTESIAN_POINT('Ctrl Pts',(-5.42176401779696,0.759210212241224,
24.3885525919169));
#55814=CARTESIAN_POINT('Ctrl Pts',(-5.12263470778918,-1.93146029252551,
24.5277260493389));
#55815=CARTESIAN_POINT('Ctrl Pts',(-3.57084168401882,-4.14982106586813,
24.6668995067608));
#55816=CARTESIAN_POINT('Ctrl Pts',(-1.14585272489122,-5.35340515409665,
24.8060729641828));
#55817=CARTESIAN_POINT('Ctrl Pts',(1.5593373829938,-5.24789406686598,24.9452464216047));
#55818=CARTESIAN_POINT('Ctrl Pts',(3.88321485224389,-3.85908896274257,25.0844198790267));
#55819=CARTESIAN_POINT('Ctrl Pts',(5.25751019908472,-1.5266013617082,25.2235933364486));
#55820=CARTESIAN_POINT('Ctrl Pts',(5.34616004769862,1.1791937734911,25.3627667938706));
#55821=CARTESIAN_POINT('Ctrl Pts',(4.12748640327948,3.59663470508086,25.5019402512925));
#55822=CARTESIAN_POINT('Ctrl Pts',(1.89949768148914,5.1345724037223,25.6411137087145));
#55823=CARTESIAN_POINT('Ctrl Pts',(-0.792984793166221,5.41692720357734,
25.7802871661364));
#55824=CARTESIAN_POINT('Ctrl Pts',(-3.29155469497027,4.3746534606833,25.9194606235584));
#55825=CARTESIAN_POINT('Ctrl Pts',(-4.98522411812324,2.26262363267325,26.0586340809804));
#55826=CARTESIAN_POINT('Ctrl Pts',(-5.45983153237451,-0.402696969367929,
26.1978075384023));
#55827=CARTESIAN_POINT('Ctrl Pts',(-4.59931879186191,-2.96954404949229,
26.3369809958243));
#55828=CARTESIAN_POINT('Ctrl Pts',(-2.61411141914543,-4.81023353896073,
26.4761544532462));
#55829=CARTESIAN_POINT('Ctrl Pts',(0.0103378096254605,-5.47465234884748,
26.6153279106682));
#55830=CARTESIAN_POINT('Ctrl Pts',(2.63225908164434,-4.80032679493282,26.7545013680901));
#55831=CARTESIAN_POINT('Ctrl Pts',(4.61050075812538,-2.95215310754276,26.8936748255121));
#55832=CARTESIAN_POINT('Ctrl Pts',(5.46131341976825,-0.382074524285904,
27.032848282934));
#55833=CARTESIAN_POINT('Ctrl Pts',(4.9766435532453,2.28143467033162,27.172021740356));
#55834=CARTESIAN_POINT('Ctrl Pts',(3.27500992664753,4.38705313295944,27.3111951977779));
#55835=CARTESIAN_POINT('Ctrl Pts',(0.772521597081072,5.4198833560412,27.4503686551999));
#55836=CARTESIAN_POINT('Ctrl Pts',(-1.91887533674131,5.12736215349522,27.5895421126219));
#55837=CARTESIAN_POINT('Ctrl Pts',(-4.14104000188076,3.58102121103358,27.7287155700437));
#55838=CARTESIAN_POINT('Ctrl Pts',(-5.350575259792,1.15899508210823,27.8678890274658));
#55839=CARTESIAN_POINT('Ctrl Pts',(-5.25170735057791,-1.54644596250082,
28.0070624848877));
#55840=CARTESIAN_POINT('Ctrl Pts',(-3.86861294296327,-3.87372677257782,
28.1462359423097));
#55841=CARTESIAN_POINT('Ctrl Pts',(-1.53950709149657,-5.25374562824285,
28.2854093997316));
#55842=CARTESIAN_POINT('Ctrl Pts',(1.16606219736214,-5.34903955518484,28.4245828571536));
#55843=CARTESIAN_POINT('Ctrl Pts',(3.58648841318369,-4.13630584859827,28.5637563145755));
#55844=CARTESIAN_POINT('Ctrl Pts',(5.1298925200124,-1.91210040117403,28.7029297719975));
#55845=CARTESIAN_POINT('Ctrl Pts',(5.41885812363289,0.779680605752741,28.8421032294194));
#55846=CARTESIAN_POINT('Ctrl Pts',(4.38272300687972,3.28080237990896,28.9812766868414));
#55847=CARTESIAN_POINT('Ctrl Pts',(2.27485851816045,4.97965299327192,29.1204501442633));
#55848=CARTESIAN_POINT('Ctrl Pts',(-0.389288602875022,5.4608039330048,29.2596236016852));
#55849=CARTESIAN_POINT('Ctrl Pts',(-2.95824101751041,4.60659693194099,29.3987970591072));
#55850=CARTESIAN_POINT('Ctrl Pts',(-4.80379982893518,2.62591553835446,29.5379705165292));
#55851=CARTESIAN_POINT('Ctrl Pts',(-5.47466122835514,0.003105767880113,
29.6771439739511));
#55852=CARTESIAN_POINT('Ctrl Pts',(-4.80677609262286,-2.62046347168559,
29.8163174313731));
#55853=CARTESIAN_POINT('Ctrl Pts',(-2.96346574410807,-4.60323755573695,
29.955490888795));
#55854=CARTESIAN_POINT('Ctrl Pts',(-0.395484163623925,-5.46035873248011,
30.0946643462169));
#55855=CARTESIAN_POINT('Ctrl Pts',(2.26920715499286,-4.98223083555733,30.2338378036389));
#55856=CARTESIAN_POINT('Ctrl Pts',(4.37899779764542,-3.28577289222272,30.3730112610609));
#55857=CARTESIAN_POINT('Ctrl Pts',(5.41797001254325,-0.785828323637693,
30.5121847184828));
#55858=CARTESIAN_POINT('Ctrl Pts',(5.13205868135355,1.90627881019349,30.6513581759048));
#55859=CARTESIAN_POINT('Ctrl Pts',(3.59117914459247,4.13223396754023,30.7905316333268));
#55860=CARTESIAN_POINT('Ctrl Pts',(1.17213045061785,5.34771310167099,30.9297050907486));
#55861=CARTESIAN_POINT('Ctrl Pts',(-1.53354521698279,5.25548896664414,31.0688785481707));
#55862=CARTESIAN_POINT('Ctrl Pts',(-3.86421533444969,3.87811359555816,31.2080520055926));
#55863=CARTESIAN_POINT('Ctrl Pts',(-5.24994937746456,1.55240353810105,31.3472254630145));
#55864=CARTESIAN_POINT('Ctrl Pts',(-5.35188680811497,-1.15292358991135,
31.4863989204365));
#55865=CARTESIAN_POINT('Ctrl Pts',(-4.14510035211066,-3.57632049486357,
31.6255723778584));
#55866=CARTESIAN_POINT('Ctrl Pts',(-1.92469159094798,-5.1251817031968,31.7647458352804));
#55867=CARTESIAN_POINT('Ctrl Pts',(0.766371716887421,-5.42075636812835,
31.9039192927023));
#55868=CARTESIAN_POINT('Ctrl Pts',(3.27003028170278,-4.3907661253813,32.0430927501243));
#55869=CARTESIAN_POINT('Ctrl Pts',(4.97405184125494,-2.28707968631561,32.1822662075462));
#55870=CARTESIAN_POINT('Ctrl Pts',(5.46174340514298,0.375877888982928,32.3214396649682));
#55871=CARTESIAN_POINT('Ctrl Pts',(4.61384729437183,2.9469201474195,32.4606131223901));
#55872=CARTESIAN_POINT('Ctrl Pts',(2.63770382336763,4.79733715213355,32.5997865798121));
#55873=CARTESIAN_POINT('Ctrl Pts',(0.0165493266579919,5.47463709581159,
32.738960037234));
#55874=CARTESIAN_POINT('Ctrl Pts',(-2.60865206040676,4.81319640559002,32.8781334946561));
#55875=CARTESIAN_POINT('Ctrl Pts',(-4.59594659595723,2.97476051105938,33.0173069520779));
#55876=CARTESIAN_POINT('Ctrl Pts',(-5.45937111938441,0.408891418203707,
33.1564804094999));
#55877=CARTESIAN_POINT('Ctrl Pts',(-4.98778807515939,-2.25696595639962,
33.2956538669219));
#55878=CARTESIAN_POINT('Ctrl Pts',(-3.296516044681,-4.37091605709946,33.4348273243438));
#55879=CARTESIAN_POINT('Ctrl Pts',(-0.799130311671916,-5.4160239988405,
33.5740007817658));
#55880=CARTESIAN_POINT('Ctrl Pts',(1.89367078883877,-5.13672426304429,33.7131742391877));
#55881=CARTESIAN_POINT('Ctrl Pts',(4.12340301594658,-3.60131542344347,33.8523476966097));
#55882=CARTESIAN_POINT('Ctrl Pts',(5.34481869699234,-1.18525875121433,33.9915211540316));
#55883=CARTESIAN_POINT('Ctrl Pts',(5.25923889226169,1.5206352242307,34.1306946114536));
#55884=CARTESIAN_POINT('Ctrl Pts',(3.88759086323862,3.85468059521315,34.2698680688755));
#55885=CARTESIAN_POINT('Ctrl Pts',(1.56529062375651,5.24612146964108,34.4090415262975));
#55886=CARTESIAN_POINT('Ctrl Pts',(-1.13977803036409,5.35470178932016,34.5482149837195));
#55887=CARTESIAN_POINT('Ctrl Pts',(-3.56613101143271,4.15386986078608,34.6873884411414));
#55888=CARTESIAN_POINT('Ctrl Pts',(-5.12043998168154,1.93727117488656,34.8265618985634));
#55889=CARTESIAN_POINT('Ctrl Pts',(-5.42262192561739,-0.753058206822416,
34.9657353559852));
#55890=CARTESIAN_POINT('Ctrl Pts',(-4.39878276768831,-3.25923846530712,
35.1049088134073));
#55891=CARTESIAN_POINT('Ctrl Pts',(-2.29928706344549,-4.96842069584705,
35.2440822708292));
#55892=CARTESIAN_POINT('Ctrl Pts',(0.362464908557797,-5.46264994312406,
35.3832557282512));
#55893=CARTESIAN_POINT('Ctrl Pts',(2.935581507484,-4.62106983543499,35.5224291856731));
#55894=CARTESIAN_POINT('Ctrl Pts',(4.79084554752555,-2.64947620310197,35.6616026430951));
#55895=CARTESIAN_POINT('Ctrl Pts',(5.47457995136234,-0.0299927856439818,
35.800776100517));
#55896=CARTESIAN_POINT('Ctrl Pts',(4.81958769512005,2.59682491903027,35.939949557939));
#55897=CARTESIAN_POINT('Ctrl Pts',(2.98603734028964,4.58862792275044,36.0791230153609));
#55898=CARTESIAN_POINT('Ctrl Pts',(0.422296207179969,5.4583505864364,36.2182964727829));
#55899=CARTESIAN_POINT('Ctrl Pts',(-2.2447111483659,4.99331523854152,36.3574699302048));
#55900=CARTESIAN_POINT('Ctrl Pts',(-4.36280796005417,3.30723931924151,36.4966433876268));
#55901=CARTESIAN_POINT('Ctrl Pts',(-5.41404532666736,0.812427480973212,
36.6358168450487));
#55902=CARTESIAN_POINT('Ctrl Pts',(-5.1413588704341,-1.88105134870308,36.7749903024707));
#55903=CARTESIAN_POINT('Ctrl Pts',(-3.61142998646512,-4.1145472003502,36.9141637598926));
#55904=CARTESIAN_POINT('Ctrl Pts',(-1.19837990473434,-5.34189206320926,
37.0533372173146));
#55905=CARTESIAN_POINT('Ctrl Pts',(1.50771606209154,-5.26295710481857,37.1925106747365));
#55906=CARTESIAN_POINT('Ctrl Pts',(3.84512261236244,-3.89704468885695,37.3316841321585));
#55907=CARTESIAN_POINT('Ctrl Pts',(5.24226192785463,-1.5781682707541,37.4708575895804));
#55908=CARTESIAN_POINT('Ctrl Pts',(5.35748448182613,1.12662559798778,37.6100310470024));
#55909=CARTESIAN_POINT('Ctrl Pts',(4.16261432174461,3.55592002433348,37.7492045044243));
#55910=CARTESIAN_POINT('Ctrl Pts',(1.94983907713515,5.11566738405907,37.8883779618463));
#55911=CARTESIAN_POINT('Ctrl Pts',(-0.739740155837876,5.42445478485075,
38.0275514192682));
#55912=CARTESIAN_POINT('Ctrl Pts',(-3.24842699579643,4.40677288546053,38.1667248766902));
#55913=CARTESIAN_POINT('Ctrl Pts',(-4.962759591004,2.31148057593983,38.3058983341121));
#55914=CARTESIAN_POINT('Ctrl Pts',(-5.46352354148162,-0.349049742479761,
38.4450717915341));
#55915=CARTESIAN_POINT('Ctrl Pts',(-4.62826451157864,-2.92422516607577,
38.5842452489561));
#55916=CARTESIAN_POINT('Ctrl Pts',(-2.66123260657016,-4.7843250542555,38.723418706378));
#55917=CARTESIAN_POINT('Ctrl Pts',(-0.0434360637741723,-5.47448979535197,
38.8625921638));
#55918=CARTESIAN_POINT('Ctrl Pts',(2.58498211887365,-4.82594992267353,39.0017656212219));
#55919=CARTESIAN_POINT('Ctrl Pts',(4.58128158024812,-2.99729616379969,39.1409390786439));
#55920=CARTESIAN_POINT('Ctrl Pts',(5.4572971397899,-0.435698449721977,39.2801125360658));
#55921=CARTESIAN_POINT('Ctrl Pts',(4.99881229237497,2.23244280478805,39.4192859934878));
#55922=CARTESIAN_POINT('Ctrl Pts',(3.31794265124305,4.3546735554013,39.5584594509097));
#55923=CARTESIAN_POINT('Ctrl Pts',(0.825719751359792,5.41203400795518,39.6976329083317));
#55924=CARTESIAN_POINT('Ctrl Pts',(-1.86842056588151,5.14596247557638,39.8368063657536));
#55925=CARTESIAN_POINT('Ctrl Pts',(-4.10566657415155,3.62152277266674,39.9759798231756));
#55926=CARTESIAN_POINT('Ctrl Pts',(-5.33893321796927,1.21149383205752,40.1151532805975));
#55927=CARTESIAN_POINT('Ctrl Pts',(-5.26664358189404,-1.49478780846764,
40.2543267380195));
#55928=CARTESIAN_POINT('Ctrl Pts',(-3.90647501540673,-3.83554144353207,
40.3935001954414));
#55929=CARTESIAN_POINT('Ctrl Pts',(-1.59103640144185,-5.23837077537817,
40.5326736528633));
#55930=CARTESIAN_POINT('Ctrl Pts',(1.11346637209138,-5.3602348688533,40.6718471102854));
#55931=CARTESIAN_POINT('Ctrl Pts',(3.54568759513793,-4.17133368225729,40.8110205677072));
#55932=CARTESIAN_POINT('Ctrl Pts',(5.11086393910812,-1.96239522190952,40.9501940251292));
#55933=CARTESIAN_POINT('Ctrl Pts',(5.42625493477628,0.726417644241425,41.0893674825512));
#55934=CARTESIAN_POINT('Ctrl Pts',(4.41473643051778,3.23759593836356,41.2285409399732));
#55935=CARTESIAN_POINT('Ctrl Pts',(2.32366015027217,4.95706856086197,41.3677143973951));
#55936=CARTESIAN_POINT('Ctrl Pts',(-0.335632471641556,5.46436419494793,
41.5068878548171));
#55937=CARTESIAN_POINT('Ctrl Pts',(-2.91285119167301,4.63543127941923,41.6460613122389));
#55938=CARTESIAN_POINT('Ctrl Pts',(-4.77777571164161,2.67297296288171,41.785234769661));
#55939=CARTESIAN_POINT('Ctrl Pts',(-5.47436662832414,0.0568790799862881,
41.9244082270828));
#55940=CARTESIAN_POINT('Ctrl Pts',(-4.83228304988656,-2.57312373134837,
42.063581684505));
#55941=CARTESIAN_POINT('Ctrl Pts',(-3.00853691369941,-4.57390761274833,
42.2027551419267));
#55942=CARTESIAN_POINT('Ctrl Pts',(-0.449098065014904,-5.45621078579713,
42.3419285993489));
#55943=CARTESIAN_POINT('Ctrl Pts',(2.22016099964357,-5.00427920351281,42.4811020567706));
#55944=CARTESIAN_POINT('Ctrl Pts',(4.34651289219087,-3.32862597614506,42.6202755141927));
#55945=CARTESIAN_POINT('Ctrl Pts',(5.40999005483213,-0.839007042679954,
42.7594489716146));
#55946=CARTESIAN_POINT('Ctrl Pts',(5.15053505071161,1.85577851653701,42.8986224290366));
#55947=CARTESIAN_POINT('Ctrl Pts',(3.63159372118936,4.09676119090033,43.0377958864585));
#55948=CARTESIAN_POINT('Ctrl Pts',(1.22460045410757,5.33594217911408,43.1769693438805));
#55949=CARTESIAN_POINT('Ctrl Pts',(-1.48185054131569,5.2702983012588,43.3161428013024));
#55950=CARTESIAN_POINT('Ctrl Pts',(-3.82593714649597,3.91588178602361,43.4553162587244));
#55951=CARTESIAN_POINT('Ctrl Pts',(-5.23444803567515,1.60389493822557,43.5944897161463));
#55952=CARTESIAN_POINT('Ctrl Pts',(-5.36295293381699,-1.10030043202433,
43.7336631735683));
#55953=CARTESIAN_POINT('Ctrl Pts',(-4.18002788974679,-3.53543378554715,
43.8728366309903));
#55954=CARTESIAN_POINT('Ctrl Pts',(-1.97493953349668,-5.10602967579324,
44.0120100884122));
#55955=CARTESIAN_POINT('Ctrl Pts',(0.713090752367286,-5.42802236453917,
44.1511835458341));
#55956=CARTESIAN_POINT('Ctrl Pts',(3.22674535831947,-4.42267335484013,44.2903570032561));
#55957=CARTESIAN_POINT('Ctrl Pts',(4.95134763973783,-2.33582571299994,44.4295304606781));
#55958=CARTESIAN_POINT('Ctrl Pts',(5.46517189845383,0.322213176949267,44.5687039181));
#55959=CARTESIAN_POINT('Ctrl Pts',(4.64257009574122,2.90145965286068,44.7078773755219));
#55960=CARTESIAN_POINT('Ctrl Pts',(2.68469720124231,4.77119755917639,44.8470508329439));
#55961=CARTESIAN_POINT('Ctrl Pts',(0.0703217532190181,5.47421045102153,
44.9862242903658));
#55962=CARTESIAN_POINT('Ctrl Pts',(-2.56124982796045,4.83858703857042,45.1253977477878));
#55963=CARTESIAN_POINT('Ctrl Pts',(-4.56650606471606,3.01975952220713,45.2645712052098));
#55964=CARTESIAN_POINT('Ctrl Pts',(-5.45509153100881,0.462494972259141,
45.4037446626316));
#55965=CARTESIAN_POINT('Ctrl Pts',(-5.00971593898958,-2.20786580699166,
45.5429181200538));
#55966=CARTESIAN_POINT('Ctrl Pts',(-3.33928922952715,-4.33832601963165,
45.6820915774755));
#55967=CARTESIAN_POINT('Ctrl Pts',(-0.852289274811402,-5.40791347962323,
45.8212650348977));
#55968=CARTESIAN_POINT('Ctrl Pts',(1.84312527690108,-5.15507656826719,45.9604384923194));
#55969=CARTESIAN_POINT('Ctrl Pts',(4.08783110429599,-3.64164277130519,46.0996119497416));
#55970=CARTESIAN_POINT('Ctrl Pts',(5.33291896467962,-1.23769969185162,46.2387854071634));
#55971=CARTESIAN_POINT('Ctrl Pts',(5.27392124087496,1.46890433864736,46.3779588645854));
#55972=CARTESIAN_POINT('Ctrl Pts',(3.92526494398478,3.816309779168,46.5171323220073));
#55973=CARTESIAN_POINT('Ctrl Pts',(1.61674380356837,5.23049373239969,46.6563057794293));
#55974=CARTESIAN_POINT('Ctrl Pts',(-1.08712785717717,5.36563866032725,46.7954792368512));
#55975=CARTESIAN_POINT('Ctrl Pts',(-3.5251586573914,4.18869689178719,46.9346526942733));
#55976=CARTESIAN_POINT('Ctrl Pts',(-5.10116462326485,1.98747193625476,47.073826151695));
#55977=CARTESIAN_POINT('Ctrl Pts',(-5.4297570634819,-0.699759560576068,
47.2129996091172));
#55978=CARTESIAN_POINT('Ctrl Pts',(-4.43058361056827,-3.21587532109269,
47.3521730665389));
#55979=CARTESIAN_POINT('Ctrl Pts',(-2.34797719076535,-4.94559686212844,
47.4913465239611));
#55980=CARTESIAN_POINT('Ctrl Pts',(0.308791939320552,-5.46594664712891,
47.6305199813829));
#55981=CARTESIAN_POINT('Ctrl Pts',(2.89005061832919,-4.64968091749791,47.769693438805));
#55982=CARTESIAN_POINT('Ctrl Pts',(4.76459063652578,-2.69640525095543,47.9088668962268));
#55983=CARTESIAN_POINT('Ctrl Pts',(5.47402126438588,-0.0837640024137416,
48.0480403536489));
#55984=CARTESIAN_POINT('Ctrl Pts',(4.84486185071238,2.54936048030892,48.1872138110707));
#55985=CARTESIAN_POINT('Ctrl Pts',(3.03096392165112,4.55907698078223,48.3263872684927));
#55986=CARTESIAN_POINT('Ctrl Pts',(0.475889090672027,5.453939382174,48.4655607259146));
#55987=CARTESIAN_POINT('Ctrl Pts',(-2.19555730097171,5.01512246602204,48.6047341833367));
#55988=CARTESIAN_POINT('Ctrl Pts',(-4.33011298709005,3.34993234709049,48.7439076407585));
#55989=CARTESIAN_POINT('Ctrl Pts',(-5.40580429485011,0.865566367662955,
48.8830810981806));
#55990=CARTESIAN_POINT('Ctrl Pts',(-5.15958700085801,-1.8304609232721,49.0222545556024));
#55991=CARTESIAN_POINT('Ctrl Pts',(-3.651669862419,-4.07887636818645,49.1614280130245));
#55992=CARTESIAN_POINT('Ctrl Pts',(-1.25079146630195,-5.32986359289572,
49.3006014704464));
#55993=CARTESIAN_POINT('Ctrl Pts',(1.45594927852757,-5.27751237889635,49.4397749278683));
#55994=CARTESIAN_POINT('Ctrl Pts',(3.8066593996007,-3.93462443271029,49.5789483852903));
#55995=CARTESIAN_POINT('Ctrl Pts',(5.226507889396,-1.62958291999226,49.7181218427122));
#55996=CARTESIAN_POINT('Ctrl Pts',(5.36829203218933,1.07394872697987,49.8572953001341));
#55997=CARTESIAN_POINT('Ctrl Pts',(4.19734063610474,3.51486227262932,49.9964687575562));
#55998=CARTESIAN_POINT('Ctrl Pts',(1.99999235461371,5.09626881085917,50.135642214978));
#55999=CARTESIAN_POINT('Ctrl Pts',(-0.686424149254752,5.43145902114425,
50.2748156724001));
#56000=CARTESIAN_POINT('Ctrl Pts',(-3.20498589222948,4.43846715000337,50.4139891298219));
#56001=CARTESIAN_POINT('Ctrl Pts',(-4.93981626271097,2.36011451029508,50.553162587244));
#56002=CARTESIAN_POINT('Ctrl Pts',(-5.46668843630145,-0.295368839685396,
50.6923360446659));
#56003=CARTESIAN_POINT('Ctrl Pts',(-4.65676370181106,-2.87862415687495,
50.8315095020878));
#56004=CARTESIAN_POINT('Ctrl Pts',(-2.70809704142158,-4.75795498352946,
50.9706829595098));
#56005=CARTESIAN_POINT('Ctrl Pts',(-0.0972057465137546,-5.47379906955798,
51.1098564169317));
#56006=CARTESIAN_POINT('Ctrl Pts',(2.53745576008646,-4.85110744847536,51.2490298743538));
#56007=CARTESIAN_POINT('Ctrl Pts',(4.55162040574421,-3.04215004446889,51.3882033317756));
#56008=CARTESIAN_POINT('Ctrl Pts',(5.45275434624012,-0.489280339487104,
51.5273767891977));
#56009=CARTESIAN_POINT('Ctrl Pts',(5.02049875200887,2.18323555580393,51.6665502466195));
#56010=CARTESIAN_POINT('Ctrl Pts',(3.36055526465709,4.32187384409062,51.8057237040416));
#56011=CARTESIAN_POINT('Ctrl Pts',(0.878838241173826,5.40366251323115,51.9448971614634));
#56012=CARTESIAN_POINT('Ctrl Pts',(-1.81778553201607,5.16406632128618,52.0840706188854));
#56013=CARTESIAN_POINT('Ctrl Pts',(-4.06989703656874,3.66167493406748,52.2232440763074));
#56014=CARTESIAN_POINT('Ctrl Pts',(-5.32677608218628,1.26387569851522,52.3624175337293));
#56015=CARTESIAN_POINT('Ctrl Pts',(-5.28107169366842,-1.44298543907526,
52.5015909911513));
#56016=CARTESIAN_POINT('Ctrl Pts',(-3.94396019576248,-3.7969860659858,52.6407644485732));
#56017=CARTESIAN_POINT('Ctrl Pts',(-1.64241221007741,-5.22249053069871,
52.7799379059952));
#56018=CARTESIAN_POINT('Ctrl Pts',(1.06076312090249,-5.37091303340338,52.9191113634171));
#56019=CARTESIAN_POINT('Ctrl Pts',(3.50454469334802,-4.20595907057776,53.0582848208391));
#56020=CARTESIAN_POINT('Ctrl Pts',(5.09134226809777,-2.01250071307568,53.1974582782611));
#56021=CARTESIAN_POINT('Ctrl Pts',(5.43312822726344,0.673084598815311,53.336631735683));
#56022=CARTESIAN_POINT('Ctrl Pts',(4.44632392560814,3.19407713739254,53.475805193105));
#56023=CARTESIAN_POINT('Ctrl Pts',(2.37223759840168,4.93400587634211,53.6149786505269));
#56024=CARTESIAN_POINT('Ctrl Pts',(-0.281943958984394,5.46739726149851,
53.7541521079489));
#56025=CARTESIAN_POINT('Ctrl Pts',(-2.86718033739894,4.66381840597187,53.8933255653708));
#56026=CARTESIAN_POINT('Ctrl Pts',(-4.75129064020009,2.71977250213987,54.0324990227927));
#56027=CARTESIAN_POINT('Ctrl Pts',(-5.47354386787767,0.110646904466045,
54.1716724802147));
#56028=CARTESIAN_POINT('Ctrl Pts',(-4.85732379419873,-2.52553573907794,
54.3108459376367));
#56029=CARTESIAN_POINT('Ctrl Pts',(-3.0533178232087,-4.54413638456475,54.4500193950586));
#56030=CARTESIAN_POINT('Ctrl Pts',(-0.502668637955831,-5.45153643035289,
54.5891928524806));
#56031=CARTESIAN_POINT('Ctrl Pts',(2.17090064578782,-5.02584476453135,54.7283663099025));
#56032=CARTESIAN_POINT('Ctrl Pts',(4.31360864031496,-3.37115791817132,54.8675397673245));
#56033=CARTESIAN_POINT('Ctrl Pts',(5.40148814768119,-0.8921048153153,55.0067132247464));
#56034=CARTESIAN_POINT('Ctrl Pts',(5.16851450254163,1.80509917956493,55.1458866821683));
#56035=CARTESIAN_POINT('Ctrl Pts',(3.67165792592056,4.06089316358777,55.2850601395904));
#56036=CARTESIAN_POINT('Ctrl Pts',(1.27695230959419,5.3236564511688,55.4242335970122));
#56037=CARTESIAN_POINT('Ctrl Pts',(-1.43001289846173,5.28459916372871,55.5634070544343));
#56038=CARTESIAN_POINT('Ctrl Pts',(-3.787289836653,3.95327217684718,55.7025805118562));
#56039=CARTESIAN_POINT('Ctrl Pts',(-5.21844168053232,1.65523159646386,55.8417539692781));
#56040=CARTESIAN_POINT('Ctrl Pts',(-5.37350164816491,-1.04757111845367,
55.9809274267001));
#56041=CARTESIAN_POINT('Ctrl Pts',(-4.21455214323744,-3.49420598176206,
56.120100884122));
#56042=CARTESIAN_POINT('Ctrl Pts',(-2.02499693621566,-5.08638502468761,
56.259274341544));
#56043=CARTESIAN_POINT('Ctrl Pts',(0.659740989695028,-5.43476467177423,
56.3984477989659));
#56044=CARTESIAN_POINT('Ctrl Pts',(3.1831491223616,-4.45415389000624,56.5376212563878));
#56045=CARTESIAN_POINT('Ctrl Pts',(4.92816573805848,-2.38434638198303,56.6767947138099));
#56046=CARTESIAN_POINT('Ctrl Pts',(5.46807311844585,0.268517378169513,56.8159681712317));
#56047=CARTESIAN_POINT('Ctrl Pts',(4.6708449874405,2.85571922890732,56.9551416286539));
#56048=CARTESIAN_POINT('Ctrl Pts',(2.73143156270733,4.74459764672362,57.0943150860756));
#56049=CARTESIAN_POINT('Ctrl Pts',(0.124087395220497,5.47325566088379,57.2334885434978));
#56050=CARTESIAN_POINT('Ctrl Pts',(-2.51360048916101,4.86351085039795,57.3726620009195));
#56051=CARTESIAN_POINT('Ctrl Pts',(-4.53662496237246,3.06446719052892,57.5118354583416));
#56052=CARTESIAN_POINT('Ctrl Pts',(-5.45028564185634,0.516053905346834,
57.6510089157635));
#56053=CARTESIAN_POINT('Ctrl Pts',(-5.03116047135304,-2.15855264530281,
57.7901823731854));
#56054=CARTESIAN_POINT('Ctrl Pts',(-3.38174024369924,-4.30531742560222,
57.9293558306074));
#56055=CARTESIAN_POINT('Ctrl Pts',(-0.905366010090001,-5.39928121131163,
58.0685292880294));
#56056=CARTESIAN_POINT('Ctrl Pts',(1.7924019424173,-5.17293151780186,58.2077027454513));
#56057=CARTESIAN_POINT('Ctrl Pts',(4.05186480353684,-3.68161877778084,58.3468762028732));
#56058=CARTESIAN_POINT('Ctrl Pts',(5.32050471865464,-1.29002122068698,58.4860496602953));
#56059=CARTESIAN_POINT('Ctrl Pts',(5.28809476780659,1.41703173491132,58.6252231177171));
#56060=CARTESIAN_POINT('Ctrl Pts',(3.96256031981318,3.77757077007051,58.7643965751392));
#56061=CARTESIAN_POINT('Ctrl Pts',(1.66804100185088,5.21436136331128,58.903570032561));
#56062=CARTESIAN_POINT('Ctrl Pts',(-1.03437279918081,5.3760578608646,59.0427434899831));
#56063=CARTESIAN_POINT('Ctrl Pts',(-3.48384620021349,4.22311980226786,59.181916947405));
#56064=CARTESIAN_POINT('Ctrl Pts',(-5.08139711052062,2.037480948682,59.3210904048269));
#56065=CARTESIAN_POINT('Ctrl Pts',(-5.43636834480891,-0.646393402355297,
59.4602638622489));
#56066=CARTESIAN_POINT('Ctrl Pts',(-4.46195699598345,-3.17220191303188,
59.5994373196709));
#56067=CARTESIAN_POINT('Ctrl Pts',(-2.39644078802365,-4.92229588307611,
59.7386107770928));
#56068=CARTESIAN_POINT('Ctrl Pts',(0.255089178202091,-5.46871600306753,
59.8777842345147));
#56069=CARTESIAN_POINT('Ctrl Pts',(2.84424090051047,-4.67784340384815,60.0169576919367));
#56070=CARTESIAN_POINT('Ctrl Pts',(4.73787604345754,-2.74307415281825,60.1561311493586));
#56071=CARTESIAN_POINT('Ctrl Pts',(5.47293445031603,-0.137527137735913,
60.2953046067806));
#56072=CARTESIAN_POINT('Ctrl Pts',(4.86966857976191,2.50165008231294,60.4344780642026));
#56073=CARTESIAN_POINT('Ctrl Pts',(3.07559807920623,4.52908618444462,60.5736515216245));
#56074=CARTESIAN_POINT('Ctrl Pts',(0.529436060934367,5.44900198832429,60.7128249790465));
#56075=CARTESIAN_POINT('Ctrl Pts',(-2.1461916287808,5.03644584035882,60.8519984364684));
#56076=CARTESIAN_POINT('Ctrl Pts',(-4.29700024999853,3.39230217755033,60.9911718938904));
#56077=CARTESIAN_POINT('Ctrl Pts',(-5.39704171733157,0.918621745298845,
61.1303453513123));
#56078=CARTESIAN_POINT('Ctrl Pts',(-5.17731734062487,-1.77969389667896,
61.2695188087343));
#56079=CARTESIAN_POINT('Ctrl Pts',(-3.69155742920964,-4.04281201174977,
61.4086922661562));
#56080=CARTESIAN_POINT('Ctrl Pts',(-1.30308235372075,-5.31732090190619,
61.5478657235782));
#56081=CARTESIAN_POINT('Ctrl Pts',(1.40404202812768,-5.2915584882225,61.687039181));
#56082=CARTESIAN_POINT('Ctrl Pts',(3.76782892205851,-3.97182456202382,61.8262126384221));
#56083=CARTESIAN_POINT('Ctrl Pts',(5.21024960907278,-1.68084036193013,61.965386095844));
#56084=CARTESIAN_POINT('Ctrl Pts',(5.37858164549095,1.02116826789435,62.104559553266));
#56085=CARTESIAN_POINT('Ctrl Pts',(4.23166201667799,3.47346536196786,62.243733010688));
#56086=CARTESIAN_POINT('Ctrl Pts',(2.04995263487357,5.07637865165108,62.3829064681099));
#56087=CARTESIAN_POINT('Ctrl Pts',(-0.633041838628581,5.4379390494839,62.5220799255319));
#56088=CARTESIAN_POINT('Ctrl Pts',(-3.16123572883666,4.46973356166634,62.6612533829538));
#56089=CARTESIAN_POINT('Ctrl Pts',(-4.91639604752523,2.40852003127419,62.8004268403757));
#56090=CARTESIAN_POINT('Ctrl Pts',(-5.4693264952344,-0.241658050599369,
62.9396002977978));
#56091=CARTESIAN_POINT('Ctrl Pts',(-4.68481247433395,-2.83274813170046,
63.0787737552196));
#56092=CARTESIAN_POINT('Ctrl Pts',(-2.75470242334704,-4.73112058423557,
63.2179472126416));
#56093=CARTESIAN_POINT('Ctrl Pts',(-0.150961718488229,-5.47259055056005,
63.3571206700635));
#56094=CARTESIAN_POINT('Ctrl Pts',(2.48967613925437,-4.87577682760848,63.4962941274855));
#56095=CARTESIAN_POINT('Ctrl Pts',(4.52153658546732,-3.08674968495679,63.6354675849075));
#56096=CARTESIAN_POINT('Ctrl Pts',(5.44765327151243,-0.542738212792294,
63.7746410423294));
#56097=CARTESIAN_POINT('Ctrl Pts',(5.04176410147828,2.13366548356399,63.9138144997514));
#56098=CARTESIAN_POINT('Ctrl Pts',(3.40271563592693,4.2889787428324,64.0529879571733));
#56099=CARTESIAN_POINT('Ctrl Pts',(1.75568482074802,5.02557757704978,64.1457702621213));
#56100=CARTESIAN_POINT('Ctrl Pts',(0.893815385175997,5.17445361664725,64.1921614145953));
#56101=CARTESIAN_POINT('Ctrl Pts',(-2.43856727558399,5.02329722221656,-0.192161414595295));
#56102=CARTESIAN_POINT('Ctrl Pts',(-3.27525973866718,4.6171235936328,-0.145770262121311));
#56103=CARTESIAN_POINT('Ctrl Pts',(-4.7409061902274,3.37901548549523,-0.0529879571733427));
#56104=CARTESIAN_POINT('Ctrl Pts',(-5.78018190643871,0.693748699029605,
0.0861855002486099));
#56105=CARTESIAN_POINT('Ctrl Pts',(-5.40591960021603,-2.16040399080713,
0.225358957670562));
#56106=CARTESIAN_POINT('Ctrl Pts',(-3.7097635565088,-4.48663573945948,0.364532415092514));
#56107=CARTESIAN_POINT('Ctrl Pts',(-1.10641808766565,-5.71553783957422,
0.503705872514466));
#56108=CARTESIAN_POINT('Ctrl Pts',(1.76747397197042,-5.54688787644949,0.642879329936418));
#56109=CARTESIAN_POINT('Ctrl Pts',(4.20916255196555,-4.02177959155299,0.782052787358371));
#56110=CARTESIAN_POINT('Ctrl Pts',(5.62156037495095,-1.51323079903301,0.921226244780322));
#56111=CARTESIAN_POINT('Ctrl Pts',(5.65929121063359,1.36536905471062,1.06039970220228));
#56112=CARTESIAN_POINT('Ctrl Pts',(4.31312622178469,3.91008160895074,1.19957315962423));
#56113=CARTESIAN_POINT('Ctrl Pts',(1.91225111807969,5.4986456196878,1.33874661704618));
#56114=CARTESIAN_POINT('Ctrl Pts',(-0.95623660784315,5.74259630620146,1.47792007446813));
#56115=CARTESIAN_POINT('Ctrl Pts',(-3.59089086470998,4.58228184574727,1.61709353189008));
#56116=CARTESIAN_POINT('Ctrl Pts',(-5.34744651334115,2.3014384196533,1.75626698931204));
#56117=CARTESIAN_POINT('Ctrl Pts',(-5.79636405509312,-0.542187118398736,
1.89544044673399));
#56118=CARTESIAN_POINT('Ctrl Pts',(-4.82786746047639,-3.25322902643482,
2.03461390415594));
#56119=CARTESIAN_POINT('Ctrl Pts',(-2.67878806713384,-5.16874236244017,
2.17378736157789));
#56120=CARTESIAN_POINT('Ctrl Pts',(0.12534888559152,-5.82031707927296,2.31296081899985));
#56121=CARTESIAN_POINT('Ctrl Pts',(2.89883364474431,-5.04862027513358,2.4521342764218));
#56122=CARTESIAN_POINT('Ctrl Pts',(4.96345198432844,-3.04235888834433,2.59130773384375));
#56123=CARTESIAN_POINT('Ctrl Pts',(5.814332365256,-0.292134126616094,2.7304811912657));
#56124=CARTESIAN_POINT('Ctrl Pts',(5.24340471369441,2.52952766498078,2.86965464868766));
#56125=CARTESIAN_POINT('Ctrl Pts',(3.39028084955746,4.73263129387092,3.00882810610961));
#56126=CARTESIAN_POINT('Ctrl Pts',(0.708114501950619,5.7784407111682,3.14800156353156));
#56127=CARTESIAN_POINT('Ctrl Pts',(-2.14721065790853,5.41121886381668,3.28717502095351));
#56128=CARTESIAN_POINT('Ctrl Pts',(-4.47746756084426,3.72076436268896,3.42634847837546));
#56129=CARTESIAN_POINT('Ctrl Pts',(-5.71282672794544,1.1204525771617,3.56552193579742));
#56130=CARTESIAN_POINT('Ctrl Pts',(-5.55119954850806,-1.75384913087046,
3.70469539321937));
#56131=CARTESIAN_POINT('Ctrl Pts',(-4.03210953227885,-4.19927326103818,
3.84386885064132));
#56132=CARTESIAN_POINT('Ctrl Pts',(-1.52702742621441,-5.6178279112831,3.98304230806327));
#56133=CARTESIAN_POINT('Ctrl Pts',(1.35146640171921,-5.66262675497904,4.12221576548523));
#56134=CARTESIAN_POINT('Ctrl Pts',(3.89947933097964,-4.32271490483154,4.26138922290718));
#56135=CARTESIAN_POINT('Ctrl Pts',(5.49393290277561,-1.92574776670952,4.40056268032913));
#56136=CARTESIAN_POINT('Ctrl Pts',(5.74492733962891,0.942132190072912,4.53973613775108));
#56137=CARTESIAN_POINT('Ctrl Pts',(4.59108570538524,3.57962780844535,4.67890959517303));
#56138=CARTESIAN_POINT('Ctrl Pts',(2.31456271711773,5.34177897611984,4.81808305259498));
#56139=CARTESIAN_POINT('Ctrl Pts',(-0.527951971583234,5.7976779763013,4.95725651001694));
#56140=CARTESIAN_POINT('Ctrl Pts',(-3.24136390064256,4.835841526022,5.09642996743889));
#56141=CARTESIAN_POINT('Ctrl Pts',(-5.16214875924906,2.69147234586779,5.23560342486085));
#56142=CARTESIAN_POINT('Ctrl Pts',(-5.82060733370272,-0.111056148113278,
5.37477688228279));
#56143=CARTESIAN_POINT('Ctrl Pts',(-5.05572342622942,-2.88642752181006,
5.51395033970475));
#56144=CARTESIAN_POINT('Ctrl Pts',(-3.05453795830575,-4.95596620876867,
5.65312379712669));
#56145=CARTESIAN_POINT('Ctrl Pts',(-0.306410910327196,-5.81359747103461,
5.79229725454865));
#56146=CARTESIAN_POINT('Ctrl Pts',(2.51664434369428,-5.24960040846341,5.93147071197061));
#56147=CARTESIAN_POINT('Ctrl Pts',(4.72429185743747,-3.40189206867849,6.07064416939256));
#56148=CARTESIAN_POINT('Ctrl Pts',(5.77668444464111,-0.722301895490428,
6.20981762681451));
#56149=CARTESIAN_POINT('Ctrl Pts',(5.41647523561366,2.13391640491643,6.34899108423645));
#56150=CARTESIAN_POINT('Ctrl Pts',(3.7317480058439,4.46831735914848,6.48816454165842));
#56151=CARTESIAN_POINT('Ctrl Pts',(1.13447760591239,5.71005812254752,6.62733799908035));
#56152=CARTESIAN_POINT('Ctrl Pts',(-1.74021232753414,5.55548956045152,6.76651145650233));
#56153=CARTESIAN_POINT('Ctrl Pts',(-4.18935935946756,4.04240910329832,6.90568491392425));
#56154=CARTESIAN_POINT('Ctrl Pts',(-5.61406120784397,1.5408179502359,7.04485837134623));
#56155=CARTESIAN_POINT('Ctrl Pts',(-5.66592834067543,-1.33755719112062,
7.18403182876816));
#56156=CARTESIAN_POINT('Ctrl Pts',(-4.33227742625066,-3.88885272325741,
7.32320528619014));
#56157=CARTESIAN_POINT('Ctrl Pts',(-1.93923285223794,-5.48918747593746,
7.46237874361206));
#56158=CARTESIAN_POINT('Ctrl Pts',(0.928022116445518,-5.74722351684494,
7.60155220103404));
#56159=CARTESIAN_POINT('Ctrl Pts',(3.56834315422174,-4.59986199085434,7.74072565845597));
#56160=CARTESIAN_POINT('Ctrl Pts',(5.33607923473955,-2.32767300146927,7.87989911587794));
#56161=CARTESIAN_POINT('Ctrl Pts',(5.79895693428468,0.513713612335872,8.01907257329988));
#56162=CARTESIAN_POINT('Ctrl Pts',(4.84378643331985,3.22947924433246,8.15824603072184));
#56163=CARTESIAN_POINT('Ctrl Pts',(2.70414039420875,5.15552402085338,8.29741948814379));
#56164=CARTESIAN_POINT('Ctrl Pts',(-0.096762740512612,5.82086249392957,
8.43659294556575));
#56165=CARTESIAN_POINT('Ctrl Pts',(-2.8740039940344,5.06279608946103,8.57576640298769));
#56166=CARTESIAN_POINT('Ctrl Pts',(-4.94845054875377,3.06669861051362,8.71493986040966));
#56167=CARTESIAN_POINT('Ctrl Pts',(-5.81282752104771,0.320685845864631,
8.85411331783159));
#56168=CARTESIAN_POINT('Ctrl Pts',(-5.25576444825995,-2.50374584684515,
8.99328677525356));
#56169=CARTESIAN_POINT('Ctrl Pts',(-3.41348277450347,-4.71592393379662,
9.13246023267551));
#56170=CARTESIAN_POINT('Ctrl Pts',(-0.736484933562084,-5.77489334480071,
9.27163369009745));
#56171=CARTESIAN_POINT('Ctrl Pts',(2.12060928446497,-5.42169894625556,9.4108071475194));
#56172=CARTESIAN_POINT('Ctrl Pts',(4.45914021362855,-3.7427091466461,9.54998060494137));
#56173=CARTESIAN_POINT('Ctrl Pts',(5.7072550856607,-1.14849579380492,9.6891540623633));
#56174=CARTESIAN_POINT('Ctrl Pts',(5.5597460729518,1.72656503077199,9.82832751978527));
#56175=CARTESIAN_POINT('Ctrl Pts',(4.05268429870575,4.1794201961769,9.96750097720722));
#56176=CARTESIAN_POINT('Ctrl Pts',(1.5545991831692,5.610260651777,10.1066744346292));
#56177=CARTESIAN_POINT('Ctrl Pts',(-1.32363991509035,5.66919576098472,10.2458478920511));
#56178=CARTESIAN_POINT('Ctrl Pts',(-3.87820266586403,4.34181382416067,10.3850213494731));
#56179=CARTESIAN_POINT('Ctrl Pts',(-5.48440894945526,1.95270624424735,10.524194806895));
#56180=CARTESIAN_POINT('Ctrl Pts',(-5.74948503846692,-0.913906446871129,
10.663368264317));
#56181=CARTESIAN_POINT('Ctrl Pts',(-4.60861053928669,-3.55703698299067,
10.8025417217389));
#56182=CARTESIAN_POINT('Ctrl Pts',(-2.34076925001888,-5.33034731695352,
10.9417151791609));
#56183=CARTESIAN_POINT('Ctrl Pts',(0.499472155410101,-5.80020092472301,
11.0808886365829));
#56184=CARTESIAN_POINT('Ctrl Pts',(3.21757511435457,-4.8517021327235,11.2200620940048));
#56185=CARTESIAN_POINT('Ctrl Pts',(5.14886819479476,-2.71679213666018,11.3592355514268));
#56186=CARTESIAN_POINT('Ctrl Pts',(5.82108255452146,0.0824687494353655,
11.4984090088487));
#56187=CARTESIAN_POINT('Ctrl Pts',(5.06983822417648,2.86156313609655,11.6375824662707));
#56188=CARTESIAN_POINT('Ctrl Pts',(3.07884077061625,4.94090504972305,11.7767559236926));
#56189=CARTESIAN_POINT('Ctrl Pts',(0.334958847675559,5.81202251987648,11.9159293811145));
#56190=CARTESIAN_POINT('Ctrl Pts',(-2.49083225247991,5.26189679594663,12.0551028385365));
#56191=CARTESIAN_POINT('Ctrl Pts',(-4.70752757326881,3.42505289712457,12.1942762959584));
#56192=CARTESIAN_POINT('Ctrl Pts',(-5.77306742251802,0.75066353065058,12.3334497533804));
#56193=CARTESIAN_POINT('Ctrl Pts',(-5.42688996420728,-2.10728937679993,
12.4726232108023));
#56194=CARTESIAN_POINT('Ctrl Pts',(-3.75364771901881,-4.44993617962017,
12.6117966682243));
#56195=CARTESIAN_POINT('Ctrl Pts',(-1.16250705630058,-5.70441763418834,
12.7509701256463));
#56196=CARTESIAN_POINT('Ctrl Pts',(1.71290732287186,-5.56396906034169,12.8901435830682));
#56197=CARTESIAN_POINT('Ctrl Pts',(4.16945583110153,-4.06293505654238,13.0293170404902));
#56198=CARTESIAN_POINT('Ctrl Pts',(5.60642626599816,-1.56837104191373,13.1684904979121));
#56199=CARTESIAN_POINT('Ctrl Pts',(5.67242899620512,1.3097146575491,13.3076639553341));
#56200=CARTESIAN_POINT('Ctrl Pts',(4.35132404105704,3.86752922301908,13.446837412756));
#56201=CARTESIAN_POINT('Ctrl Pts',(1.96616786149375,5.47959735214338,13.586010870178));
#56202=CARTESIAN_POINT('Ctrl Pts',(-0.899785266466895,5.75171189085794,
13.7251843275999));
#56203=CARTESIAN_POINT('Ctrl Pts',(-3.54570936292791,4.61733129792882,13.8643577850219));
#56204=CARTESIAN_POINT('Ctrl Pts',(-5.32458325732504,2.35385138379666,14.0035312424438));
#56205=CARTESIAN_POINT('Ctrl Pts',(-5.80140994011502,-0.485227686681423,
14.1427046998658));
#56206=CARTESIAN_POINT('Ctrl Pts',(-4.85958857650155,-3.2056515824904,14.2818781572877));
#56207=CARTESIAN_POINT('Ctrl Pts',(-2.72942749693245,-5.14218132120763,
14.4210516147097));
#56208=CARTESIAN_POINT('Ctrl Pts',(0.068174261073915,-5.82126751415142,
14.5602250721316));
#56209=CARTESIAN_POINT('Ctrl Pts',(2.84910502301452,-5.07684978791188,14.6993985295536));
#56210=CARTESIAN_POINT('Ctrl Pts',(4.93332975717568,-3.09096436539676,14.8385719869756));
#56211=CARTESIAN_POINT('Ctrl Pts',(5.81118247237508,-0.349229829694178,
14.9777454443975));
#56212=CARTESIAN_POINT('Ctrl Pts',(5.26799741454557,2.47790363846716,15.1169189018194));
#56213=CARTESIAN_POINT('Ctrl Pts',(3.43660236677431,4.69910282648388,15.2560923592414));
#56214=CARTESIAN_POINT('Ctrl Pts',(0.764837601259375,5.77120668880326,15.3952658166634));
#56215=CARTESIAN_POINT('Ctrl Pts',(-2.09395676223998,5.43204825816717,15.5344392740853));
#56216=CARTESIAN_POINT('Ctrl Pts',(-4.4407053126234,3.76456365700274,15.6736127315073));
#56217=CARTESIAN_POINT('Ctrl Pts',(-5.70154578524018,1.17651130891186,15.8127861889292));
#56218=CARTESIAN_POINT('Ctrl Pts',(-5.56815849715669,-1.69923928618934,
15.9519596463512));
#56219=CARTESIAN_POINT('Ctrl Pts',(-4.07316131499641,-4.15946632432628,
16.0911331037731));
#56220=CARTESIAN_POINT('Ctrl Pts',(-1.5821334434256,-5.60255807362867,16.2303065611951));
#56221=CARTESIAN_POINT('Ctrl Pts',(1.29578150246575,-5.6756280268403,16.369480018617));
#56222=CARTESIAN_POINT('Ctrl Pts',(3.8568324590831,-4.36080801959346,16.508653476039));
#56223=CARTESIAN_POINT('Ctrl Pts',(5.47475271301557,-1.97961762280401,16.6478269334609));
#56224=CARTESIAN_POINT('Ctrl Pts',(5.75390406059017,0.885658660383087,16.7870003908829));
#56225=CARTESIAN_POINT('Ctrl Pts',(4.62602421419481,3.5343603623387,16.9261738483048));
#56226=CARTESIAN_POINT('Ctrl Pts',(2.36691932391769,5.31878709061123,17.0653473057268));
#56227=CARTESIAN_POINT('Ctrl Pts',(-0.470980292043627,5.80258397317041,
17.2045207631488));
#56228=CARTESIAN_POINT('Ctrl Pts',(-3.19370872063852,4.86744571709895,17.3436942205707));
#56229=CARTESIAN_POINT('Ctrl Pts',(-5.13546344041366,2.7420463988347,17.4828676779926));
#56230=CARTESIAN_POINT('Ctrl Pts',(-5.82141737170413,-0.0538793616236169,
17.6220411354146));
#56231=CARTESIAN_POINT('Ctrl Pts',(-5.08383073838774,-2.83662972991039,
17.7612145928365));
#56232=CARTESIAN_POINT('Ctrl Pts',(-3.10306932175022,-4.92572471679043,
17.9003880502585));
#56233=CARTESIAN_POINT('Ctrl Pts',(-0.363498705866874,-5.81030738360895,
18.0395615076804));
#56234=CARTESIAN_POINT('Ctrl Pts',(2.46496008276608,-5.2740662672702,18.1787349651024));
#56235=CARTESIAN_POINT('Ctrl Pts',(4.6906497442428,-3.4481311138097,18.3179084225244));
#56236=CARTESIAN_POINT('Ctrl Pts',(5.7693111548766,-0.779007059919226,18.4570818799463));
#56237=CARTESIAN_POINT('Ctrl Pts',(5.43717379703085,2.08061152118044,18.5962553373683));
#56238=CARTESIAN_POINT('Ctrl Pts',(3.77545689477508,4.43144766830016,18.7354287947902));
#56239=CARTESIAN_POINT('Ctrl Pts',(1.19050846719343,5.6986395561334,18.8746022522122));
#56240=CARTESIAN_POINT('Ctrl Pts',(-1.68556100314242,5.57231435813462,19.0137757096341));
#56241=CARTESIAN_POINT('Ctrl Pts',(-4.14945173608767,4.0833630124037,19.1529491670561));
#56242=CARTESIAN_POINT('Ctrl Pts',(-5.59865609799368,1.59588630471778,19.292122624478));
#56243=CARTESIAN_POINT('Ctrl Pts',(-5.67879283360018,-1.28184053385698,
19.4312960819));
#56244=CARTESIAN_POINT('Ctrl Pts',(-4.3702657025817,-3.84611243855737,19.5704695393219));
#56245=CARTESIAN_POINT('Ctrl Pts',(-1.99305544707629,-5.46987506128495,
19.7096429967438));
#56246=CARTESIAN_POINT('Ctrl Pts',(0.871526713802932,-5.75606153444484,
19.8488164541659));
#56247=CARTESIAN_POINT('Ctrl Pts',(3.52299004965729,-4.63468923566654,19.9879899115878));
#56248=CARTESIAN_POINT('Ctrl Pts',(5.31295885176283,-2.37997299158259,20.1271633690097));
#56249=CARTESIAN_POINT('Ctrl Pts',(5.80372301680978,0.456730057408082,20.2663368264317));
#56250=CARTESIAN_POINT('Ctrl Pts',(4.87527350713739,3.18174660081407,20.4055102838537));
#56251=CARTESIAN_POINT('Ctrl Pts',(2.75464876627528,5.12871459292147,20.5446837412756));
#56252=CARTESIAN_POINT('Ctrl Pts',(-0.0395841372822963,5.82153212627597,
20.6838571986975));
#56253=CARTESIAN_POINT('Ctrl Pts',(-2.82413733200982,5.09078103350911,20.8230306561195));
#56254=CARTESIAN_POINT('Ctrl Pts',(-4.91808997442551,3.11515556668409,20.9622041135414));
#56255=CARTESIAN_POINT('Ctrl Pts',(-5.80939725885485,0.377765390152733,
21.1013775709634));
#56256=CARTESIAN_POINT('Ctrl Pts',(-5.28010331752553,-2.45200166342593,
21.2405510283853));
#56257=CARTESIAN_POINT('Ctrl Pts',(-3.45963906871272,-4.68216837751742,
21.3797244858073));
#56258=CARTESIAN_POINT('Ctrl Pts',(-0.793171821188707,-5.76738083216808,
21.5188979432292));
#56259=CARTESIAN_POINT('Ctrl Pts',(2.06725373409271,-5.44226654989145,21.6580714006512));
#56260=CARTESIAN_POINT('Ctrl Pts',(4.42216330247374,-3.78632736664991,21.7972448580731));
#56261=CARTESIAN_POINT('Ctrl Pts',(5.6956989643925,-1.20449844674284,21.9364183154952));
#56262=CARTESIAN_POINT('Ctrl Pts',(5.57643661821572,1.67187255621067,22.075591772917));
#56263=CARTESIAN_POINT('Ctrl Pts',(4.0935400872484,4.13941212677331,22.214765230339));
#56264=CARTESIAN_POINT('Ctrl Pts',(1.60962954286109,5.59472036262192,22.353938687761));
#56265=CARTESIAN_POINT('Ctrl Pts',(-1.26789183578624,5.68192339740111,22.4931121451829));
#56266=CARTESIAN_POINT('Ctrl Pts',(-3.83536922608317,4.37969703299233,22.6322856026049));
#56267=CARTESIAN_POINT('Ctrl Pts',(-5.46496442636354,2.00648125328111,22.7714590600268));
#56268=CARTESIAN_POINT('Ctrl Pts',(-5.75818429941249,-0.857389511941446,
22.9106325174488));
#56269=CARTESIAN_POINT('Ctrl Pts',(-4.64332631009428,-3.51159849344621,
23.0498059748707));
#56270=CARTESIAN_POINT('Ctrl Pts',(-2.39301230807819,-5.30709857592394,
23.1889794322927));
#56271=CARTESIAN_POINT('Ctrl Pts',(0.442477068703314,-5.80482706416472,
23.3281528897146));
#56272=CARTESIAN_POINT('Ctrl Pts',(3.16976529514827,-4.88307189941549,23.4673263471366));
#56273=CARTESIAN_POINT('Ctrl Pts',(5.12193481942643,-2.76723452326229,23.6064998045585));
#56274=CARTESIAN_POINT('Ctrl Pts',(5.82161177717496,0.0252886742497559,
23.7456732619805));
#56275=CARTESIAN_POINT('Ctrl Pts',(5.0977006313659,2.81162790464161,23.8848467194024));
#56276=CARTESIAN_POINT('Ctrl Pts',(3.12722302731866,4.91042557611817,24.0240201768244));
#56277=CARTESIAN_POINT('Ctrl Pts',(0.39202979652405,5.80845210360083,24.1631936342463));
#56278=CARTESIAN_POINT('Ctrl Pts',(-2.43902845858562,5.28610852890829,24.3023670916683));
#56279=CARTESIAN_POINT('Ctrl Pts',(-4.67365877745015,3.47112616209074,24.4415405490902));
#56280=CARTESIAN_POINT('Ctrl Pts',(-5.76541573231747,0.807331799654702,
24.5807140065122));
#56281=CARTESIAN_POINT('Ctrl Pts',(-5.44732648603983,-2.05388348152386,
24.7198874639342));
#56282=CARTESIAN_POINT('Ctrl Pts',(-3.79717500707861,-4.41285227112865,
24.8590609213561));
#56283=CARTESIAN_POINT('Ctrl Pts',(-1.21848116320093,-5.69272402774911,
24.9982343787781));
#56284=CARTESIAN_POINT('Ctrl Pts',(1.65817402793505,-5.58052525254293,25.1374078362));
#56285=CARTESIAN_POINT('Ctrl Pts',(4.12934755692176,-4.10369247816303,25.276581293622));
#56286=CARTESIAN_POINT('Ctrl Pts',(5.5907508912458,-1.62336307498414,25.4157547510439));
#56287=CARTESIAN_POINT('Ctrl Pts',(5.68501969936585,1.25393549236386,25.5549282084659));
#56288=CARTESIAN_POINT('Ctrl Pts',(4.38910195395465,3.82460288644182,25.6941016658878));
#56289=CARTESIAN_POINT('Ctrl Pts',(2.01989496046113,5.46002083786238,25.8332751233098));
#56290=CARTESIAN_POINT('Ctrl Pts',(-0.843247140045628,5.76027234269287,
25.9724485807317));
#56291=CARTESIAN_POINT('Ctrl Pts',(-3.5001857623963,4.6519353853967,26.1116220381537));
#56292=CARTESIAN_POINT('Ctrl Pts',(-5.30120629843185,2.40603719477776,26.2507954955756));
#56293=CARTESIAN_POINT('Ctrl Pts',(-5.80589610857789,-0.428221411874423,
26.3899689529976));
#56294=CARTESIAN_POINT('Ctrl Pts',(-4.89084084690916,-3.15776487588807,
26.5291424104195));
#56295=CARTESIAN_POINT('Ctrl Pts',(-2.77980359390399,-5.11512416081038,
26.6683158678415));
#56296=CARTESIAN_POINT('Ctrl Pts',(0.0109930587272379,-5.82165632392082,
26.8074893252635));
#56297=CARTESIAN_POINT('Ctrl Pts',(2.79910152323723,-5.10458949023314,26.9466627826854));
#56298=CARTESIAN_POINT('Ctrl Pts',(4.90273156808454,-3.13927163088748,27.0858362401074));
#56299=CARTESIAN_POINT('Ctrl Pts',(5.80747192354612,-0.406291838966868,
27.2250096975293));
#56300=CARTESIAN_POINT('Ctrl Pts',(5.29208186520726,2.42604054647321,27.3641831549512));
#56301=CARTESIAN_POINT('Ctrl Pts',(3.48259232467691,4.66512099535361,27.5033566123732));
#56302=CARTESIAN_POINT('Ctrl Pts',(0.821486909932954,5.76341586717429,27.6425300697952));
#56303=CARTESIAN_POINT('Ctrl Pts',(-2.04050084409615,5.45235357496472,27.7817035272171));
#56304=CARTESIAN_POINT('Ctrl Pts',(-4.40351463041004,3.80799975065023,27.920876984639));
#56305=CARTESIAN_POINT('Ctrl Pts',(-5.68971476414206,1.23245653225239,28.0600504420611));
#56306=CARTESIAN_POINT('Ctrl Pts',(-5.58458023646188,-1.64446550091725,
28.1992238994829));
#56307=CARTESIAN_POINT('Ctrl Pts',(-4.11382012392897,-4.11925808722209,
28.338397356905));
#56308=CARTESIAN_POINT('Ctrl Pts',(-1.63708681827409,-5.58674770780111,
28.4775708143268));
#56309=CARTESIAN_POINT('Ctrl Pts',(1.23997158774619,-5.68808172082379,28.6167442717488));
#56310=CARTESIAN_POINT('Ctrl Pts',(3.81381348455404,-4.39848040875725,28.7559177291707));
#56311=CARTESIAN_POINT('Ctrl Pts',(5.45504432559113,-2.03329648773209,28.8950911865927));
#56312=CARTESIAN_POINT('Ctrl Pts',(5.76232565169517,0.829099683393584,29.0342646440147));
#56313=CARTESIAN_POINT('Ctrl Pts',(4.66051640966128,3.48875192532595,29.1734381014366));
#56314=CARTESIAN_POINT('Ctrl Pts',(2.4190475731416,5.29528205481685,29.3126115588586));
#56315=CARTESIAN_POINT('Ctrl Pts',(-0.413963172882623,5.80693014360295,
29.4517850162805));
#56316=CARTESIAN_POINT('Ctrl Pts',(-3.14574541539564,4.89858030277191,29.5909584737025));
#56317=CARTESIAN_POINT('Ctrl Pts',(-5.10828265814138,2.79235590240922,29.7301319311244));
#56318=CARTESIAN_POINT('Ctrl Pts',(-5.82166576624494,0.00330262308311963,
29.8693053885464));
#56319=CARTESIAN_POINT('Ctrl Pts',(-5.1114475685712,-2.78655826333045,30.0084788459683));
#56320=CARTESIAN_POINT('Ctrl Pts',(-3.15130130473782,-4.89500799671923,
30.1476523033903));
#56321=CARTESIAN_POINT('Ctrl Pts',(-0.420551431481474,-5.8064567246012,
30.2868257608123));
#56322=CARTESIAN_POINT('Ctrl Pts',(2.41303800540543,-5.29802329040337,30.4259992182342));
#56323=CARTESIAN_POINT('Ctrl Pts',(4.6565550827104,-3.4940374873306,30.5651726756561));
#56324=CARTESIAN_POINT('Ctrl Pts',(5.76138124879765,-0.835637066668541,
30.7043461330781));
#56325=CARTESIAN_POINT('Ctrl Pts',(5.4573477863529,2.02710590250649,30.8435195905));
#56326=CARTESIAN_POINT('Ctrl Pts',(3.81880153209184,4.39415043662375,30.9826930479221));
#56327=CARTESIAN_POINT('Ctrl Pts',(1.24642446962601,5.6866711917171,31.1218665053439));
#56328=CARTESIAN_POINT('Ctrl Pts',(-1.63074705781936,5.58860154552112,31.261039962766));
#56329=CARTESIAN_POINT('Ctrl Pts',(-4.10914377851356,4.12392296347676,31.4002134201878));
#56330=CARTESIAN_POINT('Ctrl Pts',(-5.58271083642691,1.65080068997717,31.5393868776098));
#56331=CARTESIAN_POINT('Ctrl Pts',(-5.69110944331103,-1.22600020613517,
31.6785603350318));
#56332=CARTESIAN_POINT('Ctrl Pts',(-4.40783234084832,-3.80300108547963,
31.8177337924537));
#56333=CARTESIAN_POINT('Ctrl Pts',(-2.04668575428317,-5.45003491955803,
31.9569072498757));
#56334=CARTESIAN_POINT('Ctrl Pts',(0.814947227294078,-5.76434421403799,
32.0960807072976));
#56335=CARTESIAN_POINT('Ctrl Pts',(3.47729705118092,-4.66906933114471,32.2352541647196));
#56336=CARTESIAN_POINT('Ctrl Pts',(5.28932588080193,-2.43204336471751,32.3744276221415));
#56337=CARTESIAN_POINT('Ctrl Pts',(5.8079291630047,0.399702437704683,32.5136010795635));
#56338=CARTESIAN_POINT('Ctrl Pts',(4.906290220335,3.13370698614799,32.6527745369854));
#56339=CARTESIAN_POINT('Ctrl Pts',(2.80489137308793,5.10141035267351,32.7919479944074));
#56340=CARTESIAN_POINT('Ctrl Pts',(0.0175982849787489,5.82164010409038,
32.9311214518293));
#56341=CARTESIAN_POINT('Ctrl Pts',(-2.77399820055673,5.11827482502606,33.0702949092513));
#56342=CARTESIAN_POINT('Ctrl Pts',(-4.88725490859519,3.16331197633109,33.2094683666733));
#56343=CARTESIAN_POINT('Ctrl Pts',(-5.80540651288768,0.434808488082928,
33.3486418240952));
#56344=CARTESIAN_POINT('Ctrl Pts',(-5.30393276867,-2.40002091378723,33.4878152815172));
#56345=CARTESIAN_POINT('Ctrl Pts',(-3.5054615810378,-4.64796109117274,33.6269887389391));
#56346=CARTESIAN_POINT('Ctrl Pts',(-0.849782184536431,-5.75931188945624,
33.766162196361));
#56347=CARTESIAN_POINT('Ctrl Pts',(2.013698737526,-5.46230909008945,33.905335653783));
#56348=CARTESIAN_POINT('Ctrl Pts',(4.38475974623548,-3.82958028626905,34.044509111205));
#56349=CARTESIAN_POINT('Ctrl Pts',(5.68359332882687,-1.26038489109569,34.1836825686269));
#56350=CARTESIAN_POINT('Ctrl Pts',(5.59258915547232,1.61701878136309,34.3228560260489));
#56351=CARTESIAN_POINT('Ctrl Pts',(4.13400093588665,4.09900469178505,34.4620294834708));
#56352=CARTESIAN_POINT('Ctrl Pts',(1.66450460739921,5.57864030146543,34.6012029408928));
#56353=CARTESIAN_POINT('Ctrl Pts',(-1.21202143177777,5.69410284857053,34.7403763983147));
#56354=CARTESIAN_POINT('Ctrl Pts',(-3.79216575441697,4.41715769383601,34.8795498557367));
#56355=CARTESIAN_POINT('Ctrl Pts',(-5.44499264996964,2.06006267937756,35.0187233131586));
#56356=CARTESIAN_POINT('Ctrl Pts',(-5.76632801754946,-0.80078985708593,
35.1578967705806));
#56357=CARTESIAN_POINT('Ctrl Pts',(-4.67759409827316,-3.46582120903368,
35.2970702280025));
#56358=CARTESIAN_POINT('Ctrl Pts',(-2.4450244911413,-5.28333781230264,35.4362436854245));
#56359=CARTESIAN_POINT('Ctrl Pts',(0.385439292332358,-5.80889316075911,
35.5754171428464));
#56360=CARTESIAN_POINT('Ctrl Pts',(3.12164966073643,-4.91397055310791,35.7145906002684));
#56361=CARTESIAN_POINT('Ctrl Pts',(5.09450728584655,-2.81740993035165,35.8537640576903));
#56362=CARTESIAN_POINT('Ctrl Pts',(5.82157933761185,-0.0318938407573063,
35.9929375151123));
#56363=CARTESIAN_POINT('Ctrl Pts',(5.12507121842963,2.76142141065283,36.1321109725343));
#56364=CARTESIAN_POINT('Ctrl Pts',(3.17530357324334,4.87947235046327,36.2712844299562));
#56365=CARTESIAN_POINT('Ctrl Pts',(0.449062922801674,5.8043212947383,36.4104578873782));
#56366=CARTESIAN_POINT('Ctrl Pts',(-2.38698935011123,5.3098102643732,36.5496313448001));
#56367=CARTESIAN_POINT('Ctrl Pts',(-4.63933907256208,3.51686453691161,36.6888048022221));
#56368=CARTESIAN_POINT('Ctrl Pts',(-5.75720780162824,0.863922178242041,
36.827978259644));
#56369=CARTESIAN_POINT('Ctrl Pts',(-5.46723745625785,-2.00027942999941,
36.967151717066));
#56370=CARTESIAN_POINT('Ctrl Pts',(-3.84033594818631,-4.37534261587085,
37.1063251744879));
#56371=CARTESIAN_POINT('Ctrl Pts',(-1.27433771248041,-5.68048119403081,
37.2454986319099));
#56372=CARTESIAN_POINT('Ctrl Pts',(1.60328075432964,-5.59654304227027,37.3846720893318));
#56373=CARTESIAN_POINT('Ctrl Pts',(4.08884088817506,-4.1440539803887,37.5238455467538));
#56374=CARTESIAN_POINT('Ctrl Pts',(5.5745361274619,-1.6781984879059,37.6630190041757));
#56375=CARTESIAN_POINT('Ctrl Pts',(5.69706191855208,1.19803534896567,37.8021924615977));
#56376=CARTESIAN_POINT('Ctrl Pts',(4.42645641148869,3.78130755670287,37.9413659190196));
#56377=CARTESIAN_POINT('Ctrl Pts',(2.07342718235268,5.43991754723071,38.0805393764416));
#56378=CARTESIAN_POINT('Ctrl Pts',(-0.786627658137758,5.76827705026729,
38.2197128338635));
#56379=CARTESIAN_POINT('Ctrl Pts',(-3.45432446808336,4.68609065964246,38.3588862912855));
#56380=CARTESIAN_POINT('Ctrl Pts',(-5.27731788542694,2.45799087413699,38.4980597487074));
#56381=CARTESIAN_POINT('Ctrl Pts',(-5.80982213105326,-0.371173822772242,
38.6372332061294));
#56382=CARTESIAN_POINT('Ctrl Pts',(-4.92162125477832,-3.10957351186651,
38.7764066635514));
#56383=CARTESIAN_POINT('Ctrl Pts',(-2.82991149871363,-5.08757349928589,
38.9155801209733));
#56384=CARTESIAN_POINT('Ctrl Pts',(-0.0461892042167428,-5.82148346717581,
39.0547535783952));
#56385=CARTESIAN_POINT('Ctrl Pts',(2.74882796945665,-5.1318367077997,39.1939270358172));
#56386=CARTESIAN_POINT('Ctrl Pts',(4.87166036925221,-3.18727602316538,39.3331004932391));
#56387=CARTESIAN_POINT('Ctrl Pts',(5.80320107669691,-0.463314649683628,
39.4722739506611));
#56388=CARTESIAN_POINT('Ctrl Pts',(5.31565574207175,2.37394339295762,39.611447408083));
#56389=CARTESIAN_POINT('Ctrl Pts',(3.52824628619234,4.63068907886911,39.750620865505));
#56390=CARTESIAN_POINT('Ctrl Pts',(0.878056962521374,5.75506899800126,39.8897943229269));
#56391=CARTESIAN_POINT('Ctrl Pts',(-1.98684806084503,5.47213285514013,40.0289677803489));
#56392=CARTESIAN_POINT('Ctrl Pts',(-4.36589910231502,3.85106845298709,40.1681412377708));
#56393=CARTESIAN_POINT('Ctrl Pts',(-5.67733480609507,1.28828284964488,40.3073146951929));
#56394=CARTESIAN_POINT('Ctrl Pts',(-5.6004631820731,-1.58953305955909,40.4464881526147));
#56395=CARTESIAN_POINT('Ctrl Pts',(-4.15408203636321,-4.07865242897112,
40.5856616100368));
#56396=CARTESIAN_POINT('Ctrl Pts',(-1.69188224892336,-5.57039833916441,
40.7248350674586));
#56397=CARTESIAN_POINT('Ctrl Pts',(1.18404204203471,-5.69998663541256,40.8640085248806));
#56398=CARTESIAN_POINT('Ctrl Pts',(3.77042655781207,-4.43572843773523,41.0031819823026));
#56399=CARTESIAN_POINT('Ctrl Pts',(5.43480964194405,-2.08677918262082,41.1423554397245));
#56400=CARTESIAN_POINT('Ctrl Pts',(5.77019130043884,0.772460715847387,41.2815288971464));
#56401=CARTESIAN_POINT('Ctrl Pts',(4.69455896401856,3.44280689765496,41.4207023545685));
#56402=CARTESIAN_POINT('Ctrl Pts',(2.47094243551778,5.27126613647471,41.5598758119903));
#56403=CARTESIAN_POINT('Ctrl Pts',(-0.356906115044386,5.81071606828552,
41.6990492694124));
#56404=CARTESIAN_POINT('Ctrl Pts',(-3.09747861235679,4.92924227921288,41.8382227268342));
#56405=CARTESIAN_POINT('Ctrl Pts',(-5.08060903480191,2.84239600279005,41.9773961842563));
#56406=CARTESIAN_POINT('Ctrl Pts',(-5.82135249336035,0.0604842891567615,
42.1165696416782));
#56407=CARTESIAN_POINT('Ctrl Pts',(-5.13857125234072,-2.736217952906,42.2557430991002));
#56408=CARTESIAN_POINT('Ctrl Pts',(-3.19922925390397,-4.86381901206784,
42.3949165565221));
#56409=CARTESIAN_POINT('Ctrl Pts',(-0.477563582791606,-5.80204586551837,
42.534090013944));
#56410=CARTESIAN_POINT('Ctrl Pts',(2.36088312099284,-5.32146916651771,42.673263471366));
#56411=CARTESIAN_POINT('Ctrl Pts',(4.62201116225283,-3.53960676024863,42.812436928788));
#56412=CARTESIAN_POINT('Ctrl Pts',(5.75289549147219,-0.892186452142408,
42.9516103862099));
#56413=CARTESIAN_POINT('Ctrl Pts',(5.47699525721726,1.97340471105329,43.0907838436319));
#56414=CARTESIAN_POINT('Ctrl Pts',(3.86177773595497,4.35642926251191,43.2299573010538));
#56415=CARTESIAN_POINT('Ctrl Pts',(1.30222021850063,5.67415418399216,43.3691307584758));
#56416=CARTESIAN_POINT('Ctrl Pts',(-1.57577577994933,5.60434955124256,43.5083042158977));
#56417=CARTESIAN_POINT('Ctrl Pts',(-4.06843937560915,4.16408504334153,43.6474776733197));
#56418=CARTESIAN_POINT('Ctrl Pts',(-5.56622696152361,1.70555580793924,43.7866511307416));
#56419=CARTESIAN_POINT('Ctrl Pts',(-5.70287698151609,-1.17004159536382,
43.9258245881636));
#56420=CARTESIAN_POINT('Ctrl Pts',(-4.44497371666576,-3.75952282335648,
44.0649980455855));
#56421=CARTESIAN_POINT('Ctrl Pts',(-2.10011859967,-5.4296689649101,44.2041715030075));
#56422=CARTESIAN_POINT('Ctrl Pts',(0.75828911564091,-5.77207075652127,44.3433449604294));
#56423=CARTESIAN_POINT('Ctrl Pts',(3.43126856719911,-4.70299896033786,44.4825184178514));
#56424=CARTESIAN_POINT('Ctrl Pts',(5.26518260193794,-2.483879097186,44.6216918752733));
#56425=CARTESIAN_POINT('Ctrl Pts',(5.81157496706545,0.342636255182992,44.7608653326952));
#56426=CARTESIAN_POINT('Ctrl Pts',(4.93683358045688,3.08536503513943,44.9000387901173));
#56427=CARTESIAN_POINT('Ctrl Pts',(2.85486336729942,5.0736139343903,45.0392122475392));
#56428=CARTESIAN_POINT('Ctrl Pts',(0.0747790093780736,5.82118641695523,
45.1783857049612));
#56429=CARTESIAN_POINT('Ctrl Pts',(-2.7235914370392,5.14527481144343,45.317559162383));
#56430=CARTESIAN_POINT('Ctrl Pts',(-4.85594832619352,3.21116319338118,45.4567326198051));
#56431=CARTESIAN_POINT('Ctrl Pts',(-5.8008556681686,0.491809636204625,45.595906077227));
#56432=CARTESIAN_POINT('Ctrl Pts',(-5.32725050265616,-2.34780861297027,
45.7350795346489));
#56433=CARTESIAN_POINT('Ctrl Pts',(-3.55094589057689,-4.61330537504105,
45.8742529920709));
#56434=CARTESIAN_POINT('Ctrl Pts',(-0.906310561904393,-5.75068729514726,
46.0134264494928));
#56435=CARTESIAN_POINT('Ctrl Pts',(1.95994946168753,-5.48182463316899,46.1525999069148));
#56436=CARTESIAN_POINT('Ctrl Pts',(4.34693315356459,-3.87246373251302,46.2917733643367));
#56437=CARTESIAN_POINT('Ctrl Pts',(5.67093934690125,-1.3161497350054,46.4309468217587));
#56438=CARTESIAN_POINT('Ctrl Pts',(5.60820212634388,1.56200899845666,46.5701202791807));
#56439=CARTESIAN_POINT('Ctrl Pts',(4.17406294100556,4.05820178967379,46.7092937366026));
#56440=CARTESIAN_POINT('Ctrl Pts',(1.71921908250202,5.56202201969288,46.8484671940246));
#56441=CARTESIAN_POINT('Ctrl Pts',(-1.15603409337561,5.70573293943389,46.9876406514465));
#56442=CARTESIAN_POINT('Ctrl Pts',(-3.74859641908543,4.45419219253138,47.1268141088685));
#56443=CARTESIAN_POINT('Ctrl Pts',(-5.42449554712695,2.11344535306392,47.2659875662903));
#56444=CARTESIAN_POINT('Ctrl Pts',(-5.77391540718154,-0.744112942972513,
47.4051610237125));
#56445=CARTESIAN_POINT('Ctrl Pts',(-4.71141059770752,-3.41970954629144,
47.5443344811342));
#56446=CARTESIAN_POINT('Ctrl Pts',(-2.49680078113419,-5.25906731850005,
47.6835079385564));
#56447=CARTESIAN_POINT('Ctrl Pts',(0.328364329234575,-5.81239882221393,
47.8226813959781));
#56448=CARTESIAN_POINT('Ctrl Pts',(3.07323285325868,-4.94439511273513,47.9618548534003));
#56449=CARTESIAN_POINT('Ctrl Pts',(5.06658824023115,-2.86731351706418,48.101028310822));
#56450=CARTESIAN_POINT('Ctrl Pts',(5.82098523896187,-0.0890732786842594,
48.2402017682442));
#56451=CARTESIAN_POINT('Ctrl Pts',(5.15194734468573,2.71094849799351,48.379375225666));
#56452=CARTESIAN_POINT('Ctrl Pts',(3.22307776963596,4.84804835908905,48.518548683088));
#56453=CARTESIAN_POINT('Ctrl Pts',(0.50605272401972,5.79963049182444,48.65772214051));
#56454=CARTESIAN_POINT('Ctrl Pts',(-2.33471994772851,5.33299971562592,48.7968955979319));
#56455=CARTESIAN_POINT('Ctrl Pts',(-4.60457176972921,3.56226360880274,48.9360690553539));
#56456=CARTESIAN_POINT('Ctrl Pts',(-5.74844442234177,0.920429206639673,
49.0752425127758));
#56457=CARTESIAN_POINT('Ctrl Pts',(-5.48662095387445,-1.94648239388221,
49.2144159701978));
#56458=CARTESIAN_POINT('Ctrl Pts',(-3.88312637822522,-4.33741083273409,
49.3535894276197));
#56459=CARTESIAN_POINT('Ctrl Pts',(-1.33007131516494,-5.66769031420763,
49.4927628850416));
#56460=CARTESIAN_POINT('Ctrl Pts',(1.54823279809409,-5.61202088414622,49.6319363424636));
#56461=CARTESIAN_POINT('Ctrl Pts',(4.04793973289715,-4.18401566918912,49.7711097998856));
#56462=CARTESIAN_POINT('Ctrl Pts',(5.55778353902781,-1.7328719902229,49.9102832573075));
#56463=CARTESIAN_POINT('Ctrl Pts',(5.70855449194466,1.14201962053459,50.0494567147295));
#56464=CARTESIAN_POINT('Ctrl Pts',(4.46338380974508,3.7376474108847,50.1886301721514));
#56465=CARTESIAN_POINT('Ctrl Pts',(2.12675936244259,5.41928941979025,50.3278036295734));
#56466=CARTESIAN_POINT('Ctrl Pts',(-0.729932283324382,5.77572524129643,
50.4669770869953));
#56467=CARTESIAN_POINT('Ctrl Pts',(-3.40812990463278,4.71979382540543,50.6061505444173));
#56468=CARTESIAN_POINT('Ctrl Pts',(-5.25292032303615,2.50970740944466,50.7453240018392));
#56469=CARTESIAN_POINT('Ctrl Pts',(-5.81318762876312,-0.31409042325878,
50.8844974592612));
#56470=CARTESIAN_POINT('Ctrl Pts',(-4.95192683045167,-3.06108213987153,
51.0236709166831));
#56471=CARTESIAN_POINT('Ctrl Pts',(-2.87974637700998,-5.05953199468938,
51.1628443741051));
#56472=CARTESIAN_POINT('Ctrl Pts',(-0.103367010880947,-5.8207489605934,
51.302017831527));
#56473=CARTESIAN_POINT('Ctrl Pts',(2.69828921200576,-5.15858881183226,51.4411912889491));
#56474=CARTESIAN_POINT('Ctrl Pts',(4.84011915839122,-3.2349729108235,51.5803647463709));
#56475=CARTESIAN_POINT('Ctrl Pts',(5.79837034387368,-0.520292760351136,
51.719538203793));
#56476=CARTESIAN_POINT('Ctrl Pts',(5.3387167707593,2.32161720419214,51.8587116612148));
#56477=CARTESIAN_POINT('Ctrl Pts',(3.57355984668041,4.59581039898092,51.9978851186368));
#56478=CARTESIAN_POINT('Ctrl Pts',(0.9345423012129,5.74616688658024,52.1370585760588));
#56479=CARTESIAN_POINT('Ctrl Pts',(-1.93300358884367,5.49138419041184,52.2762320334806));
#56480=CARTESIAN_POINT('Ctrl Pts',(-4.32786235743999,3.89376560879588,52.4154054909027));
#56481=CARTESIAN_POINT('Ctrl Pts',(-5.66440710550295,1.34398487503219,52.5545789483246));
#56482=CARTESIAN_POINT('Ctrl Pts',(-5.6158058016225,-1.53444726193202,52.6937524057466));
#56483=CARTESIAN_POINT('Ctrl Pts',(-4.1939431678773,-4.03765326715939,52.8329258631685));
#56484=CARTESIAN_POINT('Ctrl Pts',(-1.74651444877488,-5.55351154508642,
52.9720993205905));
#56485=CARTESIAN_POINT('Ctrl Pts',(1.12799826134796,-5.71134162203449,53.1112727780124));
#56486=CARTESIAN_POINT('Ctrl Pts',(3.72667586477672,-4.47254851288147,53.2504462354344));
#56487=CARTESIAN_POINT('Ctrl Pts',(5.41405061429276,-2.14006054752284,53.3896196928563));
#56488=CARTESIAN_POINT('Ctrl Pts',(5.77750024795265,0.715747222205316,53.5287931502783));
#56489=CARTESIAN_POINT('Ctrl Pts',(4.72814859288117,3.39652971204778,53.6679666077002));
#56490=CARTESIAN_POINT('Ctrl Pts',(2.52259890429111,5.24674165261229,53.8071400651222));
#56491=CARTESIAN_POINT('Ctrl Pts',(-0.29981462332651,5.81394138195658,53.9463135225441));
#56492=CARTESIAN_POINT('Ctrl Pts',(-3.04891296824617,4.95942868819059,54.0854869799661));
#56493=CARTESIAN_POINT('Ctrl Pts',(-5.05244524031375,2.89216187216734,54.2246604373881));
#56494=CARTESIAN_POINT('Ctrl Pts',(-5.82047758327454,0.117660119777667,
54.3638338948099));
#56495=CARTESIAN_POINT('Ctrl Pts',(-5.16519917283532,-2.68561365541081,
54.503007352232));
#56496=CARTESIAN_POINT('Ctrl Pts',(-3.2468485452167,-4.83216077191268,54.6421808096539));
#56497=CARTESIAN_POINT('Ctrl Pts',(-0.534529659332205,-5.79707523191495,
54.7813542670758));
#56498=CARTESIAN_POINT('Ctrl Pts',(2.30850046137003,-5.34440163358274,54.9205277244978));
#56499=CARTESIAN_POINT('Ctrl Pts',(4.58702131562675,-3.58483453609416,55.0597011819197));
#56500=CARTESIAN_POINT('Ctrl Pts',(5.74385470159609,-0.948649760522845,
55.1988746393417));
#56501=CARTESIAN_POINT('Ctrl Pts',(5.49611431405908,1.91951312784842,55.3380480967636));
#56502=CARTESIAN_POINT('Ctrl Pts',(3.904381360071,4.31828778525907,55.4772215541856));
#56503=CARTESIAN_POINT('Ctrl Pts',(1.3578903307091,5.66108974058479,55.6163950116076));
#56504=CARTESIAN_POINT('Ctrl Pts',(-1.52065247309652,5.61955685594985,55.7555684690295));
#56505=CARTESIAN_POINT('Ctrl Pts',(-4.02734245448736,4.2038453772078,55.8947419264515));
#56506=CARTESIAN_POINT('Ctrl Pts',(-5.54920606362863,1.76014637589462,56.0339153838734));
#56507=CARTESIAN_POINT('Ctrl Pts',(-5.7140943128971,-1.11397010036391,56.1730888412954));
#56508=CARTESIAN_POINT('Ctrl Pts',(-4.48168624667778,-3.71568184691945,
56.3122622987173));
#56509=CARTESIAN_POINT('Ctrl Pts',(-2.15334882809892,-5.40877916222438,
56.4514357561393));
#56510=CARTESIAN_POINT('Ctrl Pts',(0.701557845151013,-5.779240416447,56.5906092135613));
#56511=CARTESIAN_POINT('Ctrl Pts',(3.38490903848553,-4.73647484975552,56.7297826709831));
#56512=CARTESIAN_POINT('Ctrl Pts',(5.24053134448586,-2.53547518793791,56.8689561284052));
#56513=CARTESIAN_POINT('Ctrl Pts',(5.81466007724915,0.285537015520778,57.0081295858271));
#56514=CARTESIAN_POINT('Ctrl Pts',(4.96690064071577,3.03672541176262,57.1473030432491));
#56515=CARTESIAN_POINT('Ctrl Pts',(2.90455992767087,5.04532801983738,57.286476500671));
#56516=CARTESIAN_POINT('Ctrl Pts',(0.131952519187058,5.82017110864172,57.4256499580929));
#56517=CARTESIAN_POINT('Ctrl Pts',(-2.67292190464218,5.17177838783446,57.5648234155149));
#56518=CARTESIAN_POINT('Ctrl Pts',(-4.82417324764246,3.25870460120556,57.7039968729369));
#56519=CARTESIAN_POINT('Ctrl Pts',(-5.79574516375778,0.548763335114487,
57.8431703303588));
#56520=CARTESIAN_POINT('Ctrl Pts',(-5.35005426981655,-2.29536979835607,
57.9823437877808));
#56521=CARTESIAN_POINT('Ctrl Pts',(-3.59608760905766,-4.57820457266488,
58.1215172452027));
#56522=CARTESIAN_POINT('Ctrl Pts',(-0.962751499501605,-5.74150788133178,
58.2606907026247));
#56523=CARTESIAN_POINT('Ctrl Pts',(1.90601109224386,-5.50081129629358,58.3998641600466));
#56524=CARTESIAN_POINT('Ctrl Pts',(4.30868717392597,-3.91497356803764,58.5390376174686));
#56525=CARTESIAN_POINT('Ctrl Pts',(5.65773823945683,-1.37178759834585,58.6782110748905));
#56526=CARTESIAN_POINT('Ctrl Pts',(5.62327402450946,1.5068485147701,58.8173845323124));
#56527=CARTESIAN_POINT('Ctrl Pts',(4.21372223747032,4.01700735705519,58.9565579897345));
#56528=CARTESIAN_POINT('Ctrl Pts',(1.77376768938181,5.54486712061639,59.0957314471563));
#56529=CARTESIAN_POINT('Ctrl Pts',(-1.09993522217184,5.71681254793381,59.2349049045784));
#56530=CARTESIAN_POINT('Ctrl Pts',(-3.7046654236064,4.49079695603381,59.3740783620002));
#56531=CARTESIAN_POINT('Ctrl Pts',(-5.40347509537171,2.16662412404312,59.5132518194223));
#56532=CARTESIAN_POINT('Ctrl Pts',(-5.78094573628633,-0.687364237722812,
59.6524252768441));
#56533=CARTESIAN_POINT('Ctrl Pts',(-4.74477254582164,-3.37326795401793,
59.7915987342661));
#56534=CARTESIAN_POINT('Ctrl Pts',(-2.54833618274159,-5.23428943610499,
59.9307721916881));
#56535=CARTESIAN_POINT('Ctrl Pts',(0.271257685934548,-5.81534371030653,
60.06994564911));
#56536=CARTESIAN_POINT('Ctrl Pts',(3.02451954391174,-4.97434264297288,60.209119106532));
#56537=CARTESIAN_POINT('Ctrl Pts',(5.03818037617574,-2.91694046875862,60.3482925639539));
#56538=CARTESIAN_POINT('Ctrl Pts',(5.81982953854485,-0.146244122931207,
60.487466021376));
#56539=CARTESIAN_POINT('Ctrl Pts',(5.17832641715366,2.66021403623932,60.6266394787978));
#56540=CARTESIAN_POINT('Ctrl Pts',(3.2705410073059,4.81615663372771,60.7658129362198));
#56541=CARTESIAN_POINT('Ctrl Pts',(0.562993701855536,5.79438014745602,60.9049863936418));
#56542=CARTESIAN_POINT('Ctrl Pts',(-2.28222529429992,5.35567464531002,61.0441598510637));
#56543=CARTESIAN_POINT('Ctrl Pts',(-4.56936022331354,3.60731899784347,61.1833333084857));
#56544=CARTESIAN_POINT('Ctrl Pts',(-5.73912643983364,0.976847432866766,
61.3225067659076));
#56545=CARTESIAN_POINT('Ctrl Pts',(-5.50547510899733,-1.89249756295959,
61.4616802233296));
#56546=CARTESIAN_POINT('Ctrl Pts',(-3.92554216842628,-4.29906058228176,
61.6008536807515));
#56547=CARTESIAN_POINT('Ctrl Pts',(-1.38567659492106,-5.65435262047561,
61.7400271381735));
#56548=CARTESIAN_POINT('Ctrl Pts',(1.49303547170834,-5.62695728850115,61.8792005955955));
#56549=CARTESIAN_POINT('Ctrl Pts',(4.00664803422118,-4.22357368205809,62.0183740530173));
#56550=CARTESIAN_POINT('Ctrl Pts',(5.54049474799077,-1.78737832085199,62.1575475104394));
#56551=CARTESIAN_POINT('Ctrl Pts',(5.71949629948441,1.08589373822549,62.2967209678611));
#56552=CARTESIAN_POINT('Ctrl Pts',(4.49988060799419,3.69362660894395,62.4358944252834));
#56553=CARTESIAN_POINT('Ctrl Pts',(2.17988631242708,5.39813854777881,62.5750678827051));
#56554=CARTESIAN_POINT('Ctrl Pts',(-0.673166401869321,5.78261599810781,
62.7142413401272));
#56555=CARTESIAN_POINT('Ctrl Pts',(-3.36160669198678,4.75304201937018,62.853414797549));
#56556=CARTESIAN_POINT('Ctrl Pts',(-5.22801564687486,2.56118105368074,62.9925882549711));
#56557=CARTESIAN_POINT('Ctrl Pts',(-5.81599289775397,-0.256975243148529,
63.1317617123929));
#56558=CARTESIAN_POINT('Ctrl Pts',(-4.98175343925368,-3.0122983203602,63.270935169815));
#56559=CARTESIAN_POINT('Ctrl Pts',(-2.92930578263549,-5.03099673064092,
63.4101086272369));
#56560=CARTESIAN_POINT('Ctrl Pts',(-0.160530237740378,-5.81946384113401,
63.5492820846588));
#56561=CARTESIAN_POINT('Ctrl Pts',(2.64748113981279,-5.18482182863154,63.6884555420808));
#56562=CARTESIAN_POINT('Ctrl Pts',(4.80812851288484,-3.2823994436052,63.8276289995028));
#56563=CARTESIAN_POINT('Ctrl Pts',(5.79294594392005,-0.577138993930893,
63.9668024569247));
#56564=CARTESIAN_POINT('Ctrl Pts',(5.36132999774257,2.26890519507368,64.1059759143467));
#56565=CARTESIAN_POINT('Ctrl Pts',(3.61839250022299,4.56083028297295,64.2451493717686));
#56566=CARTESIAN_POINT('Ctrl Pts',(1.8669667018529,5.34411751075773,64.3379316767166));
#56567=CARTESIAN_POINT('Ctrl Pts',(0.950468752709476,5.50242987146594,64.3843228291906));
#56568=CARTESIAN_POINT('Ctrl Pts',(-2.58391981634373,5.3227144339337,-1.4432899320127E-14));
#56569=CARTESIAN_POINT('Ctrl Pts',(-3.47048393011347,4.89233053668302,0.0463911524739698));
#56570=CARTESIAN_POINT('Ctrl Pts',(-5.02349128318444,3.58042411219188,0.139173457421938));
#56571=CARTESIAN_POINT('Ctrl Pts',(-6.12471376929358,0.735100084764204,
0.278346914843891));
#56572=CARTESIAN_POINT('Ctrl Pts',(-5.72814329152084,-2.28917641069296,
0.417520372265842));
#56573=CARTESIAN_POINT('Ctrl Pts',(-3.93088665774734,-4.75406486094537,
0.556693829687795));
#56574=CARTESIAN_POINT('Ctrl Pts',(-1.17236692647549,-6.05621654674303,
0.695867287109747));
#56575=CARTESIAN_POINT('Ctrl Pts',(1.87282551798883,-5.87751408234647,0.835040744531699));
#56576=CARTESIAN_POINT('Ctrl Pts',(4.460052686318,-4.2615006309766,0.974214201953651));
#56577=CARTESIAN_POINT('Ctrl Pts',(5.95663748835038,-1.60342799949463,1.1133876593756));
#56578=CARTESIAN_POINT('Ctrl Pts',(5.99661729738974,1.44675285050091,1.25256111679755));
#56579=CARTESIAN_POINT('Ctrl Pts',(4.57021318478563,4.14314481049915,1.39173457421951));
#56580=CARTESIAN_POINT('Ctrl Pts',(2.02623220909413,5.82639631148172,1.53090803164146));
#56581=CARTESIAN_POINT('Ctrl Pts',(-1.01323377249359,6.0848878525618,1.67008148906341));
#56582=CARTESIAN_POINT('Ctrl Pts',(-3.80492847441726,4.85541202157831,1.80925494648536));
#56583=CARTESIAN_POINT('Ctrl Pts',(-5.66618487462113,2.43861729720475,1.94842840390732));
#56584=CARTESIAN_POINT('Ctrl Pts',(-6.14186046645374,-0.574504568081465,
2.08760186132927));
#56585=CARTESIAN_POINT('Ctrl Pts',(-5.11563594193564,-3.44714006157422,
2.22677531875122));
#56586=CARTESIAN_POINT('Ctrl Pts',(-2.83845913941177,-5.47682893541894,
2.36594877617318));
#56587=CARTESIAN_POINT('Ctrl Pts',(0.132820395270488,-6.16724122771442,
2.50512223359512));
#56588=CARTESIAN_POINT('Ctrl Pts',(3.07162069053227,-5.34954688547102,2.64429569101708));
#56589=CARTESIAN_POINT('Ctrl Pts',(5.25930207798151,-3.22370085858687,2.78346914843903));
#56590=CARTESIAN_POINT('Ctrl Pts',(6.16089979055235,-0.309546989476669,
2.92264260586099));
#56591=CARTESIAN_POINT('Ctrl Pts',(5.55594158934163,2.68030196459035,3.06181606328293));
#56592=CARTESIAN_POINT('Ctrl Pts',(3.5923609563094,5.01472315573198,3.20098952070489));
#56593=CARTESIAN_POINT('Ctrl Pts',(0.750322171608787,6.1228687888378,3.34016297812684));
#56594=CARTESIAN_POINT('Ctrl Pts',(-2.27519667978226,5.7337584215059,3.47933643554879));
#56595=CARTESIAN_POINT('Ctrl Pts',(-4.74435020650838,3.94254317482165,3.61850989297074));
#56596=CARTESIAN_POINT('Ctrl Pts',(-6.05334383737304,1.18723795172224,3.7576833503927));
#56597=CARTESIAN_POINT('Ctrl Pts',(-5.88208275469158,-1.85838855852283,
3.89685680781465));
#56598=CARTESIAN_POINT('Ctrl Pts',(-4.27244629518299,-4.44957393715546,
4.0360302652366));
#56599=CARTESIAN_POINT('Ctrl Pts',(-1.61804698447391,-5.95268254852498,
4.17520372265855));
#56600=CARTESIAN_POINT('Ctrl Pts',(1.43202151996764,-6.0001516592336,4.3143771800805));
#56601=CARTESIAN_POINT('Ctrl Pts',(4.13191057619189,-4.58037340812065,4.45355063750246));
#56602=CARTESIAN_POINT('Ctrl Pts',(5.82140268971859,-2.04053333508643,4.59272409492441));
#56603=CARTESIAN_POINT('Ctrl Pts',(6.08735782889834,0.998288650848016,4.73189755234636));
#56604=CARTESIAN_POINT('Ctrl Pts',(4.86474064154572,3.79299407565527,4.87107100976832));
#56605=CARTESIAN_POINT('Ctrl Pts',(2.45252387777502,5.66017951980371,5.01024446719026));
#56606=CARTESIAN_POINT('Ctrl Pts',(-0.559420925192705,6.14325270487215,
5.14941792461222));
#56607=CARTESIAN_POINT('Ctrl Pts',(-3.43456770650121,5.12408530734228,5.28859138203417));
#56608=CARTESIAN_POINT('Ctrl Pts',(-5.46984231580947,2.85189947362147,5.42776483945613));
#56609=CARTESIAN_POINT('Ctrl Pts',(-6.16754878296635,-0.117675728986478,
5.56693829687808));
#56610=CARTESIAN_POINT('Ctrl Pts',(-5.35707342495131,-3.05847509179701,
5.70611175430003));
#56611=CARTESIAN_POINT('Ctrl Pts',(-3.23660587069502,-5.25137010743336,
5.84528521172199));
#56612=CARTESIAN_POINT('Ctrl Pts',(-0.324674751057878,-6.16012109243705,
5.98445866914392));
#56613=CARTESIAN_POINT('Ctrl Pts',(2.66665072375488,-5.56250658291383,6.12363212656589));
#56614=CARTESIAN_POINT('Ctrl Pts',(5.00588664124526,-3.60466427042304,6.26280558398783));
#56615=CARTESIAN_POINT('Ctrl Pts',(6.12100783879243,-0.765355214853815,
6.4019790414098));
#56616=CARTESIAN_POINT('Ctrl Pts',(5.73932810309077,2.26111001336394,6.54115249883174));
#56617=CARTESIAN_POINT('Ctrl Pts',(3.95418150585638,4.73465460051793,6.6803259562537));
#56618=CARTESIAN_POINT('Ctrl Pts',(1.20209895230915,6.05041020727682,6.81949941367564));
#56619=CARTESIAN_POINT('Ctrl Pts',(-1.84393892380284,5.886628475855,6.9586728710976));
#56620=CARTESIAN_POINT('Ctrl Pts',(-4.43906911041475,4.28335977947497,7.09784632851955));
#56621=CARTESIAN_POINT('Ctrl Pts',(-5.94869132804232,1.63265950251008,7.2370197859415));
#56622=CARTESIAN_POINT('Ctrl Pts',(-6.00365003829891,-1.41728324095633,
7.37619324336345));
#56623=CARTESIAN_POINT('Ctrl Pts',(-4.59050591044546,-4.12065056194135,
7.51536670078541));
#56624=CARTESIAN_POINT('Ctrl Pts',(-2.05482220875044,-5.81637440833104,
7.65454015820736));
#56625=CARTESIAN_POINT('Ctrl Pts',(0.983337536223896,-6.08979087139413,
7.79371361562931));
#56626=CARTESIAN_POINT('Ctrl Pts',(3.78103679157256,-4.87404004376625,7.93288707305127));
#56627=CARTESIAN_POINT('Ctrl Pts',(5.65414004127548,-2.4664156099708,8.07206053047321));
#56628=CARTESIAN_POINT('Ctrl Pts',(6.14460789605782,0.544333878392784,8.21123398789517));
#56629=CARTESIAN_POINT('Ctrl Pts',(5.13250377650304,3.42197465677996,8.35040744531711));
#56630=CARTESIAN_POINT('Ctrl Pts',(2.86532261001403,5.46282270515937,8.48958090273908));
#56631=CARTESIAN_POINT('Ctrl Pts',(-0.102530352636915,6.16781915220042,
8.62875436016102));
#56632=CARTESIAN_POINT('Ctrl Pts',(-3.04531105079234,5.36456765931648,8.76792781758298));
#56633=CARTESIAN_POINT('Ctrl Pts',(-5.24340647114583,3.24949136724629,8.90710127500493));
#56634=CARTESIAN_POINT('Ctrl Pts',(-6.15930524903233,0.339800554303714,
9.04627473242688));
#56635=CARTESIAN_POINT('Ctrl Pts',(-5.56903803469641,-2.65298340280655,
9.18544818984883));
#56636=CARTESIAN_POINT('Ctrl Pts',(-3.61694584853098,-4.99701994155083,
9.32462164727079));
#56637=CARTESIAN_POINT('Ctrl Pts',(-0.780383643019917,-6.11910997916929,
9.46379510469274));
#56638=CARTESIAN_POINT('Ctrl Pts',(2.24700971251217,-5.74486317672912,9.60296856211469));
#56639=CARTESIAN_POINT('Ctrl Pts',(4.72493044469749,-3.96579599326958,9.74214201953664));
#56640=CARTESIAN_POINT('Ctrl Pts',(6.04744009337826,-1.21695270428369,9.8813154769586));
#56641=CARTESIAN_POINT('Ctrl Pts',(5.89113870081706,1.8294781701889,10.0204889343805));
#56642=CARTESIAN_POINT('Ctrl Pts',(4.2942474352292,4.42853751621115,10.1596623918025));
#56643=CARTESIAN_POINT('Ctrl Pts',(1.64726217565612,5.94466423712179,10.2988358492245));
#56644=CARTESIAN_POINT('Ctrl Pts',(-1.40253641576754,6.00711221552488,10.4380093066464));
#56645=CARTESIAN_POINT('Ctrl Pts',(-4.1093657002853,4.60061073215078,10.5771827640684));
#56646=CARTESIAN_POINT('Ctrl Pts',(-5.81131105437156,2.06909869189489,10.7163562214903));
#56647=CARTESIAN_POINT('Ctrl Pts',(-6.09218719262449,-0.968380492102368,
10.8555296789123));
#56648=CARTESIAN_POINT('Ctrl Pts',(-4.88331005566418,-3.76905670794581,
10.9947031363342));
#56649=CARTESIAN_POINT('Ctrl Pts',(-2.4802924697507,-5.64806646844389,11.1338765937562));
#56650=CARTESIAN_POINT('Ctrl Pts',(0.529243549275131,-6.14592603543298,
11.2730500511781));
#56651=CARTESIAN_POINT('Ctrl Pts',(3.40936097264904,-5.14089129681224,11.4122235086001));
#56652=CARTESIAN_POINT('Ctrl Pts',(5.455770153844,-2.87872846859289,11.551396966022));
#56653=CARTESIAN_POINT('Ctrl Pts',(6.16805232966076,0.0873843580322454,
11.690570423444));
#56654=CARTESIAN_POINT('Ctrl Pts',(5.37202954549153,3.03212864664881,11.8297438808659));
#56655=CARTESIAN_POINT('Ctrl Pts',(3.2623572694572,5.23541121726669,11.9689173382879));
#56656=CARTESIAN_POINT('Ctrl Pts',(0.354924308561887,6.15845226519246,12.1080907957098));
#56657=CARTESIAN_POINT('Ctrl Pts',(-2.63930008444389,5.57553590533831,12.2472642531318));
#56658=CARTESIAN_POINT('Ctrl Pts',(-4.98812310996854,3.62920561655853,12.3864377105538));
#56659=CARTESIAN_POINT('Ctrl Pts',(-6.11717522148735,0.795407365494881,
12.5256111679757));
#56660=CARTESIAN_POINT('Ctrl Pts',(-5.75036360900621,-2.23289586225585,
12.6647846253977));
#56661=CARTESIAN_POINT('Ctrl Pts',(-3.97738656704597,-4.71517779768107,
12.8039580828196));
#56662=CARTESIAN_POINT('Ctrl Pts',(-1.23179911806814,-6.04443351358825,
12.9431315402416));
#56663=CARTESIAN_POINT('Ctrl Pts',(1.81500638487368,-5.89561340238062,13.0823049976635));
#56664=CARTESIAN_POINT('Ctrl Pts',(4.4179792180525,-4.30510919679378,13.2214784550855));
#56665=CARTESIAN_POINT('Ctrl Pts',(5.94060130004532,-1.6618549158582,13.3606519125074));
#56666=CARTESIAN_POINT('Ctrl Pts',(6.01053817003534,1.38778113332413,13.4998253699294));
#56667=CARTESIAN_POINT('Ctrl Pts',(4.61068781230449,4.09805605927116,13.6389988273513));
#56668=CARTESIAN_POINT('Ctrl Pts',(2.08336269843318,5.80621265837202,13.7781722847733));
#56669=CARTESIAN_POINT('Ctrl Pts',(-0.953417608674055,6.09454677813966,
13.9173457421952));
#56670=CARTESIAN_POINT('Ctrl Pts',(-3.75705389701448,4.89255062134165,14.0565191996172));
#56671=CARTESIAN_POINT('Ctrl Pts',(-5.64195883793242,2.49415437343771,14.1956926570391));
#56672=CARTESIAN_POINT('Ctrl Pts',(-6.14720711504926,-0.514150028833914,
14.3348661144611));
#56673=CARTESIAN_POINT('Ctrl Pts',(-5.14924781769343,-3.39672673016858,
14.474039571883));
#56674=CARTESIAN_POINT('Ctrl Pts',(-2.89211696852113,-5.44868470439008,
14.613213029305));
#56675=CARTESIAN_POINT('Ctrl Pts',(0.0722378365023835,-6.16824831394129,
14.7523864867269));
#56676=CARTESIAN_POINT('Ctrl Pts',(3.01892795885593,-5.37945903848149,14.8915599441489));
#56677=CARTESIAN_POINT('Ctrl Pts',(5.2273843940071,-3.27520349974674,15.0307334015708));
#56678=CARTESIAN_POINT('Ctrl Pts',(6.15756214606091,-0.370045922636593,
15.1699068589928));
#56679=CARTESIAN_POINT('Ctrl Pts',(5.58200015565758,2.62560085117693,15.3090803164147));
#56680=CARTESIAN_POINT('Ctrl Pts',(3.64144350057961,4.97919620014604,15.4482537738367));
#56681=CARTESIAN_POINT('Ctrl Pts',(0.810426291686102,6.11520357741311,15.5874272312586));
#56682=CARTESIAN_POINT('Ctrl Pts',(-2.21876854770109,5.7558293667546,15.7266006886806));
#56683=CARTESIAN_POINT('Ctrl Pts',(-4.70539671827687,3.98895315729471,15.8657741461025));
#56684=CARTESIAN_POINT('Ctrl Pts',(-6.04139048603638,1.24663810413905,16.0049476035245));
#56685=CARTESIAN_POINT('Ctrl Pts',(-5.90005255356337,-1.80052365512164,
16.1441210609464));
#56686=CARTESIAN_POINT('Ctrl Pts',(-4.31594499867261,-4.40739427960503,
16.2832945183684));
#56687=CARTESIAN_POINT('Ctrl Pts',(-1.67643763512254,-5.93650254131226,
16.4224679757903));
#56688=CARTESIAN_POINT('Ctrl Pts',(1.37301748259998,-6.01392788117193,16.5616414332123));
#56689=CARTESIAN_POINT('Ctrl Pts',(4.08672170709572,-4.62073709014209,16.7008148906342));
#56690=CARTESIAN_POINT('Ctrl Pts',(5.80107925107558,-2.09761414235381,16.8399883480562));
#56691=CARTESIAN_POINT('Ctrl Pts',(6.09686961371142,0.938448976164669,16.9791618054781));
#56692=CARTESIAN_POINT('Ctrl Pts',(4.90176168507831,3.74502843115517,17.1183352629001));
#56693=CARTESIAN_POINT('Ctrl Pts',(2.50800123744496,5.63581718656992,17.257508720322));
#56694=CARTESIAN_POINT('Ctrl Pts',(-0.499053408082674,6.14845112718181,
17.396682177744));
#56695=CARTESIAN_POINT('Ctrl Pts',(-3.38407200552272,5.15757328875699,17.5358556351659));
#56696=CARTESIAN_POINT('Ctrl Pts',(-5.44156639952264,2.90548802906646,17.6750290925879));
#56697=CARTESIAN_POINT('Ctrl Pts',(-6.16840710386026,-0.057090879380428,
17.8142025500099));
#56698=CARTESIAN_POINT('Ctrl Pts',(-5.38685609348673,-3.00570906701349,
17.9533760074318));
#56699=CARTESIAN_POINT('Ctrl Pts',(-3.2880299806525,-5.21932604976855,18.0925494648538));
#56700=CARTESIAN_POINT('Ctrl Pts',(-0.385165305344935,-6.15663489700508,
18.2317229222757));
#56701=CARTESIAN_POINT('Ctrl Pts',(2.61188578561166,-5.58843074667496,18.3708963796977));
#56702=CARTESIAN_POINT('Ctrl Pts',(4.97023926591231,-3.65365942680015,18.5100698371196));
#56703=CARTESIAN_POINT('Ctrl Pts',(6.11319505883557,-0.825440331029876,
18.6492432945416));
#56704=CARTESIAN_POINT('Ctrl Pts',(5.7612604170159,2.20462785403522,18.7884167519635));
#56705=CARTESIAN_POINT('Ctrl Pts',(4.00049569426957,4.69558726546455,18.9275902093855));
#56706=CARTESIAN_POINT('Ctrl Pts',(1.26146957301766,6.03831102907202,19.0667636668074));
#56707=CARTESIAN_POINT('Ctrl Pts',(-1.78603006826333,5.90445612759732,19.2059371242294));
#56708=CARTESIAN_POINT('Ctrl Pts',(-4.39678276469571,4.32675477552601,19.3451105816513));
#56709=CARTESIAN_POINT('Ctrl Pts',(-5.93236798563808,1.69101024551557,19.4842840390733));
#56710=CARTESIAN_POINT('Ctrl Pts',(-6.01728132849471,-1.35824555261966,
19.6234574964952));
#56711=CARTESIAN_POINT('Ctrl Pts',(-4.63075850506662,-4.07536271210495,
19.7626309539172));
#56712=CARTESIAN_POINT('Ctrl Pts',(-2.11185293772081,-5.79591086343658,
19.9018044113391));
#56713=CARTESIAN_POINT('Ctrl Pts',(0.92347468483484,-6.09915568533313,20.0409778687611));
#56714=CARTESIAN_POINT('Ctrl Pts',(3.73298038288122,-4.9109431913316,20.1801513261831));
#56715=CARTESIAN_POINT('Ctrl Pts',(5.62964155139038,-2.52183297827614,20.319324783605));
#56716=CARTESIAN_POINT('Ctrl Pts',(6.14965806432926,0.483953778053599,20.458498241027));
#56717=CARTESIAN_POINT('Ctrl Pts',(5.16586765980059,3.3713968750191,20.5976716984489));
#56718=CARTESIAN_POINT('Ctrl Pts',(2.91884156960177,5.43441528216485,20.7368451558709));
#56719=CARTESIAN_POINT('Ctrl Pts',(-0.0419435780020967,6.16852869846015,
20.8760186132928));
#56720=CARTESIAN_POINT('Ctrl Pts',(-2.99247205083102,5.39422066590322,21.0151920707148));
#56721=CARTESIAN_POINT('Ctrl Pts',(-5.21123623314264,3.30083663483117,21.1543655281367));
#56722=CARTESIAN_POINT('Ctrl Pts',(-6.15567052361625,0.400282365517453,
21.2935389855587));
#56723=CARTESIAN_POINT('Ctrl Pts',(-5.59482763961418,-2.5981549704495,21.4327124429806));
#56724=CARTESIAN_POINT('Ctrl Pts',(-3.66585332155845,-4.96125236127746,
21.5718859004026));
#56725=CARTESIAN_POINT('Ctrl Pts',(-0.840449392991975,-6.11114967786599,
21.7110593578245));
#56726=CARTESIAN_POINT('Ctrl Pts',(2.19047386652622,-5.76665672704107,21.8502328152465));
#56727=CARTESIAN_POINT('Ctrl Pts',(4.68574949839482,-4.01201410836936,21.9894062726684));
#56728=CARTESIAN_POINT('Ctrl Pts',(6.03519516126426,-1.27629343527068,22.1285797300904));
#56729=CARTESIAN_POINT('Ctrl Pts',(5.90882409792905,1.7715257116946,22.2677531875123));
#56730=CARTESIAN_POINT('Ctrl Pts',(4.33753846217141,4.38614473731157,22.4069266449343));
#56731=CARTESIAN_POINT('Ctrl Pts',(1.70557265916508,5.92819765795395,22.5461001023563));
#56732=CARTESIAN_POINT('Ctrl Pts',(-1.34346543245728,6.02059849178258,22.6852735597782));
#56733=CARTESIAN_POINT('Ctrl Pts',(-4.06397914279307,4.64075199664936,22.8244470172002));
#56734=CARTESIAN_POINT('Ctrl Pts',(-5.79070752662021,2.12607899867485,22.9636204746221));
#56735=CARTESIAN_POINT('Ctrl Pts',(-6.10140497921985,-0.908494824978891,
23.102793932044));
#56736=CARTESIAN_POINT('Ctrl Pts',(-4.92009508473742,-3.72090982484188,
23.241967389466));
#56737=CARTESIAN_POINT('Ctrl Pts',(-2.53564951252636,-5.62343196963269,
23.3811408468879));
#56738=CARTESIAN_POINT('Ctrl Pts',(0.468851229797039,-6.15082791921381,
23.5203143043099));
#56739=CARTESIAN_POINT('Ctrl Pts',(3.35870141508839,-5.1741308808094,23.6594877617318));
#56740=CARTESIAN_POINT('Ctrl Pts',(5.42723139543778,-2.93217750960558,23.7986612191538));
#56741=CARTESIAN_POINT('Ctrl Pts',(6.16861309700777,0.0267960237051835,
23.9378346765757));
#56742=CARTESIAN_POINT('Ctrl Pts',(5.4015527113228,2.97921699012736,24.0770081339977));
#56743=CARTESIAN_POINT('Ctrl Pts',(3.31362338505898,5.20311499291073,24.2161815914197));
#56744=CARTESIAN_POINT('Ctrl Pts',(0.415397011998718,6.15466903170957,24.3553550488416));
#56745=CARTESIAN_POINT('Ctrl Pts',(-2.58440848848693,5.60119079590215,24.4945285062636));
#56746=CARTESIAN_POINT('Ctrl Pts',(-4.95223554043221,3.67802511132568,24.6337019636856));
#56747=CARTESIAN_POINT('Ctrl Pts',(-6.10906744683801,0.855453387068176,
24.7728754211075));
#56748=CARTESIAN_POINT('Ctrl Pts',(-5.77201826429046,-2.1763066705222,24.9120488785295));
#56749=CARTESIAN_POINT('Ctrl Pts',(-4.0235083301384,-4.67588347638917,25.0512223359514));
#56750=CARTESIAN_POINT('Ctrl Pts',(-1.29110960151063,-6.03204290140159,
25.1903957933733));
#56751=CARTESIAN_POINT('Ctrl Pts',(1.7570106728763,-5.91315643821987,25.3295692507953));
#56752=CARTESIAN_POINT('Ctrl Pts',(4.37548026159963,-4.34829599358349,25.4687427082172));
#56753=CARTESIAN_POINT('Ctrl Pts',(5.92399158340687,-1.72012478826007,25.6079161656392));
#56754=CARTESIAN_POINT('Ctrl Pts',(6.02387935103308,1.32867721123663,25.7470896230612));
#56755=CARTESIAN_POINT('Ctrl Pts',(4.65071750462981,4.05257106780277,25.8862630804831));
#56756=CARTESIAN_POINT('Ctrl Pts',(2.14029223943311,5.78546927200246,26.0254365379051));
#56757=CARTESIAN_POINT('Ctrl Pts',(-0.893509486925035,6.1036174818084,26.164609995327));
#56758=CARTESIAN_POINT('Ctrl Pts',(-3.70881682982232,4.92921731011009,26.303783452749));
#56759=CARTESIAN_POINT('Ctrl Pts',(-5.61718847874047,2.54945075688227,26.4429569101709));
#56760=CARTESIAN_POINT('Ctrl Pts',(-6.15196068478126,-0.453745854380916,
26.5821303675929));
#56761=CARTESIAN_POINT('Ctrl Pts',(-5.18236290195643,-3.34598570228385,
26.7213038250148));
#56762=CARTESIAN_POINT('Ctrl Pts',(-2.94549576866256,-5.42001478266002,
26.8604772824367));
#56763=CARTESIAN_POINT('Ctrl Pts',(0.0116483078290116,-6.16866029899418,
26.9996507398587));
#56764=CARTESIAN_POINT('Ctrl Pts',(2.96594396483013,-5.40885218553345,27.1388241972807));
#56765=CARTESIAN_POINT('Ctrl Pts',(5.19496237804368,-3.3263901542322,27.2779976547026));
#56766=CARTESIAN_POINT('Ctrl Pts',(6.15363042732399,-0.430509153647837,
27.4171711121246));
#56767=CARTESIAN_POINT('Ctrl Pts',(5.60752017716922,2.5706464226148,27.5563445695465));
#56768=CARTESIAN_POINT('Ctrl Pts',(3.69017472270629,4.94318885774778,27.6955180269685));
#56769=CARTESIAN_POINT('Ctrl Pts',(0.870452222784836,6.10694837830739,27.8346914843904));
#56770=CARTESIAN_POINT('Ctrl Pts',(-2.16212635145099,5.77734499643421,27.9738649418124));
#56771=CARTESIAN_POINT('Ctrl Pts',(-4.66598925893933,4.03497829026688,28.1130383992343));
#56772=CARTESIAN_POINT('Ctrl Pts',(-6.02885426849212,1.30591798239655,28.2522118566564));
#56773=CARTESIAN_POINT('Ctrl Pts',(-5.91745312234585,-1.74248503933367,
28.3913853140782));
#56774=CARTESIAN_POINT('Ctrl Pts',(-4.35902730489465,-4.36478940186638,
28.5305587715003));
#56775=CARTESIAN_POINT('Ctrl Pts',(-1.7346665450516,-5.91974978735934,28.6697322289221));
#56776=CARTESIAN_POINT('Ctrl Pts',(1.31388097813024,-6.02712388646274,28.8089056863441));
#56777=CARTESIAN_POINT('Ctrl Pts',(4.0411385559244,-4.66065496891622,28.948079143766));
#56778=CARTESIAN_POINT('Ctrl Pts',(5.78019613116984,-2.15449257429016,29.087252601188));
#56779=CARTESIAN_POINT('Ctrl Pts',(6.10579317975746,0.878518761034432,29.2264260586099));
#56780=CARTESIAN_POINT('Ctrl Pts',(4.93830981244283,3.69670147074295,29.3655995160319));
#56781=CARTESIAN_POINT('Ctrl Pts',(2.56323662812275,5.61091111636177,29.5047729734539));
#56782=CARTESIAN_POINT('Ctrl Pts',(-0.438637742890223,6.15305635420109,
29.6439464308758));
#56783=CARTESIAN_POINT('Ctrl Pts',(-3.33324981328087,5.19056367360283,29.7831198882978));
#56784=CARTESIAN_POINT('Ctrl Pts',(-5.41276548734757,2.95879626646398,29.9222933457198));
#56785=CARTESIAN_POINT('Ctrl Pts',(-6.16867030413476,0.00349947828611944,
30.0614668031416));
#56786=CARTESIAN_POINT('Ctrl Pts',(-5.41611904451953,-2.9526530549753,30.2006402605636));
#56787=CARTESIAN_POINT('Ctrl Pts',(-3.33913686536758,-5.18677843770153,
30.3398137179856));
#56788=CARTESIAN_POINT('Ctrl Pts',(-0.445618699339021,-6.15255471672228,
30.4789871754075));
#56789=CARTESIAN_POINT('Ctrl Pts',(2.55686885581799,-5.61381574524941,30.6181606328295));
#56790=CARTESIAN_POINT('Ctrl Pts',(4.93411236777539,-3.70230208243847,30.7573340902514));
#56791=CARTESIAN_POINT('Ctrl Pts',(6.10479248505205,-0.885445809699391,
30.8965075476734));
#56792=CARTESIAN_POINT('Ctrl Pts',(5.78263689135225,2.14793299481948,31.0356810050953));
#56793=CARTESIAN_POINT('Ctrl Pts',(4.04642391959121,4.65606690570727,31.1748544625173));
#56794=CARTESIAN_POINT('Ctrl Pts',(1.32071848863418,6.02562928176321,31.3140279199392));
#56795=CARTESIAN_POINT('Ctrl Pts',(-1.72794889865594,5.9217141243981,31.4532013773612));
#56796=CARTESIAN_POINT('Ctrl Pts',(-4.35407222257742,4.36973233139537,31.5923748347831));
#56797=CARTESIAN_POINT('Ctrl Pts',(-5.91547229538928,1.74919784185328,31.7315482922051));
#56798=CARTESIAN_POINT('Ctrl Pts',(-6.03033207850711,-1.299076822359,31.870721749627));
#56799=CARTESIAN_POINT('Ctrl Pts',(-4.67056432958597,-4.0296816760957,32.009895207049));
#56800=CARTESIAN_POINT('Ctrl Pts',(-2.16867991761837,-5.77488813591925,
32.1490686644709));
#56801=CARTESIAN_POINT('Ctrl Pts',(0.863522737700732,-6.10793205994764,
32.2882421218929));
#56802=CARTESIAN_POINT('Ctrl Pts',(3.68456382065906,-4.9473725369081,32.4274155793149));
#56803=CARTESIAN_POINT('Ctrl Pts',(5.60459992034892,-2.57700704311941,32.5665890367368));
#56804=CARTESIAN_POINT('Ctrl Pts',(6.15411492086643,0.423526986426445,32.7057624941588));
#56805=CARTESIAN_POINT('Ctrl Pts',(5.19873314629818,3.32049382487648,32.8449359515807));
#56806=CARTESIAN_POINT('Ctrl Pts',(2.97207892280822,5.40548355321348,32.9841094090027));
#56807=CARTESIAN_POINT('Ctrl Pts',(0.0186472432995035,6.16864311236916,
33.1232828664246));
#56808=CARTESIAN_POINT('Ctrl Pts',(-2.9393443407067,5.42335324446212,33.2624563238466));
#56809=CARTESIAN_POINT('Ctrl Pts',(-5.17856322123317,3.35186344160279,33.4016297812685));
#56810=CARTESIAN_POINT('Ctrl Pts',(-6.15144190639095,0.460725557962153,
33.5408032386905));
#56811=CARTESIAN_POINT('Ctrl Pts',(-5.62007746218061,-2.54307587117484,
33.6799766961124));
#56812=CARTESIAN_POINT('Ctrl Pts',(-3.71440711739459,-4.925006125246,33.8191501535344));
#56813=CARTESIAN_POINT('Ctrl Pts',(-0.900434057400942,-6.10259978007199,
33.9583236109563));
#56814=CARTESIAN_POINT('Ctrl Pts',(2.13372668621321,-5.78789391713461,34.0974970683783));
#56815=CARTESIAN_POINT('Ctrl Pts',(4.64611647652438,-4.05784514909464,34.2366705258002));
#56816=CARTESIAN_POINT('Ctrl Pts',(6.02236796066139,-1.33551103097705,34.3758439832222));
#56817=CARTESIAN_POINT('Ctrl Pts',(5.92593941868295,1.71340233849548,34.5150174406441));
#56818=CARTESIAN_POINT('Ctrl Pts',(4.38041100853469,4.34332878835697,34.6541908980661));
#56819=CARTESIAN_POINT('Ctrl Pts',(1.76371859104191,5.91115913328978,34.793364355488));
#56820=CARTESIAN_POINT('Ctrl Pts',(-1.28426483319145,6.0335039078209,34.93253781291));
#56821=CARTESIAN_POINT('Ctrl Pts',(-4.01820049740123,4.68044552688595,35.0717112703319));
#56822=CARTESIAN_POINT('Ctrl Pts',(-5.76954531825774,2.18285418386855,35.2108847277539));
#56823=CARTESIAN_POINT('Ctrl Pts',(-6.11003410948152,-0.848521507349445,
35.3500581851759));
#56824=CARTESIAN_POINT('Ctrl Pts',(-4.95640542885802,-3.67240395276024,
35.4892316425978));
#56825=CARTESIAN_POINT('Ctrl Pts',(-2.5907619188371,-5.59825492875822,35.6284051000198));
#56826=CARTESIAN_POINT('Ctrl Pts',(0.408413676106909,-6.15513637839415,
35.7675785574417));
#56827=CARTESIAN_POINT('Ctrl Pts',(3.30771781398888,-5.20687127078083,35.9067520148636));
#56828=CARTESIAN_POINT('Ctrl Pts',(5.39816902416752,-2.98534365760133,36.0459254722856));
#56829=CARTESIAN_POINT('Ctrl Pts',(6.16857872386138,-0.0337948958706249,
36.1850989297076));
#56830=CARTESIAN_POINT('Ctrl Pts',(5.43055474173921,2.92601790227538,36.3242723871295));
#56831=CARTESIAN_POINT('Ctrl Pts',(3.36456980619704,5.17031677817611,36.4634458445514));
#56832=CARTESIAN_POINT('Ctrl Pts',(0.475829638423382,6.15029200304019,36.6026193019734));
#56833=CARTESIAN_POINT('Ctrl Pts',(-2.52926755185657,5.6263052902049,36.7417927593954));
#56834=CARTESIAN_POINT('Ctrl Pts',(-4.91587018506997,3.7264897545817,36.8809662168174));
#56835=CARTESIAN_POINT('Ctrl Pts',(-6.10037027658913,0.915416875510875,
37.0201396742393));
#56836=CARTESIAN_POINT('Ctrl Pts',(-5.7931160420816,-2.11950751129575,37.1593131316613));
#56837=CARTESIAN_POINT('Ctrl Pts',(-4.06924190990749,-4.6361380313915,37.2984865890831));
#56838=CARTESIAN_POINT('Ctrl Pts',(-1.35029552022647,-6.01907032485238,
37.4376600465052));
#56839=CARTESIAN_POINT('Ctrl Pts',(1.69884544656774,-5.93012897972197,37.5768335039271));
#56840=CARTESIAN_POINT('Ctrl Pts',(4.33255916398767,-4.39106327192045,37.7160069613491));
#56841=CARTESIAN_POINT('Ctrl Pts',(5.90681032706917,-1.77822870505769,37.855180418771));
#56842=CARTESIAN_POINT('Ctrl Pts',(6.03663935527803,1.26944509994355,37.994353876193));
#56843=CARTESIAN_POINT('Ctrl Pts',(4.69029850123278,4.00669508907226,38.1335273336149));
#56844=CARTESIAN_POINT('Ctrl Pts',(2.19701528757021,5.76416771040234,38.2727007910369));
#56845=CARTESIAN_POINT('Ctrl Pts',(-0.833515160437645,6.11209931568384,
38.4118742484588));
#56846=CARTESIAN_POINT('Ctrl Pts',(-3.66022194037028,4.96540843382439,38.5510477058808));
#56847=CARTESIAN_POINT('Ctrl Pts',(-5.59187617984988,2.60450117233415,38.6902211633027));
#56848=CARTESIAN_POINT('Ctrl Pts',(-6.15612072062488,-0.393297903064726,
38.8293946207246));
#56849=CARTESIAN_POINT('Ctrl Pts',(-5.21497799797801,-3.29492185765726,
38.9685680781466));
#56850=CARTESIAN_POINT('Ctrl Pts',(-2.99859039085709,-5.39082194431627,
39.1077415355686));
#56851=CARTESIAN_POINT('Ctrl Pts',(-0.0489423446593162,-6.16847713899966,
39.2469149929905));
#56852=CARTESIAN_POINT('Ctrl Pts',(2.91267382003966,-5.43772349292586,39.3860884504125));
#56853=CARTESIAN_POINT('Ctrl Pts',(5.1620391582563,-3.37725588253109,39.5252619078344));
#56854=CARTESIAN_POINT('Ctrl Pts',(6.14910501360392,-0.490930849645275,
39.6644353652564));
#56855=CARTESIAN_POINT('Ctrl Pts',(5.63249919176854,2.51544398112719,39.8036088226783));
#56856=CARTESIAN_POINT('Ctrl Pts',(3.73854992114163,4.9067046023369,39.9427822801003));
#56857=CARTESIAN_POINT('Ctrl Pts',(0.930394173682962,6.09810398804735,40.0819557375222));
#56858=CARTESIAN_POINT('Ctrl Pts',(-2.10527555580855,5.79830323470386,40.2211291949442));
#56859=CARTESIAN_POINT('Ctrl Pts',(-4.6261316304785,4.08061413330745,40.3603026523661));
#56860=CARTESIAN_POINT('Ctrl Pts',(-6.01573639422086,1.36507186723222,40.4994761097882));
#56861=CARTESIAN_POINT('Ctrl Pts',(-5.93428278225215,-1.68427831065054,
40.63864956721));
#56862=CARTESIAN_POINT('Ctrl Pts',(-4.40168905731968,-4.32176341441019,
40.7778230246321));
#56863=CARTESIAN_POINT('Ctrl Pts',(-1.79272809640488,-5.90242590295064,
40.9169964820539));
#56864=CARTESIAN_POINT('Ctrl Pts',(1.25461771197804,-6.03973840197183,41.056169939476));
#56865=CARTESIAN_POINT('Ctrl Pts',(3.99516552048621,-4.70012319321317,41.1953433968978));
#56866=CARTESIAN_POINT('Ctrl Pts',(5.75875534477997,-2.21116314333212,41.3345168543199));
#56867=CARTESIAN_POINT('Ctrl Pts',(6.11412766610142,0.818503787453346,41.4736903117417));
#56868=CARTESIAN_POINT('Ctrl Pts',(4.97438149751934,3.64801785694636,41.6128637691638));
#56869=CARTESIAN_POINT('Ctrl Pts',(2.61822472076339,5.58546371208744,41.7520372265856));
#56870=CARTESIAN_POINT('Ctrl Pts',(-0.378179758447216,6.15706794162312,
41.8912106840077));
#56871=CARTESIAN_POINT('Ctrl Pts',(-3.28210603304057,5.22305327900653,42.0303841414296));
#56872=CARTESIAN_POINT('Ctrl Pts',(-5.3834423579622,3.01181904269839,42.1695575988515));
#56873=CARTESIAN_POINT('Ctrl Pts',(-6.16833835839655,0.0640894983272365,
42.3087310562735));
#56874=CARTESIAN_POINT('Ctrl Pts',(-5.44485945479489,-2.89931217446363,
42.4479045136954));
#56875=CARTESIAN_POINT('Ctrl Pts',(-3.38992159410854,-5.15373041138735,
42.5870779711174));
#56876=CARTESIAN_POINT('Ctrl Pts',(-0.506029100568308,-6.14788094523961,
42.7262514285393));
#56877=CARTESIAN_POINT('Ctrl Pts',(2.50160524234212,-5.6386591295226,42.8654248859613));
#56878=CARTESIAN_POINT('Ctrl Pts',(4.89750943231479,-3.75058754435221,43.0045983433832));
#56879=CARTESIAN_POINT('Ctrl Pts',(6.09580092811226,-0.945365861604859,
43.1437718008052));
#56880=CARTESIAN_POINT('Ctrl Pts',(5.8034554637229,2.09103090556957,43.2829452582271));
#56881=CARTESIAN_POINT('Ctrl Pts',(4.09196175072059,4.61609733412348,43.4221187156491));
#56882=CARTESIAN_POINT('Ctrl Pts',(1.37983998289368,6.01236618887025,43.561292173071));
#56883=CARTESIAN_POINT('Ctrl Pts',(-1.66970101858295,5.93840080122631,43.700465630493));
#56884=CARTESIAN_POINT('Ctrl Pts',(-4.31094160472234,4.41228830065944,43.839639087915));
#56885=CARTESIAN_POINT('Ctrl Pts',(-5.89800588737206,1.8072166776529,43.9788125453369));
#56886=CARTESIAN_POINT('Ctrl Pts',(-6.04280102921519,-1.23978275870331,
44.1179860027589));
#56887=CARTESIAN_POINT('Ctrl Pts',(-4.70991954358473,-3.98361186116582,
44.2571594601808));
#56888=CARTESIAN_POINT('Ctrl Pts',(-2.22529766584334,-5.75330825402695,
44.3963329176028));
#56889=CARTESIAN_POINT('Ctrl Pts',(0.80348747891454,-6.11611914850338,44.5355063750247));
#56890=CARTESIAN_POINT('Ctrl Pts',(3.63579177607875,-4.98332456583558,44.6746798324467));
#56891=CARTESIAN_POINT('Ctrl Pts',(5.57901756413806,-2.63193248137206,44.8138532898686));
#56892=CARTESIAN_POINT('Ctrl Pts',(6.15797803567706,0.363059333416714,44.9530267472906));
#56893=CARTESIAN_POINT('Ctrl Pts',(5.23109706517253,3.26927041741817,45.0922002047125));
#56894=CARTESIAN_POINT('Ctrl Pts',(3.02502953335652,5.3760303096042,45.2313736621344));
#56895=CARTESIAN_POINT('Ctrl Pts',(0.0792362655371347,6.16816238288892,
45.3705471195565));
#56896=CARTESIAN_POINT('Ctrl Pts',(-2.88593304611797,5.45196258431645,45.5097205769783));
#56897=CARTESIAN_POINT('Ctrl Pts',(-5.14539058767098,3.40256686455523,45.6488940344004));
#56898=CARTESIAN_POINT('Ctrl Pts',(-6.14661980532839,0.521124300150113,
45.7880674918222));
#56899=CARTESIAN_POINT('Ctrl Pts',(-5.64478506632273,-2.48775141894889,
45.9272409492443));
#56900=CARTESIAN_POINT('Ctrl Pts',(-3.76260255162662,-4.88828473045045,
46.0664144066661));
#56901=CARTESIAN_POINT('Ctrl Pts',(-0.96033184899738,-6.0934611106713,46.2055878640882));
#56902=CARTESIAN_POINT('Ctrl Pts',(2.07677364647398,-5.80857269807079,46.34476132151));
#56903=CARTESIAN_POINT('Ctrl Pts',(4.60603520283319,-4.10328469372083,46.4839347789321));
#56904=CARTESIAN_POINT('Ctrl Pts',(6.00895972912288,-1.39459977815919,46.6231082363539));
#56905=CARTESIAN_POINT('Ctrl Pts',(5.9424830118128,1.65511365826597,46.762281693776));
#56906=CARTESIAN_POINT('Ctrl Pts',(4.42286093802635,4.30009380017957,46.9014551511978));
#56907=CARTESIAN_POINT('Ctrl Pts',(1.82169436143568,5.89355030698609,47.0406286086199));
#56908=CARTESIAN_POINT('Ctrl Pts',(-1.22494032957404,6.0458272185405,47.1798020660416));
#56909=CARTESIAN_POINT('Ctrl Pts',(-3.97203418077946,4.71968749327557,47.3189755234639));
#56910=CARTESIAN_POINT('Ctrl Pts',(-5.74782647098904,2.23941876987309,47.4581489808855));
#56911=CARTESIAN_POINT('Ctrl Pts',(-6.11807375088118,-0.788466325368954,
47.5973224383078));
#56912=CARTESIAN_POINT('Ctrl Pts',(-4.99223758484679,-3.62354377149019,
47.7364958957295));
#56913=CARTESIAN_POINT('Ctrl Pts',(-2.64562437150301,-5.57253777487165,
47.8756693531516));
#56914=CARTESIAN_POINT('Ctrl Pts',(0.347936719148598,-6.15885099729895,
48.0148428105735));
#56915=CARTESIAN_POINT('Ctrl Pts',(3.25641508818817,-5.23910930797237,48.1540162679955));
#56916=CARTESIAN_POINT('Ctrl Pts',(5.36858584393653,-3.03822178317292,48.2931897254174));
#56917=CARTESIAN_POINT('Ctrl Pts',(6.16794921353787,-0.0943825549547815,
48.4323631828394));
#56918=CARTESIAN_POINT('Ctrl Pts',(5.45903283865907,2.87253651567811,48.5715366402613));
#56919=CARTESIAN_POINT('Ctrl Pts',(3.41519161762082,5.13701973739587,48.7107100976833));
#56920=CARTESIAN_POINT('Ctrl Pts',(0.536216357367407,6.14532160147488,48.8498835551052));
#56921=CARTESIAN_POINT('Ctrl Pts',(-2.47388259448532,5.65087696522981,48.9890570125272));
#56922=CARTESIAN_POINT('Ctrl Pts',(-4.87903055236837,3.774594870515,49.1282304699491));
#56923=CARTESIAN_POINT('Ctrl Pts',(-6.09108454983344,0.975292045616384,
49.2674039273711));
#56924=CARTESIAN_POINT('Ctrl Pts',(-5.81365490689088,-2.06250386449231,
49.4065773847931));
#56925=CARTESIAN_POINT('Ctrl Pts',(-4.11458289403143,-4.59594529728175,
49.545750842215));
#56926=CARTESIAN_POINT('Ctrl Pts',(-1.40935116402794,-6.00551703551953,
49.684924299637));
#56927=CARTESIAN_POINT('Ctrl Pts',(1.64051631766061,-5.9465293893961,49.8240977570588));
#56928=CARTESIAN_POINT('Ctrl Pts',(4.28922006619361,-4.43340690566795,49.9632712144809));
#56929=CARTESIAN_POINT('Ctrl Pts',(5.88905918865963,-1.83616106045353,50.1024446719028));
#56930=CARTESIAN_POINT('Ctrl Pts',(6.04881695169999,1.21009051408931,50.2416181293247));
#56931=CARTESIAN_POINT('Ctrl Pts',(4.72942698338542,3.96043254914008,50.3807915867467));
#56932=CARTESIAN_POINT('Ctrl Pts',(2.25352637027147,5.74231002872132,50.5199650441686));
#56933=CARTESIAN_POINT('Ctrl Pts',(-0.773440417394008,6.1199914614486,50.6591385015906));
#56934=CARTESIAN_POINT('Ctrl Pts',(-3.61127391703609,5.0011205008075,50.7983119590126));
#56935=CARTESIAN_POINT('Ctrl Pts',(-5.56602438336132,2.65930030859425,50.9374854164345));
#56936=CARTESIAN_POINT('Ctrl Pts',(-6.15968682122481,-0.332812006832159,
51.0766588738565));
#56937=CARTESIAN_POINT('Ctrl Pts',(-5.24708995909226,-3.24354012286813,
51.2158323312784));
#56938=CARTESIAN_POINT('Ctrl Pts',(-3.0513957125984,-5.36110900584928,51.3550057887004));
#56939=CARTESIAN_POINT('Ctrl Pts',(-0.109528275248135,-6.16769885162882,
51.4941792461224));
#56940=CARTESIAN_POINT('Ctrl Pts',(2.85912266392506,-5.46607017518914,51.6333527035443));
#56941=CARTESIAN_POINT('Ctrl Pts',(5.12861791103823,-3.42779577717813,51.7725261609662));
#56942=CARTESIAN_POINT('Ctrl Pts',(6.14398634150724,-0.551305181215167,
51.9116996183881));
#56943=CARTESIAN_POINT('Ctrl Pts',(5.65693478950973,2.45999885258035,52.0508730758102));
#56944=CARTESIAN_POINT('Ctrl Pts',(3.78656442870373,4.86974695387121,52.190046533232));
#56945=CARTESIAN_POINT('Ctrl Pts',(0.990246361251975,6.08867125992932,52.3292199906541));
#56946=CARTESIAN_POINT('Ctrl Pts',(-2.04822164567128,5.8187020595375,52.4683934480759));
#56947=CARTESIAN_POINT('Ctrl Pts',(-4.58582767831123,4.12585628352428,52.607566905498));
#56948=CARTESIAN_POINT('Ctrl Pts',(-6.00203812881962,1.42409405154916,52.7467403629199));
#56949=CARTESIAN_POINT('Ctrl Pts',(-5.95053990957657,-1.62590908478877,
52.8859138203418));
#56950=CARTESIAN_POINT('Ctrl Pts',(-4.44392613999212,-4.27832046833299,
53.0250872777638));
#56951=CARTESIAN_POINT('Ctrl Pts',(-1.85061668747234,-5.88453255947412,
53.1642607351857));
#56952=CARTESIAN_POINT('Ctrl Pts',(1.19523340179344,-6.0517702106656,53.3034341926077));
#56953=CARTESIAN_POINT('Ctrl Pts',(3.94880703620541,-4.73913795518518,53.4426076500296));
#56954=CARTESIAN_POINT('Ctrl Pts',(5.73675896048776,-2.26762038196999,53.5817811074516));
#56955=CARTESIAN_POINT('Ctrl Pts',(6.12187226864186,0.758409845595327,53.7209545648735));
#56956=CARTESIAN_POINT('Ctrl Pts',(5.0099732601542,3.59898228670302,53.8601280222956));
#56957=CARTESIAN_POINT('Ctrl Pts',(2.67296021018055,5.55947742888248,53.9993014797174));
#56958=CARTESIAN_POINT('Ctrl Pts',(-0.31768528766863,6.16048550241465,54.1384749371395));
#56959=CARTESIAN_POINT('Ctrl Pts',(-3.2306455990934,5.25503897040932,54.2776483945613));
#56960=CARTESIAN_POINT('Ctrl Pts',(-5.35359984042742,3.06455124219481,54.4168218519833));
#56961=CARTESIAN_POINT('Ctrl Pts',(-6.16741129867142,0.12467333508929,54.5559953094053));
#56962=CARTESIAN_POINT('Ctrl Pts',(-5.47307455147189,-2.84569157174367,
54.6951687668272));
#56963=CARTESIAN_POINT('Ctrl Pts',(-3.44037926722471,-5.12018515926061,
54.8343422242492));
#56964=CARTESIAN_POINT('Ctrl Pts',(-0.566390680708578,-6.14261403347702,
54.9735156816711));
#56965=CARTESIAN_POINT('Ctrl Pts',(2.44610027695225,-5.66295850263414,55.1126891390931));
#56966=CARTESIAN_POINT('Ctrl Pts',(4.86043399093854,-3.79851115401699,55.251862596515));
#56967=CARTESIAN_POINT('Ctrl Pts',(6.086221255511,-1.00519470573039,55.391036053937));
#56968=CARTESIAN_POINT('Ctrl Pts',(5.82371412557653,2.03392707613192,55.530209511359));
#56969=CARTESIAN_POINT('Ctrl Pts',(4.13710479422145,4.57568240693037,55.6693829687809));
#56970=CARTESIAN_POINT('Ctrl Pts',(1.438828351824,5.99852303000078,55.8085564262028));
#56971=CARTESIAN_POINT('Ctrl Pts',(-1.61129204773131,5.954514548171,55.9477298836248));
#56972=CARTESIAN_POINT('Ctrl Pts',(-4.26739507232172,4.45441857756841,56.0869033410467));
#56973=CARTESIAN_POINT('Ctrl Pts',(-5.87997044672494,1.86506115532538,56.2260767984687));
#56974=CARTESIAN_POINT('Ctrl Pts',(-6.05468697762929,-1.18036908227415,
56.3652502558907));
#56975=CARTESIAN_POINT('Ctrl Pts',(-4.74882035011812,-3.93715771207684,
56.5044237133125));
#56976=CARTESIAN_POINT('Ctrl Pts',(-2.28170071998218,-5.73117329976114,
56.6435971707346));
#56977=CARTESIAN_POINT('Ctrl Pts',(0.743374700607,-6.1237161611198,56.7827706281565));
#56978=CARTESIAN_POINT('Ctrl Pts',(3.58666895460946,-5.01879580950479,56.9219440855785));
#56979=CARTESIAN_POINT('Ctrl Pts',(5.55289695091324,-2.68660399389279,57.0611175430004));
#56980=CARTESIAN_POINT('Ctrl Pts',(6.16124703605245,0.302556652872041,57.2002910004224));
#56981=CARTESIAN_POINT('Ctrl Pts',(5.26295629399103,3.21773159461793,57.3394644578443));
#56982=CARTESIAN_POINT('Ctrl Pts',(3.07768829263442,5.34605839295113,57.4786379152663));
#56983=CARTESIAN_POINT('Ctrl Pts',(0.139817643153607,6.16708655639964,57.6178113726882));
#56984=CARTESIAN_POINT('Ctrl Pts',(-2.83224332012334,5.48004592527096,57.7569848301102));
#56985=CARTESIAN_POINT('Ctrl Pts',(-5.11172153291249,3.4529420118822,57.8961582875321));
#56986=CARTESIAN_POINT('Ctrl Pts',(-6.1412046856592,0.581472764882143,58.0353317449541));
#56987=CARTESIAN_POINT('Ctrl Pts',(-5.66894806828008,-2.43218695140933,
58.174505202376));
#56988=CARTESIAN_POINT('Ctrl Pts',(-3.81043497441608,-4.85109171972752,
58.313678659798));
#56989=CARTESIAN_POINT('Ctrl Pts',(-1.02013698891321,-6.08373455135193,
58.4528521172199));
#56990=CARTESIAN_POINT('Ctrl Pts',(2.01962024207041,-5.82869107478529,58.5920255746419));
#56991=CARTESIAN_POINT('Ctrl Pts',(4.5655095443151,-4.14832835829445,58.7311990320639));
#56992=CARTESIAN_POINT('Ctrl Pts',(5.99497176025902,-1.45355397600471,58.8703724894857));
#56993=CARTESIAN_POINT('Ctrl Pts',(5.95845328121232,1.59666529462889,59.0095459469078));
#56994=CARTESIAN_POINT('Ctrl Pts',(4.46488415512748,4.25644394403988,59.1487194043297));
#56995=CARTESIAN_POINT('Ctrl Pts',(1.87949437691273,5.87537287792151,59.2878928617516));
#56996=CARTESIAN_POINT('Ctrl Pts',(-1.16549764516288,6.05756723500302,59.4270663191736));
#56997=CARTESIAN_POINT('Ctrl Pts',(-3.92548464699931,4.75847410979977,59.5662397765955));
#56998=CARTESIAN_POINT('Ctrl Pts',(-5.7255530802228,2.29576729940424,59.7054132340175));
#56999=CARTESIAN_POINT('Ctrl Pts',(-6.12552312776374,-0.728335073090324,
59.8445866914395));
#57000=CARTESIAN_POINT('Ctrl Pts',(-5.02758809565984,-3.57433399500399,
59.9837601488614));
#57001=CARTESIAN_POINT('Ctrl Pts',(-2.70023157745952,-5.54628298913386,
60.1229336062834));
#57002=CARTESIAN_POINT('Ctrl Pts',(0.287426193667008,-6.16197141754554,
60.2621070637053));
#57003=CARTESIAN_POINT('Ctrl Pts',(3.20479818731301,-5.2708418820976,60.4012805211273));
#57004=CARTESIAN_POINT('Ctrl Pts',(5.33848470889396,-3.090806784699,60.5404539785492));
#57005=CARTESIAN_POINT('Ctrl Pts',(6.16672462677367,-0.154961108126498,
60.6796274359711));
#57006=CARTESIAN_POINT('Ctrl Pts',(5.4869842545454,2.8187779901657,60.8188008933931));
#57007=CARTESIAN_POINT('Ctrl Pts',(3.46548393540557,5.1032270830108,60.9579743508151));
#57008=CARTESIAN_POINT('Ctrl Pts',(0.596551342776706,6.13975830658775,61.097147808237));
#57009=CARTESIAN_POINT('Ctrl Pts',(-2.41825895981904,5.67490345026123,61.236321265659));
#57010=CARTESIAN_POINT('Ctrl Pts',(-4.84172019662853,3.82233581813661,61.3754947230809));
#57011=CARTESIAN_POINT('Ctrl Pts',(-6.08121116233572,1.03507312043469,61.5146681805029));
#57012=CARTESIAN_POINT('Ctrl Pts',(-5.83363287736978,-2.00530122924022,
61.6538416379248));
#57013=CARTESIAN_POINT('Ctrl Pts',(-4.15952690764293,-4.55530915281376,
61.7930150953468));
#57014=CARTESIAN_POINT('Ctrl Pts',(-1.46827083612136,-5.99138433904502,
61.9321885527687));
#57015=CARTESIAN_POINT('Ctrl Pts',(1.58202891528899,-5.96235608877982,62.0713620101907));
#57016=CARTESIAN_POINT('Ctrl Pts',(4.24546714638385,-4.47532280209235,62.2105354676127));
#57017=CARTESIAN_POINT('Ctrl Pts',(5.87073988690873,-1.89391627977385,62.3497089250346));
#57018=CARTESIAN_POINT('Ctrl Pts',(6.06041095347787,1.15061920855663,62.4888823824565));
#57019=CARTESIAN_POINT('Ctrl Pts',(4.76809919931039,3.91378785592005,62.6280558398785));
#57020=CARTESIAN_POINT('Ctrl Pts',(2.3098199899806,5.71989844390654,62.7672292973004));
#57021=CARTESIAN_POINT('Ctrl Pts',(-0.713290965110059,6.12729294673171,
62.9064027547224));
#57022=CARTESIAN_POINT('Ctrl Pts',(-3.5619776551369,5.03635047707401,63.0455762121444));
#57023=CARTESIAN_POINT('Ctrl Pts',(-5.53963524622449,2.71384207608729,63.1847496695663));
#57024=CARTESIAN_POINT('Ctrl Pts',(-6.16265930027355,-0.272292435697687,
63.3239231269883));
#57025=CARTESIAN_POINT('Ctrl Pts',(-5.2786944041734,-3.19184850901995,63.4630965844102));
#57026=CARTESIAN_POINT('Ctrl Pts',(-3.10390914192393,-5.33087287704626,
63.6022700418322));
#57027=CARTESIAN_POINT('Ctrl Pts',(-0.170098756992531,-6.16633713170798,
63.7414434992541));
#57028=CARTESIAN_POINT('Ctrl Pts',(2.8052861403712,-5.49386682965458,63.8806169566761));
#57029=CARTESIAN_POINT('Ctrl Pts',(5.09472044030236,-3.47804920225361,64.019790414098));
#57030=CARTESIAN_POINT('Ctrl Pts',(6.13823861632767,-0.611539775069484,
64.15896387152));
#57031=CARTESIAN_POINT('Ctrl Pts',(5.68089589400686,2.40414490658337,64.2981373289419));
#57032=CARTESIAN_POINT('Ctrl Pts',(3.83406936451904,4.8326818231135,64.4373107863639));
#57033=CARTESIAN_POINT('Ctrl Pts',(1.97824858295778,5.66265744446568,64.5300930913119));
#57034=CARTESIAN_POINT('Ctrl Pts',(1.00712212024295,5.83040612628463,64.5764842437858));
#57035=CARTESIAN_POINT('Ctrl Pts',(-5.91644646386006,0.000128480793576948,
61.5616248077951));
#57036=CARTESIAN_POINT('Ctrl Pts',(-5.91593193090335,-0.652955704091308,
61.5923637511717));
#57037=CARTESIAN_POINT('Ctrl Pts',(-5.80809740540869,-1.30620561360789,
61.6231026945482));
#57038=CARTESIAN_POINT('Ctrl Pts',(-5.59587826324296,-1.92357349155666,
61.6538416379248));
#57039=CARTESIAN_POINT('Ctrl Pts',(-5.27559755412752,-2.85530387043135,
61.7002327903988));
#57040=CARTESIAN_POINT('Ctrl Pts',(-4.71756223088528,-3.70530651162249,
61.7466239428728));
#57041=CARTESIAN_POINT('Ctrl Pts',(-3.99000189067727,-4.36965369658994,
61.7930150953468));
#57042=CARTESIAN_POINT('Ctrl Pts',(-3.26244155046918,-5.03400088155746,
61.8394062478208));
#57043=CARTESIAN_POINT('Ctrl Pts',(-2.36535619329527,-5.51269261030126,
61.8857974002948));
#57044=CARTESIAN_POINT('Ctrl Pts',(-1.40843022280656,-5.74720043296228,
61.9321885527687));
#57045=CARTESIAN_POINT('Ctrl Pts',(-0.451504252317853,-5.9817082556233,
61.9785797052427));
#57046=CARTESIAN_POINT('Ctrl Pts',(0.565262331485657,-5.97203217220155,
62.0249708577167));
#57047=CARTESIAN_POINT('Ctrl Pts',(1.51755199523657,-5.71935524937607,62.0713620101907));
#57048=CARTESIAN_POINT('Ctrl Pts',(2.46984165898738,-5.46667832655061,62.1177531626647));
#57049=CARTESIAN_POINT('Ctrl Pts',(3.3576544026856,-4.97100056432147,62.1641443151387));
#57050=CARTESIAN_POINT('Ctrl Pts',(4.07243956462219,-4.29292726282051,62.2105354676127));
#57051=CARTESIAN_POINT('Ctrl Pts',(4.78722472655881,-3.61485396131952,62.2569266200867));
#57052=CARTESIAN_POINT('Ctrl Pts',(5.32898230673377,-2.75438512054668,62.3033177725606));
#57053=CARTESIAN_POINT('Ctrl Pts',(5.63147294124944,-1.81672811877186,62.3497089250346));
#57054=CARTESIAN_POINT('Ctrl Pts',(5.93396357576511,-0.879071116997042,
62.3961000775086));
#57055=CARTESIAN_POINT('Ctrl Pts',(5.99718726462149,0.135774045779763,62.4424912299826));
#57056=CARTESIAN_POINT('Ctrl Pts',(5.81341381668844,1.10372473506206,62.4888823824565));
#57057=CARTESIAN_POINT('Ctrl Pts',(5.62964036875539,2.07167542434442,62.5352735349305));
#57058=CARTESIAN_POINT('Ctrl Pts',(5.19886978403288,2.99273164013226,62.5816646874045));
#57059=CARTESIAN_POINT('Ctrl Pts',(4.57377129011664,3.75427817935727,62.6280558398785));
#57060=CARTESIAN_POINT('Ctrl Pts',(3.94867279620046,4.51582471858219,62.6744469923525));
#57061=CARTESIAN_POINT('Ctrl Pts',(3.1292463930906,5.11786158124432,62.7208381448265));
#57062=CARTESIAN_POINT('Ctrl Pts',(2.21568136568727,5.4867790963796,62.7672292973004));
#57063=CARTESIAN_POINT('Ctrl Pts',(1.30211633828383,5.85569661151491,62.8136204497744));
#57064=CARTESIAN_POINT('Ctrl Pts',(0.294412686586882,5.99149477912333,62.8600116022484));
#57065=CARTESIAN_POINT('Ctrl Pts',(-0.68422025426609,5.87757011798457,62.9064027547224));
#57066=CARTESIAN_POINT('Ctrl Pts',(-1.66285319511901,5.76364545684581,62.9527939071964));
#57067=CARTESIAN_POINT('Ctrl Pts',(-2.61241542512795,5.39999796695991,62.9991850596704));
#57068=CARTESIAN_POINT('Ctrl Pts',(-3.41680613864703,4.83108948851917,63.0455762121444));
#57069=CARTESIAN_POINT('Ctrl Pts',(-4.22119685216606,4.26218101007847,63.0919673646183));
#57070=CARTESIAN_POINT('Ctrl Pts',(-4.88041604919522,3.48801154308295,63.1383585170923));
#57071=CARTESIAN_POINT('Ctrl Pts',(-5.31386299005133,2.60323772428773,63.1847496695663));
#57072=CARTESIAN_POINT('Ctrl Pts',(-5.70900759272686,1.79664857546361,63.2270413823092));
#57073=CARTESIAN_POINT('Ctrl Pts',(-5.91651851507,0.898138913726484,63.2693330950522));
#57074=CARTESIAN_POINT('Ctrl Pts',(-5.9171574445836,-8.64418186984388E-5,
63.3116248077951));
#57075=CARTESIAN_POINT('',(-2.85728222003707,-4.00342940649516,-1.53523027623947E-15));
#57076=CARTESIAN_POINT('Ctrl Pts',(-2.85728222003706,-4.00342940649517,
-5.3776427755281E-16));
#57077=CARTESIAN_POINT('Ctrl Pts',(-2.95928271123691,-3.94487512701868,
-5.18176765844195E-16));
#57078=CARTESIAN_POINT('Ctrl Pts',(-3.05898490657923,-3.88272744726811,
-7.71266662334843E-16));
#57079=CARTESIAN_POINT('Ctrl Pts',(-3.15618864747685,-3.81711101865418,
-7.21644966006352E-16));
#57080=CARTESIAN_POINT('Ctrl Pts',(-3.27550031648898,-3.73657085075272,
-6.98637490506031E-16));
#57081=CARTESIAN_POINT('Ctrl Pts',(-3.39104882900031,-3.65080626318817,
-5.84937091110779E-16));
#57082=CARTESIAN_POINT('Ctrl Pts',(-3.50262914174305,-3.56021018039735,
-6.52256026967279E-16));
#57083=CARTESIAN_POINT('Ctrl Pts',(-3.61584744679976,-3.46828415253254,
-7.20563200773708E-16));
#57084=CARTESIAN_POINT('Ctrl Pts',(-3.72498077963315,-3.3713833795464,-7.19044273329439E-16));
#57085=CARTESIAN_POINT('Ctrl Pts',(-3.82979628327283,-3.26986793650992,
-6.80011602582908E-16));
#57086=CARTESIAN_POINT('Ctrl Pts',(-3.9300117525662,-3.17280769817535,-6.42691957293752E-16));
#57087=CARTESIAN_POINT('Ctrl Pts',(-4.02628037930183,-3.07152824151411,
-1.00568777733274E-15));
#57088=CARTESIAN_POINT('Ctrl Pts',(-4.11837549701657,-2.96630706901007,
-1.1518563880486E-15));
#57089=CARTESIAN_POINT('Ctrl Pts',(-4.15643398619576,-2.92282421178012,
-1.21226085494441E-15));
#57090=CARTESIAN_POINT('Ctrl Pts',(-4.19377942809832,-2.87866780488849,
-5.54864022283868E-16));
#57091=CARTESIAN_POINT('Ctrl Pts',(-4.23039440888198,-2.83385586799541,
-4.9960036108132E-16));
#57092=CARTESIAN_POINT('Ctrl Pts',(-4.25014618584021,-2.8096822821124,-4.69788642309225E-16));
#57093=CARTESIAN_POINT('Ctrl Pts',(-4.26968538238833,-2.78531792146795,
-3.55933796205804E-16));
#57094=CARTESIAN_POINT('Ctrl Pts',(-4.28900915147612,-2.76076551556,-3.19189119579733E-16));
#57095=CARTESIAN_POINT('Ctrl Pts',(-4.30443367755228,-2.74116741213417,
-2.8985896042683E-16));
#57096=CARTESIAN_POINT('Ctrl Pts',(-4.31972315914379,-2.72144646705537,
-2.13147410180917E-16));
#57097=CARTESIAN_POINT('Ctrl Pts',(-4.33485992958826,-2.70162560333916,
-2.08166817117217E-16));
#57098=CARTESIAN_POINT('Ctrl Pts',(-4.4278307771548,-2.57988480625452,-1.77575750137973E-16));
#57099=CARTESIAN_POINT('Ctrl Pts',(-4.51516326633763,-2.45422884936395,
-1.03603524343314E-15));
#57100=CARTESIAN_POINT('Ctrl Pts',(-4.59662203129057,-2.32508248185065,
-8.88178419700125E-16));
#57101=CARTESIAN_POINT('Ctrl Pts',(-4.67808079624352,-2.19593611433734,
-7.40321595967114E-16));
#57102=CARTESIAN_POINT('Ctrl Pts',(-4.75366645541919,-2.06329874970035,
-1.11603729512037E-16));
#57103=CARTESIAN_POINT('Ctrl Pts',(-4.82311411010153,-1.92754875329055,
2.77555756156289E-17));
#57104=CARTESIAN_POINT('Ctrl Pts',(-4.89136206219792,-1.79414382702721,
1.68047749947343E-16));
#57105=CARTESIAN_POINT('Ctrl Pts',(-4.95368291217718,-1.65773229238894,
-1.11642256479697E-15));
#57106=CARTESIAN_POINT('Ctrl Pts',(-5.01004456451512,-1.51873876158455,
-1.27675647831893E-15));
#57107=CARTESIAN_POINT('Ctrl Pts',(-5.06678008578305,-1.37882323221405,
-1.43815394952959E-15));
#57108=CARTESIAN_POINT('Ctrl Pts',(-5.11747740025848,-1.23629066654526,
-2.18559075597774E-17));
#57109=CARTESIAN_POINT('Ctrl Pts',(-5.1620585192726,-1.09154709310106,0.));
#57110=CARTESIAN_POINT('Ctrl Pts',(-5.17533073261087,-1.04845558645932,
6.50670674602739E-18));
#57111=CARTESIAN_POINT('Ctrl Pts',(-5.18806054212299,-1.00516797275366,
-3.13319586228567E-16));
#57112=CARTESIAN_POINT('Ctrl Pts',(-5.20024505801854,-0.96169464478646,
-3.05311331771918E-16));
#57113=CARTESIAN_POINT('Ctrl Pts',(-5.2055486682428,-0.94277180955312,-3.01825542054964E-16));
#57114=CARTESIAN_POINT('Ctrl Pts',(-5.21074888095922,-0.923813872462111,
1.00782795168963E-16));
#57115=CARTESIAN_POINT('Ctrl Pts',(-5.21584187742371,-0.904835564223655,
1.11022302462516E-16));
#57116=CARTESIAN_POINT('Ctrl Pts',(-5.25575457855815,-0.756106706852481,
1.91267085120645E-16));
#57117=CARTESIAN_POINT('Ctrl Pts',(-5.28914618801543,-0.605917493293632,
1.21266317269936E-16));
#57118=CARTESIAN_POINT('Ctrl Pts',(-5.31602599346966,-0.454734459029675,
1.11022302462516E-16));
#57119=CARTESIAN_POINT('Ctrl Pts',(-5.34317079103733,-0.302061000594503,
1.00677297968299E-16));
#57120=CARTESIAN_POINT('Ctrl Pts',(-5.36367506573315,-0.148373349291817,
1.13229940710053E-15));
#57121=CARTESIAN_POINT('Ctrl Pts',(-5.37750436397203,0.00587829643313097,
1.0547118733939E-15));
#57122=CARTESIAN_POINT('Ctrl Pts',(-5.39135928407949,0.160415727837723,
9.76980591424825E-16));
#57123=CARTESIAN_POINT('Ctrl Pts',(-5.39851473413966,0.315519992364312,
1.72186685042656E-16));
#57124=CARTESIAN_POINT('Ctrl Pts',(-5.39888790157043,0.47075779833462,2.77555756156289E-16));
#57125=CARTESIAN_POINT('Ctrl Pts',(-5.39902973997675,0.529762634193127,
3.17605824544993E-16));
#57126=CARTESIAN_POINT('Ctrl Pts',(-5.39819122013145,0.588786903914602,
7.39732282841607E-16));
#57127=CARTESIAN_POINT('Ctrl Pts',(-5.39636585059798,0.647807199370088,
7.7715611723761E-16));
#57128=CARTESIAN_POINT('Ctrl Pts',(-5.39278164456781,0.7636965549195,7.9126101240072E-16));
#57129=CARTESIAN_POINT('Ctrl Pts',(-5.38539362454781,0.879570616150454,
2.25912163058052E-16));
#57130=CARTESIAN_POINT('Ctrl Pts',(-5.37425683908509,0.995265406518742,
2.22044604925031E-16));
#57131=CARTESIAN_POINT('Ctrl Pts',(-5.37119198986139,1.02710467375017,2.20980250890262E-16));
#57132=CARTESIAN_POINT('Ctrl Pts',(-5.3678431309615,1.05893036198002,-4.98345963791524E-17));
#57133=CARTESIAN_POINT('Ctrl Pts',(-5.36421119278863,1.09073904150971,-5.55111512312578E-17));
#57134=CARTESIAN_POINT('Ctrl Pts',(-5.36130959000465,1.11615141052175,-6.00462249517562E-17));
#57135=CARTESIAN_POINT('Ctrl Pts',(-5.35822677414316,1.14155649394533,-1.11305744570047E-16));
#57136=CARTESIAN_POINT('Ctrl Pts',(-5.35496675861173,1.16692638663651,-1.11022302462516E-16));
#57137=CARTESIAN_POINT('Ctrl Pts',(-5.33509845623767,1.32154426938163,-1.09294852564294E-16));
#57138=CARTESIAN_POINT('Ctrl Pts',(-5.30863314216658,1.4750401212272,2.16862255230366E-16));
#57139=CARTESIAN_POINT('Ctrl Pts',(-5.27581080798388,1.62701588796501,2.22044604925031E-16));
#57140=CARTESIAN_POINT('Ctrl Pts',(-5.24225444461877,1.78239039676614,2.27342851188421E-16));
#57141=CARTESIAN_POINT('Ctrl Pts',(-5.20205360448928,1.93617674988367,3.58795532194926E-16));
#57142=CARTESIAN_POINT('Ctrl Pts',(-5.15541121814811,2.08796002984681,2.77555756156289E-16));
#57143=CARTESIAN_POINT('Ctrl Pts',(-5.10857408351102,2.24037705815435,1.95976775604635E-16));
#57144=CARTESIAN_POINT('Ctrl Pts',(-5.05524139421354,2.39077501296198,7.1419842572492E-16));
#57145=CARTESIAN_POINT('Ctrl Pts',(-4.99556586525404,2.53873318984042,7.7715611723761E-16));
#57146=CARTESIAN_POINT('Ctrl Pts',(-4.94308833481477,2.66884480956559,8.32519919290971E-16));
#57147=CARTESIAN_POINT('Ctrl Pts',(-4.88570498504201,2.79707005286713,-9.60359478345213E-16));
#57148=CARTESIAN_POINT('Ctrl Pts',(-4.82348716797381,2.9231153225656,-1.0547118733939E-15));
#57149=CARTESIAN_POINT('Ctrl Pts',(-4.79237825943971,2.98613795741484,-1.10188807091824E-15));
#57150=CARTESIAN_POINT('Ctrl Pts',(-4.76006026636089,3.04861544670858,-2.34131068753582E-16));
#57151=CARTESIAN_POINT('Ctrl Pts',(-4.72653934608425,3.11050991069538,-2.22044604925031E-16));
#57152=CARTESIAN_POINT('Ctrl Pts',(-4.71542868620718,3.13102510932223,-2.18038492097365E-16));
#57153=CARTESIAN_POINT('Ctrl Pts',(-4.70418510044029,3.15147759934516,-9.30594094610435E-17));
#57154=CARTESIAN_POINT('Ctrl Pts',(-4.69281112422588,3.17186176124398,-1.11022302462516E-16));
#57155=CARTESIAN_POINT('Ctrl Pts',(-4.66986975336546,3.21297672482261,-1.47253553724545E-16));
#57156=CARTESIAN_POINT('Ctrl Pts',(-4.64641569423652,3.25378205022521,4.87358186177378E-16));
#57157=CARTESIAN_POINT('Ctrl Pts',(-4.6224537842997,3.29426742849354,4.44089209850063E-16));
#57158=CARTESIAN_POINT('Ctrl Pts',(-4.5407901963357,3.43224396117347,1.8116204744435E-16));
#57159=CARTESIAN_POINT('Ctrl Pts',(-4.45323198209242,3.56650537742696,-3.2643330626556E-16));
#57160=CARTESIAN_POINT('Ctrl Pts',(-4.36016765818568,3.69680903327971,-1.66533453693773E-16));
#57161=CARTESIAN_POINT('Ctrl Pts',(-4.26589053581423,3.828810784247,-4.54981339791011E-18));
#57162=CARTESIAN_POINT('Ctrl Pts',(-4.16596252106395,3.95675153466492,-4.38639487339398E-16));
#57163=CARTESIAN_POINT('Ctrl Pts',(-4.06073706621468,4.08036089658611,-2.77555756156289E-16));
#57164=CARTESIAN_POINT('Ctrl Pts',(-4.00840964546727,4.14183042502705,-1.97450650511893E-16));
#57165=CARTESIAN_POINT('Ctrl Pts',(-3.95477144372171,4.2022284838368,4.11439993416818E-16));
#57166=CARTESIAN_POINT('Ctrl Pts',(-3.89986178457086,4.26151948427011,4.9960036108132E-16));
#57167=CARTESIAN_POINT('Ctrl Pts',(-3.87477357591952,4.28860952658727,5.3988080960258E-16));
#57168=CARTESIAN_POINT('Ctrl Pts',(-3.8494199054371,4.31546843826014,-4.89272403562093E-16));
#57169=CARTESIAN_POINT('Ctrl Pts',(-3.82380434918523,4.34209269619914,-5.55111512312578E-16));
#57170=CARTESIAN_POINT('Ctrl Pts',(-3.8018891935949,4.36487083732063,-6.11439561487415E-16));
#57171=CARTESIAN_POINT('Ctrl Pts',(-3.77977994088804,4.38747952479312,1.3621248594443E-16));
#57172=CARTESIAN_POINT('Ctrl Pts',(-3.75749701858742,4.40989850208082,1.11022302462516E-16));
#57173=CARTESIAN_POINT('Ctrl Pts',(-3.64082422534835,4.52728367564249,-2.08728336147496E-17));
#57174=CARTESIAN_POINT('Ctrl Pts',(-3.5192998591356,4.63956980826707,-2.21183261000239E-15));
#57175=CARTESIAN_POINT('Ctrl Pts',(-3.39330838152807,4.74648957497586,-4.10782519111308E-15));
#57176=CARTESIAN_POINT('Ctrl Pts',(-3.26677453657137,4.85386960924834,-6.0119796295953E-15));
#57177=CARTESIAN_POINT('Ctrl Pts',(-3.13573457516067,4.95583757780676,-8.63900142651335E-15));
#57178=CARTESIAN_POINT('Ctrl Pts',(-3.00053335242381,5.05209514857636,-1.06581410364015E-14));
#57179=CARTESIAN_POINT('Ctrl Pts',(-2.86569963082772,5.14809107402686,-1.26717922631599E-14));
#57180=CARTESIAN_POINT('Ctrl Pts',(-2.72672672727089,5.23840818298683,-1.44182212246245E-14));
#57181=CARTESIAN_POINT('Ctrl Pts',(-2.58391981634373,5.3227144339337,-1.4432899320127E-14));
#57182=CARTESIAN_POINT('Ctrl Pts',(-2.85728222003707,-4.00342940649516,
-1.52221985016965E-15));
#57183=CARTESIAN_POINT('Ctrl Pts',(-2.28500641414625,-4.41104155800517,
0.0397943477746339));
#57184=CARTESIAN_POINT('Ctrl Pts',(-0.854537515415942,-5.02713941244452,
0.125979848023253));
#57185=CARTESIAN_POINT('Ctrl Pts',(1.5567708799336,-4.88563546465558,0.258556500745857));
#57186=CARTESIAN_POINT('Ctrl Pts',(3.70738228326065,-3.54233751270576,0.39772995816781));
#57187=CARTESIAN_POINT('Ctrl Pts',(4.95140614815209,-1.33283639810976,0.536903415589762));
#57188=CARTESIAN_POINT('Ctrl Pts',(4.98463903712129,1.20260146313003,0.676076873011714));
#57189=CARTESIAN_POINT('Ctrl Pts',(3.79895229578282,3.44395520585394,0.815250330433666));
#57190=CARTESIAN_POINT('Ctrl Pts',(1.68428893605082,4.84314423609996,0.954423787855619));
#57191=CARTESIAN_POINT('Ctrl Pts',(-0.842242278542283,5.05801321348077,
1.09359724527757));
#57192=CARTESIAN_POINT('Ctrl Pts',(-3.16281564529539,4.03602149408518,1.23277070269952));
#57193=CARTESIAN_POINT('Ctrl Pts',(-4.61370980268822,2.15207184328641,1.36328514227675));
#57194=CARTESIAN_POINT('Ctrl Pts',(-4.91768134020962,0.666110914719361,
1.44740842938));
#57195=CARTESIAN_POINT('Ctrl Pts',(-4.91836475234218,-0.000121599733084975,
1.48514056400926));
#57196=CARTESIAN_POINT('Origin',(0.,0.,-3.23514056400933));
#57197=CARTESIAN_POINT('',(2.85706463458462,-4.00329423553976,0.));
#57198=CARTESIAN_POINT('Origin',(0.,0.,0.));
#57199=CARTESIAN_POINT('Ctrl Pts',(2.85706463458441,-4.0032942355399,0.));
#57200=CARTESIAN_POINT('Ctrl Pts',(3.52386294776537,-3.52741468062806,0.046391152473984));
#57201=CARTESIAN_POINT('Ctrl Pts',(4.61438908619534,-2.23650256226449,0.139173457421952));
#57202=CARTESIAN_POINT('Ctrl Pts',(5.12163790500659,0.248365779535813,0.278346914843904));
#57203=CARTESIAN_POINT('Ctrl Pts',(4.37650875504895,2.67182739135543,0.417520372265856));
#57204=CARTESIAN_POINT('Ctrl Pts',(2.56115201646861,4.44226470421493,0.556693829687809));
#57205=CARTESIAN_POINT('Ctrl Pts',(0.119512633872891,5.12624413067081,0.695867287109761));
#57206=CARTESIAN_POINT('Ctrl Pts',(-2.35135624542669,4.55676348086115,0.835040744531713));
#57207=CARTESIAN_POINT('Ctrl Pts',(-4.24723382866677,2.87295023988583,0.974214201953666));
#57208=CARTESIAN_POINT('Ctrl Pts',(-4.8731083061567,1.13076638505056,1.07582043244));
#57209=CARTESIAN_POINT('Ctrl Pts',(-4.91851593873139,0.155927429260441,
1.13103551045236));
#57210=CARTESIAN_POINT('Ctrl Pts',(-4.91835559909507,0.00012341875379537,
1.13985943599073));
#57211=CARTESIAN_POINT('Ctrl Pts',(3.43710408716079,-4.81604049573118,-0.576484243785842));
#57212=CARTESIAN_POINT('Ctrl Pts',(4.23927537156343,-4.24354817498196,-0.530093091311858));
#57213=CARTESIAN_POINT('Ctrl Pts',(5.55119943592679,-2.69055589595426,-0.43731078636389));
#57214=CARTESIAN_POINT('Ctrl Pts',(6.16142958866421,0.298788842793687,-0.298137328941937));
#57215=CARTESIAN_POINT('Ctrl Pts',(5.26502479061354,3.21426009613248,-0.158963871519986));
#57216=CARTESIAN_POINT('Ctrl Pts',(3.08111547673245,5.34413047093264,-0.0197904140980329));
#57217=CARTESIAN_POINT('Ctrl Pts',(0.143776013107478,6.16697096734542,0.119383043323919));
#57218=CARTESIAN_POINT('Ctrl Pts',(-2.82872710112941,5.48187471669485,0.258556500745872));
#57219=CARTESIAN_POINT('Ctrl Pts',(-5.10950455055458,3.45621477798876,0.397729958167823));
#57220=CARTESIAN_POINT('Ctrl Pts',(-6.14083048116305,0.58541647896675,0.536903415589776));
#57221=CARTESIAN_POINT('Ctrl Pts',(-5.67050742409554,-2.42855065362853,
0.676076873011728));
#57222=CARTESIAN_POINT('Ctrl Pts',(-3.81354694446943,-4.84864486784236,
0.815250330433681));
#57223=CARTESIAN_POINT('Ctrl Pts',(-1.02404039718864,-6.08307916434686,
0.954423787855633));
#57224=CARTESIAN_POINT('Ctrl Pts',(2.01587981812662,-5.82998553179797,1.09359724527759));
#57225=CARTESIAN_POINT('Ctrl Pts',(4.56284681947448,-4.15125708628714,1.23277070269954));
#57226=CARTESIAN_POINT('Ctrl Pts',(5.99403783840857,-1.45740030245642,1.37194416012149));
#57227=CARTESIAN_POINT('Ctrl Pts',(5.95947655212953,1.59284167705623,1.51111761754344));
#57228=CARTESIAN_POINT('Ctrl Pts',(4.46761438646609,4.25357817423206,1.65029107496539));
#57229=CARTESIAN_POINT('Ctrl Pts',(1.88326393488574,5.87416567017125,1.78946453238735));
#57230=CARTESIAN_POINT('Ctrl Pts',(-1.16161055136132,6.05831382819653,1.9286379898093));
#57231=CARTESIAN_POINT('Ctrl Pts',(-3.9224305471212,4.76099191815651,2.06781144723125));
#57232=CARTESIAN_POINT('Ctrl Pts',(-5.72407880918856,2.29944063955624,2.2069849046532));
#57233=CARTESIAN_POINT('Ctrl Pts',(-6.12598919626941,-0.724404466168149,
2.34615836207515));
#57234=CARTESIAN_POINT('Ctrl Pts',(-5.02988053374446,-3.57110729008621,
2.48533181949711));
#57235=CARTESIAN_POINT('Ctrl Pts',(-2.70378980360807,-5.54454922987053,
2.62450527691906));
#57236=CARTESIAN_POINT('Ctrl Pts',(0.283472290417655,-6.16215456821602,
2.76367873434101));
#57237=CARTESIAN_POINT('Ctrl Pts',(3.20141547489109,-5.2728971562611,2.90285219176296));
#57238=CARTESIAN_POINT('Ctrl Pts',(5.33650037903085,-3.09423159563492,3.04202564918492));
#57239=CARTESIAN_POINT('Ctrl Pts',(6.16662391766363,-0.158917969608813,
3.18119910660686));
#57240=CARTESIAN_POINT('Ctrl Pts',(5.48879179310159,2.8152566694643,3.32037256402882));
#57241=CARTESIAN_POINT('Ctrl Pts',(3.46875771508856,5.10100238942732,3.45954602145077));
#57242=CARTESIAN_POINT('Ctrl Pts',(0.600490809753028,6.13937425560414,3.59871947887272));
#57243=CARTESIAN_POINT('Ctrl Pts',(-2.41461714335042,5.67645395594698,3.73789293629468));
#57244=CARTESIAN_POINT('Ctrl Pts',(-4.83926658230211,3.82544172722223,3.87706639371663));
#57245=CARTESIAN_POINT('Ctrl Pts',(-6.08054574508388,1.03897492986976,4.01623985113858));
#57246=CARTESIAN_POINT('Ctrl Pts',(-5.83491837456198,-2.0015576497205,4.15541330856054));
#57247=CARTESIAN_POINT('Ctrl Pts',(-4.16244897107871,-4.55263923742286,
4.29458676598249));
#57248=CARTESIAN_POINT('Ctrl Pts',(-1.47211491710019,-5.99044097991182,
4.43376022340444));
#57249=CARTESIAN_POINT('Ctrl Pts',(1.57820282580624,-5.96336996199074,4.57293368082639));
#57250=CARTESIAN_POINT('Ctrl Pts',(4.24259466815234,-4.47804599627128,4.71210713824835));
#57251=CARTESIAN_POINT('Ctrl Pts',(5.86952342828491,-1.89768284699277,4.85128059567029));
#57252=CARTESIAN_POINT('Ctrl Pts',(6.06114800705314,1.14673026451377,4.99045405309225));
#57253=CARTESIAN_POINT('Ctrl Pts',(4.77060947927874,3.91072763807093,5.1296275105142));
#57254=CARTESIAN_POINT('Ctrl Pts',(2.31348974317856,5.71841504887182,5.26880096793615));
#57255=CARTESIAN_POINT('Ctrl Pts',(-0.709359313623553,6.12774957281476,
5.40797442535811));
#57256=CARTESIAN_POINT('Ctrl Pts',(-3.55874515805866,5.03863457326983,5.54714788278005));
#57257=CARTESIAN_POINT('Ctrl Pts',(-5.53789309166834,2.71739683671858,5.68632134020202));
#57258=CARTESIAN_POINT('Ctrl Pts',(-6.16283208352363,-0.268339660221467,
5.82549479762395));
#57259=CARTESIAN_POINT('Ctrl Pts',(-5.28074264852207,-3.18845770601339,
5.96466825504592));
#57260=CARTESIAN_POINT('Ctrl Pts',(-3.10732656720241,-5.32888610008828,
6.10384171246786));
#57261=CARTESIAN_POINT('Ctrl Pts',(-0.174060240924557,-6.16621508670314,
6.24301516988982));
#57262=CARTESIAN_POINT('Ctrl Pts',(2.80176991436952,-5.49568838362309,6.38218862731176));
#57263=CARTESIAN_POINT('Ctrl Pts',(5.0924691348527,-3.48127326901073,6.52136208473373));
#57264=CARTESIAN_POINT('Ctrl Pts',(6.13788118133806,-0.615564835522726,
6.66053554215567));
#57265=CARTESIAN_POINT('Ctrl Pts',(5.68236617097953,2.40067077331804,6.79970899957763));
#57266=CARTESIAN_POINT('Ctrl Pts',(3.83731348777568,4.82985824424392,6.93888245699957));
#57267=CARTESIAN_POINT('Ctrl Pts',(1.05390317443291,6.07797610737952,7.07805591442153));
#57268=CARTESIAN_POINT('Ctrl Pts',(-1.98722340011894,5.83981580368557,7.21722937184348));
#57269=CARTESIAN_POINT('Ctrl Pts',(-4.54240420916778,4.17361587397437,7.35640282926544));
#57270=CARTESIAN_POINT('Ctrl Pts',(-5.98680799610826,1.48682059465498,7.49557628668739));
#57271=CARTESIAN_POINT('Ctrl Pts',(-5.96722741450003,-1.5635544271292,7.63474974410934));
#57272=CARTESIAN_POINT('Ctrl Pts',(-4.48845060276677,-4.23158559519698,
7.77392320153129));
#57273=CARTESIAN_POINT('Ctrl Pts',(-1.91209031654676,-5.86484578521245,
7.91309665895325));
#57274=CARTESIAN_POINT('Ctrl Pts',(1.13184306313101,-6.06394564152732,8.0522701163752));
#57275=CARTESIAN_POINT('Ctrl Pts',(3.89900114733389,-4.78019827162483,8.19144357379714));
#57276=CARTESIAN_POINT('Ctrl Pts',(5.71271680673197,-2.32752489761939,8.33061703121911));
#57277=CARTESIAN_POINT('Ctrl Pts',(6.12947299917573,0.694309884224369,8.46979048864104));
#57278=CARTESIAN_POINT('Ctrl Pts',(5.04735822998721,3.54636156661111,8.60896394606302));
#57279=CARTESIAN_POINT('Ctrl Pts',(2.73098748399595,5.53120356027632,8.74813740348494));
#57280=CARTESIAN_POINT('Ctrl Pts',(-0.25320541194086,6.16347243705364,8.88731086090693));
#57281=CARTESIAN_POINT('Ctrl Pts',(-3.17548071082857,5.28855629809418,9.02648431832885));
#57282=CARTESIAN_POINT('Ctrl Pts',(-5.32123968811336,3.12040280165932,9.16565777575082));
#57283=CARTESIAN_POINT('Ctrl Pts',(-6.16576907364188,0.189201462672217,
9.30483123317277));
#57284=CARTESIAN_POINT('Ctrl Pts',(-5.50255183529998,-2.78826626468724,
9.44400469059472));
#57285=CARTESIAN_POINT('Ctrl Pts',(-3.4937678309544,-5.08390517283163,9.58317814801667));
#57286=CARTESIAN_POINT('Ctrl Pts',(-0.630635149453913,-6.13635109582472,
9.72235160543862));
#57287=CARTESIAN_POINT('Ctrl Pts',(2.38670992730932,-5.68824412150526,9.86152506286057));
#57288=CARTESIAN_POINT('Ctrl Pts',(4.82042078227819,-3.84916210943844,10.0006985202825));
#57289=CARTESIAN_POINT('Ctrl Pts',(6.07536981965241,-1.0688250639897,10.1398719777045));
#57290=CARTESIAN_POINT('Ctrl Pts',(5.84467801888626,1.97287716761684,10.2790454351264));
#57291=CARTESIAN_POINT('Ctrl Pts',(4.18475761008524,4.53214179034479,10.4182188925484));
#57292=CARTESIAN_POINT('Ctrl Pts',(1.50151730672395,5.98313891202306,10.5573923499703));
#57293=CARTESIAN_POINT('Ctrl Pts',(-1.54889660026354,5.97104888479805,10.6965658073923));
#57294=CARTESIAN_POINT('Ctrl Pts',(-4.22055100590104,4.49882814403304,10.8357392648142));
#57295=CARTESIAN_POINT('Ctrl Pts',(-5.86013277728699,1.92648625625064,10.9749127222362));
#57296=CARTESIAN_POINT('Ctrl Pts',(-6.0667067105821,-1.11694903676676,11.1140861796581));
#57297=CARTESIAN_POINT('Ctrl Pts',(-4.78975823951158,-3.887251145731,11.2532596370801));
#57298=CARTESIAN_POINT('Ctrl Pts',(-2.34154601715145,-5.70698411707254,
11.3924330945021));
#57299=CARTESIAN_POINT('Ctrl Pts',(0.679256268156358,-6.13115946498918,
11.531606551924));
#57300=CARTESIAN_POINT('Ctrl Pts',(3.53395659070436,-5.05605145127828,11.670780009346));
#57301=CARTESIAN_POINT('Ctrl Pts',(5.52448067588446,-2.74456166349661,11.8099534667679));
#57302=CARTESIAN_POINT('Ctrl Pts',(6.16407562502046,0.238069636838827,11.9491269241898));
#57303=CARTESIAN_POINT('Ctrl Pts',(5.29633805782252,3.16248456758555,12.0883003816118));
#57304=CARTESIAN_POINT('Ctrl Pts',(3.13346022017625,5.31356118921473,12.2274738390338));
#57305=CARTESIAN_POINT('Ctrl Pts',(0.204341543540447,6.16528588116882,12.3666472964557));
#57306=CARTESIAN_POINT('Ctrl Pts',(-2.77474580183883,5.50938210674607,12.5058207538777));
#57307=CARTESIAN_POINT('Ctrl Pts',(-5.07531055500723,3.50624132557761,12.6449942112996));
#57308=CARTESIAN_POINT('Ctrl Pts',(-6.13478400828913,0.645701660673112,
12.7841676687216));
#57309=CARTESIAN_POINT('Ctrl Pts',(-5.69408777208102,-2.37273468950772,
12.9233411261435));
#57310=CARTESIAN_POINT('Ctrl Pts',(-3.8609875207634,-4.81095425331247,13.0625145835655));
#57311=CARTESIAN_POINT('Ctrl Pts',(-1.08374050856188,-6.07272689761841,
13.2016880409874));
#57312=CARTESIAN_POINT('Ctrl Pts',(1.95851903872161,-5.84950499084504,13.3408614984094));
#57313=CARTESIAN_POINT('Ctrl Pts',(4.52185204283595,-4.19587411222696,13.4800349558314));
#57314=CARTESIAN_POINT('Ctrl Pts',(5.97943374978069,-1.51620496468635,13.6192084132533));
#57315=CARTESIAN_POINT('Ctrl Pts',(5.97483434984145,1.53422943359551,13.7583818706753));
#57316=CARTESIAN_POINT('Ctrl Pts',(4.50917855749375,4.20949096680282,13.8975553280972));
#57317=CARTESIAN_POINT('Ctrl Pts',(1.94087057929726,5.8553844329279,14.0367287855192));
#57318=CARTESIAN_POINT('Ctrl Pts',(-1.10204827523175,6.06943119756825,14.1759022429411));
#57319=CARTESIAN_POINT('Ctrl Pts',(-3.87547770411452,4.79928932529257,14.315075700363));
#57320=CARTESIAN_POINT('Ctrl Pts',(-5.70121701446153,2.35555301722769,14.454249157785));
#57321=CARTESIAN_POINT('Ctrl Pts',(-6.13280896008574,-0.664198556192439,
14.5934226152069));
#57322=CARTESIAN_POINT('Ctrl Pts',(-5.06471418472317,-3.52153030514006,
14.7325960726289));
#57323=CARTESIAN_POINT('Ctrl Pts',(-2.75811929336864,-5.51772447903153,
14.8717695300509));
#57324=CARTESIAN_POINT('Ctrl Pts',(0.222932426183668,-6.16464164378691,
15.0109429874728));
#57325=CARTESIAN_POINT('Ctrl Pts',(3.14946935465071,-5.30408788078328,15.1501164448948));
#57326=CARTESIAN_POINT('Ctrl Pts',(5.30585064969353,-3.14649874401734,15.2892899023167));
#57327=CARTESIAN_POINT('Ctrl Pts',(6.16476551219756,-0.21948039223499,15.4284633597387));
#57328=CARTESIAN_POINT('Ctrl Pts',(5.51617915677505,2.7612086073523,15.5676368171606));
#57329=CARTESIAN_POINT('Ctrl Pts',(3.51869367766553,5.06668533320481,15.7068102745826));
#57330=CARTESIAN_POINT('Ctrl Pts',(0.660764278329698,6.13317992818077,15.8459837320045));
#57331=CARTESIAN_POINT('Ctrl Pts',(-2.35874514418357,5.69989708746978,15.9851571894265));
#57332=CARTESIAN_POINT('Ctrl Pts',(-4.8014587144297,3.8727896504436,16.1243306468484));
#57333=CARTESIAN_POINT('Ctrl Pts',(-6.07004735721424,1.09864941820965,16.2635041042704));
#57334=CARTESIAN_POINT('Ctrl Pts',(-5.85429669045541,-1.94414910001237,
16.4026775616923));
#57335=CARTESIAN_POINT('Ctrl Pts',(-4.20696531336737,-4.51153502868811,
16.5418510191143));
#57336=CARTESIAN_POINT('Ctrl Pts',(-1.53088347997605,-5.9756925317232,16.6810244765362));
#57337=CARTESIAN_POINT('Ctrl Pts',(1.51955301556766,-5.97858378680396,16.8201979339582));
#57338=CARTESIAN_POINT('Ctrl Pts',(4.19840554459396,-4.51950178073632,16.9593713913801));
#57339=CARTESIAN_POINT('Ctrl Pts',(5.85060078076748,-1.95524319894966,17.0985448488021));
#57340=CARTESIAN_POINT('Ctrl Pts',(6.07211908605725,1.0871408683769,17.2377183062241));
#57341=CARTESIAN_POINT('Ctrl Pts',(4.80879147149576,3.86368089347784,17.376891763646));
#57342=CARTESIAN_POINT('Ctrl Pts',(2.36954581338641,5.69541553367435,17.516065221068));
#57343=CARTESIAN_POINT('Ctrl Pts',(-0.649136839130126,6.13442147451903,
17.6552386784899));
#57344=CARTESIAN_POINT('Ctrl Pts',(-3.50908278484838,5.07334637808584,17.7944121359118));
#57345=CARTESIAN_POINT('Ctrl Pts',(-5.51093501045721,2.77166029185993,17.9335855933338));
#57346=CARTESIAN_POINT('Ctrl Pts',(-6.16517048993992,-0.20779387125234,
18.0727590507557));
#57347=CARTESIAN_POINT('Ctrl Pts',(-5.31180572024526,-3.13643515050539,
18.2119325081777));
#57348=CARTESIAN_POINT('Ctrl Pts',(-3.15951829456067,-5.29810811604411,
18.3511059655997));
#57349=CARTESIAN_POINT('Ctrl Pts',(-0.234617917469024,-6.16420796986592,
18.4902794230216));
#57350=CARTESIAN_POINT('Ctrl Pts',(2.74765476285655,-5.5229429444009,18.6294528804436));
#57351=CARTESIAN_POINT('Ctrl Pts',(5.05802955943419,-3.53112481213083,18.7686263378655));
#57352=CARTESIAN_POINT('Ctrl Pts',(6.1315388651722,-0.675822911596517,18.9077997952875));
#57353=CARTESIAN_POINT('Ctrl Pts',(5.70567203264151,2.3447413756934,19.0469732527094));
#57354=CARTESIAN_POINT('Ctrl Pts',(3.88456842731257,4.7919342228877,19.1861467101314));
#57355=CARTESIAN_POINT('Ctrl Pts',(1.11355170303273,6.06733121459748,19.3253201675533));
#57356=CARTESIAN_POINT('Ctrl Pts',(-1.92976743813947,5.85905308882354,19.4644936249753));
#57357=CARTESIAN_POINT('Ctrl Pts',(-4.50119081011263,4.21803114662679,19.6036670823972));
#57358=CARTESIAN_POINT('Ctrl Pts',(-5.97191528041001,1.54555276408195,19.7428405398192));
#57359=CARTESIAN_POINT('Ctrl Pts',(-5.9822971730766,-1.50486743467848,19.8820139972411));
#57360=CARTESIAN_POINT('Ctrl Pts',(-4.52979775151187,-4.18729480611934,
20.0211874546631));
#57361=CARTESIAN_POINT('Ctrl Pts',(-1.96960402854123,-5.84578184965109,
20.160360912085));
#57362=CARTESIAN_POINT('Ctrl Pts',(1.07222690609371,-6.07477035984117,20.299534369507));
#57363=CARTESIAN_POINT('Ctrl Pts',(3.85186078495554,-4.81826462082334,20.4387078269289));
#57364=CARTESIAN_POINT('Ctrl Pts',(5.6895797096938,-2.38352432125133,20.5778812843509));
#57365=CARTESIAN_POINT('Ctrl Pts',(6.13599699856562,0.634071207791177,20.7170547417728));
#57366=CARTESIAN_POINT('Ctrl Pts',(5.08194797931441,3.49661410488748,20.8562281991948));
#57367=CARTESIAN_POINT('Ctrl Pts',(2.78518457731863,5.50411231110181,20.9954016566167));
#57368=CARTESIAN_POINT('Ctrl Pts',(-0.192654063329878,6.16566216029053,
21.1345751140387));
#57369=CARTESIAN_POINT('Ctrl Pts',(-3.12338203374549,5.31949152967011,21.2737485714607));
#57370=CARTESIAN_POINT('Ctrl Pts',(-5.29033363495371,3.1725187932987,21.4129220288826));
#57371=CARTESIAN_POINT('Ctrl Pts',(-6.16361325753588,0.249754027963704,
21.5520954863046));
#57372=CARTESIAN_POINT('Ctrl Pts',(-5.52967342883816,-2.73408435008088,
21.6912689437265));
#57373=CARTESIAN_POINT('Ctrl Pts',(-3.54353465401414,-5.04934328588946,
21.8304424011485));
#57374=CARTESIAN_POINT('Ctrl Pts',(-0.69087746967043,-6.12986082915899,
21.9696158585704));
#57375=CARTESIAN_POINT('Ctrl Pts',(2.33072346847955,-5.71141257277345,22.1087893159923));
#57376=CARTESIAN_POINT('Ctrl Pts',(4.78238083611889,-3.89632378034461,22.2479627734144));
#57377=CARTESIAN_POINT('Ctrl Pts',(6.06457848614637,-1.12844727317076,22.3871362308362));
#57378=CARTESIAN_POINT('Ctrl Pts',(5.8637741572685,1.91537413982392,22.5263096882583));
#57379=CARTESIAN_POINT('Ctrl Pts',(4.22907154527857,4.49081944948481,22.6654831456801));
#57380=CARTESIAN_POINT('Ctrl Pts',(1.56021272854873,5.96810201861786,22.8046566031022));
#57381=CARTESIAN_POINT('Ctrl Pts',(-1.49017277948154,5.98597448626773,22.9438300605241));
#57382=CARTESIAN_POINT('Ctrl Pts',(-4.17615881837635,4.54006640773607,23.0830035179461));
#57383=CARTESIAN_POINT('Ctrl Pts',(-5.84092766863672,1.98395298147663,23.222176975368));
#57384=CARTESIAN_POINT('Ctrl Pts',(-6.07738500293291,-1.05730647831276,
23.36135043279));
#57385=CARTESIAN_POINT('Ctrl Pts',(-4.82770871615259,-3.84001744982238,
23.5005238902119));
#57386=CARTESIAN_POINT('Ctrl Pts',(-2.39748845653263,-5.68370957770968,
23.6396973476339));
#57387=CARTESIAN_POINT('Ctrl Pts',(0.619001753020852,-6.13753552272517,
23.7788708050558));
#57388=CARTESIAN_POINT('Ctrl Pts',(3.48412434044316,-5.0905189365415,23.9180442624778));
#57389=CARTESIAN_POINT('Ctrl Pts',(5.49725642210601,-2.79869206819369,24.0572177198997));
#57390=CARTESIAN_POINT('Ctrl Pts',(6.166116651874,0.177513093708911,24.1963911773217));
#57391=CARTESIAN_POINT('Ctrl Pts',(5.32714526271259,3.11031008308092,24.3355646347436));
#57392=CARTESIAN_POINT('Ctrl Pts',(3.18550016183881,5.28252725330224,24.4747380921656));
#57393=CARTESIAN_POINT('Ctrl Pts',(0.264888632448706,6.1629813787935,24.6139115495875));
#57394=CARTESIAN_POINT('Ctrl Pts',(-2.72049745085447,5.53637056950222,24.7530850070095));
#57395=CARTESIAN_POINT('Ctrl Pts',(-5.04062656494859,3.55592312848445,24.8922584644314));
#57396=CARTESIAN_POINT('Ctrl Pts',(-6.12814583025965,0.705927861772895,
25.0314319218534));
#57397=CARTESIAN_POINT('Ctrl Pts',(-5.71711867325033,-2.3166915070696,25.1706053792753));
#57398=CARTESIAN_POINT('Ctrl Pts',(-3.90805563865528,-4.77279861172988,
25.3097788366973));
#57399=CARTESIAN_POINT('Ctrl Pts',(-1.14333603880389,-6.06178918845982,
25.4489522941192));
#57400=CARTESIAN_POINT('Ctrl Pts',(1.90096929185687,-5.86845986732236,25.5881257515412));
#57401=CARTESIAN_POINT('Ctrl Pts',(4.48042100934369,-4.24008644274946,25.7272992089631));
#57402=CARTESIAN_POINT('Ctrl Pts',(5.96425276934059,-1.5748632849772,25.8664726663851));
#57403=CARTESIAN_POINT('Ctrl Pts',(5.98961570420329,1.47546913858521,26.0056461238071));
#57404=CARTESIAN_POINT('Ctrl Pts',(4.55030768748918,4.16499764851469,26.144819581229));
#57405=CARTESIAN_POINT('Ctrl Pts',(1.99828997123208,5.83603826699494,26.2839930386509));
#57406=CARTESIAN_POINT('Ctrl Pts',(-1.04237967500393,6.07996299956626,26.4231664960729));
#57407=CARTESIAN_POINT('Ctrl Pts',(-3.82815095949345,4.83712370053581,26.5623399534948));
#57408=CARTESIAN_POINT('Ctrl Pts',(-5.67780517311883,2.41143813502674,26.7015134109168));
#57409=CARTESIAN_POINT('Ctrl Pts',(-6.13903703772037,-0.603928565687683,
26.8406868683387));
#57410=CARTESIAN_POINT('Ctrl Pts',(-5.09905919808441,-3.47161356682837,
26.9798603257607));
#57411=CARTESIAN_POINT('Ctrl Pts',(-2.81218268303532,-5.49036738481062,
27.1190337831827));
#57412=CARTESIAN_POINT('Ctrl Pts',(0.162371053689043,-6.16653396194977,
27.2582072406046));
#57413=CARTESIAN_POINT('Ctrl Pts',(3.09721937733518,-5.33476687322094,27.3973806980266));
#57414=CARTESIAN_POINT('Ctrl Pts',(5.27468901816195,-3.19846232190371,27.5365541554485));
#57415=CARTESIAN_POINT('Ctrl Pts',(6.16231233744904,-0.280021639662804,
27.6757276128705));
#57416=CARTESIAN_POINT('Ctrl Pts',(5.54303432600949,2.70689414710596,27.8149010702924));
#57417=CARTESIAN_POINT('Ctrl Pts',(3.56829016083962,5.03187944917316,27.9540745277144));
#57418=CARTESIAN_POINT('Ctrl Pts',(0.720973997150462,6.12639387881557,28.0932479851363));
#57419=CARTESIAN_POINT('Ctrl Pts',(-2.30264557607587,5.72279029966451,28.2324214425583));
#57420=CARTESIAN_POINT('Ctrl Pts',(-4.76318760750126,3.9197639315018,28.3715948999802));
#57421=CARTESIAN_POINT('Ctrl Pts',(-6.05896333835717,1.15821791015328,28.5107683574022));
#57422=CARTESIAN_POINT('Ctrl Pts',(-5.87311019073044,-1.88655298109917,
28.6499418148241));
#57423=CARTESIAN_POINT('Ctrl Pts',(-4.25107577261991,-4.46999555239154,
28.7891152722461));
#57424=CARTESIAN_POINT('Ctrl Pts',(-1.58950434502494,-5.96036755578906,
28.9282887296681));
#57425=CARTESIAN_POINT('Ctrl Pts',(1.46075660065201,-5.99322080492681,29.06746218709));
#57426=CARTESIAN_POINT('Ctrl Pts',(4.15381136383588,-4.56052152901661,29.2066356445119));
#57427=CARTESIAN_POINT('Ctrl Pts',(5.8311136742087,-2.01261491135594,29.3458091019339));
#57428=CARTESIAN_POINT('Ctrl Pts',(6.08250433419597,1.02744658617533,29.4849825593558));
#57429=CARTESIAN_POINT('Ctrl Pts',(4.84650951720095,3.81626138552335,29.6241560167778));
#57430=CARTESIAN_POINT('Ctrl Pts',(2.42537327261766,5.67186653152452,29.7633294741997));
#57431=CARTESIAN_POINT('Ctrl Pts',(-0.588851736682384,6.14050153449717,
29.9025029316217));
#57432=CARTESIAN_POINT('Ctrl Pts',(-3.4590818594826,5.10756871244572,30.0416763890437));
#57433=CARTESIAN_POINT('Ctrl Pts',(-5.48344524075633,2.82565634049557,30.1808498464656));
#57434=CARTESIAN_POINT('Ctrl Pts',(-6.16691408800147,-0.147228034576321,
30.3200233038876));
#57435=CARTESIAN_POINT('Ctrl Pts',(-5.34235631523705,-3.08410999544485,
30.4591967613095));
#57436=CARTESIAN_POINT('Ctrl Pts',(-3.21140519533195,-5.26681897679718,
30.5983702187315));
#57437=CARTESIAN_POINT('Ctrl Pts',(-0.295152958354393,-6.16160613753677,
30.7375436761534));
#57438=CARTESIAN_POINT('Ctrl Pts',(2.69327452086287,-5.54966465817772,30.8767171335754));
#57439=CARTESIAN_POINT('Ctrl Pts',(5.02310199130804,-3.5806356765068,31.0158905909973));
#57440=CARTESIAN_POINT('Ctrl Pts',(6.12460498539096,-0.736015785075372,
31.1550640484193));
#57441=CARTESIAN_POINT('Ctrl Pts',(5.72842741781626,2.28858576019494,31.2942375058412));
#57442=CARTESIAN_POINT('Ctrl Pts',(3.9314485882835,4.75354788138709,31.4334109632632));
#57443=CARTESIAN_POINT('Ctrl Pts',(1.17309279748168,6.05610095287823,31.5725844206851));
#57444=CARTESIAN_POINT('Ctrl Pts',(-1.87212529448077,5.87772509945144,31.7117578781071));
#57445=CARTESIAN_POINT('Ctrl Pts',(-4.45954314149362,4.26203946862453,31.850931335529));
#57446=CARTESIAN_POINT('Ctrl Pts',(-5.95644640139103,1.6041358204067,31.990104792951));
#57447=CARTESIAN_POINT('Ctrl Pts',(-5.99678976669964,-1.44603525439822,
32.1292782503729));
#57448=CARTESIAN_POINT('Ctrl Pts',(-4.57070787072909,-4.14260003179297,
32.2684517077949));
#57449=CARTESIAN_POINT('Ctrl Pts',(-2.02692771546916,-5.82615391997319,
32.4076251652168));
#57450=CARTESIAN_POINT('Ctrl Pts',(1.0125073018732,-6.08500899149783,32.5467986226388));
#57451=CARTESIAN_POINT('Ctrl Pts',(3.80434879960589,-4.85586610955176,32.6859720800607));
#57452=CARTESIAN_POINT('Ctrl Pts',(5.66589368873668,-2.43929378527674,32.8251455374827));
#57453=CARTESIAN_POINT('Ctrl Pts',(6.14192900422469,0.573771356918033,32.9643189949047));
#57454=CARTESIAN_POINT('Ctrl Pts',(5.11604742831312,3.44652929397193,33.1034924523266));
#57455=CARTESIAN_POINT('Ctrl Pts',(2.83911295932849,5.47649003168353,33.2426659097486));
#57456=CARTESIAN_POINT('Ctrl Pts',(-0.132084127682804,6.16725702773691,
33.3818393671704));
#57457=CARTESIAN_POINT('Ctrl Pts',(-3.07098201645912,5.34991354299681,33.5210128245925));
#57458=CARTESIAN_POINT('Ctrl Pts',(-5.25891717666406,3.22432870407837,33.6601862820144));
#57459=CARTESIAN_POINT('Ctrl Pts',(-6.16086278331505,0.310282497282057,
33.7993597394364));
#57460=CARTESIAN_POINT('Ctrl Pts',(-5.5562615260262,-2.67963865425116,33.9385331968583));
#57461=CARTESIAN_POINT('Ctrl Pts',(-3.59295960104287,-5.01429424428103,
34.0777066542803));
#57462=CARTESIAN_POINT('Ctrl Pts',(-0.751053134846073,-6.12277916077282,
34.2168801117022));
#57463=CARTESIAN_POINT('Ctrl Pts',(2.27451214420708,-5.7340299937139,34.3560535691242));
#57464=CARTESIAN_POINT('Ctrl Pts',(4.74387949151463,-3.94310953854224,34.4952270265461));
#57465=CARTESIAN_POINT('Ctrl Pts',(6.05320204928312,-1.18796061109394,34.6344004839681));
#57466=CARTESIAN_POINT('Ctrl Pts',(5.88230456565756,1.85768631900013,34.7735739413901));
#57467=CARTESIAN_POINT('Ctrl Pts',(4.27297746465269,4.44906383967755,34.912747398812));
#57468=CARTESIAN_POINT('Ctrl Pts',(1.61875762289533,5.95248932979087,35.0519208562339));
#57469=CARTESIAN_POINT('Ctrl Pts',(-1.43130518859287,6.00032256800109,35.1910943136559));
#57470=CARTESIAN_POINT('Ctrl Pts',(-4.13136371998978,4.58086665120348,35.3302677710778));
#57471=CARTESIAN_POINT('Ctrl Pts',(-5.8211590341955,2.04122829726617,35.4694412284998));
#57472=CARTESIAN_POINT('Ctrl Pts',(-6.0874769563689,-0.997561912180709,
35.6086146859218));
#57473=CARTESIAN_POINT('Ctrl Pts',(-4.86519342116839,-3.79241327357342,
35.7477881433437));
#57474=CARTESIAN_POINT('Ctrl Pts',(-2.45319958906397,-5.65988668077129,
35.8869616007657));
#57475=CARTESIAN_POINT('Ctrl Pts',(0.558687517328578,-6.14331943829534,
36.0261350581876));
#57476=CARTESIAN_POINT('Ctrl Pts',(3.43395594598768,-5.12449529456042,36.1653085156095));
#57477=CARTESIAN_POINT('Ctrl Pts',(5.46950179953183,-2.85255245839129,36.3044819730315));
#57478=CARTESIAN_POINT('Ctrl Pts',(6.16756277908821,0.116939424325645,36.4436554304534));
#57479=CARTESIAN_POINT('Ctrl Pts',(5.3574385109304,3.05783551953926,36.5828288878754));
#57480=CARTESIAN_POINT('Ctrl Pts',(3.23723277021465,5.25098366541017,36.7220023452973));
#57481=CARTESIAN_POINT('Ctrl Pts',(0.32541016521519,6.1600822792663,36.8611758027193));
#57482=CARTESIAN_POINT('Ctrl Pts',(-2.66598662949465,5.56282488977604,37.0003492601412));
#57483=CARTESIAN_POINT('Ctrl Pts',(-5.00545626120256,3.605261860135,37.1395227175633));
#57484=CARTESIAN_POINT('Ctrl Pts',(-6.12091641597078,0.766085955787854,
37.2786961749851));
#57485=CARTESIAN_POINT('Ctrl Pts',(-5.73959799357409,-2.26042481297572,
37.4178696324071));
#57486=CARTESIAN_POINT('Ctrl Pts',(-3.95474671196289,-4.73418249618397,
37.5570430898291));
#57487=CARTESIAN_POINT('Ctrl Pts',(-1.20282126133765,-6.05026664505211,
37.6962165472511));
#57488=CARTESIAN_POINT('Ctrl Pts',(1.84323614172387,-5.88684856173478,37.8353900046729));
#57489=CARTESIAN_POINT('Ctrl Pts',(4.43855771013327,-4.28388969474851,37.974563462095));
#57490=CARTESIAN_POINT('Ctrl Pts',(5.94849636484969,-1.63336966432161,38.1137369195168));
#57491=CARTESIAN_POINT('Ctrl Pts',(6.00381918752842,1.41656649205803,38.2529103769389));
#57492=CARTESIAN_POINT('Ctrl Pts',(4.59099780918249,4.12010249618109,38.3920838343607));
#57493=CARTESIAN_POINT('Ctrl Pts',(2.05551657051471,5.8161290469947,38.5312572917828));
#57494=CARTESIAN_POINT('Ctrl Pts',(-0.982610507218312,6.08990821392738,
38.6704307492047));
#57495=CARTESIAN_POINT('Ctrl Pts',(-3.78045487939699,4.87449139580732,38.8096042066266));
#57496=CARTESIAN_POINT('Ctrl Pts',(-5.65384554385049,2.46709060012758,38.9487776640486));
#57497=CARTESIAN_POINT('Ctrl Pts',(-6.14467282832481,-0.54360030886931,
39.0879511214705));
#57498=CARTESIAN_POINT('Ctrl Pts',(-5.1329122602471,-3.42136189134693,39.2271245788925));
#57499=CARTESIAN_POINT('Ctrl Pts',(-2.86597475664404,-5.46248058644011,
39.3662980363144));
#57500=CARTESIAN_POINT('Ctrl Pts',(0.101794015827083,-6.16783134021171,
39.5054714937364));
#57501=CARTESIAN_POINT('Ctrl Pts',(3.04467058395836,-5.36493117366241,39.6446449511584));
#57502=CARTESIAN_POINT('Ctrl Pts',(5.24301849087439,-3.25011731592957,39.7838184085803));
#57503=CARTESIAN_POINT('Ctrl Pts',(6.15926463009694,-0.340535870934299,
39.9229918660023));
#57504=CARTESIAN_POINT('Ctrl Pts',(5.56935470985029,2.65231852891472,40.0621653234242));
#57505=CARTESIAN_POINT('Ctrl Pts',(3.61754237960085,4.99658809536546,40.2013387808462));
#57506=CARTESIAN_POINT('Ctrl Pts',(0.781114157253151,6.11901676221718,40.3405122382681));
#57507=CARTESIAN_POINT('Ctrl Pts',(-2.24632385144714,5.74513138382193,40.4796856956901));
#57508=CARTESIAN_POINT('Ctrl Pts',(-4.72445695386775,3.96636003837356,40.618859153112));
#57509=CARTESIAN_POINT('Ctrl Pts',(-6.04729475788563,1.21767465860342,40.758032610534));
#57510=CARTESIAN_POINT('Ctrl Pts',(-5.89135706028292,-1.8287748497862,40.8972060679559));
#57511=CARTESIAN_POINT('Ctrl Pts',(-4.29477609311154,-4.42802481621249,
41.0363795253779));
#57512=CARTESIAN_POINT('Ctrl Pts',(-1.64797185657537,-5.9444675306449,41.1755529827998));
#57513=CARTESIAN_POINT('Ctrl Pts',(1.4018192536676,-6.00727960419713,41.3147264402217));
#57514=CARTESIAN_POINT('Ctrl Pts',(4.10881642827179,-4.60110128357549,41.4538998976438));
#57515=CARTESIAN_POINT('Ctrl Pts',(5.81106398870155,-2.06979244905675,41.5930733550657));
#57516=CARTESIAN_POINT('Ctrl Pts',(6.09230274951283,0.967653177142854,41.7322468124877));
#57517=CARTESIAN_POINT('Ctrl Pts',(4.88375997740181,3.76847368918562,41.8714202699095));
#57518=CARTESIAN_POINT('Ctrl Pts',(2.48096673470485,5.64777031440231,42.0105937273315));
#57519=CARTESIAN_POINT('Ctrl Pts',(-0.528509822516023,6.14598916615219,
42.1497671847535));
#57520=CARTESIAN_POINT('Ctrl Pts',(-3.40874720599174,5.14129827461892,42.2889406421755));
#57521=CARTESIAN_POINT('Ctrl Pts',(-5.45542643474629,2.87937977315038,42.4281140995974));
#57522=CARTESIAN_POINT('Ctrl Pts',(-6.16806270948796,-0.0866479935138681,
42.5672875570194));
#57523=CARTESIAN_POINT('Ctrl Pts',(-5.37239148601215,-3.03148728910088,
42.7064610144413));
#57524=CARTESIAN_POINT('Ctrl Pts',(-3.26298226352938,-5.2350217010867,42.8456344718633));
#57525=CARTESIAN_POINT('Ctrl Pts',(-0.355659523231457,-6.15840984073736,
42.9848079292852));
#57526=CARTESIAN_POINT('Ctrl Pts',(2.63863443492995,-5.5758509468742,43.1239813867072));
#57527=CARTESIAN_POINT('Ctrl Pts',(4.98768980024473,-3.62980108538893,43.2631548441291));
#57528=CARTESIAN_POINT('Ctrl Pts',(6.11708021096689,-0.796137648621998,
43.402328301551));
#57529=CARTESIAN_POINT('Ctrl Pts',(5.7506301310911,2.23220934465008,43.541501758973));
#57530=CARTESIAN_POINT('Ctrl Pts',(3.97794944774594,4.71470292321093,43.680675216395));
#57531=CARTESIAN_POINT('Ctrl Pts',(1.23252071332536,6.04428640570416,43.8198486738169));
#57532=CARTESIAN_POINT('Ctrl Pts',(-1.81430253038862,5.89583003411575,43.9590221312389));
#57533=CARTESIAN_POINT('Ctrl Pts',(-4.41746522142847,4.30563659409686,44.0981955886608));
#57534=CARTESIAN_POINT('Ctrl Pts',(-5.94040285147039,1.66256411160545,44.2373690460828));
#57535=CARTESIAN_POINT('Ctrl Pts',(-6.01070379714092,-1.38706356234736,
44.3765425035047));
#57536=CARTESIAN_POINT('Ctrl Pts',(-4.61117701345869,-4.09750558431666,
44.5157159609267));
#57537=CARTESIAN_POINT('Ctrl Pts',(-2.08405584680928,-5.80596388985809,
44.6548894183486));
#57538=CARTESIAN_POINT('Ctrl Pts',(0.952690012146062,-6.0946605486863,44.7940628757706));
#57539=CARTESIAN_POINT('Ctrl Pts',(3.75646977518502,-4.89299911006301,44.9332363331926));
#57540=CARTESIAN_POINT('Ctrl Pts',(5.64166102905991,-2.49482790912372,45.0724097906145));
#57541=CARTESIAN_POINT('Ctrl Pts',(6.14726844384006,0.513416149263214,45.2115832480365));
#57542=CARTESIAN_POINT('Ctrl Pts',(5.14965328710884,3.39611196598774,45.3507567054584));
#57543=CARTESIAN_POINT('Ctrl Pts',(2.89276742707903,5.44833938698633,45.4899301628804));
#57544=CARTESIAN_POINT('Ctrl Pts',(-0.0715014487153603,6.16825688552184,
45.6291036203023));
#57545=CARTESIAN_POINT('Ctrl Pts',(-3.01828571446114,5.37981940299448,45.7682770777242));
#57546=CARTESIAN_POINT('Ctrl Pts',(-5.22699334426712,3.27582753543943,45.9074505351462));
#57547=CARTESIAN_POINT('Ctrl Pts',(-6.15751791634193,0.370781030912171,
46.0466239925682));
#57548=CARTESIAN_POINT('Ctrl Pts',(-5.58231356167591,-2.62493443005441,
46.1857974499901));
#57549=CARTESIAN_POINT('Ctrl Pts',(-3.64203790358019,-4.97876142949642,
46.3249709074121));
#57550=CARTESIAN_POINT('Ctrl Pts',(-0.811156339303846,-6.11510677389718,
46.464144364834));
#57551=CARTESIAN_POINT('Ctrl Pts',(2.21808137769395,-5.75609420222458,46.603317822256));
#57552=CARTESIAN_POINT('Ctrl Pts',(4.70492046302962,-3.98951487019676,46.7424912796779));
#57553=CARTESIAN_POINT('Ctrl Pts',(6.0412416066478,-1.24735933598286,46.8816647370999));
#57554=CARTESIAN_POINT('Ctrl Pts',(5.90026745626159,1.79981927079816,47.0208381945218));
#57555=CARTESIAN_POINT('Ctrl Pts',(4.31647113221644,4.4068789894548,47.1600116519438));
#57556=CARTESIAN_POINT('Ctrl Pts',(1.67714634142165,5.93630235183586,47.2991851093657));
#57557=CARTESIAN_POINT('Ctrl Pts',(-1.37229950707301,6.01409174571216,47.4383585667878));
#57558=CARTESIAN_POINT('Ctrl Pts',(-4.08617003251941,4.62122493807609,47.5775320242095));
#57559=CARTESIAN_POINT('Ctrl Pts',(-5.80082878121777,2.09830667776461,47.7167054816318));
#57560=CARTESIAN_POINT('Ctrl Pts',(-6.09698159723034,-0.937721102455593,
47.8558789390534));
#57561=CARTESIAN_POINT('Ctrl Pts',(-4.90220873807901,-3.74444320977871,
47.9950523964757));
#57562=CARTESIAN_POINT('Ctrl Pts',(-2.50867403980139,-5.63551772466226,
48.1342258538973));
#57563=CARTESIAN_POINT('Ctrl Pts',(0.498319380125655,-6.14851065367438,
48.2733993113196));
#57564=CARTESIAN_POINT('Ctrl Pts',(3.38345624752536,-5.15797724733616,48.4125727687412));
#57565=CARTESIAN_POINT('Ctrl Pts',(5.44121948589513,-2.90613763770253,48.5517462261634));
#57566=CARTESIAN_POINT('Ctrl Pts',(6.16841386714245,0.056354472765162,48.6909196835852));
#57567=CARTESIAN_POINT('Ctrl Pts',(5.38721487981911,3.00506593964454,48.8300931410073));
#57568=CARTESIAN_POINT('Ctrl Pts',(3.28865305420277,5.21893346882663,48.9692665984291));
#57569=CARTESIAN_POINT('Ctrl Pts',(0.385900302793842,6.1565888622889,49.1084400558511));
#57570=CARTESIAN_POINT('Ctrl Pts',(-2.61121859689906,5.58874251528593,49.247613513273));
#57571=CARTESIAN_POINT('Ctrl Pts',(-4.96980303695856,3.65425276038667,49.386786970695));
#57572=CARTESIAN_POINT('Ctrl Pts',(-6.11309646290787,0.826170138736081,
49.5259604281169));
#57573=CARTESIAN_POINT('Ctrl Pts',(-5.76152356427402,-2.20394003577031,
49.665133885539));
#57574=CARTESIAN_POINT('Ctrl Pts',(-4.00105623598661,-4.69510963231198,
49.8043073429608));
#57575=CARTESIAN_POINT('Ctrl Pts',(-1.2621904370991,-6.03816037907669,49.9434808003828));
#57576=CARTESIAN_POINT('Ctrl Pts',(1.78532515834877,-5.90466929996279,50.0826542578047));
#57577=CARTESIAN_POINT('Ctrl Pts',(4.39626618412638,-4.3272796421381,50.2218277152268));
#57578=CARTESIAN_POINT('Ctrl Pts',(5.93216605646731,-1.6917184580932,50.3610011726486));
#57579=CARTESIAN_POINT('Ctrl Pts',(6.01744342948154,1.35752717687174,50.5001746300706));
#57580=CARTESIAN_POINT('Ctrl Pts',(4.6312449968388,4.07480984123329,50.6393480874926));
#57581=CARTESIAN_POINT('Ctrl Pts',(2.11254485599046,5.7956586937452,50.7785215449145));
#57582=CARTESIAN_POINT('Ctrl Pts',(-0.922746538333597,6.09926588114908,
50.9176950023365));
#57583=CARTESIAN_POINT('Ctrl Pts',(-3.73239406548654,4.91138880591599,51.0568684597585));
#57584=CARTESIAN_POINT('Ctrl Pts',(-5.62934043825332,2.52250504324608,51.1960419171804));
#57585=CARTESIAN_POINT('Ctrl Pts',(-6.14971578816463,-0.483219606136435,
51.3352153746023));
#57586=CARTESIAN_POINT('Ctrl Pts',(-5.16627010510767,-3.37078012691822,
51.4743888320243));
#57587=CARTESIAN_POINT('Ctrl Pts',(-2.91949032439888,-5.43406677440547,
51.6135622894462));
#57588=CARTESIAN_POINT('Ctrl Pts',(0.0412071569990902,-6.16853365340321,
51.7527357468682));
#57589=CARTESIAN_POINT('Ctrl Pts',(2.99182804436595,-5.39457787189151,51.8919092042902));
#57590=CARTESIAN_POINT('Ctrl Pts',(5.21084212336603,-3.3014587424819,52.0310826617121));
#57591=CARTESIAN_POINT('Ctrl Pts',(6.15562268418046,-0.401017247707679,
52.170256119134));
#57592=CARTESIAN_POINT('Ctrl Pts',(5.59513776893782,2.59748701816997,52.3094295765561));
#57593=CARTESIAN_POINT('Ctrl Pts',(3.66644558215312,4.96081467664999,52.4486030339779));
#57594=CARTESIAN_POINT('Ctrl Pts',(0.84117895638593,6.11104929012109,52.5877764913999));
#57595=CARTESIAN_POINT('Ctrl Pts',(-2.18978540415105,5.76691818450055,52.7269499488218));
#57596=CARTESIAN_POINT('Ctrl Pts',(-4.68527049021703,4.01257347552135,52.8661234062438));
#57597=CARTESIAN_POINT('Ctrl Pts',(-6.03504274157056,1.27701392724298,53.0052968636658));
#57598=CARTESIAN_POINT('Ctrl Pts',(-5.90903553867634,-1.77082028043954,
53.1444703210877));
#57599=CARTESIAN_POINT('Ctrl Pts',(-4.33806205868681,-4.38562686943817,
53.2836437785097));
#57600=CARTESIAN_POINT('Ctrl Pts',(-1.70628037375065,-5.92799399030643,
53.4228172359316));
#57601=CARTESIAN_POINT('Ctrl Pts',(1.34274666082029,-6.02075882823852,53.5619906933536));
#57602=CARTESIAN_POINT('Ctrl Pts',(4.06342507895993,-4.64123712932612,53.7011641507755));
#57603=CARTESIAN_POINT('Ctrl Pts',(5.79045365861584,-2.12677029563103,53.8403376081975));
#57604=CARTESIAN_POINT('Ctrl Pts',(6.10151338666836,0.907766410076269,53.9795110656194));
#57605=CARTESIAN_POINT('Ctrl Pts',(4.92053925821843,3.7203224149645,54.1186845230414));
#57606=CARTESIAN_POINT('Ctrl Pts',(2.53632083605719,5.62312920708197,54.2578579804633));
#57607=CARTESIAN_POINT('Ctrl Pts',(-0.468116918346931,6.15088384004395,
54.3970314378853));
#57608=CARTESIAN_POINT('Ctrl Pts',(-3.35808368060321,5.17453181041749,54.5362048953072));
#57609=CARTESIAN_POINT('Ctrl Pts',(-5.42688129564815,2.93282540665145,54.6753783527292));
#57610=CARTESIAN_POINT('Ctrl Pts',(-6.16861624358182,-0.026059592755391,
54.8145518101512));
#57611=CARTESIAN_POINT('Ctrl Pts',(-5.40190833481288,-2.97857210844981,
54.9537252675732));
#57612=CARTESIAN_POINT('Ctrl Pts',(-3.3142445230586,-5.20271935667608,55.092898724995));
#57613=CARTESIAN_POINT('Ctrl Pts',(-0.416131774498588,-6.15461938784266,
55.232072182417));
#57614=CARTESIAN_POINT('Ctrl Pts',(2.58373977666849,-5.60149928406824,55.3712456398389));
#57615=CARTESIAN_POINT('Ctrl Pts',(4.95179640277048,-3.67861629535691,55.5104190972609));
#57616=CARTESIAN_POINT('Ctrl Pts',(6.10896526788126,-0.856182701750285,
55.6495925546829));
#57617=CARTESIAN_POINT('Ctrl Pts',(5.77227803037462,2.17561756818853,55.7887660121049));
#57618=CARTESIAN_POINT('Ctrl Pts',(4.0240665193521,4.67540309607475,55.9279394695267));
#57619=CARTESIAN_POINT('Ctrl Pts',(1.29182971702892,6.03188871292874,56.0671129269488));
#57620=CARTESIAN_POINT('Ctrl Pts',(-1.75630472453483,5.91336614607388,56.2062863843706));
#57621=CARTESIAN_POINT('Ctrl Pts',(-4.37496110954512,4.34881831684468,56.3454598417927));
#57622=CARTESIAN_POINT('Ctrl Pts',(-5.92378617851085,1.72083200058572,56.4846332992145));
#57623=CARTESIAN_POINT('Ctrl Pts',(-6.02403792199122,-1.32795804804506,
56.6238067566366));
#57624=CARTESIAN_POINT('Ctrl Pts',(-4.65120127528559,-4.0520158143494,56.7629802140584));
#57625=CARTESIAN_POINT('Ctrl Pts',(-2.14098291090698,-5.78521370721604,
56.9021536714805));
#57626=CARTESIAN_POINT('Ctrl Pts',(0.892780808013698,-6.10372410023572,
57.0413271289024));
#57627=CARTESIAN_POINT('Ctrl Pts',(3.7082283310046,-4.92966003980913,57.1805005863244));
#57628=CARTESIAN_POINT('Ctrl Pts',(5.6168840686018,-2.55012133492571,57.3196740437463));
#57629=CARTESIAN_POINT('Ctrl Pts',(6.15201480226891,0.453011407825745,57.4588475011683));
#57630=CARTESIAN_POINT('Ctrl Pts',(5.18276231344806,3.34536698513908,57.5980209585902));
#57631=CARTESIAN_POINT('Ctrl Pts',(2.9461428040507,5.4196630929511,57.7371944160122));
#57632=CARTESIAN_POINT('Ctrl Pts',(-0.0109118713727406,6.16866163718024,
57.8763678734341));
#57633=CARTESIAN_POINT('Ctrl Pts',(-2.96529821182842,5.4092062243811,58.0155413308561));
#57634=CARTESIAN_POINT('Ctrl Pts',(-5.19456521773649,3.32701031883556,58.154714788278));
#57635=CARTESIAN_POINT('Ctrl Pts',(-6.1535789793253,0.431243792027107,58.2938882457));
#57636=CARTESIAN_POINT('Ctrl Pts',(-5.60782702231775,-2.56997695528946,
58.4330617031219));
#57637=CARTESIAN_POINT('Ctrl Pts',(-3.69076482660954,-4.94274826969955,
58.5722351605439));
#57638=CARTESIAN_POINT('Ctrl Pts',(-0.871181284357699,-6.10684440875489,
58.7114086179658));
#57639=CARTESIAN_POINT('Ctrl Pts',(2.16143661331375,-5.77760306957677,58.8505820753878));
#57640=CARTESIAN_POINT('Ctrl Pts',(4.6655075093848,-4.03553529817666,58.9897555328097));
#57641=CARTESIAN_POINT('Ctrl Pts',(6.02869831216978,-1.30663771711886,59.1289289902318));
#57642=CARTESIAN_POINT('Ctrl Pts',(5.91766109604211,1.74177857816241,59.2681024476536));
#57643=CARTESIAN_POINT('Ctrl Pts',(4.35954835175235,4.36426896876084,59.4072759050756));
#57644=CARTESIAN_POINT('Ctrl Pts',(1.73537325085302,5.91954264645359,59.5464493624975));
#57645=CARTESIAN_POINT('Ctrl Pts',(-1.31316142771993,6.0272806909664,59.6856228199195));
#57646=CARTESIAN_POINT('Ctrl Pts',(-4.04058211619944,4.66113737463529,59.8247962773414));
#57647=CARTESIAN_POINT('Ctrl Pts',(-5.77993887114087,2.15518261611504,59.9639697347634));
#57648=CARTESIAN_POINT('Ctrl Pts',(-6.10589800852354,-0.877789822503519,
60.1031431921854));
#57649=CARTESIAN_POINT('Ctrl Pts',(-4.93875109568499,-3.69611188654187,
60.2423166496073));
#57650=CARTESIAN_POINT('Ctrl Pts',(-2.56390645664619,-5.61060506045379,
60.3814901070292));
#57651=CARTESIAN_POINT('Ctrl Pts',(0.437903165679336,-6.15310866805281,
60.5206635644512));
#57652=CARTESIAN_POINT('Ctrl Pts',(3.3326301171667,-5.19096156450552,60.6598370218731));
#57653=CARTESIAN_POINT('Ctrl Pts',(5.41241220991924,-2.95944243641773,60.7990104792952));
#57654=CARTESIAN_POINT('Ctrl Pts',(6.16866983377028,-0.00423591556452433,
60.938183936717));
#57655=CARTESIAN_POINT('Ctrl Pts',(5.41647149689117,2.95200643406812,61.077357394139));
#57656=CARTESIAN_POINT('Ctrl Pts',(3.3397560522476,5.18637975664333,61.2165308515609));
#57657=CARTESIAN_POINT('Ctrl Pts',(0.446353210313549,6.15250146309482,61.3557043089829));
#57658=CARTESIAN_POINT('Ctrl Pts',(-2.55619863925694,5.61412094905446,61.4948777664048));
#57659=CARTESIAN_POINT('Ctrl Pts',(-4.93367032764008,3.70289109578226,61.6340512238268));
#57660=CARTESIAN_POINT('Ctrl Pts',(-6.10468673402829,0.886174627170678,
61.7732246812487));
#57661=CARTESIAN_POINT('Ctrl Pts',(-5.78289325342531,-2.14724265117775,
61.9123981386708));
#57662=CARTESIAN_POINT('Ctrl Pts',(-4.04697977515619,-4.6555837388399,62.0515715960926));
#57663=CARTESIAN_POINT('Ctrl Pts',(-1.32143777519505,-6.02547165794721,
62.1907450535147));
#57664=CARTESIAN_POINT('Ctrl Pts',(1.72724180600375,-5.92192016880478,62.3299185109365));
#57665=CARTESIAN_POINT('Ctrl Pts',(4.35355075125749,-4.37025247680389,62.4690919683585));
#57666=CARTESIAN_POINT('Ctrl Pts',(5.91526295226815,-1.74990329951406,62.6082654257805));
#57667=CARTESIAN_POINT('Ctrl Pts',(6.03048802723082,1.29835545109493,62.7474388832024));
#57668=CARTESIAN_POINT('Ctrl Pts',(4.67104358963708,4.0291268577618,62.8866123406244));
#57669=CARTESIAN_POINT('Ctrl Pts',(2.16937279271135,5.77462371327947,63.0257857980464));
#57670=CARTESIAN_POINT('Ctrl Pts',(-0.862800305444146,6.10804576400077,
63.1649592554682));
#57671=CARTESIAN_POINT('Ctrl Pts',(-3.68395996768377,4.94779156902649,63.3041327128903));
#57672=CARTESIAN_POINT('Ctrl Pts',(-5.60431794598028,2.5777167089644,63.4433061703121));
#57673=CARTESIAN_POINT('Ctrl Pts',(-6.15411517187233,-0.422871685852421,
63.5824796277342));
#57674=CARTESIAN_POINT('Ctrl Pts',(-5.19922846621166,-3.3197157566242,63.7216530851561));
#57675=CARTESIAN_POINT('Ctrl Pts',(-2.97252143221046,-5.40546228751415,
63.8608265425781));
#57676=CARTESIAN_POINT('Ctrl Pts',(-1.00409531133336,-5.91362404918468,
63.953608847526));
#57677=CARTESIAN_POINT('Ctrl Pts',(-0.0185920708322156,-5.91672078920428,
64.));
#57678=CARTESIAN_POINT('Ctrl Pts',(3.24375760296866,-4.54512507566742,-0.384322829190561));
#57679=CARTESIAN_POINT('Ctrl Pts',(4.00080456363074,-4.00483701019733,-0.337931676716577));
#57680=CARTESIAN_POINT('Ctrl Pts',(5.23892931934964,-2.53920478472433,-0.245149371768609));
#57681=CARTESIAN_POINT('Ctrl Pts',(5.81483236077834,0.281981155041063,-0.105975914346657));
#57682=CARTESIAN_POINT('Ctrl Pts',(4.96885277875867,3.03344919454013,0.0331975430752952));
#57683=CARTESIAN_POINT('Ctrl Pts',(2.90779432331117,5.0435085486934,0.172371000497248));
#57684=CARTESIAN_POINT('Ctrl Pts',(0.135688220029282,5.82006202178721,0.311544457919199));
#57685=CARTESIAN_POINT('Ctrl Pts',(-2.66960348256184,5.17350430475029,0.450717915341153));
#57686=CARTESIAN_POINT('Ctrl Pts',(-4.82208097659197,3.26179326528778,0.589891372763104));
#57687=CARTESIAN_POINT('Ctrl Pts',(-5.79539200928568,0.552485204520095,
0.729064830185058));
#57688=CARTESIAN_POINT('Ctrl Pts',(-5.35152590761217,-2.2919380522483,0.868238287607008));
#57689=CARTESIAN_POINT('Ctrl Pts',(-3.59902452230347,-4.5758953628753,1.00741174502896));
#57690=CARTESIAN_POINT('Ctrl Pts',(-0.966435330409787,-5.74088936163419,
1.14658520245091));
#57691=CARTESIAN_POINT('Ctrl Pts',(1.90248107735391,-5.50203293656693,1.28575865987286));
#57692=CARTESIAN_POINT('Ctrl Pts',(4.30617423462377,-3.91773754708874,1.42493211729482));
#57693=CARTESIAN_POINT('Ctrl Pts',(5.65685685325898,-1.37541755843866,1.56410557471677));
#57694=CARTESIAN_POINT('Ctrl Pts',(5.62423973364523,1.50323998611993,1.70327903213872));
#57695=CARTESIAN_POINT('Ctrl Pts',(4.2162988858458,4.01430279461926,1.84245248956067));
#57696=CARTESIAN_POINT('Ctrl Pts',(1.77732519943232,5.54372782159637,1.98162594698263));
#57697=CARTESIAN_POINT('Ctrl Pts',(-1.09626678800386,5.71751714322285,2.12079940440458));
#57698=CARTESIAN_POINT('Ctrl Pts',(-3.70178312518057,4.49317313079981,2.25997286182653));
#57699=CARTESIAN_POINT('Ctrl Pts',(-5.40208375610618,2.17009082878763,2.39914631924848));
#57700=CARTESIAN_POINT('Ctrl Pts',(-5.78138558716672,-0.683654738165986,
2.53831977667044));
#57701=CARTESIAN_POINT('Ctrl Pts',(-4.74693602800832,-3.37022276005692,
2.67749323409239));
#57702=CARTESIAN_POINT('Ctrl Pts',(-2.55169424895947,-5.23265320553137,
2.81666669151434));
#57703=CARTESIAN_POINT('Ctrl Pts',(0.267526200532523,-5.815516558252,2.95584014893629));
#57704=CARTESIAN_POINT('Ctrl Pts',(3.02132711829442,-4.97628230235617,3.09501360635824));
#57705=CARTESIAN_POINT('Ctrl Pts',(5.03630767028235,-2.92017262473365,3.2341870637802));
#57706=CARTESIAN_POINT('Ctrl Pts',(5.81973449459707,-0.149978400157519,
3.37336052120215));
#57707=CARTESIAN_POINT('Ctrl Pts',(5.18003227673358,2.65689079943647,3.5125339786241));
#57708=CARTESIAN_POINT('Ctrl Pts',(3.27363062794811,4.81405708522912,3.65170743604605));
#57709=CARTESIAN_POINT('Ctrl Pts',(0.566711563064284,5.79401770038826,3.79088089346801));
#57710=CARTESIAN_POINT('Ctrl Pts',(-2.27878833994558,5.35713793081986,3.93005435088995));
#57711=CARTESIAN_POINT('Ctrl Pts',(-4.56704463148848,3.61025019106752,4.06922780831191));
#57712=CARTESIAN_POINT('Ctrl Pts',(-5.73849845411803,0.980529754873716,
4.20840126573386));
#57713=CARTESIAN_POINT('Ctrl Pts',(-5.50668829346455,-1.88896457000346,
4.34757472315581));
#57714=CARTESIAN_POINT('Ctrl Pts',(-3.92829985781997,-4.29654085691737,
4.48674818057777));
#57715=CARTESIAN_POINT('Ctrl Pts',(-1.38930443585496,-5.65346232786791,
4.62592163799971));
#57716=CARTESIAN_POINT('Ctrl Pts',(1.48942461019975,-5.62791412857727,4.76509509542168));
#57717=CARTESIAN_POINT('Ctrl Pts',(4.00393714072872,-4.22614368913331,4.90426855284362));
#57718=CARTESIAN_POINT('Ctrl Pts',(5.53934671848404,-1.79093300838651,5.04344201026558));
#57719=CARTESIAN_POINT('Ctrl Pts',(5.72019189178477,1.08222355789733,5.18261546768752));
#57720=CARTESIAN_POINT('Ctrl Pts',(4.50224967786418,3.69073853669968,5.32178892510949));
#57721=CARTESIAN_POINT('Ctrl Pts',(2.18334963199351,5.39673859776273,5.46096238253143));
#57722=CARTESIAN_POINT('Ctrl Pts',(-0.669455916507752,5.78304693772763,
5.60013583995339));
#57723=CARTESIAN_POINT('Ctrl Pts',(-3.35855603169015,4.75519762892206,5.73930929737534));
#57724=CARTESIAN_POINT('Ctrl Pts',(-5.22637149326653,2.56453584932617,5.87848275479729));
#57725=CARTESIAN_POINT('Ctrl Pts',(-5.81615596147474,-0.253244822079318,
6.01765621221924));
#57726=CARTESIAN_POINT('Ctrl Pts',(-4.98368646426841,-3.0090982592757,6.1568296696412));
#57727=CARTESIAN_POINT('Ctrl Pts',(-2.93253096841646,-5.02912171530841,
6.29600312706314));
#57728=CARTESIAN_POINT('Ctrl Pts',(-0.164268877390996,-5.81934866149373,
6.4351765844851));
#57729=CARTESIAN_POINT('Ctrl Pts',(2.6441627111189,-5.1865409152186,6.57435004190705));
#57730=CARTESIAN_POINT('Ctrl Pts',(4.80600384951016,-3.28544214780928,6.71352349932901));
#57731=CARTESIAN_POINT('Ctrl Pts',(5.79260861562399,-0.580937633749912,
6.85269695675095));
#57732=CARTESIAN_POINT('Ctrl Pts',(5.36271756762338,2.26562649128486,6.99187041417291));
#57733=CARTESIAN_POINT('Ctrl Pts',(3.62145413269375,4.55816553811986,7.13104387159486));
#57734=CARTESIAN_POINT('Ctrl Pts',(0.994618244943479,5.73607336554666,7.2702173290168));
#57735=CARTESIAN_POINT('Ctrl Pts',(-1.87543666105779,5.51131022883567,7.40939078643877));
#57736=CARTESIAN_POINT('Ctrl Pts',(-4.28688157693133,3.93883859195511,7.54856424386071));
#57737=CARTESIAN_POINT('Ctrl Pts',(-5.65003370931712,1.40318287891794,7.68773770128267));
#57738=CARTESIAN_POINT('Ctrl Pts',(-5.63155458885656,-1.47560022392137,
7.82691115870462));
#57739=CARTESIAN_POINT('Ctrl Pts',(-4.23596300812098,-3.99354735816903,
7.96608461612657));
#57740=CARTESIAN_POINT('Ctrl Pts',(-1.80453001846248,-5.53493220559892,
8.10525807354854));
#57741=CARTESIAN_POINT('Ctrl Pts',(1.06817380221706,-5.7228321516855,8.24443153097047));
#57742=CARTESIAN_POINT('Ctrl Pts',(3.67967169306626,-4.51129907447457,8.38360498839244));
#57743=CARTESIAN_POINT('Ctrl Pts',(5.3913608972928,-2.19659527069743,8.52277844581438));
#57744=CARTESIAN_POINT('Ctrl Pts',(5.78467341665285,0.655253058579685,8.66195190323633));
#57745=CARTESIAN_POINT('Ctrl Pts',(4.76343055614367,3.34686905105429,8.80112536065828));
#57746=CARTESIAN_POINT('Ctrl Pts',(2.57736198560756,5.22005826626995,8.94029881808025));
#57747=CARTESIAN_POINT('Ctrl Pts',(-0.238961916563357,5.81676029337126,
9.07947227550219));
#57748=CARTESIAN_POINT('Ctrl Pts',(-2.9968512554821,4.99106057472994,9.21864573292415));
#57749=CARTESIAN_POINT('Ctrl Pts',(-5.02190543487286,2.94487162900228,9.35781919034609));
#57750=CARTESIAN_POINT('Ctrl Pts',(-5.81892773788428,0.178558364097456,
9.49699264776805));
#57751=CARTESIAN_POINT('Ctrl Pts',(-5.19301827900942,-2.63141867858048,
9.63616610518999));
#57752=CARTESIAN_POINT('Ctrl Pts',(-3.29723385654803,-4.79792163372242,
9.77533956261196));
#57753=CARTESIAN_POINT('Ctrl Pts',(-0.595160201398069,-5.79116460159612,
9.9145130200339));
#57754=CARTESIAN_POINT('Ctrl Pts',(2.25245098096098,-5.36826486739209,10.0536864774559));
#57755=CARTESIAN_POINT('Ctrl Pts',(4.54925895914298,-3.63263623705505,10.1928599348778));
#57756=CARTESIAN_POINT('Ctrl Pts',(5.73361368861633,-1.00870073749333,10.3320333922998));
#57757=CARTESIAN_POINT('Ctrl Pts',(5.51589893116313,1.86189744328243,10.4712068497217));
#57758=CARTESIAN_POINT('Ctrl Pts',(3.94935357500579,4.27719644717158,10.6103803071437));
#57759=CARTESIAN_POINT('Ctrl Pts',(1.41705286082813,5.64657102122404,10.7495537645656));
#57760=CARTESIAN_POINT('Ctrl Pts',(-1.46176693981568,5.63516109102216,10.8887272219876));
#57761=CARTESIAN_POINT('Ctrl Pts',(-3.98313349463256,4.24575678437242,11.0279006794095));
#57762=CARTESIAN_POINT('Ctrl Pts',(-5.53048431723029,1.81811614727388,11.1670741368315));
#57763=CARTESIAN_POINT('Ctrl Pts',(-5.72543790307144,-1.05411760547914,
11.3062475942534));
#57764=CARTESIAN_POINT('Ctrl Pts',(-4.52032126808012,-3.66858266111734,
11.4454210516754));
#57765=CARTESIAN_POINT('Ctrl Pts',(-2.20982766399449,-5.38595068707029,
11.5845945090973));
#57766=CARTESIAN_POINT('Ctrl Pts',(0.641046249494328,-5.7862650141622,11.7237679665193));
#57767=CARTESIAN_POINT('Ctrl Pts',(3.33516188889343,-4.77163476001475,11.8629414239412));
#57768=CARTESIAN_POINT('Ctrl Pts',(5.21371356247076,-2.59017258046961,12.0021148813632));
#57769=CARTESIAN_POINT('Ctrl Pts',(5.81732955036896,0.224677570113848,12.1412883387851));
#57770=CARTESIAN_POINT('Ctrl Pts',(4.99840458923842,2.98458618076083,12.2804617962071));
#57771=CARTESIAN_POINT('Ctrl Pts',(2.9571945320961,5.01465887249064,12.419635253629));
#57772=CARTESIAN_POINT('Ctrl Pts',(0.192846774102069,5.81847172630637,12.558808711051));
#57773=CARTESIAN_POINT('Ctrl Pts',(-2.6186587786624,5.19946432904799,12.697982168473));
#57774=CARTESIAN_POINT('Ctrl Pts',(-4.78981048660394,3.30900568306057,12.8371556258949));
#57775=CARTESIAN_POINT('Ctrl Pts',(-5.78968566701073,0.60937918024717,12.9763290833169));
#57776=CARTESIAN_POINT('Ctrl Pts',(-5.37377979667661,-2.23926188842183,
13.1155025407388));
#57777=CARTESIAN_POINT('Ctrl Pts',(-3.64379643672339,-4.54032494826418,
13.2546759981608));
#57778=CARTESIAN_POINT('Ctrl Pts',(-1.02277714760654,-5.73111943815883,
13.3938494555827));
#57779=CARTESIAN_POINT('Ctrl Pts',(1.84834699831852,-5.52045437277723,13.5330229130047));
#57780=CARTESIAN_POINT('Ctrl Pts',(4.26748552603914,-3.95984474356694,13.6721963704266));
#57781=CARTESIAN_POINT('Ctrl Pts',(5.64307428446858,-1.43091429794995,13.8113698278486));
#57782=CARTESIAN_POINT('Ctrl Pts',(5.63873361332696,1.447924841297,13.9505432852705));
#57783=CARTESIAN_POINT('Ctrl Pts',(4.2555249588314,3.97269561291463,14.0897167426925));
#57784=CARTESIAN_POINT('Ctrl Pts',(1.83169131289668,5.52600308019885,14.2288902001144));
#57785=CARTESIAN_POINT('Ctrl Pts',(-1.04005505244218,5.72800913022995,14.3680636575364));
#57786=CARTESIAN_POINT('Ctrl Pts',(-3.65747150771956,4.52931620427717,14.5072371149583));
#57787=CARTESIAN_POINT('Ctrl Pts',(-5.38050799971861,2.22304673209365,14.6464105723803));
#57788=CARTESIAN_POINT('Ctrl Pts',(-5.78782172065838,-0.626835574918385,
14.7855840298022));
#57789=CARTESIAN_POINT('Ctrl Pts',(-4.7798101910642,-3.32343461580141,14.9247574872242));
#57790=CARTESIAN_POINT('Ctrl Pts',(-2.60296755666481,-5.20733742012736,
15.0639309446461));
#57791=CARTESIAN_POINT('Ctrl Pts',(0.21039186886499,-5.81786372903523,15.2031044020681));
#57792=CARTESIAN_POINT('Ctrl Pts',(2.97230310906994,-5.00571846350965,15.34227785949));
#57793=CARTESIAN_POINT('Ctrl Pts',(5.0073820718583,-2.96949960339115,15.481451316912));
#57794=CARTESIAN_POINT('Ctrl Pts',(5.81798062950974,-0.207134021246128,
15.620624774334));
#57795=CARTESIAN_POINT('Ctrl Pts',(5.20587902646482,2.60588308830651,15.7597982317559));
#57796=CARTESIAN_POINT('Ctrl Pts',(3.32075755636313,4.78167045706469,15.8989716891779));
#57797=CARTESIAN_POINT('Ctrl Pts',(0.623594484557181,5.78817182078575,16.0381451465998));
#57798=CARTESIAN_POINT('Ctrl Pts',(-2.22605929319732,5.37926232222207,16.1773186040218));
#57799=CARTESIAN_POINT('Ctrl Pts',(-4.53136355935532,3.65493466440303,16.3164920614437));
#57800=CARTESIAN_POINT('Ctrl Pts',(-5.72859062921443,1.03684739040267,16.4556655188657));
#57801=CARTESIAN_POINT('Ctrl Pts',(-5.52497652620875,-1.83478540787485,
16.5948389762876));
#57802=CARTESIAN_POINT('Ctrl Pts',(-3.97031203437715,-4.25774887209054,
16.7340124337096));
#57803=CARTESIAN_POINT('Ctrl Pts',(-1.44476710669936,-5.63954352013598,
16.8731858911315));
#57804=CARTESIAN_POINT('Ctrl Pts',(1.43407401183274,-5.64227213422874,17.0123593485535));
#57805=CARTESIAN_POINT('Ctrl Pts',(3.96223377595531,-4.2652674725962,17.1515328059754));
#57806=CARTESIAN_POINT('Ctrl Pts',(5.52148852152625,-1.84525543347313,17.2907062633974));
#57807=CARTESIAN_POINT('Ctrl Pts',(5.73054581765664,1.02598622790277,17.4298797208193));
#57808=CARTESIAN_POINT('Ctrl Pts',(4.53828382882664,3.64633829987275,17.5690531782413));
#57809=CARTESIAN_POINT('Ctrl Pts',(2.23625239528441,5.37503286805699,17.7082266356632));
#57810=CARTESIAN_POINT('Ctrl Pts',(-0.612621120541769,5.78934352675451,
17.8474000930852));
#57811=CARTESIAN_POINT('Ctrl Pts',(-3.31168730249335,4.78795679999438,17.9865735505071));
#57812=CARTESIAN_POINT('Ctrl Pts',(-5.20092987768768,2.61574683703981,18.1257470079291));
#57813=CARTESIAN_POINT('Ctrl Pts',(-5.81836282614899,-0.196104898959158,
18.264920465351));
#57814=CARTESIAN_POINT('Ctrl Pts',(-5.01300215344117,-2.96000211447599,
18.404093922773));
#57815=CARTESIAN_POINT('Ctrl Pts',(-2.98178676868822,-5.00007507685475,
18.5432673801949));
#57816=CARTESIAN_POINT('Ctrl Pts',(-0.221420019377939,-5.81745445045571,
18.6824408376169));
#57817=CARTESIAN_POINT('Ctrl Pts',(2.59309168454985,-5.21226233257945,18.8216142950388));
#57818=CARTESIAN_POINT('Ctrl Pts',(4.77350159418886,-3.33248940559225,18.9607877524608));
#57819=CARTESIAN_POINT('Ctrl Pts',(5.78662307204959,-0.637806028610215,
19.0999612098827));
#57820=CARTESIAN_POINT('Ctrl Pts',(5.38471241096902,2.21284327489869,19.2391346673047));
#57821=CARTESIAN_POINT('Ctrl Pts',(3.66605085293078,4.52237484645332,19.3783081247266));
#57822=CARTESIAN_POINT('Ctrl Pts',(1.05091138103857,5.72602727703176,19.5174815821486));
#57823=CARTESIAN_POINT('Ctrl Pts',(-1.82121275372749,5.52946536418925,19.6566550395706));
#57824=CARTESIAN_POINT('Ctrl Pts',(-4.24798654403758,3.98075538431889,19.7958284969925));
#57825=CARTESIAN_POINT('Ctrl Pts',(-5.63597874951666,1.45861120354425,19.9350019544145));
#57826=CARTESIAN_POINT('Ctrl Pts',(-5.64577663239032,-1.4202145349431,20.0741754118364));
#57827=CARTESIAN_POINT('Ctrl Pts',(-4.27498426691963,-3.95174804683925,
20.2133488692584));
#57828=CARTESIAN_POINT('Ctrl Pts',(-1.85880842721184,-5.51694066843522,
20.3525223266803));
#57829=CARTESIAN_POINT('Ctrl Pts',(1.01191121669575,-5.73304795005533,20.4916957841023));
#57830=CARTESIAN_POINT('Ctrl Pts',(3.63518310470994,-4.54722408765388,20.6308692415243));
#57831=CARTESIAN_POINT('Ctrl Pts',(5.36952532510035,-2.2494445739369,20.7700426989462));
#57832=CARTESIAN_POINT('Ctrl Pts',(5.79083042327413,0.598402972077256,20.9092161563682));
#57833=CARTESIAN_POINT('Ctrl Pts',(4.79607453768151,3.29992001980522,21.0483896137901));
#57834=CARTESIAN_POINT('Ctrl Pts',(2.62851034453592,5.19449097378905,21.187563071212));
#57835=CARTESIAN_POINT('Ctrl Pts',(-0.181816746546373,5.81882683870069,
21.326736528634));
#57836=CARTESIAN_POINT('Ctrl Pts',(-2.94768327115363,5.02025561511257,21.4659099860559));
#57837=CARTESIAN_POINT('Ctrl Pts',(-4.99273793154097,2.99405595389602,21.6050834434779));
#57838=CARTESIAN_POINT('Ctrl Pts',(-5.81689319231709,0.235704682353347,
21.7442569008998));
#57839=CARTESIAN_POINT('Ctrl Pts',(-5.21861420890074,-2.58028464452422,
21.8834303583218));
#57840=CARTESIAN_POINT('Ctrl Pts',(-3.34420116000522,-4.76530394723442,
22.0226038157437));
#57841=CARTESIAN_POINT('Ctrl Pts',(-0.65201372671107,-5.78503943014121,
22.1617772731657));
#57842=CARTESIAN_POINT('Ctrl Pts',(2.19961391321817,-5.39013003005356,22.3009507305877));
#57843=CARTESIAN_POINT('Ctrl Pts',(4.51335886375986,-3.67714493527635,22.4401241880096));
#57844=CARTESIAN_POINT('Ctrl Pts',(5.72342939706778,-1.06496903470879,22.5792976454316));
#57845=CARTESIAN_POINT('Ctrl Pts',(5.53392085965116,1.80762911771912,22.7184711028535));
#57846=CARTESIAN_POINT('Ctrl Pts',(3.99117473041909,4.23819860074681,22.8576445602755));
#57847=CARTESIAN_POINT('Ctrl Pts',(1.47244650500515,5.63237999410608,22.9968180176974));
#57848=CARTESIAN_POINT('Ctrl Pts',(-1.40634649420028,5.64924708667967,23.1359914751194));
#57849=CARTESIAN_POINT('Ctrl Pts',(-3.94123848879507,4.28467528320974,23.2751649325413));
#57850=CARTESIAN_POINT('Ctrl Pts',(-5.51235954834917,1.8723502123887,23.4143383899633));
#57851=CARTESIAN_POINT('Ctrl Pts',(-5.73551551233822,-0.997830103692873,
23.5535118473852));
#57852=CARTESIAN_POINT('Ctrl Pts',(-4.55613692684949,-3.62400598949653,
23.6926853048072));
#57853=CARTESIAN_POINT('Ctrl Pts',(-2.2626231885028,-5.36398540405897,23.8318587622291));
#57854=CARTESIAN_POINT('Ctrl Pts',(0.584181215259813,-5.79228240125133,
23.9710322196511));
#57855=CARTESIAN_POINT('Ctrl Pts',(3.28813283869339,-4.80416335517584,24.1102056770731));
#57856=CARTESIAN_POINT('Ctrl Pts',(5.18802074725785,-2.64125800218955,24.249379134495));
#57857=CARTESIAN_POINT('Ctrl Pts',(5.81925576389236,0.167527497783788,24.388552591917));
#57858=CARTESIAN_POINT('Ctrl Pts',(5.02747880478565,2.93534665338514,24.5277260493389));
#57859=CARTESIAN_POINT('Ctrl Pts',(3.00630708503173,4.98537068015971,24.6668995067608));
#57860=CARTESIAN_POINT('Ctrl Pts',(0.249987924036234,5.81629685847829,24.8060729641828));
#57861=CARTESIAN_POINT('Ctrl Pts',(-2.5674620454557,5.22493461712705,24.9452464216047));
#57862=CARTESIAN_POINT('Ctrl Pts',(-4.75707756563297,3.35589274898047,25.0844198790267));
#57863=CARTESIAN_POINT('Ctrl Pts',(-5.7834209046099,0.666217493187736,25.2235933364487));
#57864=CARTESIAN_POINT('Ctrl Pts',(-5.39551514680761,-2.18637128792844,
25.3627667938706));
#57865=CARTESIAN_POINT('Ctrl Pts',(-3.68821684454273,-4.50431566564105,
25.5019402512926));
#57866=CARTESIAN_POINT('Ctrl Pts',(-1.07902026664608,-5.72079700498761,
25.6411137087145));
#57867=CARTESIAN_POINT('Ctrl Pts',(1.79403458175868,-5.53834298572796,25.7802871661365));
#57868=CARTESIAN_POINT('Ctrl Pts',(4.22838510123925,-4.0015700098494,25.9194606235584));
#57869=CARTESIAN_POINT('Ctrl Pts',(5.62874727560461,-1.48627292765558,26.0586340809804));
#57870=CARTESIAN_POINT('Ctrl Pts',(5.65268347617007,1.39246997322817,26.1978075384023));
#57871=CARTESIAN_POINT('Ctrl Pts',(4.29434046302999,3.93070516519512,26.3369809958243));
#57872=CARTESIAN_POINT('Ctrl Pts',(1.88588070734713,5.5077451888921,26.4761544532462));
#57873=CARTESIAN_POINT('Ctrl Pts',(-0.983742973802929,5.73794848962602,
26.6153279106682));
#57874=CARTESIAN_POINT('Ctrl Pts',(-3.61280702163031,4.56502229266922,26.7545013680901));
#57875=CARTESIAN_POINT('Ctrl Pts',(-5.35841313833848,2.27578815951525,26.8936748255121));
#57876=CARTESIAN_POINT('Ctrl Pts',(-5.79369945193068,-0.569955935846374,
27.032848282934));
#57877=CARTESIAN_POINT('Ctrl Pts',(-4.81222320370199,-3.27632583023427,
27.172021740356));
#57878=CARTESIAN_POINT('Ctrl Pts',(-2.65398973313268,-5.18151923710938,
27.3111951977779));
#57879=CARTESIAN_POINT('Ctrl Pts',(0.153237238835168,-5.81964959913759,
27.4503686551999));
#57880=CARTESIAN_POINT('Ctrl Pts',(2.92299233555996,-5.03467167890479,27.5895421126218));
#57881=CARTESIAN_POINT('Ctrl Pts',(4.97797336713532,-3.01854008822139,27.7287155700438));
#57882=CARTESIAN_POINT('Ctrl Pts',(5.81566545253513,-0.264269658299064,
27.8678890274657));
#57883=CARTESIAN_POINT('Ctrl Pts',(5.23122351914651,2.55462396466421,28.0070624848877));
#57884=CARTESIAN_POINT('Ctrl Pts',(3.36756410201807,4.74882249898934,28.1462359423097));
#57885=CARTESIAN_POINT('Ctrl Pts',(0.680417242391902,5.78176750521534,28.2854093997316));
#57886=CARTESIAN_POINT('Ctrl Pts',(-2.17311547888214,5.40086772875906,28.4245828571536));
#57887=CARTESIAN_POINT('Ctrl Pts',(-4.49524530662713,3.69926651396665,28.5637563145755));
#57888=CARTESIAN_POINT('Ctrl Pts',(-5.71813011666452,1.0930649921219,28.7029297719975));
#57889=CARTESIAN_POINT('Ctrl Pts',(-5.54273171575438,-1.78042922782082,
28.8421032294194));
#57890=CARTESIAN_POINT('Ctrl Pts',(-4.01194115992657,-4.21854610469001,
28.9812766868414));
#57891=CARTESIAN_POINT('Ctrl Pts',(-1.50009038812259,-5.62508061591747,
29.1204501442633));
#57892=CARTESIAN_POINT('Ctrl Pts',(1.37858505570179,-5.65608578014017,29.2596236016853));
#57893=CARTESIAN_POINT('Ctrl Pts',(3.92014813955503,-4.3039797480996,29.3987970591072));
#57894=CARTESIAN_POINT('Ctrl Pts',(5.50309761788848,-1.89939983049864,29.5379705165292));
#57895=CARTESIAN_POINT('Ctrl Pts',(5.74034686724793,0.969649911970882,29.6771439739511));
#57896=CARTESIAN_POINT('Ctrl Pts',(4.5738801315346,3.60158626864069,29.8163174313731));
#57897=CARTESIAN_POINT('Ctrl Pts',(2.28893940758999,5.35280856153943,29.955490888795));
#57898=CARTESIAN_POINT('Ctrl Pts',(-0.555727219614797,5.79508156676741,
30.094664346217));
#57899=CARTESIAN_POINT('Ctrl Pts',(-3.26449906562366,4.82025403465942,30.2338378036389));
#57900=CARTESIAN_POINT('Ctrl Pts',(-5.17498648254752,2.6667054605934,30.3730112610609));
#57901=CARTESIAN_POINT('Ctrl Pts',(-5.82000834206158,-0.138946055870331,
30.5121847184828));
#57902=CARTESIAN_POINT('Ctrl Pts',(-5.04183419409715,-2.9106203921743,30.6513581759048));
#57903=CARTESIAN_POINT('Ctrl Pts',(-3.03075488970033,-4.97054603707336,
30.7905316333267));
#57904=CARTESIAN_POINT('Ctrl Pts',(-0.27854979902338,-5.81499897829503,
30.9297050907487));
#57905=CARTESIAN_POINT('Ctrl Pts',(2.541770479563,-5.23748087703718,31.0688785481706));
#57906=CARTESIAN_POINT('Ctrl Pts',(4.74053879708136,-3.3792151487401,31.2080520055926));
#57907=CARTESIAN_POINT('Ctrl Pts',(5.78007924192746,-0.694612888699475,
31.3472254630146));
#57908=CARTESIAN_POINT('Ctrl Pts',(5.406187743632,2.15984656601141,31.4863989204365));
#57909=CARTESIAN_POINT('Ctrl Pts',(3.71029387691888,4.48614784141211,31.6255723778585));
#57910=CARTESIAN_POINT('Ctrl Pts',(1.10710312644696,5.71542874817974,31.7647458352804));
#57911=CARTESIAN_POINT('Ctrl Pts',(-1.76681313794548,5.5470870232665,31.9039192927023));
#57912=CARTESIAN_POINT('Ctrl Pts',(-4.20868167042801,4.02228811811282,32.0430927501244));
#57913=CARTESIAN_POINT('Ctrl Pts',(-5.62138003715451,1.51389880308725,32.1822662075462));
#57914=CARTESIAN_POINT('Ctrl Pts',(-5.65945397807416,-1.3646918253469,32.3214396649683));
#57915=CARTESIAN_POINT('Ctrl Pts',(-4.31359308029392,-3.9095674755334,32.4606131223902));
#57916=CARTESIAN_POINT('Ctrl Pts',(-1.9129075003232,-5.49841686336308,32.5997865798122));
#57917=CARTESIAN_POINT('Ctrl Pts',(0.955551003177575,-5.74271063074177,
32.7389600372341));
#57918=CARTESIAN_POINT('Ctrl Pts',(3.59034379818857,-4.58271039003308,32.8781334946561));
#57919=CARTESIAN_POINT('Ctrl Pts',(5.34717170745731,-2.30207685342522,33.017306952078));
#57920=CARTESIAN_POINT('Ctrl Pts',(5.79642873742743,0.541495152364058,33.1564804095));
#57921=CARTESIAN_POINT('Ctrl Pts',(4.82825579962227,3.25265261617684,33.2956538669219));
#57922=CARTESIAN_POINT('Ctrl Pts',(2.67940510789608,5.16842252296468,33.4348273243439));
#57923=CARTESIAN_POINT('Ctrl Pts',(-0.124654035064796,5.82033199050108,
33.5740007817657));
#57924=CARTESIAN_POINT('Ctrl Pts',(-2.89823089783061,5.048966307173,33.7131742391878));
#57925=CARTESIAN_POINT('Ctrl Pts',(-4.96308873476043,3.04295141581364,33.8523476966097));
#57926=CARTESIAN_POINT('Ctrl Pts',(-5.81429743977679,0.292828260100349,
33.9915211540317));
#57927=CARTESIAN_POINT('Ctrl Pts',(-5.24370665306742,-2.52890166765823,
34.1306946114536));
#57928=CARTESIAN_POINT('Ctrl Pts',(-3.39084581889107,-4.73222650985951,
34.2698680688756));
#57929=CARTESIAN_POINT('Ctrl Pts',(-0.708804346511129,-5.77835612492646,
34.4090415262975));
#57930=CARTESIAN_POINT('Ctrl Pts',(2.14656462932744,-5.4114751593469,34.5482149837194));
#57931=CARTESIAN_POINT('Ctrl Pts',(4.47702332485341,-3.72129886690476,34.6873884411414));
#57932=CARTESIAN_POINT('Ctrl Pts',(5.71269291582249,-1.12113458497172,34.8265618985634));
#57933=CARTESIAN_POINT('Ctrl Pts',(5.55140888200191,1.75318639423721,34.9657353559853));
#57934=CARTESIAN_POINT('Ctrl Pts',(4.0326108220164,4.19879185793537,35.1049088134072));
#57935=CARTESIAN_POINT('Ctrl Pts',(1.52769808928541,5.61764556163005,35.2440822708293));
#57936=CARTESIAN_POINT('Ctrl Pts',(-1.35079036593903,5.66278804966198,35.3832557282512));
#57937=CARTESIAN_POINT('Ctrl Pts',(-3.89896323693118,4.32318040164498,35.5224291856731));
#57938=CARTESIAN_POINT('Ctrl Pts',(-5.4937029535406,1.92640363537021,35.6616026430951));
#57939=CARTESIAN_POINT('Ctrl Pts',(-5.74503976585416,-0.941446332438793,
35.800776100517));
#57940=CARTESIAN_POINT('Ctrl Pts',(-4.59151301491858,-3.57907967806551,
35.939949557939));
#57941=CARTESIAN_POINT('Ctrl Pts',(-2.31520041780278,-5.34150261008211,
36.0791230153609));
#57942=CARTESIAN_POINT('Ctrl Pts',(0.527259819912814,-5.79774095578733,
36.2182964727829));
#57943=CARTESIAN_POINT('Ctrl Pts',(3.2407865533273,-4.83622845034032,36.3574699302048));
#57944=CARTESIAN_POINT('Ctrl Pts',(5.16182739794124,-2.69208859846242,36.4966433876268));
#57945=CARTESIAN_POINT('Ctrl Pts',(5.82062054250453,0.110361262598867,36.6358168450488));
#57946=CARTESIAN_POINT('Ctrl Pts',(5.05606797512593,2.88582392723711,36.7749903024707));
#57947=CARTESIAN_POINT('Ctrl Pts',(3.05512959301669,4.95560150516381,36.9141637598927));
#57948=CARTESIAN_POINT('Ctrl Pts',(0.307104955431337,5.81356084121064,37.0533372173146));
#57949=CARTESIAN_POINT('Ctrl Pts',(-2.51601760654839,5.24990080969599,37.1925106747365));
#57950=CARTESIAN_POINT('Ctrl Pts',(-4.72388568744661,3.40245604233844,37.3316841321585));
#57951=CARTESIAN_POINT('Ctrl Pts',(-5.77659816460266,0.722991530252853,
37.4708575895804));
#57952=CARTESIAN_POINT('Ctrl Pts',(-5.41672994402081,-2.13326974891985,
37.6100310470024));
#57953=CARTESIAN_POINT('Ctrl Pts',(-3.73228141756457,-4.46787181197159,
37.7492045044243));
#57954=CARTESIAN_POINT('Ctrl Pts',(-1.13515928308697,-5.70992263608972,
37.8883779618464));
#57955=CARTESIAN_POINT('Ctrl Pts',(1.73954907886489,-5.55569726589998,38.0275514192682));
#57956=CARTESIAN_POINT('Ctrl Pts',(4.18887672684745,-4.04290920939167,38.1667248766903));
#57957=CARTESIAN_POINT('Ctrl Pts',(5.61387721186295,-1.54148816350762,38.3058983341121));
#57958=CARTESIAN_POINT('Ctrl Pts',(5.6660879747992,1.33688076130373,38.4450717915342));
#57959=CARTESIAN_POINT('Ctrl Pts',(4.33274165434142,3.88833548769174,38.584245248956));
#57960=CARTESIAN_POINT('Ctrl Pts',(1.93988815425818,5.48895591684585,38.723418706378));
#57961=CARTESIAN_POINT('Ctrl Pts',(-0.927335984805442,5.74733425854047,
38.8625921638));
#57962=CARTESIAN_POINT('Ctrl Pts',(-3.56779397619399,4.60028795311144,39.0017656212219));
#57963=CARTESIAN_POINT('Ctrl Pts',(-5.33580130359836,2.32831002158779,39.1409390786439));
#57964=CARTESIAN_POINT('Ctrl Pts',(-5.79901821393447,-0.513021308099881,
39.2801125360658));
#57965=CARTESIAN_POINT('Ctrl Pts',(-4.84417193873862,-3.22890094862718,
39.4192859934878));
#57966=CARTESIAN_POINT('Ctrl Pts',(-2.70475585581123,-5.15520114724567,
39.5584594509097));
#57967=CARTESIAN_POINT('Ctrl Pts',(0.0960678246576714,-5.82087399633197,
39.6976329083317));
#57968=CARTESIAN_POINT('Ctrl Pts',(2.87339955520757,-5.06313915513303,39.8368063657536));
#57969=CARTESIAN_POINT('Ctrl Pts',(4.94808439343132,-3.06728934787535,39.9759798231756));
#57970=CARTESIAN_POINT('Ctrl Pts',(5.81278918703828,-0.32137979892819,40.1151532805975));
#57971=CARTESIAN_POINT('Ctrl Pts',(5.25606330957228,2.50311837392407,40.2543267380195));
#57972=CARTESIAN_POINT('Ctrl Pts',(3.41404574907282,4.71551638013761,40.3935001954414));
#57973=CARTESIAN_POINT('Ctrl Pts',(0.73717435437625,5.77480537155652,40.5326736528634));
#57974=CARTESIAN_POINT('Ctrl Pts',(-2.11996200495645,5.4219520659675,40.6718471102854));
#57975=CARTESIAN_POINT('Ctrl Pts',(-4.45869335795006,3.74324146267378,40.8110205677073));
#57976=CARTESIAN_POINT('Ctrl Pts',(-5.70711792568614,1.14917713622408,40.9501940251293));
#57977=CARTESIAN_POINT('Ctrl Pts',(-5.55995214910184,-1.72590127406118,
41.0893674825512));
#57978=CARTESIAN_POINT('Ctrl Pts',(-4.0531832181396,-4.17893633695223,41.2285409399732));
#57979=CARTESIAN_POINT('Ctrl Pts',(-1.55526894260013,-5.61007501057621,
41.3677143973951));
#57980=CARTESIAN_POINT('Ctrl Pts',(1.32296309531554,-5.66935373358739,41.506887854817));
#57981=CARTESIAN_POINT('Ctrl Pts',(3.87768429190016,-4.34227678072911,41.646061312239));
#57982=CARTESIAN_POINT('Ctrl Pts',(5.4841757819034,-1.95336097567572,41.7852347696609));
#57983=CARTESIAN_POINT('Ctrl Pts',(5.74959409496496,0.913220045362813,41.924408227083));
#57984=CARTESIAN_POINT('Ctrl Pts',(4.6090351516988,3.55648676062669,42.0635816845048));
#57985=CARTESIAN_POINT('Ctrl Pts',(2.34140558572941,5.33006782238494,42.2027551419269));
#57986=CARTESIAN_POINT('Ctrl Pts',(-0.49877970278341,5.80026050416698,42.3419285993487));
#57987=CARTESIAN_POINT('Ctrl Pts',(-3.21699587374662,4.85208621691798,42.4811020567708));
#57988=CARTESIAN_POINT('Ctrl Pts',(-5.14854381083423,2.717406803559,42.6202755141927));
#57989=CARTESIAN_POINT('Ctrl Pts',(-5.82109235045507,-0.0817738074305616,
42.7594489716147));
#57990=CARTESIAN_POINT('Ctrl Pts',(-5.07017980455513,-2.86095785666086,
42.8986224290365));
#57991=CARTESIAN_POINT('Ctrl Pts',(-3.07943060706636,-4.9405374448911,43.0377958864585));
#57992=CARTESIAN_POINT('Ctrl Pts',(-0.335652704513683,-5.81198248191277,
43.1769693438805));
#57993=CARTESIAN_POINT('Ctrl Pts',(2.49020404756757,-5.26219411553643,43.3161428013024));
#57994=CARTESIAN_POINT('Ctrl Pts',(4.70711863839939,-3.42561486920834,43.4553162587244));
#57995=CARTESIAN_POINT('Ctrl Pts',(5.7729777565986,-0.751352733358968,43.5944897161463));
#57996=CARTESIAN_POINT('Ctrl Pts',(5.42714149369761,2.10664147768288,43.7336631735683));
#57997=CARTESIAN_POINT('Ctrl Pts',(3.75417893614339,4.44948801813483,43.8728366309902));
#57998=CARTESIAN_POINT('Ctrl Pts',(1.16318805985547,5.70427880152416,44.0120100884122));
#57999=CARTESIAN_POINT('Ctrl Pts',(-1.71224306212229,5.56417350595057,44.1511835458341));
#58000=CARTESIAN_POINT('Ctrl Pts',(-4.16897074819021,4.06343278630797,44.2903570032561));
#58001=CARTESIAN_POINT('Ctrl Pts',(-5.6062389806971,1.56904034346491,44.429530460678));
#58002=CARTESIAN_POINT('Ctrl Pts',(-5.67258530633404,-1.30903745189791,
44.5687039181));
#58003=CARTESIAN_POINT('Ctrl Pts',(-4.35178572331137,-3.86700971378293,
44.707877375522));
#58004=CARTESIAN_POINT('Ctrl Pts',(-1.96682201838221,-5.47936257753721,
44.8470508329439));
#58005=CARTESIAN_POINT('Ctrl Pts',(0.899098599229094,-5.75181926150087,
44.9862242903659));
#58006=CARTESIAN_POINT('Ctrl Pts',(3.54515809954533,-4.61775455793575,45.1253977477878));
#58007=CARTESIAN_POINT('Ctrl Pts',(5.32430220101428,-2.35448703126236,45.2645712052098));
#58008=CARTESIAN_POINT('Ctrl Pts',(5.80146781899398,0.484535089839209,45.4037446626317));
#58009=CARTESIAN_POINT('Ctrl Pts',(4.85997123715588,3.20507140047233,45.5429181200536));
#58010=CARTESIAN_POINT('Ctrl Pts',(2.73004136542148,5.14185542885016,45.6820915774757));
#58011=CARTESIAN_POINT('Ctrl Pts',(-0.0674792971093948,5.82127560355717,
45.8212650348976));
#58012=CARTESIAN_POINT('Ctrl Pts',(-2.84849890661951,5.07718988093764,45.9604384923196));
#58013=CARTESIAN_POINT('Ctrl Pts',(-4.93296070505069,3.09155329737884,46.0996119497415));
#58014=CARTESIAN_POINT('Ctrl Pts',(-5.81114073069848,0.349923586123267,
46.2387854071635));
#58015=CARTESIAN_POINT('Ctrl Pts',(-5.26829319062015,-2.47727470535134,
46.3779588645854));
#58016=CARTESIAN_POINT('Ctrl Pts',(-3.43716333298409,-4.69869251286972,
46.5171323220073));
#58017=CARTESIAN_POINT('Ctrl Pts',(-0.765526581706437,-5.77111533074925,
46.6563057794293));
#58018=CARTESIAN_POINT('Ctrl Pts',(2.09330824742092,-5.43229819591927,46.7954792368513));
#58019=CARTESIAN_POINT('Ctrl Pts',(4.44025584803343,-3.76509377202123,46.9346526942732));
#58020=CARTESIAN_POINT('Ctrl Pts',(5.70140528072348,-1.17719196949634,47.0738261516952));
#58021=CARTESIAN_POINT('Ctrl Pts',(5.5683613109917,1.69857452540621,47.2129996091171));
#58022=CARTESIAN_POINT('Ctrl Pts',(4.07365785209267,4.15898002065313,47.3521730665391));
#58023=CARTESIAN_POINT('Ctrl Pts',(1.58280228306146,5.6023691453566,47.4913465239609));
#58024=CARTESIAN_POINT('Ctrl Pts',(-1.29510391502142,5.675782673553,47.630519981383));
#58025=CARTESIAN_POINT('Ctrl Pts',(-3.85631181770711,4.36126842474991,47.7696934388049));
#58026=CARTESIAN_POINT('Ctrl Pts',(-5.47451633277077,1.98027120120814,47.9088668962269));
#58027=CARTESIAN_POINT('Ctrl Pts',(-5.75400974473055,-0.884971731556399,
48.0480403536488));
#58028=CARTESIAN_POINT('Ctrl Pts',(-4.62644611924429,-3.53380806126163,
48.1872138110708));
#58029=CARTESIAN_POINT('Ctrl Pts',(-2.36755427930561,-5.31850447425306,
48.3263872684927));
#58030=CARTESIAN_POINT('Ctrl Pts',(0.47028755516223,-5.80264015113532,48.4655607259147));
#58031=CARTESIAN_POINT('Ctrl Pts',(3.19312760070882,-4.86782695190572,48.6047341833366));
#58032=CARTESIAN_POINT('Ctrl Pts',(5.13513604162437,-2.7426594652123,48.7439076407586));
#58033=CARTESIAN_POINT('Ctrl Pts',(5.82142375453324,0.0531843798899842,
48.8830810981805));
#58034=CARTESIAN_POINT('Ctrl Pts',(5.08416934200986,2.83602278021093,49.0222545556025));
#58035=CARTESIAN_POINT('Ctrl Pts',(3.10365734571302,4.92535421959779,49.1614280130244));
#58036=CARTESIAN_POINT('Ctrl Pts',(0.364192357703599,5.81026393847117,49.3006014704464));
#58037=CARTESIAN_POINT('Ctrl Pts',(-2.46433042523922,5.27436049804604,49.4397749278683));
#58038=CARTESIAN_POINT('Ctrl Pts',(-4.69023805435808,3.44869107076287,49.5789483852903));
#58039=CARTESIAN_POINT('Ctrl Pts',(-5.7692181052389,0.779695813950434,49.7181218427123));
#58040=CARTESIAN_POINT('Ctrl Pts',(-5.4374221415376,-2.07996239456987,49.8572953001342));
#58041=CARTESIAN_POINT('Ctrl Pts',(-3.77598590449091,-4.43099690331579,
49.9964687575561));
#58042=CARTESIAN_POINT('Ctrl Pts',(-1.19118878070317,-5.69849738061141,
50.1356422149781));
#58043=CARTESIAN_POINT('Ctrl Pts',(1.68489574633413,-5.5725155389728,50.2748156724));
#58044=CARTESIAN_POINT('Ctrl Pts',(4.14896421458505,-4.08385835383659,50.413989129822));
#58045=CARTESIAN_POINT('Ctrl Pts',(5.59846552788978,-1.59655467840533,50.553162587244));
#58046=CARTESIAN_POINT('Ctrl Pts',(5.67894581596416,1.28116256870522,50.6923360446659));
#58047=CARTESIAN_POINT('Ctrl Pts',(4.37072482786413,3.84559066818093,50.8315095020879));
#58048=CARTESIAN_POINT('Ctrl Pts',(1.99370844305515,5.46963707682683,50.9706829595098));
#58049=CARTESIAN_POINT('Ctrl Pts',(-0.870839527529374,5.75616553144545,
51.1098564169318));
#58050=CARTESIAN_POINT('Ctrl Pts',(-3.52243671421602,4.63510978321455,51.2490298743537));
#58051=CARTESIAN_POINT('Ctrl Pts',(-5.31267467706141,2.38060725106401,51.3882033317757));
#58052=CARTESIAN_POINT('Ctrl Pts',(-5.8037774935219,-0.456037184664693,
51.5273767891976));
#58053=CARTESIAN_POINT('Ctrl Pts',(-4.87565331379773,-3.18116454647687,
51.6665502466195));
#58054=CARTESIAN_POINT('Ctrl Pts',(-2.75526102684471,-5.12838568967457,
51.8057237040416));
#58055=CARTESIAN_POINT('Ctrl Pts',(0.038889141970282,-5.82153680248996,
51.9448971614634));
#58056=CARTESIAN_POINT('Ctrl Pts',(2.82352955266579,-5.09111814568579,52.0840706188855));
#58057=CARTESIAN_POINT('Ctrl Pts',(4.91771803439929,-3.11574267908185,52.2232440763073));
#58058=CARTESIAN_POINT('Ctrl Pts',(5.80935211051787,-0.378458933214385,
52.3624175337294));
#58059=CARTESIAN_POINT('Ctrl Pts',(5.28039600122842,2.45137128528485,52.5015909911512));
#58060=CARTESIAN_POINT('Ctrl Pts',(3.46019801303277,4.68175531384462,52.6407644485732));
#58061=CARTESIAN_POINT('Ctrl Pts',(0.793860344650892,5.76728609150777,52.7799379059952));
#58062=CARTESIAN_POINT('Ctrl Pts',(-2.06660399960485,5.44251329965536,52.9191113634171));
#58063=CARTESIAN_POINT('Ctrl Pts',(-4.42171123981307,3.78685526787318,53.0582848208391));
#58064=CARTESIAN_POINT('Ctrl Pts',(-5.69555511872252,1.2051784090756,53.197458278261));
#58065=CARTESIAN_POINT('Ctrl Pts',(-5.57663616484398,-1.67120680738872,
53.336631735683));
#58066=CARTESIAN_POINT('Ctrl Pts',(-4.09403423003101,-4.13892339038096,
53.475805193105));
#58067=CARTESIAN_POINT('Ctrl Pts',(-1.61029744656999,-5.59452815183536,
53.6149786505269));
#58068=CARTESIAN_POINT('Ctrl Pts',(1.26721349701524,-5.68207471449387,53.7541521079489));
#58069=CARTESIAN_POINT('Ctrl Pts',(3.83484632985259,-4.38015487563218,53.8933255653708));
#58070=CARTESIAN_POINT('Ctrl Pts',(5.46472483912719,-2.00713366289706,54.0324990227928));
#58071=CARTESIAN_POINT('Ctrl Pts',(5.75828660864619,0.856702072364817,54.1716724802147));
#58072=CARTESIAN_POINT('Ctrl Pts',(4.6437454976049,3.51104412697739,54.3108459376366));
#58073=CARTESIAN_POINT('Ctrl Pts',(2.39364586782849,5.30681284459288,54.4500193950587));
#58074=CARTESIAN_POINT('Ctrl Pts',(-0.441784064276092,5.80487983929558,
54.5891928524805));
#58075=CARTESIAN_POINT('Ctrl Pts',(-3.16918230991358,4.88345027563905,54.7283663099026));
#58076=CARTESIAN_POINT('Ctrl Pts',(-5.12160441370534,2.76784597433134,54.8675397673244));
#58077=CARTESIAN_POINT('Ctrl Pts',(-5.82161474674563,-0.0245936695504916,
55.0067132247464));
#58078=CARTESIAN_POINT('Ctrl Pts',(-5.09803625006422,-2.81101929931819,
55.1458866821684));
#58079=CARTESIAN_POINT('Ctrl Pts',(-3.12780922461082,-4.91005219550135,
55.2850601395903));
#58080=CARTESIAN_POINT('Ctrl Pts',(-0.392723226628261,-5.80840525233691,
55.4242335970124));
#58081=CARTESIAN_POINT('Ctrl Pts',(2.43839736363178,-5.28639966377323,55.5634070544342));
#58082=CARTESIAN_POINT('Ctrl Pts',(4.67324434248021,-3.47168409040697,55.7025805118563));
#58083=CARTESIAN_POINT('Ctrl Pts',(5.76531930120589,-0.808020088395763,
55.8417539692781));
#58084=CARTESIAN_POINT('Ctrl Pts',(5.44757163957287,2.05323314307691,55.9809274267001));
#58085=CARTESIAN_POINT('Ctrl Pts',(3.79770179662585,4.41239891351779,56.120100884122));
#58086=CARTESIAN_POINT('Ctrl Pts',(1.21916077025623,5.69257851279861,56.259274341544));
#58087=CARTESIAN_POINT('Ctrl Pts',(-1.6575077911142,5.58072316375789,56.3984477989659));
#58088=CARTESIAN_POINT('Ctrl Pts',(-4.128857608587,4.10418541931544,56.5376212563879));
#58089=CARTESIAN_POINT('Ctrl Pts',(-5.59055704093568,1.6240305046866,56.6767947138098));
#58090=CARTESIAN_POINT('Ctrl Pts',(-5.68516935027489,-1.2532567840643,56.8159681712319));
#58091=CARTESIAN_POINT('Ctrl Pts',(-4.38955851119091,-3.8240788675104,56.9551416286537));
#58092=CARTESIAN_POINT('Ctrl Pts',(-2.02054677977986,-5.45977964929258,
57.0943150860758));
#58093=CARTESIAN_POINT('Ctrl Pts',(0.842559451311496,-5.76037296354271,
57.2334885434976));
#58094=CARTESIAN_POINT('Ctrl Pts',(3.49963036824299,-4.65235321034202,57.3726620009197));
#58095=CARTESIAN_POINT('Ctrl Pts',(5.30091901219416,-2.40667005097636,57.5118354583415));
#58096=CARTESIAN_POINT('Ctrl Pts',(5.80594718180918,0.427528279942165,57.6510089157636));
#58097=CARTESIAN_POINT('Ctrl Pts',(4.89121779041446,3.15718096327107,57.7901823731854));
#58098=CARTESIAN_POINT('Ctrl Pts',(2.7804142317859,5.11479225460728,57.9293558306075));
#58099=CARTESIAN_POINT('Ctrl Pts',(-0.0102980488312426,5.82165758683027,
58.0685292880293));
#58100=CARTESIAN_POINT('Ctrl Pts',(-2.79849209560402,5.1049236134295,58.2077027454514));
#58101=CARTESIAN_POINT('Ctrl Pts',(-4.9023567491284,3.13985690953957,58.3468762028732));
#58102=CARTESIAN_POINT('Ctrl Pts',(-5.80742336963775,0.406985151932601,
58.4860496602953));
#58103=CARTESIAN_POINT('Ctrl Pts',(-5.29237144947885,-2.42540873851179,
58.6252231177171));
#58104=CARTESIAN_POINT('Ctrl Pts',(-3.4831492336253,-4.66470519158539,58.7643965751392));
#58105=CARTESIAN_POINT('Ctrl Pts',(-0.822174959802854,-5.76331774619284,
58.9035700325611));
#58106=CARTESIAN_POINT('Ctrl Pts',(2.03984990561131,-5.45259713078876,59.042743489983));
#58107=CARTESIAN_POINT('Ctrl Pts',(4.40305998058257,-3.80852542534511,59.181916947405));
#58108=CARTESIAN_POINT('Ctrl Pts',(5.68956758078844,-1.23313577993252,59.321090404827));
#58109=CARTESIAN_POINT('Ctrl Pts',(5.58477651107019,1.64379878011469,59.4602638622489));
#58110=CARTESIAN_POINT('Ctrl Pts',(4.11431186047907,4.11876692989892,59.5994373196709));
#58111=CARTESIAN_POINT('Ctrl Pts',(1.63775376994569,5.58655221913655,59.7386107770928));
#58112=CARTESIAN_POINT('Ctrl Pts',(-1.23929251400999,5.68822970464623,59.8777842345147));
#58113=CARTESIAN_POINT('Ctrl Pts',(-3.81328834608205,4.39893567783821,60.0169576919367));
#58114=CARTESIAN_POINT('Ctrl Pts',(-5.45480153714079,2.03394771282132,60.1561311493587));
#58115=CARTESIAN_POINT('Ctrl Pts',(-5.7624245835571,-0.828411749644193,
60.2953046067806));
#58116=CARTESIAN_POINT('Ctrl Pts',(-4.66093286951688,-3.48819550684506,
60.4344780642026));
#58117=CARTESIAN_POINT('Ctrl Pts',(-2.41967972198274,-5.29499321538886,
60.5736515216245));
#58118=CARTESIAN_POINT('Ctrl Pts',(0.413269917644382,-5.80697951465775,
60.7128249790465));
#58119=CARTESIAN_POINT('Ctrl Pts',(3.14516057887895,-4.89895581122554,60.8519984364683));
#58120=CARTESIAN_POINT('Ctrl Pts',(5.10794925353242,-2.79296572353979,60.9911718938905));
#58121=CARTESIAN_POINT('Ctrl Pts',(5.82166532233976,-0.00399763375499086,
61.1303453513122));
#58122=CARTESIAN_POINT('Ctrl Pts',(5.11178019453513,2.78594801661381,61.2695188087344));
#58123=CARTESIAN_POINT('Ctrl Pts',(3.15188566066619,4.8946317425585,61.4086922661561));
#58124=CARTESIAN_POINT('Ctrl Pts',(0.421244624209318,5.8064064666356,61.5478657235783));
#58125=CARTESIAN_POINT('Ctrl Pts',(-2.41240549035484,5.29831132566154,61.6870391810001));
#58126=CARTESIAN_POINT('Ctrl Pts',(-4.65613790853897,3.49459336706648,61.8262126384222));
#58127=CARTESIAN_POINT('Ctrl Pts',(-5.76128144655755,0.836324886168248,
61.965386095844));
#58128=CARTESIAN_POINT('Ctrl Pts',(-5.45758972735978,-2.02645439257844,
62.104559553266));
#58129=CARTESIAN_POINT('Ctrl Pts',(-3.81932611926446,-4.39369444921115,
62.2437330106879));
#58130=CARTESIAN_POINT('Ctrl Pts',(-1.24710329435501,-5.68652243467089,
62.3829064681099));
#58131=CARTESIAN_POINT('Ctrl Pts',(1.6300797410584,-5.58879599936766,62.5220799255319));
#58132=CARTESIAN_POINT('Ctrl Pts',(4.10865164137838,-4.12441384928666,62.6612533829538));
#58133=CARTESIAN_POINT('Ctrl Pts',(5.58251326942761,-1.65146646371945,62.8004268403757));
#58134=CARTESIAN_POINT('Ctrl Pts',(5.69125661949348,1.22531941397321,62.9396002977978));
#58135=CARTESIAN_POINT('Ctrl Pts',(4.40828464121373,3.80247747719103,63.0787737552196));
#58136=CARTESIAN_POINT('Ctrl Pts',(2.04733965326144,5.44978537141329,63.2179472126416));
#58137=CARTESIAN_POINT('Ctrl Pts',(-0.814265433823321,5.76445152192786,
63.3571206700635));
#58138=CARTESIAN_POINT('Ctrl Pts',(-3.47672716658331,4.66946479156297,63.4962941274855));
#58139=CARTESIAN_POINT('Ctrl Pts',(-5.28905976826099,2.43271310992216,63.6354675849074));
#58140=CARTESIAN_POINT('Ctrl Pts',(-5.80792939989083,-0.399083999576159,
63.7746410423294));
#58141=CARTESIAN_POINT('Ctrl Pts',(-4.90675767715171,-3.13297268635812,
63.9138144997514));
#58142=CARTESIAN_POINT('Ctrl Pts',(-2.80530899012875,-5.1013902832278,64.0529879571733));
#58143=CARTESIAN_POINT('Ctrl Pts',(-0.947612210060709,-5.58096655911489,
64.1457702621213));
#58144=CARTESIAN_POINT('Ctrl Pts',(-0.0175462161132968,-5.58388909905792,
64.1921614145953));
#58145=CARTESIAN_POINT('Ctrl Pts',(3.05041111877654,-4.27420965560366,-0.192161414595281));
#58146=CARTESIAN_POINT('Ctrl Pts',(3.76233375569806,-3.7661258454127,-0.145770262121297));
#58147=CARTESIAN_POINT('Ctrl Pts',(4.92665920277249,-2.38785367349441,-0.0529879571733284));
#58148=CARTESIAN_POINT('Ctrl Pts',(5.46823513289247,0.26517346728844,0.0861855002486236));
#58149=CARTESIAN_POINT('Ctrl Pts',(4.67268076690381,2.85263829294777,0.225358957670576));
#58150=CARTESIAN_POINT('Ctrl Pts',(2.73447316988989,4.74288662645417,0.364532415092528));
#58151=CARTESIAN_POINT('Ctrl Pts',(0.127600426951083,5.47315307622901,0.50370587251448));
#58152=CARTESIAN_POINT('Ctrl Pts',(-2.51047986399426,4.86513389280572,0.642879329936433));
#58153=CARTESIAN_POINT('Ctrl Pts',(-4.53465740262938,3.0673717525868,0.782052787358385));
#58154=CARTESIAN_POINT('Ctrl Pts',(-5.44995353740829,0.51955393007344,0.921226244780337));
#58155=CARTESIAN_POINT('Ctrl Pts',(-5.03254439112882,-2.15532545086806,
1.06039970220229));
#58156=CARTESIAN_POINT('Ctrl Pts',(-3.38450210013749,-4.30314585790824,
1.19957315962424));
#58157=CARTESIAN_POINT('Ctrl Pts',(-0.908830263630935,-5.39869955892152,
1.3387466170462));
#58158=CARTESIAN_POINT('Ctrl Pts',(1.78908233658119,-5.17408034133589,1.47792007446815));
#58159=CARTESIAN_POINT('Ctrl Pts',(4.04950164977306,-3.68421800789032,1.6170935318901));
#58160=CARTESIAN_POINT('Ctrl Pts',(5.3196758681094,-1.29343481442091,1.75626698931205));
#58161=CARTESIAN_POINT('Ctrl Pts',(5.28900291516093,1.41363829518363,1.895440446734));
#58162=CARTESIAN_POINT('Ctrl Pts',(3.9649833852255,3.77502741500648,2.03461390415595));
#58163=CARTESIAN_POINT('Ctrl Pts',(1.67138646397891,5.21328997302147,2.17378736157791));
#58164=CARTESIAN_POINT('Ctrl Pts',(-1.0309230246464,5.37672045824918,2.31296081899986));
#58165=CARTESIAN_POINT('Ctrl Pts',(-3.48113570323994,4.22535434344311,2.45213427642181));
#58166=CARTESIAN_POINT('Ctrl Pts',(-5.08008870302382,2.04074101801902,2.59130773384376));
#58167=CARTESIAN_POINT('Ctrl Pts',(-5.43678197806404,-0.642905010163819,
2.73048119126572));
#58168=CARTESIAN_POINT('Ctrl Pts',(-4.46399152227217,-3.16933823002763,
2.86965464868767));
#58169=CARTESIAN_POINT('Ctrl Pts',(-2.39959869431088,-4.92075718119219,
3.00882810610962));
#58170=CARTESIAN_POINT('Ctrl Pts',(0.251580110647388,-5.468878548288,3.14800156353158));
#58171=CARTESIAN_POINT('Ctrl Pts',(2.84123876169776,-4.67966744845125,3.28717502095352));
#58172=CARTESIAN_POINT('Ctrl Pts',(4.73611496153384,-2.74611365383239,3.42634847837548));
#58173=CARTESIAN_POINT('Ctrl Pts',(5.47284507153052,-0.141038830706225,
3.56552193579743));
#58174=CARTESIAN_POINT('Ctrl Pts',(4.87127276036557,2.49852492940865,3.70469539321938));
#58175=CARTESIAN_POINT('Ctrl Pts',(3.07850354080767,4.52711178103092,3.84386885064134));
#58176=CARTESIAN_POINT('Ctrl Pts',(0.532932316375539,5.44866114517237,3.98304230806329));
#58177=CARTESIAN_POINT('Ctrl Pts',(-2.14295953654073,5.03782190569276,4.12221576548524));
#58178=CARTESIAN_POINT('Ctrl Pts',(-4.29482268067486,3.3950586549128,4.26138922290719));
#58179=CARTESIAN_POINT('Ctrl Pts',(-5.39645116315218,0.922084579877679,
4.40056268032915));
#58180=CARTESIAN_POINT('Ctrl Pts',(-5.17845821236713,-1.77637149028642,
4.53973613775109));
#58181=CARTESIAN_POINT('Ctrl Pts',(-3.69415074456122,-4.04044247641186,
4.67890959517305));
#58182=CARTESIAN_POINT('Ctrl Pts',(-1.30649395460974,-5.316483675824,4.818083052595));
#58183=CARTESIAN_POINT('Ctrl Pts',(1.40064639459327,-5.29245829516381,4.95725651001695));
#58184=CARTESIAN_POINT('Ctrl Pts',(3.76527961330509,-3.97424138199533,5.0964299674389));
#58185=CARTESIAN_POINT('Ctrl Pts',(5.20917000868316,-1.68418316978025,5.23560342486086));
#58186=CARTESIAN_POINT('Ctrl Pts',(5.37923577651641,1.01771685128088,5.37477688228281));
#58187=CARTESIAN_POINT('Ctrl Pts',(4.23388987644961,3.47074943532844,5.51395033970476));
#58188=CARTESIAN_POINT('Ctrl Pts',(2.05320952080847,5.07506214665364,5.65312379712671));
#58189=CARTESIAN_POINT('Ctrl Pts',(-0.629552519391957,5.4383443026405,5.79229725454867));
#58190=CARTESIAN_POINT('Ctrl Pts',(-3.15836690532162,4.47176068457429,5.93147071197062));
#58191=CARTESIAN_POINT('Ctrl Pts',(-4.91484989486473,2.41167486193376,6.07064416939257));
#58192=CARTESIAN_POINT('Ctrl Pts',(-5.46947983942586,-0.238149983937169,
6.20981762681453));
#58193=CARTESIAN_POINT('Ctrl Pts',(-4.68663028001475,-2.82973881253801,
6.34899108423647));
#58194=CARTESIAN_POINT('Ctrl Pts',(-2.75773536963051,-4.72935733052854,
6.48816454165843));
#58195=CARTESIAN_POINT('Ctrl Pts',(-0.154477513857432,-5.47248223628434,
6.62733799908038));
#58196=CARTESIAN_POINT('Ctrl Pts',(2.48655550786828,-4.87739344681409,6.76651145650233));
#58197=CARTESIAN_POINT('Ctrl Pts',(4.51953856416763,-3.08961102660784,6.90568491392428));
#58198=CARTESIAN_POINT('Ctrl Pts',(5.44733604990991,-0.546310431977095,
7.04485837134624));
#58199=CARTESIAN_POINT('Ctrl Pts',(5.04306896426723,2.13058220925168,7.18403182876818));
#58200=CARTESIAN_POINT('Ctrl Pts',(3.40559477761184,4.2864728319958,7.32320528619014));
#58201=CARTESIAN_POINT('Ctrl Pts',(0.935333315454048,5.3941706237138,7.46237874361209));
#58202=CARTESIAN_POINT('Ctrl Pts',(-1.76364992199664,5.18280465398576,7.60155220103404));
#58203=CARTESIAN_POINT('Ctrl Pts',(-4.03135894469488,3.70406130993586,7.74072565845601));
#58204=CARTESIAN_POINT('Ctrl Pts',(-5.31325942252598,1.31954516318089,7.87989911587794));
#58205=CARTESIAN_POINT('Ctrl Pts',(-5.2958817632131,-1.38764602071352,8.01907257329991));
#58206=CARTESIAN_POINT('Ctrl Pts',(-3.98347541347518,-3.75550912114109,
8.15824603072185));
#58207=CARTESIAN_POINT('Ctrl Pts',(-1.6969697203782,-5.20501862598538,8.29741948814381));
#58208=CARTESIAN_POINT('Ctrl Pts',(1.00450454130311,-5.38171866184369,8.43659294556577));
#58209=CARTESIAN_POINT('Ctrl Pts',(3.46034223879862,-4.2423998773243,8.5757664029877));
#58210=CARTESIAN_POINT('Ctrl Pts',(5.07000498785365,-2.06566564377547,8.71493986040967));
#58211=CARTESIAN_POINT('Ctrl Pts',(5.43987383412996,0.616196232935,8.8541133178316));
#58212=CARTESIAN_POINT('Ctrl Pts',(4.47950288230013,3.14737653549747,8.99328677525359));
#58213=CARTESIAN_POINT('Ctrl Pts',(2.42373648721916,4.90891297226358,9.13246023267551));
#58214=CARTESIAN_POINT('Ctrl Pts',(-0.224718421185856,5.4700481496889,9.27163369009748));
#58215=CARTESIAN_POINT('Ctrl Pts',(-2.81822180013563,4.69356485136569,9.41080714751942));
#58216=CARTESIAN_POINT('Ctrl Pts',(-4.72257118163238,2.76934045634526,9.54998060494138));
#58217=CARTESIAN_POINT('Ctrl Pts',(-5.47208640212667,0.167915265522693,
9.68915406236333));
#58218=CARTESIAN_POINT('Ctrl Pts',(-4.88348472271888,-2.47457109247371,
9.82832751978529));
#58219=CARTESIAN_POINT('Ctrl Pts',(-3.10069988214165,-4.5119380946132,9.96750097720723));
#58220=CARTESIAN_POINT('Ctrl Pts',(-0.559685253342231,-5.44597810736753,
10.1066744346292));
#58221=CARTESIAN_POINT('Ctrl Pts',(2.11819203461263,-5.04828561327891,10.2458478920511));
#58222=CARTESIAN_POINT('Ctrl Pts',(4.27809713600777,-3.41611036467168,10.3850213494731));
#58223=CARTESIAN_POINT('Ctrl Pts',(5.39185755758026,-0.94857641099696,10.524194806895));
#58224=CARTESIAN_POINT('Ctrl Pts',(5.18711984344,1.75091771894802,10.663368264317));
#58225=CARTESIAN_POINT('Ctrl Pts',(3.71394953992634,4.02225110399837,10.8025417217389));
#58226=CARTESIAN_POINT('Ctrl Pts',(1.3325884149323,5.31000313042501,10.9417151791609));
#58227=CARTESIAN_POINT('Ctrl Pts',(-1.37463727936781,5.29927329724628,11.0808886365828));
#58228=CARTESIAN_POINT('Ctrl Pts',(-3.74571598336408,3.9926854247118,11.2200620940048));
#58229=CARTESIAN_POINT('Ctrl Pts',(-5.20083585717358,1.70974603829712,11.3592355514267));
#58230=CARTESIAN_POINT('Ctrl Pts',(-5.38416909556079,-0.991286174191518,
11.4984090088487));
#58231=CARTESIAN_POINT('Ctrl Pts',(-4.25088429664866,-3.44991417650368,
11.6375824662706));
#58232=CARTESIAN_POINT('Ctrl Pts',(-2.07810931083753,-5.06491725706803,
11.7767559236926));
#58233=CARTESIAN_POINT('Ctrl Pts',(0.6028362308323,-5.44137056333522,11.9159293811146));
#58234=CARTESIAN_POINT('Ctrl Pts',(3.13636718708249,-4.48721806875122,12.0551028385365));
#58235=CARTESIAN_POINT('Ctrl Pts',(4.90294644905707,-2.43578349744261,12.1942762959585));
#58236=CARTESIAN_POINT('Ctrl Pts',(5.47058347571745,0.211285503388863,12.3334497533804));
#58237=CARTESIAN_POINT('Ctrl Pts',(4.70047112065431,2.80668779393611,12.4726232108024));
#58238=CARTESIAN_POINT('Ctrl Pts',(2.78092884401596,4.71575655576655,12.6117966682243));
#58239=CARTESIAN_POINT('Ctrl Pts',(0.181352004663688,5.47165757144393,12.7509701256463));
#58240=CARTESIAN_POINT('Ctrl Pts',(-2.46257175548597,4.88954655134992,12.8901435830682));
#58241=CARTESIAN_POINT('Ctrl Pts',(-4.50431041820064,3.11177004054354,13.0293170404902));
#58242=CARTESIAN_POINT('Ctrl Pts',(-5.44458732573234,0.57305669982123,13.1684904979121));
#58243=CARTESIAN_POINT('Ctrl Pts',(-5.05347182127219,-2.10578908733594,
13.3076639553341));
#58244=CARTESIAN_POINT('Ctrl Pts',(-3.4266053526834,-4.26969564321588,13.446837412756));
#58245=CARTESIAN_POINT('Ctrl Pts',(-0.961813786651197,-5.38951197869926,
13.586010870178));
#58246=CARTESIAN_POINT('Ctrl Pts',(1.73817495791542,-5.19140375470941,13.7251843276));
#58247=CARTESIAN_POINT('Ctrl Pts',(4.01311900924231,-3.72381537490692,13.8643577850219));
#58248=CARTESIAN_POINT('Ctrl Pts',(5.30671481915647,-1.34562363121355,14.0035312424439));
#58249=CARTESIAN_POINT('Ctrl Pts',(5.30263287681247,1.36162024899849,14.1427046998658));
#58250=CARTESIAN_POINT('Ctrl Pts',(4.00187136016905,3.73590025902645,14.2818781572877));
#58251=CARTESIAN_POINT('Ctrl Pts',(1.7225120464961,5.19662172746978,14.4210516147097));
#58252=CARTESIAN_POINT('Ctrl Pts',(-0.97806182965262,5.38658706289165,14.5602250721317));
#58253=CARTESIAN_POINT('Ctrl Pts',(-3.43946531132461,4.25934308326177,14.6993985295536));
#58254=CARTESIAN_POINT('Ctrl Pts',(-5.05979898497569,2.09054044695961,14.8385719869756));
#58255=CARTESIAN_POINT('Ctrl Pts',(-5.44283448123103,-0.589472593644336,
14.9777454443975));
#58256=CARTESIAN_POINT('Ctrl Pts',(-4.49490619740522,-3.12533892646274,
15.1169189018195));
#58257=CARTESIAN_POINT('Ctrl Pts',(-2.44781581996098,-4.89695036122319,
15.2560923592414));
#58258=CARTESIAN_POINT('Ctrl Pts',(0.197851311546307,-5.47108581428354,
15.3952658166634));
#58259=CARTESIAN_POINT('Ctrl Pts',(2.79513686348917,-4.70734904623601,15.5344392740853));
#58260=CARTESIAN_POINT('Ctrl Pts',(4.70891349402307,-2.79250046276497,15.6736127315073));
#58261=CARTESIAN_POINT('Ctrl Pts',(5.47119574682194,-0.194787650257265,
15.8127861889292));
#58262=CARTESIAN_POINT('Ctrl Pts',(4.89557889615458,2.45055756926072,15.9519596463512));
#58263=CARTESIAN_POINT('Ctrl Pts',(3.12282143506075,4.49665558092459,16.0911331037731));
#58264=CARTESIAN_POINT('Ctrl Pts',(0.586424690784659,5.44316371339071,16.2303065611951));
#58265=CARTESIAN_POINT('Ctrl Pts',(-2.09337344221106,5.05862755697437,16.369480018617));
#58266=CARTESIAN_POINT('Ctrl Pts',(-4.26126840428094,3.43707967836246,16.508653476039));
#58267=CARTESIAN_POINT('Ctrl Pts',(-5.38713390121461,0.975045362595692,
16.6478269334609));
#58268=CARTESIAN_POINT('Ctrl Pts',(-5.19565636196209,-1.72542171573735,
16.7870003908829));
#58269=CARTESIAN_POINT('Ctrl Pts',(-3.73365875538693,-4.00396271549296,
16.9261738483048));
#58270=CARTESIAN_POINT('Ctrl Pts',(-1.35865073342267,-5.30339450854876,
17.0653473057268));
#58271=CARTESIAN_POINT('Ctrl Pts',(1.34859500809782,-5.30596048165352,17.2045207631488));
#58272=CARTESIAN_POINT('Ctrl Pts',(3.72606200731666,-4.01103316445607,17.3436942205707));
#58273=CARTESIAN_POINT('Ctrl Pts',(5.192376262285,-1.7352676679966,17.4828676779927));
#58274=CARTESIAN_POINT('Ctrl Pts',(5.38897254925603,0.964831587428646,17.6220411354146));
#58275=CARTESIAN_POINT('Ctrl Pts',(4.26777618615752,3.42899570626765,17.7612145928366));
#58276=CARTESIAN_POINT('Ctrl Pts',(2.10295897718242,5.05465020243964,17.9003880502585));
#58277=CARTESIAN_POINT('Ctrl Pts',(-0.576105401953414,5.44426557899,18.0395615076805));
#58278=CARTESIAN_POINT('Ctrl Pts',(-3.11429182013832,4.50256722190293,18.1787349651024));
#58279=CARTESIAN_POINT('Ctrl Pts',(-4.89092474491816,2.4598333822197,18.3179084225244));
#58280=CARTESIAN_POINT('Ctrl Pts',(-5.47155516235805,-0.184415926665981,
18.4570818799463));
#58281=CARTESIAN_POINT('Ctrl Pts',(-4.7141985866371,-2.78356907844658,18.5962553373683));
#58282=CARTESIAN_POINT('Ctrl Pts',(-2.80405524281576,-4.7020420376654,18.7354287947902));
#58283=CARTESIAN_POINT('Ctrl Pts',(-0.208222121286857,-5.47070093104549,
18.8746022522122));
#58284=CARTESIAN_POINT('Ctrl Pts',(2.43852860624314,-4.90158172075801,19.0137757096341));
#58285=CARTESIAN_POINT('Ctrl Pts',(4.48897362894353,-3.13385399905368,19.1529491670561));
#58286=CARTESIAN_POINT('Ctrl Pts',(5.44170727892698,-0.599789145623911,
19.2921226244781));
#58287=CARTESIAN_POINT('Ctrl Pts',(5.06375278929654,2.08094517410398,19.4312960819));
#58288=CARTESIAN_POINT('Ctrl Pts',(3.44753327854899,4.25281547001894,19.5704695393219));
#58289=CARTESIAN_POINT('Ctrl Pts',(0.988271059044424,5.38472333946605,19.7096429967439));
#58290=CARTESIAN_POINT('Ctrl Pts',(-1.71265806931551,5.19987763955496,19.8488164541658));
#58291=CARTESIAN_POINT('Ctrl Pts',(-3.99478227796254,3.74347962201099,19.9879899115878));
#58292=CARTESIAN_POINT('Ctrl Pts',(-5.3000422186233,1.37166964300655,20.1271633690097));
#58293=CARTESIAN_POINT('Ctrl Pts',(-5.30925609170404,-1.33556163520771,
20.2663368264317));
#58294=CARTESIAN_POINT('Ctrl Pts',(-4.02017078232737,-3.71620128755917,
20.4055102838536));
#58295=CARTESIAN_POINT('Ctrl Pts',(-1.74801282588246,-5.18809948721934,
20.5446837412756));
#58296=CARTESIAN_POINT('Ctrl Pts',(0.951595527297795,-5.39132554026949,
20.6838571986976));
#58297=CARTESIAN_POINT('Ctrl Pts',(3.41850542446435,-4.27618355448442,20.8230306561195));
#58298=CARTESIAN_POINT('Ctrl Pts',(5.0494709405069,-2.11536482662247,20.9622041135415));
#58299=CARTESIAN_POINT('Ctrl Pts',(5.44566384798265,0.562734736363337,21.1013775709634));
#58300=CARTESIAN_POINT('Ctrl Pts',(4.5102010960486,3.10322593472296,21.2405510283854));
#58301=CARTESIAN_POINT('Ctrl Pts',(2.47183611175321,4.88486963647629,21.3797244858073));
#58302=CARTESIAN_POINT('Ctrl Pts',(-0.170979429762869,5.47199151711085,
21.5188979432293));
#58303=CARTESIAN_POINT('Ctrl Pts',(-2.77198450856176,4.72101970055504,21.6580714006512));
#58304=CARTESIAN_POINT('Ctrl Pts',(-4.69514222812823,2.81559311449334,21.7972448580732));
#58305=CARTESIAN_POINT('Ctrl Pts',(-5.47017312709831,0.221655336742991,
21.9364183154951));
#58306=CARTESIAN_POINT('Ctrl Pts',(-4.90755498896332,-2.42648493896755,
22.0755917729171));
#58307=CARTESIAN_POINT('Ctrl Pts',(-3.14486766599629,-4.48126460857939,
22.214765230339));
#58308=CARTESIAN_POINT('Ctrl Pts',(-0.613149983751713,-5.44021803112342,
22.353938687761));
#58309=CARTESIAN_POINT('Ctrl Pts',(2.0685043579568,-5.06884748733368,22.4931121451829));
#58310=CARTESIAN_POINT('Ctrl Pts',(4.24433689140084,-3.45796609020809,22.6322856026049));
#58311=CARTESIAN_POINT('Ctrl Pts',(5.38228030798918,-1.00149079624683,22.7714590600268));
#58312=CARTESIAN_POINT('Ctrl Pts',(5.20406756203382,1.69988409561432,22.9106325174488));
#58313=CARTESIAN_POINT('Ctrl Pts',(3.75327791555961,3.98557775200882,23.0498059748707));
#58314=CARTESIAN_POINT('Ctrl Pts',(1.38468028146157,5.29665796959428,23.1889794322927));
#58315=CARTESIAN_POINT('Ctrl Pts',(-1.322520208919,5.31251968709162,23.3281528897146));
#58316=CARTESIAN_POINT('Ctrl Pts',(-3.70631815921382,4.02928415868341,23.4673263471366));
#58317=CARTESIAN_POINT('Ctrl Pts',(-5.1837914280616,1.76074744330078,23.6064998045585));
#58318=CARTESIAN_POINT('Ctrl Pts',(-5.39364602174355,-0.938353729072977,
23.7456732619805));
#58319=CARTESIAN_POINT('Ctrl Pts',(-4.28456513754638,-3.40799452917068,
23.8848467194025));
#58320=CARTESIAN_POINT('Ctrl Pts',(-2.12775792047298,-5.04426123040824,
24.0240201768244));
#58321=CARTESIAN_POINT('Ctrl Pts',(0.549360677498777,-5.44702927977749,
24.1631936342464));
#58322=CARTESIAN_POINT('Ctrl Pts',(3.09214133694363,-4.51780777381018,24.3023670916683));
#58323=CARTESIAN_POINT('Ctrl Pts',(4.87878507240969,-2.4838239361854,24.4415405490903));
#58324=CARTESIAN_POINT('Ctrl Pts',(5.47239487591072,0.157541901858669,24.5807140065122));
#58325=CARTESIAN_POINT('Ctrl Pts',(4.7278123468587,2.76038322368935,24.7198874639342));
#58326=CARTESIAN_POINT('Ctrl Pts',(2.82711400822466,4.6882141070172,24.8590609213561));
#58327=CARTESIAN_POINT('Ctrl Pts',(0.235087215623762,5.46961233816304,24.9982343787781));
#58328=CARTESIAN_POINT('Ctrl Pts',(-2.41442664005693,4.91349866475189,25.1374078362));
#58329=CARTESIAN_POINT('Ctrl Pts',(-4.47352856631735,3.15586236947649,25.276581293622));
#58330=CARTESIAN_POINT('Ctrl Pts',(-5.43869597896016,0.626507124602579,
25.4157547510439));
#58331=CARTESIAN_POINT('Ctrl Pts',(-5.07391162036489,-2.05605106878728,
25.5549282084659));
#58332=CARTESIAN_POINT('Ctrl Pts',(-3.4683780504302,-4.23583271955223,25.6941016658878));
#58333=CARTESIAN_POINT('Ctrl Pts',(-1.01470449448827,-5.37980482151541,
25.8332751233098));
#58334=CARTESIAN_POINT('Ctrl Pts',(1.68709987166048,-5.20822610413357,25.9724485807317));
#58335=CARTESIAN_POINT('Ctrl Pts',(3.97634919313482,-3.76305357694934,26.1116220381537));
#58336=CARTESIAN_POINT('Ctrl Pts',(5.29324178186864,-1.39768257033394,26.2507954955757));
#58337=CARTESIAN_POINT('Ctrl Pts',(5.31575124813685,1.30947080787112,26.3899689529976));
#58338=CARTESIAN_POINT('Ctrl Pts',(4.03837323857078,3.69641268187557,26.5291424104196));
#58339=CARTESIAN_POINT('Ctrl Pts',(1.77347144346219,5.17945211078925,26.6683158678415));
#58340=CARTESIAN_POINT('Ctrl Pts',(-0.925106272601936,5.3959339796858,26.8074893252635));
#58341=CARTESIAN_POINT('Ctrl Pts',(-3.39746308376715,4.29292088480261,26.9466627826854));
#58342=CARTESIAN_POINT('Ctrl Pts',(-5.03902110355814,2.14013818400377,27.0858362401074));
#58343=CARTESIAN_POINT('Ctrl Pts',(-5.44836186614097,-0.535983306005068,
27.2250096975293));
#58344=CARTESIAN_POINT('Ctrl Pts',(-4.52538720931959,-3.08103809364017,
27.3641831549512));
#58345=CARTESIAN_POINT('Ctrl Pts',(-2.49579678323004,-4.87267108940813,
27.5033566123732));
#58346=CARTESIAN_POINT('Ctrl Pts',(0.144103423981289,-5.47276523632542,
27.6425300697952));
#58347=CARTESIAN_POINT('Ctrl Pts',(2.74876529378475,-4.73457648458863,27.7817035272171));
#58348=CARTESIAN_POINT('Ctrl Pts',(4.68125771610869,-2.83861785453907,27.9208769846391));
#58349=CARTESIAN_POINT('Ctrl Pts',(5.46901856762123,-0.248517676935322,
28.060050442061));
#58350=CARTESIAN_POINT('Ctrl Pts',(4.91941271228352,2.40235378222246,28.199223899483));
#58351=CARTESIAN_POINT('Ctrl Pts',(3.16683804319653,4.46576554880552,28.3383973569049));
#58352=CARTESIAN_POINT('Ctrl Pts',(0.639860487633334,5.43714113161511,28.4775708143269));
#58353=CARTESIAN_POINT('Ctrl Pts',(-2.04358538168839,5.07894515785361,28.6167442717489));
#58354=CARTESIAN_POINT('Ctrl Pts',(-4.227303005753,3.4787690964315,28.7559177291708));
#58355=CARTESIAN_POINT('Ctrl Pts',(-5.37729689497187,1.02791207409051,28.8950911865928));
#58356=CARTESIAN_POINT('Ctrl Pts',(-5.21235324077832,-1.67430547454247,
29.0342646440147));
#58357=CARTESIAN_POINT('Ctrl Pts',(-3.77280654723323,-3.96709665698849,
29.1734381014367));
#58358=CARTESIAN_POINT('Ctrl Pts',(-1.41067643122025,-5.28979367604586,
29.3126115588586));
#58359=CARTESIAN_POINT('Ctrl Pts',(1.29641351075158,-5.31895075535353,29.4517850162806));
#58360=CARTESIAN_POINT('Ctrl Pts',(3.68648491527416,-4.04743796718259,29.5909584737025));
#58361=CARTESIAN_POINT('Ctrl Pts',(5.17508156156827,-1.78618474964133,29.7301319311244));
#58362=CARTESIAN_POINT('Ctrl Pts',(5.39818940029989,0.911853237766431,29.8693053885464));
#58363=CARTESIAN_POINT('Ctrl Pts',(4.30125074586824,3.38691115175804,30.0084788459683));
#58364=CARTESIAN_POINT('Ctrl Pts',(2.15250554256233,5.03375059155434,30.1476523033903));
#58365=CARTESIAN_POINT('Ctrl Pts',(-0.522602702547216,5.44966159903764,
30.2868257608122));
#58366=CARTESIAN_POINT('Ctrl Pts',(-3.06991627176472,4.53293935687313,30.4259992182342));
#58367=CARTESIAN_POINT('Ctrl Pts',(-4.86652772433872,2.50775458069123,30.5651726756561));
#58368=CARTESIAN_POINT('Ctrl Pts',(-5.47310259612169,-0.130664077164341,
30.7043461330782));
#58369=CARTESIAN_POINT('Ctrl Pts',(-4.74131207295726,-2.73713078890376,
30.8435195905001));
#58370=CARTESIAN_POINT('Ctrl Pts',(-2.85010458406871,-4.67427309734954,
30.982693047922));
#58371=CARTESIAN_POINT('Ctrl Pts',(-0.261946639692367,-5.4683918190533,
31.121866505344));
#58372=CARTESIAN_POINT('Ctrl Pts',(2.39026643826314,-4.92529709589665,31.2610399627659));
#58373=CARTESIAN_POINT('Ctrl Pts',(4.45797560285469,-3.17779462097341,31.4002134201879));
#58374=CARTESIAN_POINT('Ctrl Pts',(5.43555349846396,-0.653209992323582,
31.5393868776099));
#58375=CARTESIAN_POINT('Ctrl Pts',(5.08394806944776,2.03110737182789,31.6785603350317));
#58376=CARTESIAN_POINT('Ctrl Pts',(3.48913916555426,4.21874780143712,31.8177337924538));
#58377=CARTESIAN_POINT('Ctrl Pts',(1.04111345541225,5.37475654348126,31.9569072498757));
#58378=CARTESIAN_POINT('Ctrl Pts',(-1.66150098141019,5.21644894708155,32.0960807072976));
#58379=CARTESIAN_POINT('Ctrl Pts',(-3.95782019936239,3.78253676760111,32.2352541647196));
#58380=CARTESIAN_POINT('Ctrl Pts',(-5.28631367291798,1.42366178576779,32.3744276221416));
#58381=CARTESIAN_POINT('Ctrl Pts',(-5.3221181894487,-1.28334839629558,32.5136010795635));
#58382=CARTESIAN_POINT('Ctrl Pts',(-4.05647828985874,-3.67653491927384,
32.6527745369854));
#58383=CARTESIAN_POINT('Ctrl Pts',(-1.79888728517725,-5.17067980675295,
32.7919479944074));
#58384=CARTESIAN_POINT('Ctrl Pts',(0.898594704481963,-5.4004122699857,32.9311214518293));
#58385=CARTESIAN_POINT('Ctrl Pts',(3.37633879677125,-4.30955467051439,33.0702949092513));
#58386=CARTESIAN_POINT('Ctrl Pts',(5.02844972617794,-2.16485992157371,33.2094683666733));
#58387=CARTESIAN_POINT('Ctrl Pts',(5.45092847063015,0.509218947810083,33.3486418240952));
#58388=CARTESIAN_POINT('Ctrl Pts',(4.54046417093141,3.05877593838176,33.4878152815172));
#58389=CARTESIAN_POINT('Ctrl Pts',(2.51969725646367,4.86035501424583,33.6269887389391));
#58390=CARTESIAN_POINT('Ctrl Pts',(-0.117223942446786,5.47340695326525,
33.766162196361));
#58391=CARTESIAN_POINT('Ctrl Pts',(-2.7254797792021,4.7480190713492,33.9053356537831));
#58392=CARTESIAN_POINT('Ctrl Pts',(-4.66726029285681,2.86157412754891,34.0445091112049));
#58393=CARTESIAN_POINT('Ctrl Pts',(-5.46773209623851,0.275374022918645,
34.183682568627));
#58394=CARTESIAN_POINT('Ctrl Pts',(-4.93115178010865,-2.3781646810653,34.3228560260488));
#58395=CARTESIAN_POINT('Ctrl Pts',(-3.18873203673927,-4.450158775438,34.4620294834708));
#58396=CARTESIAN_POINT('Ctrl Pts',(-0.666555558176188,-5.4339330890801,
34.6012029408928));
#58397=CARTESIAN_POINT('Ctrl Pts',(2.01861711444781,-5.0889203249799,34.7403763983148));
#58398=CARTESIAN_POINT('Ctrl Pts',(4.21016715819219,-3.49948819526728,34.8795498557366));
#58399=CARTESIAN_POINT('Ctrl Pts',(5.37218378236186,-1.05430855884951,35.0187233131587));
#58400=CARTESIAN_POINT('Ctrl Pts',(5.22051319834627,1.64868646947428,35.1578967705805));
#58401=CARTESIAN_POINT('Ctrl Pts',(3.79224417938013,3.94851987619319,35.2970702280026));
#58402=CARTESIAN_POINT('Ctrl Pts',(1.43663855567549,5.28280179346924,35.4362436854244));
#58403=CARTESIAN_POINT('Ctrl Pts',(-1.27027554328518,5.32525353132287,35.5754171428465));
#58404=CARTESIAN_POINT('Ctrl Pts',(-3.66656275387258,4.06549415208649,35.7145906002684));
#58405=CARTESIAN_POINT('Ctrl Pts',(-5.16624687288569,1.81157897347425,35.8537640576904));
#58406=CARTESIAN_POINT('Ctrl Pts',(-5.40260257533944,-0.885330752696877,
35.9929375151123));
#58407=CARTESIAN_POINT('Ctrl Pts',(-4.31783260866877,-3.3657460825576,36.1321109725343));
#58408=CARTESIAN_POINT('Ctrl Pts',(-2.17720124654159,-5.02311853939292,
36.2712844299562));
#58409=CARTESIAN_POINT('Ctrl Pts',(0.495832122497053,-5.45216247327932,
36.4104578873782));
#58410=CARTESIAN_POINT('Ctrl Pts',(3.04761716066692,-4.54796160612022,36.5496313448001));
#58411=CARTESIAN_POINT('Ctrl Pts',(4.85415299635065,-2.53162473853356,36.6888048022221));
#58412=CARTESIAN_POINT('Ctrl Pts',(5.47367830592085,0.103783100872094,36.827978259644));
#58413=CARTESIAN_POINT('Ctrl Pts',(4.75469743932145,2.71381233493496,36.967151717066));
#58414=CARTESIAN_POINT('Ctrl Pts',(2.87302641581874,4.66021934491746,37.1063251744879));
#58415=CARTESIAN_POINT('Ctrl Pts',(0.288799745647482,5.46703940315497,37.2454986319099));
#58416=CARTESIAN_POINT('Ctrl Pts',(-2.36604858360213,4.93697672961596,37.3846720893318));
#58417=CARTESIAN_POINT('Ctrl Pts',(-4.44231511369065,3.19965022454186,37.5238455467538));
#58418=CARTESIAN_POINT('Ctrl Pts',(-5.43227991323453,0.679897104717855,
37.6630190041757));
#58419=CARTESIAN_POINT('Ctrl Pts',(-5.09386189446753,-2.00611468486398,
37.8021924615977));
#58420=CARTESIAN_POINT('Ctrl Pts',(-3.50981612316625,-4.20156112775922,
37.9413659190196));
#58421=CARTESIAN_POINT('Ctrl Pts',(-1.06749730483629,-5.36957862712731,
38.0805393764416));
#58422=CARTESIAN_POINT('Ctrl Pts',(1.6358620160059,-5.22454597006517,38.2197128338635));
#58423=CARTESIAN_POINT('Ctrl Pts',(3.93919574356163,-3.80192872403483,38.3588862912855));
#58424=CARTESIAN_POINT('Ctrl Pts',(5.27925805887621,-1.44960666269362,38.4980597487074));
#58425=CARTESIAN_POINT('Ctrl Pts',(5.32835676206999,1.25719503054944,38.6372332061295));
#58426=CARTESIAN_POINT('Ctrl Pts',(4.07448549950035,3.6565684792024,38.7764066635512));
#58427=CARTESIAN_POINT('Ctrl Pts',(1.82425973800165,5.16178278669699,38.9155801209734));
#58428=CARTESIAN_POINT('Ctrl Pts',(-0.872061462392577,5.40476030315358,
39.0547535783952));
#58429=CARTESIAN_POINT('Ctrl Pts',(-3.35513307299098,4.32608451041554,39.1939270358173));
#58430=CARTESIAN_POINT('Ctrl Pts',(-5.01775706334624,2.18952944304799,39.3331004932391));
#58431=CARTESIAN_POINT('Ctrl Pts',(-5.45336359954413,-0.482442307330456,
39.4722739506611));
#58432=CARTESIAN_POINT('Ctrl Pts',(-4.55543161723014,-3.03644000590743,
39.611447408083));
#58433=CARTESIAN_POINT('Ctrl Pts',(-2.54353695497842,-4.84792170805123,
39.750620865505));
#58434=CARTESIAN_POINT('Ctrl Pts',(0.0903416334882624,-5.47391665245223,
39.8897943229269));
#58435=CARTESIAN_POINT('Ctrl Pts',(2.70212852645677,-4.76134713660365,40.028967780349));
#58436=CARTESIAN_POINT('Ctrl Pts',(4.65315029598825,-2.88446137982113,40.1681412377708));
#58437=CARTESIAN_POINT('Ctrl Pts',(5.46631374397962,-0.302223726922086,
40.3073146951928));
#58438=CARTESIAN_POINT('Ctrl Pts',(4.94277190929426,2.35391821893342,40.4464881526148));
#58439=CARTESIAN_POINT('Ctrl Pts',(3.21054911854478,4.43444466490975,40.5856616100367));
#58440=CARTESIAN_POINT('Ctrl Pts',(0.693234551499346,5.43059398089589,40.7248350674587));
#58441=CARTESIAN_POINT('Ctrl Pts',(-1.99360015846576,5.09877274811306,40.8640085248806));
#58442=CARTESIAN_POINT('Ctrl Pts',(-4.19292976203238,3.52012288697402,41.0031819823026));
#58443=CARTESIAN_POINT('Ctrl Pts',(-5.36694109348664,1.08067961384472,41.1423554397246));
#58444=CARTESIAN_POINT('Ctrl Pts',(-5.22854723792075,-1.62302769833616,
41.2815288971464));
#58445=CARTESIAN_POINT('Ctrl Pts',(-3.81159034316765,-3.92984785769199,
41.4207023545685));
#58446=CARTESIAN_POINT('Ctrl Pts',(-1.46256602862488,-5.27568249050751,
41.5598758119903));
#58447=CARTESIAN_POINT('Ctrl Pts',(1.24410693696348,-5.33142786297766,41.6990492694124));
#58448=CARTESIAN_POINT('Ctrl Pts',(3.64655215552852,-4.08345227788271,41.8382227268343));
#58449=CARTESIAN_POINT('Ctrl Pts',(5.15728757510524,-1.83692950229468,41.9773961842562));
#58450=CARTESIAN_POINT('Ctrl Pts',(5.40688544041709,0.858786913582771,42.1165696416783));
#58451=CARTESIAN_POINT('Ctrl Pts',(4.3343103259958,3.34449983206777,42.2557430991001));
#58452=CARTESIAN_POINT('Ctrl Pts',(2.20184443675396,5.01236533036757,42.3949165565222));
#58453=CARTESIAN_POINT('Ctrl Pts',(-0.469049583050801,5.45453184218179,
42.534090013944));
#58454=CARTESIAN_POINT('Ctrl Pts',(-3.02524454150149,4.56287415921704,42.673263471366));
#58455=CARTESIAN_POINT('Ctrl Pts',(-4.84166118692218,2.55543383396763,42.812436928788));
#58456=CARTESIAN_POINT('Ctrl Pts',(-5.47412199142217,-0.0768996213472616,
42.9516103862099));
#58457=CARTESIAN_POINT('Ctrl Pts',(-4.76796812309811,-2.69042842422083,
43.0907838436319));
#58458=CARTESIAN_POINT('Ctrl Pts',(-2.89587895060334,-4.64605318869551,
43.2299573010538));
#58459=CARTESIAN_POINT('Ctrl Pts',(-0.315645885795919,-5.46555512308816,
43.3691307584758));
#58460=CARTESIAN_POINT('Ctrl Pts',(2.34177366020521,-4.94853728419866,43.5083042158978));
#58461=CARTESIAN_POINT('Ctrl Pts',(4.42654747655404,-3.22142865302774,43.6474776733197));
#58462=CARTESIAN_POINT('Ctrl Pts',(5.42887530223032,-0.706567818095944,
43.7866511307416));
#58463=CARTESIAN_POINT('Ctrl Pts',(5.10365285630411,1.98107361071568,43.9258245881636));
#58464=CARTESIAN_POINT('Ctrl Pts',(3.53040842454084,4.18427311305873,44.0649980455855));
#58465=CARTESIAN_POINT('Ctrl Pts',(1.09385540638558,5.36427119734416,44.2041715030075));
#58466=CARTESIAN_POINT('Ctrl Pts',(-1.61018359385595,5.23251697778539,44.3433449604294));
#58467=CARTESIAN_POINT('Ctrl Pts',(-3.92047627495196,3.82122897851909,44.4825184178514));
#58468=CARTESIAN_POINT('Ctrl Pts',(-5.2720751099238,1.47551657532438,44.6216918752733));
#58469=CARTESIAN_POINT('Ctrl Pts',(-5.33446681552716,-1.23101134144846,
44.7608653326954));
#58470=CARTESIAN_POINT('Ctrl Pts',(-4.09239443316404,-3.6365138432492,44.9000387901172));
#58471=CARTESIAN_POINT('Ctrl Pts',(-1.84958818995514,-5.15276126521632,
45.0392122475392));
#58472=CARTESIAN_POINT('Ctrl Pts',(0.845507186312134,-5.40897797431545,
45.1783857049612));
#58473=CARTESIAN_POINT('Ctrl Pts',(3.33384642390563,-4.34251000580848,45.3175591623831));
#58474=CARTESIAN_POINT('Ctrl Pts',(5.00694337296865,-2.214146153401,45.4567326198051));
#58475=CARTESIAN_POINT('Ctrl Pts',(5.45566719414789,0.455654030415216,45.595906077227));
#58476=CARTESIAN_POINT('Ctrl Pts',(4.57028918720294,3.01403083495691,45.735079534649));
#58477=CARTESIAN_POINT('Ctrl Pts',(2.56731530376392,4.83537147071399,45.874252992071));
#58478=CARTESIAN_POINT('Ctrl Pts',(-0.0634571455034273,5.47429432159248,
46.0134264494928));
#58479=CARTESIAN_POINT('Ctrl Pts',(-2.67871209877789,4.77456035888081,46.1525999069149));
#58480=CARTESIAN_POINT('Ctrl Pts',(-4.63892806583425,2.90727905931825,46.2917733643367));
#58481=CARTESIAN_POINT('Ctrl Pts',(-5.46476354505504,0.329066141334365,
46.4309468217588));
#58482=CARTESIAN_POINT('Ctrl Pts',(-4.95427281956437,-2.32961498064827,
46.5701202791806));
#58483=CARTESIAN_POINT('Ctrl Pts',(-3.23228876238798,-4.41862359624302,
46.7092937366026));
#58484=CARTESIAN_POINT('Ctrl Pts',(-0.719896824109031,-5.42712388760133,
46.8484671940246));
#58485=CARTESIAN_POINT('Ctrl Pts',(1.96853511714788,-5.10850218961397,46.9876406514465));
#58486=CARTESIAN_POINT('Ctrl Pts',(4.17559123303725,-3.5406726738457,47.1268141088685));
#58487=CARTESIAN_POINT('Ctrl Pts',(5.36156895479916,-1.10702460300981,47.2659875662904));
#58488=CARTESIAN_POINT('Ctrl Pts',(5.23645516572182,1.59732978001426,47.4051610237123));
#58489=CARTESIAN_POINT('Ctrl Pts',(3.8308445719689,3.91108105185148,47.5443344811344));
#58490=CARTESIAN_POINT('Ctrl Pts',(1.48845822470126,5.26843593887734,47.6835079385562));
#58491=CARTESIAN_POINT('Ctrl Pts',(-1.21790832296982,5.33747360139383,47.8226813959783));
#58492=CARTESIAN_POINT('Ctrl Pts',(-3.62645360289483,4.10131191142374,47.9618548534001));
#58493=CARTESIAN_POINT('Ctrl Pts',(-5.14820388432376,1.86223572465166,48.1010283108222));
#58494=CARTESIAN_POINT('Ctrl Pts',(-5.41103789223077,-0.832222360657202,
48.240201768244));
#58495=CARTESIAN_POINT('Ctrl Pts',(-4.35068350040957,-3.32317291274456,
48.3793752256661));
#58496=CARTESIAN_POINT('Ctrl Pts',(-2.22643451880982,-5.00149122384386,
48.5185486830879));
#58497=CARTESIAN_POINT('Ctrl Pts',(0.442255730198809,-5.45676964859627,
48.65772214051));
#58498=CARTESIAN_POINT('Ctrl Pts',(3.00279895389227,-4.57767665647527,48.7968955979318));
#58499=CARTESIAN_POINT('Ctrl Pts',(4.82905259735361,-2.57918129272208,48.936069055354));
#58500=CARTESIAN_POINT('Ctrl Pts',(5.47443364192402,0.0500142870148103,
49.0752425127757));
#58501=CARTESIAN_POINT('Ctrl Pts',(4.7811238042006,2.66697962077732,49.2144159701978));
#58502=CARTESIAN_POINT('Ctrl Pts',(2.91866163722327,4.63177497036894,49.3535894276197));
#58503=CARTESIAN_POINT('Ctrl Pts',(0.342484412613354,5.46393901465346,49.4927628850417));
#58504=CARTESIAN_POINT('Ctrl Pts',(-2.31744225357938,4.95997848080615,49.6319363424636));
#58505=CARTESIAN_POINT('Ctrl Pts',(-4.4106730717576,3.24312938113907,49.7711097998856));
#58506=CARTESIAN_POINT('Ctrl Pts',(-5.42533974756993,0.733221489164787,
49.9102832573075));
#58507=CARTESIAN_POINT('Ctrl Pts',(-5.11332071880119,-1.95598475336943,
50.0494567147295));
#58508=CARTESIAN_POINT('Ctrl Pts',(-3.55091557299522,-4.1668841743196,50.1886301721514));
#58509=CARTESIAN_POINT('Ctrl Pts',(-1.12018712430723,-5.35883438214613,
50.3278036295734));
#58510=CARTESIAN_POINT('Ctrl Pts',(1.5844663343195,-5.24036177798281,50.4669770869953));
#58511=CARTESIAN_POINT('Ctrl Pts',(3.9016622450437,-3.84043706553509,50.6061505444173));
#58512=CARTESIAN_POINT('Ctrl Pts',(5.26476499931227,-1.50139089871746,50.7453240018392));
#58513=CARTESIAN_POINT('Ctrl Pts',(5.34044820244678,1.20479796053868,50.8844974592612));
#58514=CARTESIAN_POINT('Ctrl Pts',(4.11020465888946,3.61637149512858,51.0236709166831));
#58515=CARTESIAN_POINT('Ctrl Pts',(1.87487203011983,5.14361545990847,51.1628443741051));
#58516=CARTESIAN_POINT('Ctrl Pts',(-0.818932516725154,5.4130651817418,51.3020178315271));
#58517=CARTESIAN_POINT('Ctrl Pts',(-3.3124793629455,4.35883076051311,51.4411912889489));
#58518=CARTESIAN_POINT('Ctrl Pts',(-4.99600891586951,2.23870945888194,51.580364746371));
#58519=CARTESIAN_POINT('Ctrl Pts',(-5.45783919887916,-0.428854763192953,
51.7195382037929));
#58520=CARTESIAN_POINT('Ctrl Pts',(-4.58503652248779,-2.99154896603551,
51.8587116612149));
#58521=CARTESIAN_POINT('Ctrl Pts',(-2.59103172929054,-4.82270460494367,
51.9978851186368));
#58522=CARTESIAN_POINT('Ctrl Pts',(0.0365711269414716,-5.47453995157669,
52.1370585760588));
#58523=CARTESIAN_POINT('Ctrl Pts',(2.65523106096563,-4.78765841948008,52.2762320334807));
#58524=CARTESIAN_POINT('Ctrl Pts',(4.62459394543255,-2.93002661568179,52.4154054909026));
#58525=CARTESIAN_POINT('Ctrl Pts',(5.46308153685529,-0.355900618721091,
52.5545789483246));
#58526=CARTESIAN_POINT('Ctrl Pts',(4.96565423351902,2.30525555239972,52.6937524057466));
#58527=CARTESIAN_POINT('Ctrl Pts',(3.25395044391241,4.40269595103925,52.8329258631685));
#58528=CARTESIAN_POINT('Ctrl Pts',(0.746541732915853,5.42352289289444,52.9720993205905));
#58529=CARTESIAN_POINT('Ctrl Pts',(-1.94342259505864,5.11810841481017,53.1112727780124));
#58530=CARTESIAN_POINT('Ctrl Pts',(-4.15815198940913,3.56113706022502,53.2504462354344));
#58531=CARTESIAN_POINT('Ctrl Pts',(-5.35606749587446,1.13334289090821,53.3896196928563));
#58532=CARTESIAN_POINT('Ctrl Pts',(-5.24423679101162,-1.5715933343379,53.5287931502783));
#58533=CARTESIAN_POINT('Ctrl Pts',(-3.85000640137521,-3.89221991132376,
53.6679666077002));
#58534=CARTESIAN_POINT('Ctrl Pts',(-1.51431451938932,-5.26106231336427,
53.8071400651222));
#58535=CARTESIAN_POINT('Ctrl Pts',(1.19168033321019,-5.34339060074923,53.9463135225442));
#58536=CARTESIAN_POINT('Ctrl Pts',(3.60626758074524,-4.11907262193822,54.085486979966));
#58537=CARTESIAN_POINT('Ctrl Pts',(5.13899601963854,-1.88749703016309,54.2246604373881));
#58538=CARTESIAN_POINT('Ctrl Pts',(5.41505983062401,0.805637734653367,54.36383389481));
#58539=CARTESIAN_POINT('Ctrl Pts',(4.36695173699138,3.30176583899027,54.5030073522319));
#58540=CARTESIAN_POINT('Ctrl Pts',(2.25097089959977,4.99049648210379,54.6421808096539));
#58541=CARTESIAN_POINT('Ctrl Pts',(-0.415451210205248,5.4588758385472,54.7813542670759));
#58542=CARTESIAN_POINT('Ctrl Pts',(-2.98028093922396,4.59236874086062,54.9205277244978));
#58543=CARTESIAN_POINT('Ctrl Pts',(-4.81632753176252,2.60286654201122,55.0597011819197));
#58544=CARTESIAN_POINT('Ctrl Pts',(-5.47461324990945,-0.0231277463455877,
55.1988746393417));
#58545=CARTESIAN_POINT('Ctrl Pts',(-4.79416416531556,-2.64346649018657,
55.3380480967637));
#58546=CARTESIAN_POINT('Ctrl Pts',(-2.94137392616304,-4.61738503432661,
55.4772215541856));
#58547=CARTESIAN_POINT('Ctrl Pts',(-0.369314678757935,-5.46219111683115,
55.6163950116077));
#58548=CARTESIAN_POINT('Ctrl Pts',(2.29305495059507,-4.97130004347822,55.7555684690294));
#58549=CARTESIAN_POINT('Ctrl Pts',(4.39469228218995,-3.26475188545704,55.8947419264516));
#58550=CARTESIAN_POINT('Ctrl Pts',(5.4216733345305,-0.759857475041239,56.0339153838733));
#58551=CARTESIAN_POINT('Ctrl Pts',(5.12286524877114,1.93084871796528,56.1730888412955));
#58552=CARTESIAN_POINT('Ctrl Pts',(3.57133707389957,4.14939473096083,56.3122622987172));
#58553=CARTESIAN_POINT('Ctrl Pts',(1.14649182348355,5.3532683126685,56.4514357561394));
#58554=CARTESIAN_POINT('Ctrl Pts',(-1.55871085769357,5.2480801814419,56.5906092135611));
#58555=CARTESIAN_POINT('Ctrl Pts',(-3.88275410762888,3.85955252178621,56.7297826709834));
#58556=CARTESIAN_POINT('Ctrl Pts',(-5.25732790336052,1.52722900878748,56.868956128405));
#58557=CARTESIAN_POINT('Ctrl Pts',(-5.34630077855855,-1.17855552008353,
57.0081295858272));
#58558=CARTESIAN_POINT('Ctrl Pts',(-4.12791574709623,-3.5961419206714,57.1473030432489));
#58559=CARTESIAN_POINT('Ctrl Pts',(-1.90011064865274,-5.13434559136913,
57.2864765006711));
#58560=CARTESIAN_POINT('Ctrl Pts',(0.792338094609303,-5.4170218268497,57.4256499580929));
#58561=CARTESIAN_POINT('Ctrl Pts',(3.29103240548137,-4.37504638087491,57.5648234155149));
#58562=CARTESIAN_POINT('Ctrl Pts',(4.98495395578654,-2.26321876702701,57.7039968729369));
#58563=CARTESIAN_POINT('Ctrl Pts',(5.45987956134944,0.402045152058584,57.8431703303588));
#58564=CARTESIAN_POINT('Ctrl Pts',(4.59967326738087,2.96899494140306,57.9823437877808));
#58565=CARTESIAN_POINT('Ctrl Pts',(2.6146856595211,4.80992141626346,58.1215172452027));
#58566=CARTESIAN_POINT('Ctrl Pts',(-0.00968422628974487,5.47465353648031,
58.2606907026247));
#58567=CARTESIAN_POINT('Ctrl Pts',(-2.63168597937963,4.80064100247788,58.3998641600466));
#58568=CARTESIAN_POINT('Ctrl Pts',(-4.61014828052031,2.95270350024359,58.5390376174686));
#58569=CARTESIAN_POINT('Ctrl Pts',(-5.46126775995019,0.382726511838092,
58.6782110748906));
#58570=CARTESIAN_POINT('Ctrl Pts',(-4.97691587663996,-2.28084052173411,
58.8173845323124));
#58571=CARTESIAN_POINT('Ctrl Pts',(-3.27553364064106,-4.38666211347123,
58.9565579897345));
#58572=CARTESIAN_POINT('Ctrl Pts',(-0.773168635248014,-5.41979108363079,
59.0957314471564));
#58573=CARTESIAN_POINT('Ctrl Pts',(1.91826319790888,-5.12759119200075,59.2349049045783));
#58574=CARTESIAN_POINT('Ctrl Pts',(4.14061245178034,-3.58151555251356,59.3740783620003));
#58575=CARTESIAN_POINT('Ctrl Pts',(5.35043684940709,-1.1596338427462,59.5132518194222));
#58576=CARTESIAN_POINT('Ctrl Pts',(5.25189192609828,1.54581898206696,59.6524252768443));
#58577=CARTESIAN_POINT('Ctrl Pts',(3.86907536920578,3.873264891037,59.7915987342661));
#58578=CARTESIAN_POINT('Ctrl Pts',(1.54013428903837,5.25356179181951,59.9307721916881));
#58579=CARTESIAN_POINT('Ctrl Pts',(-1.16542360030005,5.34917871832605,60.06994564911));
#58580=CARTESIAN_POINT('Ctrl Pts',(-3.58599457596465,4.13673398104114,60.209119106532));
#58581=CARTESIAN_POINT('Ctrl Pts',(-5.12966420314073,1.9127128095276,60.3482925639539));
#58582=CARTESIAN_POINT('Ctrl Pts',(-5.41895115859066,-0.779033676784864,
60.4874660213759));
#58583=CARTESIAN_POINT('Ctrl Pts',(-4.38311464334877,-3.28027912714825,
60.6266394787978));
#58584=CARTESIAN_POINT('Ctrl Pts',(-2.2754529873193,-4.97938137032394,60.7658129362198));
#58585=CARTESIAN_POINT('Ctrl Pts',(0.388636669609436,-5.46085036126269,
60.9049863936417));
#58586=CARTESIAN_POINT('Ctrl Pts',(2.95769104059119,-4.60695005794557,61.0441598510637));
#58587=CARTESIAN_POINT('Ctrl Pts',(4.8034862971456,-2.62648901066184,61.1833333084856));
#58588=CARTESIAN_POINT('Ctrl Pts',(5.47466081090924,-0.00375935194546259,
61.3225067659076));
#58589=CARTESIAN_POINT('Ctrl Pts',(4.8070888921791,2.6198895991595,61.4616802233296));
#58590=CARTESIAN_POINT('Ctrl Pts',(2.96401526908478,4.60288372847367,61.6008536807515));
#58591=CARTESIAN_POINT('Ctrl Pts',(0.396136038105091,5.46031147017638,61.7400271381735));
#58592=CARTESIAN_POINT('Ctrl Pts',(-2.26861234145274,4.98250170226862,61.8792005955954));
#58593=CARTESIAN_POINT('Ctrl Pts',(-4.37860548943786,3.28629563835069,62.0183740530173));
#58594=CARTESIAN_POINT('Ctrl Pts',(-5.4178761590868,0.786475145165815,62.1575475104394));
#58595=CARTESIAN_POINT('Ctrl Pts',(-5.13228620129426,-1.90566613397912,
62.2967209678612));
#58596=CARTESIAN_POINT('Ctrl Pts',(-3.59167246337271,-4.13180515958241,
62.4358944252833));
#58597=CARTESIAN_POINT('Ctrl Pts',(-1.17276881351499,-5.34757321139456,
62.5750678827051));
#58598=CARTESIAN_POINT('Ctrl Pts',(1.53291767611305,-5.25567182993055,62.7142413401272));
#58599=CARTESIAN_POINT('Ctrl Pts',(3.86375253149927,-3.87857522176944,62.853414797549));
#58600=CARTESIAN_POINT('Ctrl Pts',(5.24976358658708,-1.55302962792484,62.9925882549711));
#58601=CARTESIAN_POINT('Ctrl Pts',(5.35202521175614,1.15228337685149,63.131761712393));
#58602=CARTESIAN_POINT('Ctrl Pts',(4.14552569279038,3.57582809662026,63.2709351698149));
#58603=CARTESIAN_POINT('Ctrl Pts',(1.92530651381152,5.12494702954711,63.410108627237));
#58604=CARTESIAN_POINT('Ctrl Pts',(-0.765730562202499,5.42085727985497,
63.5492820846588));
#58605=CARTESIAN_POINT('Ctrl Pts',(-3.26949436548285,4.39113801409943,63.6884555420809));
#58606=CARTESIAN_POINT('Ctrl Pts',(-4.97380159054169,2.28770951087992,63.8276289995027));
#58607=CARTESIAN_POINT('Ctrl Pts',(-5.46174362790934,-0.375296313299901,
63.9668024569247));
#58608=CARTESIAN_POINT('Ctrl Pts',(-4.61428688809175,-2.94622961609203,
64.1059759143467));
#58609=CARTESIAN_POINT('Ctrl Pts',(-2.63809654804704,-4.79731827894146,
64.2451493717686));
#58610=CARTESIAN_POINT('Ctrl Pts',(-0.891129108788059,-5.24830906904511,
64.3379316767166));
#58611=CARTESIAN_POINT('Ctrl Pts',(-0.016500361394378,-5.25105740891156,
64.3843228291906));
#58612=CARTESIAN_POINT('Ctrl Pts',(2.85706463458441,-4.0032942355399,0.));
#58613=CARTESIAN_POINT('Ctrl Pts',(3.52386294776537,-3.52741468062806,0.046391152473984));
#58614=CARTESIAN_POINT('Ctrl Pts',(4.61438908619534,-2.23650256226449,0.139173457421952));
#58615=CARTESIAN_POINT('Ctrl Pts',(5.12163790500659,0.248365779535813,0.278346914843904));
#58616=CARTESIAN_POINT('Ctrl Pts',(4.37650875504895,2.67182739135543,0.417520372265856));
#58617=CARTESIAN_POINT('Ctrl Pts',(2.56115201646861,4.44226470421493,0.556693829687809));
#58618=CARTESIAN_POINT('Ctrl Pts',(0.119512633872891,5.12624413067081,0.695867287109761));
#58619=CARTESIAN_POINT('Ctrl Pts',(-2.35135624542669,4.55676348086115,0.835040744531713));
#58620=CARTESIAN_POINT('Ctrl Pts',(-4.24723382866677,2.87295023988583,0.974214201953666));
#58621=CARTESIAN_POINT('Ctrl Pts',(-5.10451506553093,0.486622655626781,
1.11338765937562));
#58622=CARTESIAN_POINT('Ctrl Pts',(-4.71356287464545,-2.01871284948783,
1.25256111679757));
#58623=CARTESIAN_POINT('Ctrl Pts',(-3.16997967797153,-4.03039635294118,
1.39173457421952));
#58624=CARTESIAN_POINT('Ctrl Pts',(-0.85122519685208,-5.05650975620884,
1.53090803164147));
#58625=CARTESIAN_POINT('Ctrl Pts',(1.67568359580848,-4.84612774610485,1.67008148906343));
#58626=CARTESIAN_POINT('Ctrl Pts',(3.79282906492235,-3.45069846869191,1.80925494648538));
#58627=CARTESIAN_POINT('Ctrl Pts',(4.98249488295983,-1.21145207040314,1.94842840390733));
#58628=CARTESIAN_POINT('Ctrl Pts',(4.95376609667662,1.32403660424732,2.08760186132928));
#58629=CARTESIAN_POINT('Ctrl Pts',(3.71366788460521,3.5357520353937,2.22677531875123));
#58630=CARTESIAN_POINT('Ctrl Pts',(1.56544772852549,4.88285212444658,2.36594877617319));
#58631=CARTESIAN_POINT('Ctrl Pts',(-0.965579261288932,5.03592377327551,
2.50512223359514));
#58632=CARTESIAN_POINT('Ctrl Pts',(-3.26048828129931,3.9575355560864,2.6442956910171));
#58633=CARTESIAN_POINT('Ctrl Pts',(-4.75809364994143,1.91139120725042,2.78346914843904));
#58634=CARTESIAN_POINT('Ctrl Pts',(-5.09217836896138,-0.602155282161658,
2.922642605861));
#58635=CARTESIAN_POINT('Ctrl Pts',(-4.18104701653603,-2.96845369999834,
3.06181606328295));
#58636=CARTESIAN_POINT('Ctrl Pts',(-2.24750313966228,-4.60886115685302,
3.2009895207049));
#58637=CARTESIAN_POINT('Ctrl Pts',(0.235634020762259,-5.12224053832399,
3.34016297812685));
#58638=CARTESIAN_POINT('Ctrl Pts',(2.66115040510108,-4.38305259454633,3.47933643554881));
#58639=CARTESIAN_POINT('Ctrl Pts',(4.43592225278534,-2.57205468293112,3.61850989297076));
#58640=CARTESIAN_POINT('Ctrl Pts',(5.12595564846396,-0.132099261254929,
3.75768335039271));
#58641=CARTESIAN_POINT('Ctrl Pts',(4.56251324399756,2.34015905938081,3.89685680781466));
#58642=CARTESIAN_POINT('Ctrl Pts',(2.88337645366723,4.24016647683272,4.03603026523662));
#58643=CARTESIAN_POINT('Ctrl Pts',(0.499153069686797,5.10330458995647,4.17520372265857));
#58644=CARTESIAN_POINT('Ctrl Pts',(-2.00713073313589,4.71850588056565,4.31437718008052));
#58645=CARTESIAN_POINT('Ctrl Pts',(-4.02260072986122,3.17986711875809,4.45355063750247));
#58646=CARTESIAN_POINT('Ctrl Pts',(-5.05440387218634,0.86363940488164,4.59272409492443));
#58647=CARTESIAN_POINT('Ctrl Pts',(-4.85022813126969,-1.66377841056938,
4.73189755234637));
#58648=CARTESIAN_POINT('Ctrl Pts',(-3.46000163130249,-3.78434409590636,
4.87107100976833));
#58649=CARTESIAN_POINT('Ctrl Pts',(-1.22368347336451,-4.9795050237801,5.01024446719028));
#58650=CARTESIAN_POINT('Ctrl Pts',(1.31186817898678,-4.95700246175034,5.14941792461223));
#58651=CARTESIAN_POINT('Ctrl Pts',(3.52662208588147,-3.72233907485736,5.28859138203419));
#58652=CARTESIAN_POINT('Ctrl Pts',(4.87899329888229,-1.57743333117398,5.42776483945614));
#58653=CARTESIAN_POINT('Ctrl Pts',(5.03827966124805,0.953210144664441,5.56693829687808));
#58654=CARTESIAN_POINT('Ctrl Pts',(3.96553007503505,3.25076033395718,5.70611175430005));
#58655=CARTESIAN_POINT('Ctrl Pts',(1.92306940962342,4.75338569554455,5.84528521172199));
#58656=CARTESIAN_POINT('Ctrl Pts',(-0.589649122276164,5.09364166755337,
5.98445866914395));
#58657=CARTESIAN_POINT('Ctrl Pts',(-2.9581777789531,4.18832374022651,6.1236321265659));
#58658=CARTESIAN_POINT('Ctrl Pts',(-4.60332829646294,2.25881387454135,6.26280558398785));
#58659=CARTESIAN_POINT('Ctrl Pts',(-5.12280371737697,-0.223055145795024,
6.4019790414098));
#58660=CARTESIAN_POINT('Ctrl Pts',(-4.3895740957611,-2.65037936580031,6.54115249883176));
#58661=CARTESIAN_POINT('Ctrl Pts',(-2.58293977084456,-4.42959294574867,
6.68032595625371));
#58662=CARTESIAN_POINT('Ctrl Pts',(-0.14468615032387,-5.12561581107493,
6.81949941367566));
#58663=CARTESIAN_POINT('Ctrl Pts',(2.32894830461766,-4.5682459784096,6.95867287109761));
#58664=CARTESIAN_POINT('Ctrl Pts',(4.2330732788251,-2.89377990540639,7.09784632851956));
#58665=CARTESIAN_POINT('Ctrl Pts',(5.10206348419584,-0.51168323020428,7.23701978594152));
#58666=CARTESIAN_POINT('Ctrl Pts',(4.72342036091109,1.9955379272185,7.37619324336347));
#58667=CARTESIAN_POINT('Ctrl Pts',(3.18973542252992,4.01478012587175,7.51536670078542));
#58668=CARTESIAN_POINT('Ctrl Pts',(0.876048385964622,5.05226788188094,7.65454015820737));
#58669=CARTESIAN_POINT('Ctrl Pts',(-1.65186318293549,4.85429907913586,7.79371361562932));
#58670=CARTESIAN_POINT('Ctrl Pts',(-3.77583631245843,3.46928402791661,7.93288707305128));
#58671=CARTESIAN_POINT('Ctrl Pts',(-4.97648513573483,1.23590744744384,8.07206053047323));
#58672=CARTESIAN_POINT('Ctrl Pts',(-4.96020893756964,-1.29969181750568,
8.21123398789518));
#58673=CARTESIAN_POINT('Ctrl Pts',(-3.73098781882938,-3.51747088411314,
8.35040744531713));
#58674=CARTESIAN_POINT('Ctrl Pts',(-1.58940942229392,-4.87510504637185,
8.48958090273909));
#58675=CARTESIAN_POINT('Ctrl Pts',(0.940835280389158,-5.04060517200187,
8.62875436016105));
#58676=CARTESIAN_POINT('Ctrl Pts',(3.24101278453099,-3.97350068017404,8.76792781758299));
#58677=CARTESIAN_POINT('Ctrl Pts',(4.74864907841449,-1.93473601685351,8.90710127500494));
#58678=CARTESIAN_POINT('Ctrl Pts',(5.09507425160708,0.577139407290319,9.04627473242689));
#58679=CARTESIAN_POINT('Ctrl Pts',(4.19557520845658,2.94788401994064,9.18544818984885));
#58680=CARTESIAN_POINT('Ctrl Pts',(2.27011098883077,4.59776767825721,9.3246216472708));
#58681=CARTESIAN_POINT('Ctrl Pts',(-0.210474925808355,5.12333600600652,
9.46379510469275));
#58682=CARTESIAN_POINT('Ctrl Pts',(-2.63959234478916,4.39606912800144,9.60296856211471));
#58683=CARTESIAN_POINT('Ctrl Pts',(-4.42323692839189,2.59380928368822,9.74214201953665));
#58684=CARTESIAN_POINT('Ctrl Pts',(-5.12524506636906,0.157272166947933,
9.88131547695861));
#58685=CARTESIAN_POINT('Ctrl Pts',(-4.57395116642832,-2.31772350636695,
10.0204889343806));
#58686=CARTESIAN_POINT('Ctrl Pts',(-2.90416590773529,-4.225954555504,10.1596623918025));
#58687=CARTESIAN_POINT('Ctrl Pts',(-0.524210305286386,-5.10079161313893,
10.2988358492245));
#58688=CARTESIAN_POINT('Ctrl Pts',(1.98393308826428,-4.72830635916573,10.4380093066464));
#58689=CARTESIAN_POINT('Ctrl Pts',(4.00693531287256,-3.1995844922883,10.5771827640684));
#58690=CARTESIAN_POINT('Ctrl Pts',(5.05010142654417,-0.888452084500591,
10.7163562214903));
#58691=CARTESIAN_POINT('Ctrl Pts',(4.85834075571687,1.63993799461361,10.8555296789123));
#58692=CARTESIAN_POINT('Ctrl Pts',(3.47854550484689,3.76730576082515,10.9947031363342));
#58693=CARTESIAN_POINT('Ctrl Pts',(1.24812396903648,4.97343523962598,11.1338765937562));
#58694=CARTESIAN_POINT('Ctrl Pts',(-1.28750761891996,4.96338550347039,11.2730500511781));
#58695=CARTESIAN_POINT('Ctrl Pts',(-3.5082984720956,3.73961406505117,11.4122235086001));
#58696=CARTESIAN_POINT('Ctrl Pts',(-4.87118739711688,1.60137592932035,11.551396966022));
#58697=CARTESIAN_POINT('Ctrl Pts',(-5.04290028805014,-0.928454742903895,
11.690570423444));
#58698=CARTESIAN_POINT('Ctrl Pts',(-3.98144732521719,-3.23124569189002,
11.829743880866));
#58699=CARTESIAN_POINT('Ctrl Pts',(-1.94639095768057,-4.74388382706577,
11.9689173382879));
#58700=CARTESIAN_POINT('Ctrl Pts',(0.564626212170274,-5.09647611250825,
12.1080907957099));
#58701=CARTESIAN_POINT('Ctrl Pts',(2.93757248527155,-4.20280137748769,12.2472642531318));
#58702=CARTESIAN_POINT('Ctrl Pts',(4.59217933564339,-2.28139441441562,12.3864377105538));
#58703=CARTESIAN_POINT('Ctrl Pts',(5.12383740106595,0.197893436663885,12.5256111679757));
#58704=CARTESIAN_POINT('Ctrl Pts',(4.40253765207021,2.62878940711139,12.6647846253977));
#58705=CARTESIAN_POINT('Ctrl Pts',(2.60466315593581,4.41685423904247,12.8039580828196));
#58706=CARTESIAN_POINT('Ctrl Pts',(0.169857235225308,5.12484341658148,12.9431315402416));
#58707=CARTESIAN_POINT('Ctrl Pts',(-2.30648473230954,4.57962877365185,13.0823049976635));
#58708=CARTESIAN_POINT('Ctrl Pts',(-4.21881034979734,2.9145343980265,13.2214784550854));
#58709=CARTESIAN_POINT('Ctrl Pts',(-5.09948898445394,0.536734219395287,
13.3606519125074));
#58710=CARTESIAN_POINT('Ctrl Pts',(-4.73316384586776,-1.97231628625004,
13.4998253699294));
#58711=CARTESIAN_POINT('Ctrl Pts',(-3.20941426864339,-3.99906633816759,
13.6389988273513));
#58712=CARTESIAN_POINT('Ctrl Pts',(-0.900850425695856,-5.04790451923969,
13.7781722847733));
#58713=CARTESIAN_POINT('Ctrl Pts',(1.62800291751233,-4.86235313664159,13.9173457421952));
#58714=CARTESIAN_POINT('Ctrl Pts',(3.75875249244549,-3.4877860062469,14.0565191996172));
#58715=CARTESIAN_POINT('Ctrl Pts',(4.97035535384435,-1.26033296447714,14.1956926570391));
#58716=CARTESIAN_POINT('Ctrl Pts',(4.96653214029797,1.27531565669998,14.3348661144611));
#58717=CARTESIAN_POINT('Ctrl Pts',(3.7482177615067,3.49910490513827,14.474039571883));
#58718=CARTESIAN_POINT('Ctrl Pts',(1.61333278009552,4.86724037474072,14.613213029305));
#58719=CARTESIAN_POINT('Ctrl Pts',(-0.916068606863061,5.04516499555335,
14.7523864867269));
#58720=CARTESIAN_POINT('Ctrl Pts',(-3.22145911492965,3.98936996224636,14.8915599441489));
#58721=CARTESIAN_POINT('Ctrl Pts',(-4.73908997023278,1.95803416182558,15.0307334015708));
#58722=CARTESIAN_POINT('Ctrl Pts',(-5.09784724180366,-0.552109612370288,
15.1699068589928));
#58723=CARTESIAN_POINT('Ctrl Pts',(-4.21000220374625,-2.92724323712408,
15.3090803164148));
#58724=CARTESIAN_POINT('Ctrl Pts',(-2.29266408325714,-4.58656330231903,
15.4482537738367));
#58725=CARTESIAN_POINT('Ctrl Pts',(0.185310754227624,-5.12430789953185,
15.5874272312587));
#58726=CARTESIAN_POINT('Ctrl Pts',(2.6179706179084,-4.40897962896238,15.7266006886806));
#58727=CARTESIAN_POINT('Ctrl Pts',(4.41044491618784,-2.61550132213878,15.8657741461026));
#58728=CARTESIAN_POINT('Ctrl Pts',(5.12441086413413,-0.182441279268398,
16.0049476035245));
#58729=CARTESIAN_POINT('Ctrl Pts',(4.58527876584435,2.29523205021492,16.1441210609465));
#58730=CARTESIAN_POINT('Ctrl Pts',(2.92488531375835,4.21164070478449,16.2832945183684));
#58731=CARTESIAN_POINT('Ctrl Pts',(0.549254897012139,5.09815560599567,16.4224679757903));
#58732=CARTESIAN_POINT('Ctrl Pts',(-1.96068759122481,4.73799279172668,16.5616414332123));
#58733=CARTESIAN_POINT('Ctrl Pts',(-3.99117324920656,3.21922469232187,16.7008148906343));
#58734=CARTESIAN_POINT('Ctrl Pts',(-5.0456771732148,0.913243334788716,16.8399883480562));
#58735=CARTESIAN_POINT('Ctrl Pts',(-4.86633619771543,-1.61605802359984,
16.9791618054782));
#58736=CARTESIAN_POINT('Ctrl Pts',(-3.4970054763967,-3.75017655889538,17.1183352629001));
#58737=CARTESIAN_POINT('Ctrl Pts',(-1.27253436014598,-4.96724549696155,
17.2575087203221));
#58738=CARTESIAN_POINT('Ctrl Pts',(1.2631160043629,-4.96964882907829,17.3966821777441));
#58739=CARTESIAN_POINT('Ctrl Pts',(3.48989023867801,-3.75679885631596,17.535855635166));
#58740=CARTESIAN_POINT('Ctrl Pts',(4.86326400304377,-1.62527990252007,17.675029092588));
#58741=CARTESIAN_POINT('Ctrl Pts',(5.04739928085542,0.903676946954519,17.8142025500099));
#58742=CARTESIAN_POINT('Ctrl Pts',(3.9972685434884,3.21165311266256,17.9533760074318));
#58743=CARTESIAN_POINT('Ctrl Pts',(1.96966555908043,4.73426753682229,18.0925494648538));
#58744=CARTESIAN_POINT('Ctrl Pts',(-0.539589683365057,5.09918763122548,
18.2317229222758));
#58745=CARTESIAN_POINT('Ctrl Pts',(-2.91689633778329,4.21717764381148,18.3708963796977));
#58746=CARTESIAN_POINT('Ctrl Pts',(-4.58091961214863,2.30391992739958,18.5100698371197));
#58747=CARTESIAN_POINT('Ctrl Pts',(-5.12474749856713,-0.1727269543728,18.6492432945416));
#58748=CARTESIAN_POINT('Ctrl Pts',(-4.41539501983301,-2.60713604241717,
18.7884167519636));
#58749=CARTESIAN_POINT('Ctrl Pts',(-2.62632371694331,-4.40400899847605,
18.9275902093855));
#58750=CARTESIAN_POINT('Ctrl Pts',(-0.195024223195767,-5.12394741163527,
19.0667636668075));
#58751=CARTESIAN_POINT('Ctrl Pts',(2.28396552793643,-4.59090110893657,19.2059371242294));
#58752=CARTESIAN_POINT('Ctrl Pts',(4.2044456636982,-2.9352185925151,19.3451105816514));
#58753=CARTESIAN_POINT('Ctrl Pts',(5.09679148580437,-0.561772262637615,
19.4842840390733));
#58754=CARTESIAN_POINT('Ctrl Pts',(4.74279316762406,1.94904707330927,19.6234574964953));
#58755=CARTESIAN_POINT('Ctrl Pts',(3.22901570416719,3.98325609358456,19.7626309539172));
#58756=CARTESIAN_POINT('Ctrl Pts',(0.925630737050274,5.04341940190033,19.9018044113392));
#58757=CARTESIAN_POINT('Ctrl Pts',(-1.60410338490353,4.87028991492066,20.0409778687611));
#58758=CARTESIAN_POINT('Ctrl Pts',(-3.7415780118875,3.5062038597031,20.1801513261831));
#58759=CARTESIAN_POINT('Ctrl Pts',(-4.96410568772994,1.28472808246885,20.319324783605));
#58760=CARTESIAN_POINT('Ctrl Pts',(-4.97273555101776,-1.25090873547233,
20.458498241027));
#58761=CARTESIAN_POINT('Ctrl Pts',(-3.76535729773513,-3.48065452827909,
20.5976716984489));
#58762=CARTESIAN_POINT('Ctrl Pts',(-1.63721722455307,-4.85925830600346,
20.7368451558709));
#58763=CARTESIAN_POINT('Ctrl Pts',(0.891279837899838,-5.04960313048365,
20.8760186132929));
#58764=CARTESIAN_POINT('Ctrl Pts',(3.20182774421876,-4.00514302131496,21.0151920707148));
#58765=CARTESIAN_POINT('Ctrl Pts',(4.72941655591346,-1.98128507930803,21.1543655281368));
#58766=CARTESIAN_POINT('Ctrl Pts',(5.10049727269117,0.527066500649415,21.2935389855586));
#58767=CARTESIAN_POINT('Ctrl Pts',(4.22432765441569,2.9065318496407,21.4327124429807));
#58768=CARTESIAN_POINT('Ctrl Pts',(2.3151618789705,4.57524829916352,21.5718859004026));
#58769=CARTESIAN_POINT('Ctrl Pts',(-0.160142112979361,5.12515619552101,
21.7110593578246));
#58770=CARTESIAN_POINT('Ctrl Pts',(-2.5962857459699,4.4217837859975,21.8502328152465));
#58771=CARTESIAN_POINT('Ctrl Pts',(-4.39754652471548,2.63713027509066,21.9894062726684));
#58772=CARTESIAN_POINT('Ctrl Pts',(-5.12345306187953,0.207605991132635,
22.1285797300904));
#58773=CARTESIAN_POINT('Ctrl Pts',(-4.5964957690259,-2.27268523341089,22.2677531875124));
#58774=CARTESIAN_POINT('Ctrl Pts',(-2.94553417198737,-4.19722526992435,
22.4069266449343));
#58775=CARTESIAN_POINT('Ctrl Pts',(-0.57428624079235,-5.09539663210565,
22.5461001023563));
#58776=CARTESIAN_POINT('Ctrl Pts',(1.93739480269542,-4.74756494461378,22.6852735597782));
#58777=CARTESIAN_POINT('Ctrl Pts',(3.97531491904182,-3.23878724513983,22.8244470172002));
#58778=CARTESIAN_POINT('Ctrl Pts',(5.04113121891057,-0.938012557784862,
22.9636204746221));
#58779=CARTESIAN_POINT('Ctrl Pts',(4.87421426441648,1.59213907350953,23.1027939320441));
#58780=CARTESIAN_POINT('Ctrl Pts',(3.51538110070013,3.73295690327082,23.241967389466));
#58781=CARTESIAN_POINT('Ctrl Pts',(1.29691405791799,4.9609359450825,23.381140846888));
#58782=CARTESIAN_POINT('Ctrl Pts',(-1.23869392363774,4.97579228750355,23.52031430431));
#58783=CARTESIAN_POINT('Ctrl Pts',(-3.47139782963254,3.77389303415709,23.6594877617318));
#58784=CARTESIAN_POINT('Ctrl Pts',(-4.85522330777404,1.64914467421285,23.7986612191539));
#58785=CARTESIAN_POINT('Ctrl Pts',(-5.05177653114886,-0.878877354453079,
23.9378346765758));
#58786=CARTESIAN_POINT('Ctrl Pts',(-4.01299334824328,-3.19198306884484,
24.0770081339978));
#58787=CARTESIAN_POINT('Ctrl Pts',(-1.99289265244315,-4.72453705675752,
24.2161815914197));
#58788=CARTESIAN_POINT('Ctrl Pts',(0.514540139737736,-5.10177615830366,
24.3553550488417));
#58789=CARTESIAN_POINT('Ctrl Pts',(2.89614983519387,-4.23145219244452,24.4945285062636));
#58790=CARTESIAN_POINT('Ctrl Pts',(4.56954939756152,-2.32638987018126,24.6337019636856));
#58791=CARTESIAN_POINT('Ctrl Pts',(5.12553398792908,0.147556305933546,24.7728754211075));
#58792=CARTESIAN_POINT('Ctrl Pts',(4.42814588893175,2.58541979399356,24.9120488785295));
#58793=CARTESIAN_POINT('Ctrl Pts',(2.64792093141759,4.39105753387467,25.0512223359514));
#58794=CARTESIAN_POINT('Ctrl Pts',(0.220186507211287,5.12292781784782,25.1903957933734));
#58795=CARTESIAN_POINT('Ctrl Pts',(-2.26139123465815,4.60206271237672,25.3295692507953));
#58796=CARTESIAN_POINT('Ctrl Pts',(-4.18997956700173,2.95583198997252,25.4687427082172));
#58797=CARTESIAN_POINT('Ctrl Pts',(-5.09397105331041,0.586796756017421,
25.6079161656392));
#58798=CARTESIAN_POINT('Ctrl Pts',(-4.75230809392217,-1.92573084964611,
25.7470896230612));
#58799=CARTESIAN_POINT('Ctrl Pts',(-3.24853925631766,-3.96734977346339,
25.8862630804831));
#58800=CARTESIAN_POINT('Ctrl Pts',(-0.950388722330458,-5.03881263804321,
26.0254365379051));
#58801=CARTESIAN_POINT('Ctrl Pts',(1.58016516156227,-4.87810922253918,26.164609995327));
#58802=CARTESIAN_POINT('Ctrl Pts',(3.72431328503039,-3.52453714404928,26.303783452749));
#58803=CARTESIAN_POINT('Ctrl Pts',(4.95773628813266,-1.30909221301232,26.4429569101709));
#58804=CARTESIAN_POINT('Ctrl Pts',(4.97881902010364,1.22647164251408,26.5821303675929));
#58805=CARTESIAN_POINT('Ctrl Pts',(3.78240601411158,3.462120198556,26.7213038250149));
#58806=CARTESIAN_POINT('Ctrl Pts',(1.66106217957725,4.85115903268642,26.8604772824368));
#58807=CARTESIAN_POINT('Ctrl Pts',(-0.866469571400946,5.05391946974555,
26.9996507398587));
#58808=CARTESIAN_POINT('Ctrl Pts',(-3.182119145904,4.02081947693602,27.1388241972807));
#58809=CARTESIAN_POINT('Ctrl Pts',(-4.7196290687778,2.00448820849228,27.2779976547026));
#58810=CARTESIAN_POINT('Ctrl Pts',(-5.10302428035127,-0.502010676163758,
27.4171711121246));
#58811=CARTESIAN_POINT('Ctrl Pts',(-4.23855121493717,-2.88575035704607,
27.5563445695465));
#58812=CARTESIAN_POINT('Ctrl Pts',(-2.33760383332739,-4.56382294170687,
27.6955180269685));
#58813=CARTESIAN_POINT('Ctrl Pts',(0.134969609127406,-5.12588087351325,
27.8346914843905));
#58814=CARTESIAN_POINT('Ctrl Pts',(2.57453825200954,-4.43448129027247,27.9738649418124));
#58815=CARTESIAN_POINT('Ctrl Pts',(4.38454206508205,-2.65869562085676,28.1130383992344));
#58816=CARTESIAN_POINT('Ctrl Pts',(5.12237168270734,-0.232765695571575,
28.2522118566563));
#58817=CARTESIAN_POINT('Ctrl Pts',(4.60760190542052,2.25008359978071,28.3913853140782));
#58818=CARTESIAN_POINT('Ctrl Pts',(2.96611198437499,4.18270859862171,28.5305587715002));
#58819=CARTESIAN_POINT('Ctrl Pts',(0.59930373287477,5.09251475801487,28.6697322289221));
#58820=CARTESIAN_POINT('Ctrl Pts',(-1.91405528449465,4.75702258694817,28.8089056863441));
#58821=CARTESIAN_POINT('Ctrl Pts',(-3.95936070487888,3.25827167889634,28.948079143766));
#58822=CARTESIAN_POINT('Ctrl Pts',(-5.03646367327922,0.962759156059136,
29.0872526011881));
#58823=CARTESIAN_POINT('Ctrl Pts',(-4.88197476580226,-1.56818172126413,
29.22642605861));
#58824=CARTESIAN_POINT('Ctrl Pts',(-3.5336719345399,-3.71564720928695,29.3655995160319));
#58825=CARTESIAN_POINT('Ctrl Pts',(-1.3212624743179,-4.95450673617428,29.5047729734539));
#58826=CARTESIAN_POINT('Ctrl Pts',(1.21424196580137,-4.98181573056689,29.6439464308758));
#58827=CARTESIAN_POINT('Ctrl Pts',(3.45282169099331,-3.79089618626559,29.7831198882978));
#58828=CARTESIAN_POINT('Ctrl Pts',(4.84706550524806,-1.67296966878402,29.9222933457197));
#58829=CARTESIAN_POINT('Ctrl Pts',(5.05603193335185,0.854056563561975,30.0614668031417));
#58830=CARTESIAN_POINT('Ctrl Pts',(4.02862136020189,3.17223603487539,30.2006402605636));
#58831=CARTESIAN_POINT('Ctrl Pts',(2.01607167753466,4.71469262156925,30.3398137179856));
#58832=CARTESIAN_POINT('Ctrl Pts',(-0.48947818547963,5.10424163130788,30.4789871754075));
#58833=CARTESIAN_POINT('Ctrl Pts',(-2.87533347790578,4.24562467908683,30.6181606328295));
#58834=CARTESIAN_POINT('Ctrl Pts',(-4.55806896612991,2.34880370078906,30.7573340902515));
#58835=CARTESIAN_POINT('Ctrl Pts',(-5.12619685018181,-0.122382098458352,
30.8965075476734));
#58836=CARTESIAN_POINT('Ctrl Pts',(-4.44078995181737,-2.56364118563321,
31.0356810050954));
#58837=CARTESIAN_POINT('Ctrl Pts',(-2.66945427843709,-4.37800015762571,
31.1748544625173));
#58838=CARTESIAN_POINT('Ctrl Pts',(-0.245343480361355,-5.12178465981157,
31.3140279199393));
#58839=CARTESIAN_POINT('Ctrl Pts',(2.23876239696327,-4.61311331475612,31.4532013773612));
#58840=CARTESIAN_POINT('Ctrl Pts',(4.17541240862802,-2.97637409320671,31.5923748347831));
#58841=CARTESIAN_POINT('Ctrl Pts',(5.09102775500046,-0.611807095947689,
31.7315482922051));
#58842=CARTESIAN_POINT('Ctrl Pts',(4.7617083952635,1.90236817764437,31.8707217496271));
#58843=CARTESIAN_POINT('Ctrl Pts',(3.26798445418964,3.95134776146213,32.009895207049));
#58844=CARTESIAN_POINT('Ctrl Pts',(0.975123784377534,5.03408433878279,32.149068664471));
#58845=CARTESIAN_POINT('Ctrl Pts',(-1.5561888248749,4.8858108708966,32.2882421218929));
#58846=CARTESIAN_POINT('Ctrl Pts',(-3.70695872829678,3.5427854170894,32.4274155793149));
#58847=CARTESIAN_POINT('Ctrl Pts',(-4.95124730868146,1.33342476844834,32.5665890367368));
#58848=CARTESIAN_POINT('Ctrl Pts',(-4.98478240082323,-1.20200496724427,
32.7057624941588));
#58849=CARTESIAN_POINT('Ctrl Pts',(-3.79936349942357,-3.44350236301427,
32.8449359515807));
#58850=CARTESIAN_POINT('Ctrl Pts',(-1.68486707003129,-4.84294275014284,
32.9841094090027));
#58851=CARTESIAN_POINT('Ctrl Pts',(0.841638405786343,-5.05811390922963,
33.1232828664246));
#58852=CARTESIAN_POINT('Ctrl Pts',(3.16233379535394,-4.03639895099572,33.2624563238466));
#58853=CARTESIAN_POINT('Ctrl Pts',(4.70972774489857,-2.02764298972218,33.4016297812685));
#58854=CARTESIAN_POINT('Ctrl Pts',(5.10542820383288,0.476942743256107,33.5408032386905));
#58855=CARTESIAN_POINT('Ctrl Pts',(4.25267254224057,2.86489926058667,33.6799766961124));
#58856=CARTESIAN_POINT('Ctrl Pts',(2.35998940503126,4.55228750552699,33.8191501535344));
#58857=CARTESIAN_POINT('Ctrl Pts',(-0.109793849828778,5.12648191602942,
33.9583236109563));
#58858=CARTESIAN_POINT('Ctrl Pts',(-2.55272866057358,4.44707183552539,34.0974970683783));
#58859=CARTESIAN_POINT('Ctrl Pts',(-4.37143185095318,2.68019683928419,34.2366705258002));
#58860=CARTESIAN_POINT('Ctrl Pts',(-5.12116675270024,0.257919785736935,
34.3758439832222));
#58861=CARTESIAN_POINT('Ctrl Pts',(-4.61859690714988,-2.22742769447237,
34.5150174406442));
#58862=CARTESIAN_POINT('Ctrl Pts',(-2.98661825458746,-4.16809104101649,
34.6541908980661));
#58863=CARTESIAN_POINT('Ctrl Pts',(-0.624306769841251,-5.08951005323373,
34.7933643554881));
#58864=CARTESIAN_POINT('Ctrl Pts',(1.89066959956818,-4.76636549061291,34.93253781291));
#58865=CARTESIAN_POINT('Ctrl Pts',(3.94331099153097,-3.27767752362979,35.071711270332));
#58866=CARTESIAN_POINT('Ctrl Pts',(5.03167464890124,-0.987482532727304,
35.2108847277539));
#58867=CARTESIAN_POINT('Ctrl Pts',(4.88961751469062,1.54418654471136,35.3500581851759));
#58868=CARTESIAN_POINT('Ctrl Pts',(3.55187753674385,3.69824789445101,35.4892316425978));
#58869=CARTESIAN_POINT('Ctrl Pts',(1.34557902206557,4.94795802530842,35.6284051000198));
#58870=CARTESIAN_POINT('Ctrl Pts',(-1.18976072063133,4.98771901298376,35.7675785574417));
#58871=CARTESIAN_POINT('Ctrl Pts',(-3.43416227081397,3.807807902528,35.9067520148637));
#58872=CARTESIAN_POINT('Ctrl Pts',(-4.83879079223079,1.69675431157828,36.0459254722857));
#58873=CARTESIAN_POINT('Ctrl Pts',(-5.0601653848247,-0.829215172954957,
36.1850989297076));
#58874=CARTESIAN_POINT('Ctrl Pts',(-4.04415220241896,-3.15241248704969,
36.3242723871296));
#58875=CARTESIAN_POINT('Ctrl Pts',(-2.0392020752804,-4.70473446870373,36.4634458445515));
#58876=CARTESIAN_POINT('Ctrl Pts',(0.464404425081292,-5.10658399077132,
36.6026193019735));
#58877=CARTESIAN_POINT('Ctrl Pts',(2.85444776800653,-4.25969476190013,36.7417927593954));
#58878=CARTESIAN_POINT('Ctrl Pts',(4.54647859476008,-2.3711608786047,36.8809662168174));
#58879=CARTESIAN_POINT('Ctrl Pts',(5.12673606933716,0.0972049391453199,
37.0201396742393));
#58880=CARTESIAN_POINT('Ctrl Pts',(4.45332690351699,2.5418007426328,37.1593131316613));
#58881=CARTESIAN_POINT('Ctrl Pts',(2.69092323862078,4.3648371846711,37.2984865890832));
#58882=CARTESIAN_POINT('Ctrl Pts',(0.270494535863632,5.12051796509932,37.4376600465052));
#58883=CARTESIAN_POINT('Ctrl Pts',(-2.21607956065588,4.62405264953592,37.576833503927));
#58884=CARTESIAN_POINT('Ctrl Pts',(-4.16074453993469,2.9968444067453,37.7160069613491));
#58885=CARTESIAN_POINT('Ctrl Pts',(-5.08796166186641,0.636802679182853,
37.855180418771));
#58886=CARTESIAN_POINT('Ctrl Pts',(-4.77099384491424,-1.87895962080811,
37.994353876193));
#58887=CARTESIAN_POINT('Ctrl Pts',(-3.28735082876793,-3.93525044354685,
38.1335273336149));
#58888=CARTESIAN_POINT('Ctrl Pts',(-0.999835326585605,-5.02923461816492,
38.2727007910369));
#58889=CARTESIAN_POINT('Ctrl Pts',(1.53217495314691,-4.89339467423037,38.4118742484588));
#58890=CARTESIAN_POINT('Ctrl Pts',(3.68951476027582,-3.56094823867799,38.5510477058808));
#58891=CARTESIAN_POINT('Ctrl Pts',(4.94463890588947,-1.35772516187962,38.6902211633027));
#58892=CARTESIAN_POINT('Ctrl Pts',(4.99062554934078,1.17750929979514,38.8293946207247));
#58893=CARTESIAN_POINT('Ctrl Pts',(3.81622934465927,3.42480147071306,38.9685680781466));
#58894=CARTESIAN_POINT('Ctrl Pts',(1.70863132174512,4.83460965654813,39.1077415355686));
#58895=CARTESIAN_POINT('Ctrl Pts',(-0.81678693997971,5.06218634776669,39.2469149929905));
#58896=CARTESIAN_POINT('Ctrl Pts',(-3.14247216978798,4.05188106771966,39.3860884504125));
#58897=CARTESIAN_POINT('Ctrl Pts',(-4.69971282309411,2.0507488645082,39.5252619078343));
#58898=CARTESIAN_POINT('Ctrl Pts',(-5.10770898515378,-0.451863306561025,
39.6644353652565));
#58899=CARTESIAN_POINT('Ctrl Pts',(-4.26669129572166,-2.84397906318768,
39.8036088226782));
#58900=CARTESIAN_POINT('Ctrl Pts',(-2.3823180541456,-4.54064226885678,39.9427822801004));
#58901=CARTESIAN_POINT('Ctrl Pts',(0.0846154423188459,-5.12695930857248,
40.0819557375222));
#58902=CARTESIAN_POINT('Ctrl Pts',(2.53085749770598,-4.45955511807427,40.2211291949443));
#58903=CARTESIAN_POINT('Ctrl Pts',(4.35821619854518,-2.70163341176691,40.3603026523661));
#58904=CARTESIAN_POINT('Ctrl Pts',(5.11983830092096,-0.283067654915984,
40.4994761097881));
#58905=CARTESIAN_POINT('Ctrl Pts',(4.62948050901625,2.20471806394278,40.6386495672101));
#58906=CARTESIAN_POINT('Ctrl Pts',(3.00705248801675,4.15337294968188,40.7778230246319));
#58907=CARTESIAN_POINT('Ctrl Pts',(0.649294748622445,5.08638259023525,40.916996482054));
#58908=CARTESIAN_POINT('Ctrl Pts',(-1.86723831197507,4.77559343025863,41.0561699394759));
#58909=CARTESIAN_POINT('Ctrl Pts',(-3.92716616611468,3.29700431127425,41.1953433968979));
#58910=CARTESIAN_POINT('Ctrl Pts',(-5.02676426128715,1.01218209146538,41.3345168543198));
#58911=CARTESIAN_POINT('Ctrl Pts',(-4.89714232673967,-1.52015412261115,
41.4736903117417));
#58912=CARTESIAN_POINT('Ctrl Pts',(-3.56999746819571,-3.68075937843173,
41.6128637691637));
#58913=CARTESIAN_POINT('Ctrl Pts',(-1.36986311464964,-4.94128997043882,
41.7520372265857));
#58914=CARTESIAN_POINT('Ctrl Pts',(1.16525077861143,-4.99350199236792,41.8912106840076));
#58915=CARTESIAN_POINT('Ctrl Pts',(3.4154200191569,-3.82462777503633,42.0303841414296));
#58916=CARTESIAN_POINT('Ctrl Pts',(4.83039936830708,-1.72049802891365,42.1695575988515));
#58917=CARTESIAN_POINT('Ctrl Pts',(5.06417678586922,0.804353781802734,42.3087310562735));
#58918=CARTESIAN_POINT('Ctrl Pts',(4.05958550029279,3.13251290350884,42.4479045136954));
#58919=CARTESIAN_POINT('Ctrl Pts',(2.06228328777852,4.69466283835021,42.5870779711175));
#58920=CARTESIAN_POINT('Ctrl Pts',(-0.439319463318189,5.10880318019658,
42.7262514285393));
#58921=CARTESIAN_POINT('Ctrl Pts',(-2.83349320925637,4.2736621015161,42.8654248859613));
#58922=CARTESIAN_POINT('Ctrl Pts',(-4.53477856301013,2.39346086437625,43.0045983433833));
#58923=CARTESIAN_POINT('Ctrl Pts',(-5.12715163238927,-0.0720254352639578,
43.1437718008051));
#58924=CARTESIAN_POINT('Ctrl Pts',(-4.4657564416411,-2.51989899178081,43.2829452582272));
#58925=CARTESIAN_POINT('Ctrl Pts',(-2.71232729414031,-4.35156893249991,
43.4221187156491));
#58926=CARTESIAN_POINT('Ctrl Pts',(-0.29563906707815,-5.11912776426357,
43.5612921730711));
#58927=CARTESIAN_POINT('Ctrl Pts',(2.19334327284283,-4.63488045286089,43.700465630493));
#58928=CARTESIAN_POINT('Ctrl Pts',(4.14597631470871,-3.01724243684715,43.8396390879149));
#58929=CARTESIAN_POINT('Ctrl Pts',(5.08477284786202,-0.661782902832914,
43.978812545337));
#58930=CARTESIAN_POINT('Ctrl Pts',(4.78016421891062,1.85550574374848,44.1179860027588));
#58931=CARTESIAN_POINT('Ctrl Pts',(3.30663791293829,3.91905820798263,44.2571594601809));
#58932=CARTESIAN_POINT('Ctrl Pts',(1.0245227529157,5.02426359316417,44.3963329176028));
#58933=CARTESIAN_POINT('Ctrl Pts',(-1.50812412558962,4.90086044962019,44.5355063750247));
#58934=CARTESIAN_POINT('Ctrl Pts',(-3.67198180171369,3.57902517073021,44.6746798324467));
#58935=CARTESIAN_POINT('Ctrl Pts',(-4.93791123915052,1.38199280718384,44.8138532898685));
#58936=CARTESIAN_POINT('Ctrl Pts',(-4.99634832472027,-1.15298523099901,
44.9530267472907));
#58937=CARTESIAN_POINT('Ctrl Pts',(-3.83300314301673,-3.40601797271547,
45.0922002047124));
#58938=CARTESIAN_POINT('Ctrl Pts',(-1.73235436152806,-4.82615995289543,
45.2313736621346));
#58939=CARTESIAN_POINT('Ctrl Pts',(0.791915773395165,-5.06613668713003,
45.3705471195564));
#58940=CARTESIAN_POINT('Ctrl Pts',(3.12253474826594,-4.06726545368122,45.5097205769784));
#58941=CARTESIAN_POINT('Ctrl Pts',(4.68958454492302,-2.07380527553964,45.6488940344003));
#58942=CARTESIAN_POINT('Ctrl Pts',(5.10986656930181,0.426772970991213,45.7880674918224));
#58943=CARTESIAN_POINT('Ctrl Pts',(4.28060713724999,2.82299026944149,45.9272409492442));
#58944=CARTESIAN_POINT('Ctrl Pts',(2.40458924210636,4.52888751257782,46.0664144066663));
#58945=CARTESIAN_POINT('Ctrl Pts',(-0.0594349938974569,5.12731303962781,
46.205587864088));
#58946=CARTESIAN_POINT('Ctrl Pts',(-2.50892529093627,4.47193083682398,46.3447613215102));
#58947=CARTESIAN_POINT('Ctrl Pts',(-4.34489542661782,2.72300482125766,46.4839347789319));
#58948=CARTESIAN_POINT('Ctrl Pts',(-5.1183863594116,0.308208696545455,46.6231082363541));
#58949=CARTESIAN_POINT('Ctrl Pts',(-4.64025244850859,-2.18195525594519,
46.7622816937759));
#58950=CARTESIAN_POINT('Ctrl Pts',(-3.02741419179187,-4.13855467961632,
46.901455151198));
#58951=CARTESIAN_POINT('Ctrl Pts',(-0.674267066511626,-5.08313244445339,
47.0406286086197));
#58952=CARTESIAN_POINT('Ctrl Pts',(1.84376198687486,-4.78470618330867,47.179802066042));
#58953=CARTESIAN_POINT('Ctrl Pts',(3.91092661804106,-3.31625157567016,47.3189755234636));
#58954=CARTESIAN_POINT('Ctrl Pts',(5.02173262887484,-1.03685723652329,47.4581489808859));
#58955=CARTESIAN_POINT('Ctrl Pts',(4.90454902045194,1.49608503462231,47.5973224383075));
#58956=CARTESIAN_POINT('Ctrl Pts',(3.58803129184512,3.66318208304981,47.7364958957298));
#58957=CARTESIAN_POINT('Ctrl Pts',(1.39411416634107,4.93450273239808,47.8756693531515));
#58958=CARTESIAN_POINT('Ctrl Pts',(-1.14071273091822,4.99916452923466,48.0148428105736));
#58959=CARTESIAN_POINT('Ctrl Pts',(-3.39659538808254,3.84135539809756,48.1540162679954));
#58960=CARTESIAN_POINT('Ctrl Pts',(-4.82189143587676,1.74420024809519,48.2931897254175));
#58961=CARTESIAN_POINT('Ctrl Pts',(-5.068066039731,-0.779472989758009,48.4323631828393));
#58962=CARTESIAN_POINT('Ctrl Pts',(-4.07492088157485,-3.11253776422747,
48.5715366402614));
#58963=CARTESIAN_POINT('Ctrl Pts',(-2.08531475831404,-4.68447797343466,
48.7107100976832));
#58964=CARTESIAN_POINT('Ctrl Pts',(0.414223905235385,-5.11089914605722,
48.8498835551053));
#58965=CARTESIAN_POINT('Ctrl Pts',(2.81247030707573,-4.28752636104482,48.9890570125271));
#58966=CARTESIAN_POINT('Ctrl Pts',(4.52296915308285,-2.41570312023185,49.1282304699492));
#58967=CARTESIAN_POINT('Ctrl Pts',(5.12744352931481,0.0468441941396368,
49.2674039273711));
#58968=CARTESIAN_POINT('Ctrl Pts',(4.47807826639135,2.49793646134371,49.4065773847931));
#58969=CARTESIAN_POINT('Ctrl Pts',(2.73366592873352,4.33819572114011,49.545750842215));
#58970=CARTESIAN_POINT('Ctrl Pts',(0.320776467523109,5.11761409083573,49.6849242996369));
#58971=CARTESIAN_POINT('Ctrl Pts',(-2.17055408191953,4.64559646356626,49.8240977570589));
#58972=CARTESIAN_POINT('Ctrl Pts',(-4.13110808915714,3.03756769151527,49.9632712144808));
#58973=CARTESIAN_POINT('Ctrl Pts',(-5.08146138990095,0.686747164379139,
50.1024446719028));
#58974=CARTESIAN_POINT('Ctrl Pts',(-4.78921929606477,-1.83200711216899,
50.2416181293247));
#58975=CARTESIAN_POINT('Ctrl Pts',(-3.32584524149952,-3.90277144532342,
50.3807915867467));
#58976=CARTESIAN_POINT('Ctrl Pts',(-1.0491854679113,-5.01917138368084,50.5199650441687));
#58977=CARTESIAN_POINT('Ctrl Pts',(1.48403692230487,-4.90820801699284,50.6591385015906));
#58978=CARTESIAN_POINT('Ctrl Pts',(3.65436027550235,-3.59701577723358,50.7983119590126));
#58979=CARTESIAN_POINT('Ctrl Pts',(4.93106447073476,-1.40622711902959,50.9374854164345));
#58980=CARTESIAN_POINT('Ctrl Pts',(5.00195058892939,1.12843335237216,51.0766588738565));
#58981=CARTESIAN_POINT('Ctrl Pts',(3.8496844899148,3.38715232207621,51.2158323312784));
#58982=CARTESIAN_POINT('Ctrl Pts',(1.75603561718453,4.81759384299012,51.3550057887004));
#58983=CARTESIAN_POINT('Ctrl Pts',(-0.767025505920936,5.06996483203814,
51.4941792461224));
#58984=CARTESIAN_POINT('Ctrl Pts',(-3.10252201167498,4.08255173781169,51.6333527035442));
#58985=CARTESIAN_POINT('Ctrl Pts',(-4.67934315467761,2.09681166669986,51.7725261609663));
#58986=CARTESIAN_POINT('Ctrl Pts',(-5.11190090423642,-0.401672341721206,
51.9116996183881));
#58987=CARTESIAN_POINT('Ctrl Pts',(-4.29441973117786,-2.80193338559416,
52.0508730758102));
#58988=CARTESIAN_POINT('Ctrl Pts',(-2.42680243173636,-4.51702352021277,
52.190046533232));
#58989=CARTESIAN_POINT('Ctrl Pts',(0.0342531119126611,-5.12754310066344,
52.3292199906541));
#58990=CARTESIAN_POINT('Ctrl Pts',(2.48693256926547,-4.48419869327436,52.468393448076));
#58991=CARTESIAN_POINT('Ctrl Pts',(4.33146985646582,-2.74431055228173,52.6075669054979));
#58992=CARTESIAN_POINT('Ctrl Pts',(5.1168109631927,-0.333342304227799,52.7467403629199));
#58993=CARTESIAN_POINT('Ctrl Pts',(4.65091246580963,2.15913981951461,52.8859138203419));
#58994=CARTESIAN_POINT('Ctrl Pts',(3.04770287479204,4.12363658823389,53.0250872777638));
#58995=CARTESIAN_POINT('Ctrl Pts',(0.699223121180822,5.07975969428112,53.1642607351858));
#58996=CARTESIAN_POINT('Ctrl Pts',(-1.82024119051244,4.79370352996499,53.3034341926077));
#58997=CARTESIAN_POINT('Ctrl Pts',(-3.89459273900518,3.33541885257685,53.4426076500297));
#58998=CARTESIAN_POINT('Ctrl Pts',(-5.01657987302642,1.06150737274083,53.5817811074516));
#58999=CARTESIAN_POINT('Ctrl Pts',(-4.91183741717926,-1.47197986128708,
53.7209545648736));
#59000=CARTESIAN_POINT('Ctrl Pts',(-3.6059785727194,-3.64551643226655,53.8601280222955));
#59001=CARTESIAN_POINT('Ctrl Pts',(-1.41833159220866,-4.92759647489319,
53.9993014797174));
#59002=CARTESIAN_POINT('Ctrl Pts',(1.11614716940514,-5.00470648700459,54.1384749371395));
#59003=CARTESIAN_POINT('Ctrl Pts',(3.3776888316379,-3.85799036824427,54.2776483945613));
#59004=CARTESIAN_POINT('Ctrl Pts',(4.81326720014988,-1.76786039742912,54.4168218519834));
#59005=CARTESIAN_POINT('Ctrl Pts',(5.07183305260184,0.754573396941915,54.5559953094052));
#59006=CARTESIAN_POINT('Ctrl Pts',(4.09015797637785,3.09248755100316,54.6951687668272));
#59007=CARTESIAN_POINT('Ctrl Pts',(2.10829593137106,4.6741801196147,54.8343422242492));
#59008=CARTESIAN_POINT('Ctrl Pts',(-0.389118356134408,5.11287183779883,
54.9735156816711));
#59009=CARTESIAN_POINT('Ctrl Pts',(-2.79137956853432,4.30128720608217,55.1126891390931));
#59010=CARTESIAN_POINT('Ctrl Pts',(-4.51105064981971,2.4378871096911,55.2518625965151));
#59011=CARTESIAN_POINT('Ctrl Pts',(-5.12761175307327,-0.0216618231406892,
55.391036053937));
#59012=CARTESIAN_POINT('Ctrl Pts',(-4.4902920805669,-2.47591368105495,55.530209511359));
#59013=CARTESIAN_POINT('Ctrl Pts',(-2.75493862771526,-4.32471787315188,
55.6693829687808));
#59014=CARTESIAN_POINT('Ctrl Pts',(-0.345906130887604,-5.11597698132539,
55.808556426203));
#59015=CARTESIAN_POINT('Ctrl Pts',(2.14771253755835,-4.65620042318322,55.9477298836247));
#59016=CARTESIAN_POINT('Ctrl Pts',(4.11614022189969,-3.05781968050709,56.0869033410469));
#59017=CARTESIAN_POINT('Ctrl Pts',(5.07802736785512,-0.711694861686717,
56.2260767984686));
#59018=CARTESIAN_POINT('Ctrl Pts',(4.79815885796941,1.80846429285365,56.3652502558907));
#59019=CARTESIAN_POINT('Ctrl Pts',(3.34497235117331,3.88639054840388,56.5044237133125));
#59020=CARTESIAN_POINT('Ctrl Pts',(1.07382287671086,5.01395811253837,56.6435971707346));
#59021=CARTESIAN_POINT('Ctrl Pts',(-1.45991392427294,4.91543719912591,56.7827706281565));
#59022=CARTESIAN_POINT('Ctrl Pts',(-3.63665060667076,3.61491962425697,56.9219440855785));
#59023=CARTESIAN_POINT('Ctrl Pts',(-4.92409876578536,1.43042751288836,57.0611175430004));
#59024=CARTESIAN_POINT('Ctrl Pts',(-5.00743220684222,-1.10385425610278,
57.2002910004224));
#59025=CARTESIAN_POINT('Ctrl Pts',(-3.86627298300154,-3.36820497383239,
57.3394644578443));
#59026=CARTESIAN_POINT('Ctrl Pts',(-1.77967451752562,-4.80891153344568,
57.4786379152663));
#59027=CARTESIAN_POINT('Ctrl Pts',(0.742116737907104,-5.07367069015669,
57.6178113726882));
#59028=CARTESIAN_POINT('Ctrl Pts',(3.08243444271975,-4.09773955140781,57.7569848301102));
#59029=CARTESIAN_POINT('Ctrl Pts',(4.66898889937891,-2.11976748307766,57.8961582875321));
#59030=CARTESIAN_POINT('Ctrl Pts',(5.1138119408897,0.376562024175001,58.0353317449541));
#59031=CARTESIAN_POINT('Ctrl Pts',(4.30812874434728,2.78080891953505,58.1745052023761));
#59032=CARTESIAN_POINT('Ctrl Pts',(2.4489570872563,4.50505057791964,58.313678659798));
#59033=CARTESIAN_POINT('Ctrl Pts',(-0.00907040374824587,5.12764948613034,
58.45285211722));
#59034=CARTESIAN_POINT('Ctrl Pts',(-2.46487986315524,4.49635839152627,58.5920255746418));
#59035=CARTESIAN_POINT('Ctrl Pts',(-4.31793981191222,2.76555009094761,58.7311990320639));
#59036=CARTESIAN_POINT('Ctrl Pts',(-5.11511215026264,0.358467871743584,
58.8703724894858));
#59037=CARTESIAN_POINT('Ctrl Pts',(-4.66146030380106,-2.13627230495643,
59.0095459469077));
#59038=CARTESIAN_POINT('Ctrl Pts',(-3.06791804765684,-4.10861903535706,
59.1487194043298));
#59039=CARTESIAN_POINT('Ctrl Pts',(-0.724162310693165,-5.07626442106874,
59.2878928617516));
#59040=CARTESIAN_POINT('Ctrl Pts',(1.79667649020643,-4.80258525321274,59.4270663191736));
#59041=CARTESIAN_POINT('Ctrl Pts',(3.87816492297812,-3.35450567968201,59.5662397765956));
#59042=CARTESIAN_POINT('Ctrl Pts',(5.01130611802573,-1.08613190555986,59.7054132340175));
#59043=CARTESIAN_POINT('Ctrl Pts',(4.91900734112638,1.44783918401923,59.8445866914394));
#59044=CARTESIAN_POINT('Ctrl Pts',(3.6238388779325,3.62776285217508,59.9837601488615));
#59045=CARTESIAN_POINT('Ctrl Pts',(1.44251480813104,4.92057136450247,60.1229336062833));
#59046=CARTESIAN_POINT('Ctrl Pts',(-1.09155468659011,5.01012773200588,60.2621070637055));
#59047=CARTESIAN_POINT('Ctrl Pts',(-3.35870080584726,3.87453228424406,60.4012805211271));
#59048=CARTESIAN_POINT('Ctrl Pts',(-4.80452686914066,1.79147790623387,60.5404539785494));
#59049=CARTESIAN_POINT('Ctrl Pts',(-5.07547773362422,-0.729655603925534,
60.6796274359711));
#59050=CARTESIAN_POINT('Ctrl Pts',(-4.10529641718065,-3.07236274745144,
60.8188008933932));
#59051=CARTESIAN_POINT('Ctrl Pts',(-2.13122625265585,-4.663769525259,60.957974350815));
#59052=CARTESIAN_POINT('Ctrl Pts',(0.364003421574487,-5.11472120786763,
61.0971478082371));
#59053=CARTESIAN_POINT('Ctrl Pts',(2.77022150230343,-4.31494430466559,61.236321265659));
#59054=CARTESIAN_POINT('Ctrl Pts',(4.49902334075878,-2.46001229778389,61.375494723081));
#59055=CARTESIAN_POINT('Ctrl Pts',(5.12765629947872,-0.00352107013592945,
61.5146681805029));
#59056=CARTESIAN_POINT('Ctrl Pts',(4.50239758982308,2.45383118170519,61.6538416379248));
#59057=CARTESIAN_POINT('Ctrl Pts',(2.77614487750337,4.31113571438885,61.7930150953468));
#59058=CARTESIAN_POINT('Ctrl Pts',(0.371027452000867,5.11421647371715,61.9321885527688));
#59059=CARTESIAN_POINT('Ctrl Pts',(-2.12481919255064,4.6666920788757,62.0713620101907));
#59060=CARTESIAN_POINT('Ctrl Pts',(-4.10107307033674,3.0779979096349,62.2105354676127));
#59061=CARTESIAN_POINT('Ctrl Pts',(-5.07447087161606,0.736625404163389,
62.3497089250346));
#59062=CARTESIAN_POINT('Ctrl Pts',(-4.80698267522873,-1.78487787537981,
62.4888823824566));
#59063=CARTESIAN_POINT('Ctrl Pts',(-3.36401880748098,-3.86991586995366,
62.6280558398784));
#59064=CARTESIAN_POINT('Ctrl Pts',(-1.09843433267496,-5.00862398811822,
62.7672292973006));
#59065=CARTESIAN_POINT('Ctrl Pts',(1.4357556111677,-4.92254766049344,62.9064027547223));
#59066=CARTESIAN_POINT('Ctrl Pts',(3.61885342162015,-3.63273659425221,63.0455762121445));
#59067=CARTESIAN_POINT('Ctrl Pts',(4.91701390374655,-1.45459279213023,63.1847496695662));
#59068=CARTESIAN_POINT('Ctrl Pts',(5.01279380401881,1.07924733972977,63.3239231269884));
#59069=CARTESIAN_POINT('Ctrl Pts',(3.88276674436703,3.34917871604949,63.4630965844101));
#59070=CARTESIAN_POINT('Ctrl Pts',(1.80327337436161,4.80010868768094,63.6022700418323));
#59071=CARTESIAN_POINT('Ctrl Pts',(-0.717195690581678,5.07726303778206,
63.741443499254));
#59072=CARTESIAN_POINT('Ctrl Pts',(-3.06226156438238,4.1128112366359,63.8806169566761));
#59073=CARTESIAN_POINT('Ctrl Pts',(-4.65854341282239,2.14270591183768,64.019790414098));
#59074=CARTESIAN_POINT('Ctrl Pts',(-5.11555785592785,-0.351508627023642,
64.15896387152));
#59075=CARTESIAN_POINT('Ctrl Pts',(-4.3218160990318,-2.75948654582595,64.2981373289419));
#59076=CARTESIAN_POINT('Ctrl Pts',(-2.47088410596534,-4.49324627465512,
64.437310786364));
#59077=CARTESIAN_POINT('Ctrl Pts',(-0.834646007515407,-4.91565157897533,
64.5300930913119));
#59078=CARTESIAN_POINT('Ctrl Pts',(-0.0154545066754591,-4.91822571876519,
64.5764842437858));
#59079=CARTESIAN_POINT('Ctrl Pts',(2.58415070483638,5.32291852118006,2.35922392732846E-16));
#59080=CARTESIAN_POINT('Ctrl Pts',(2.70511861947279,5.25165405591466,2.59308817902277E-16));
#59081=CARTESIAN_POINT('Ctrl Pts',(2.82328939759037,5.1761837259702,2.60954157596921E-16));
#59082=CARTESIAN_POINT('Ctrl Pts',(2.93842118606223,5.09659358068734,2.98372437868011E-16));
#59083=CARTESIAN_POINT('Ctrl Pts',(3.07402653614829,5.00285014407668,2.98974997602692E-16));
#59084=CARTESIAN_POINT('Ctrl Pts',(3.20541718868923,4.90339199696324,5.80189110088706E-16));
#59085=CARTESIAN_POINT('Ctrl Pts',(3.33231171324647,4.79857206961274,4.71844785465692E-16));
#59086=CARTESIAN_POINT('Ctrl Pts',(3.45942568888835,4.69357086693276,3.63313090429043E-16));
#59087=CARTESIAN_POINT('Ctrl Pts',(3.58202843978269,4.58318869192379,3.87064081949451E-16));
#59088=CARTESIAN_POINT('Ctrl Pts',(3.69979700370316,4.46774699683153,4.44089209850063E-16));
#59089=CARTESIAN_POINT('Ctrl Pts',(3.81278208592582,4.35699427150552,4.98798111360991E-16));
#59090=CARTESIAN_POINT('Ctrl Pts',(3.92131782119956,4.24158400211618,-1.6541059630567E-16));
#59091=CARTESIAN_POINT('Ctrl Pts',(4.02507848003065,4.12177931674072,-3.33066907387547E-16));
#59092=CARTESIAN_POINT('Ctrl Pts',(4.10629751893176,4.02800175680941,-4.64300504062582E-16));
#59093=CARTESIAN_POINT('Ctrl Pts',(4.18459012464176,3.93153124615902,4.15462027952972E-16));
#59094=CARTESIAN_POINT('Ctrl Pts',(4.25978084755203,3.83248837704811,5.27355936696949E-16));
#59095=CARTESIAN_POINT('Ctrl Pts',(4.27272403323478,3.81543932902945,5.46617137834363E-16));
#59096=CARTESIAN_POINT('Ctrl Pts',(4.28556975141914,3.79832128448063,-6.44283739800603E-17));
#59097=CARTESIAN_POINT('Ctrl Pts',(4.29831497568012,3.78113823514667,-5.55111512312578E-17));
#59098=CARTESIAN_POINT('Ctrl Pts',(4.39680707821293,3.64835166174689,1.33990538227478E-17));
#59099=CARTESIAN_POINT('Ctrl Pts',(4.48934874550704,3.51162388599325,2.0715226758615E-16));
#59100=CARTESIAN_POINT('Ctrl Pts',(4.57564112442567,3.37129841337389,1.94289029309402E-16));
#59101=CARTESIAN_POINT('Ctrl Pts',(4.66193350334431,3.23097294075453,1.81425791032655E-16));
#59102=CARTESIAN_POINT('Ctrl Pts',(4.74197706027285,3.08704906877042,-2.38966041326046E-16));
#59103=CARTESIAN_POINT('Ctrl Pts',(4.81542054559223,2.93984529382198,-2.77555756156289E-16));
#59104=CARTESIAN_POINT('Ctrl Pts',(4.88716990501125,2.79603707842097,-3.42113286361595E-16));
#59105=CARTESIAN_POINT('Ctrl Pts',(4.95261996588971,2.64909759657784,-3.28762512571199E-17));
#59106=CARTESIAN_POINT('Ctrl Pts',(5.01163872074466,2.49946141477762,2.22044604925031E-16));
#59107=CARTESIAN_POINT('Ctrl Pts',(5.07015933458441,2.35108821996683,4.74813830927776E-16));
#59108=CARTESIAN_POINT('Ctrl Pts',(5.12235677838181,2.200062894578,5.77849218589554E-17));
#59109=CARTESIAN_POINT('Ctrl Pts',(5.16805141111303,2.0468094574673,1.38777878078145E-16));
#59110=CARTESIAN_POINT('Ctrl Pts',(5.18023517309137,2.0059468158721,1.60373388130753E-16));
#59111=CARTESIAN_POINT('Ctrl Pts',(5.19195634089117,1.96492580600586,-4.18469453909966E-16));
#59112=CARTESIAN_POINT('Ctrl Pts',(5.20321088585858,1.92375457558523,-4.16333634234434E-16));
#59113=CARTESIAN_POINT('Ctrl Pts',(5.20842035550966,1.90469736127804,-4.15345012498763E-16));
#59114=CARTESIAN_POINT('Ctrl Pts',(5.21353051364629,1.88560539766239,4.06076581793497E-17));
#59115=CARTESIAN_POINT('Ctrl Pts',(5.21853870347985,1.86648807919458,2.77555756156289E-17));
#59116=CARTESIAN_POINT('Ctrl Pts',(5.25844125851643,1.71417159805777,-7.46428854803789E-17));
#59117=CARTESIAN_POINT('Ctrl Pts',(5.29180961247242,1.56050412240968,-2.4180069860195E-16));
#59118=CARTESIAN_POINT('Ctrl Pts',(5.31857341141684,1.40590440312336,-1.66533453693773E-16));
#59119=CARTESIAN_POINT('Ctrl Pts',(5.34526406646942,1.25172719579692,-9.14719097487536E-17));
#59120=CARTESIAN_POINT('Ctrl Pts',(5.36538625816212,1.09662206745273,-1.14443556055179E-15));
#59121=CARTESIAN_POINT('Ctrl Pts',(5.37881871749598,0.941000624308486,-9.43689570931383E-16));
#59122=CARTESIAN_POINT('Ctrl Pts',(5.39204517961296,0.787765757097624,-7.46022177279958E-16));
#59123=CARTESIAN_POINT('Ctrl Pts',(5.39878545820546,0.634029605395147,-2.06261628158008E-17));
#59124=CARTESIAN_POINT('Ctrl Pts',(5.3988741101366,0.480192238475125,0.));
#59125=CARTESIAN_POINT('Ctrl Pts',(5.398916119146,0.407294160455884,9.7740078128452E-18));
#59126=CARTESIAN_POINT('Ctrl Pts',(5.39746379985764,0.334373522025099,-1.09637651355696E-15));
#59127=CARTESIAN_POINT('Ctrl Pts',(5.39449561700532,0.26147412547058,-1.11022302462516E-15));
#59128=CARTESIAN_POINT('Ctrl Pts',(5.39000601196769,0.151208176808848,-1.12870294857941E-15));
#59129=CARTESIAN_POINT('Ctrl Pts',(5.3820487164881,0.0409904590914841,-5.4025619378067E-16));
#59130=CARTESIAN_POINT('Ctrl Pts',(5.37064145959088,-0.0690162522279109,
-4.9960036108132E-16));
#59131=CARTESIAN_POINT('Ctrl Pts',(5.36710034259144,-0.103165271489568,
-4.86979705511336E-16));
#59132=CARTESIAN_POINT('Ctrl Pts',(5.3632266913415,-0.137293906145545,-8.57200446937436E-16));
#59133=CARTESIAN_POINT('Ctrl Pts',(5.35902082468953,-0.171397139460776,
-8.88178419700125E-16));
#59134=CARTESIAN_POINT('Ctrl Pts',(5.35662614050457,-0.190814415431093,
-9.05816273582604E-16));
#59135=CARTESIAN_POINT('Ctrl Pts',(5.35412341958406,-0.210225943349712,
-1.22843111941016E-15));
#59136=CARTESIAN_POINT('Ctrl Pts',(5.35151382049558,-0.22962257030035,-1.22124532708767E-15));
#59137=CARTESIAN_POINT('Ctrl Pts',(5.33114339416283,-0.381031866136956,
-1.16515331901094E-15));
#59138=CARTESIAN_POINT('Ctrl Pts',(5.30430552073536,-0.531245332604996,
-4.64315052832525E-17));
#59139=CARTESIAN_POINT('Ctrl Pts',(5.27115359261857,-0.679863637652015,
-1.11022302462516E-16));
#59140=CARTESIAN_POINT('Ctrl Pts',(5.23793248804223,-0.828792057034796,
-1.75747878006781E-16));
#59141=CARTESIAN_POINT('Ctrl Pts',(5.19837064736214,-0.976119385505511,
-6.58930197271103E-16));
#59142=CARTESIAN_POINT('Ctrl Pts',(5.15257331214529,-1.12142719841327,-8.32667268468867E-16));
#59143=CARTESIAN_POINT('Ctrl Pts',(5.10717447600833,-1.26547063579635,-1.00489259094399E-15));
#59144=CARTESIAN_POINT('Ctrl Pts',(5.0556478273115,-1.40753020406774,-5.63971542161181E-16));
#59145=CARTESIAN_POINT('Ctrl Pts',(4.99805275028795,-1.54717172655174,-4.44089209850063E-16));
#59146=CARTESIAN_POINT('Ctrl Pts',(4.9480429007657,-1.6684225675503,-3.39995288822692E-16));
#59147=CARTESIAN_POINT('Ctrl Pts',(4.89345700852936,-1.78785018655589,-1.19778754206742E-15));
#59148=CARTESIAN_POINT('Ctrl Pts',(4.8343102366916,-1.90514816028807,-1.22124532708767E-15));
#59149=CARTESIAN_POINT('Ctrl Pts',(4.80473685077273,-1.96379714715416,-1.2329742195978E-15));
#59150=CARTESIAN_POINT('Ctrl Pts',(4.77402291520497,-2.02191336562227,-1.62336207194318E-16));
#59151=CARTESIAN_POINT('Ctrl Pts',(4.74216843424644,-2.0794561600232,-1.11022302462516E-16));
#59152=CARTESIAN_POINT('Ctrl Pts',(4.73104879031827,-2.09954298501978,-9.31098351419854E-17));
#59153=CARTESIAN_POINT('Ctrl Pts',(4.71979015531546,-2.11955992072199,-5.50505449287299E-16));
#59154=CARTESIAN_POINT('Ctrl Pts',(4.70839249529098,-2.13950518784205,-5.55111512312578E-16));
#59155=CARTESIAN_POINT('Ctrl Pts',(4.69713562314994,-2.15920408404594,-5.59660679636204E-16));
#59156=CARTESIAN_POINT('Ctrl Pts',(4.68574729156115,-2.17882575777773,-4.49902034763585E-16));
#59157=CARTESIAN_POINT('Ctrl Pts',(4.67423042538155,-2.19836423113908,-4.44089209850063E-16));
#59158=CARTESIAN_POINT('Ctrl Pts',(4.66400316177994,-2.21571488142219,-4.38927276757024E-16));
#59159=CARTESIAN_POINT('Ctrl Pts',(4.65367388210654,-2.23300106829952,-2.36408244836096E-16));
#59160=CARTESIAN_POINT('Ctrl Pts',(4.64324279625684,-2.25022178954521,-2.22044604925031E-16));
#59161=CARTESIAN_POINT('Ctrl Pts',(4.56566903431785,-2.37828862262268,-1.28577692735215E-16));
#59162=CARTESIAN_POINT('Ctrl Pts',(4.48246793624052,-2.50273777206833,-8.64751003178453E-16));
#59163=CARTESIAN_POINT('Ctrl Pts',(4.39395501715838,-2.62326605186807,-6.66133814775094E-16));
#59164=CARTESIAN_POINT('Ctrl Pts',(4.30552250169377,-2.74368484584573,-4.67697046819005E-16));
#59165=CARTESIAN_POINT('Ctrl Pts',(4.21178716587762,-2.86019038329772,-1.03847678039002E-15));
#59166=CARTESIAN_POINT('Ctrl Pts',(4.11303118505379,-2.97243998135549,-7.21644966006352E-16));
#59167=CARTESIAN_POINT('Ctrl Pts',(4.06811417427852,-3.02349427055824,-5.77540903630545E-16));
#59168=CARTESIAN_POINT('Ctrl Pts',(4.02215816382635,-3.07366754203135,-5.16430948201177E-16));
#59169=CARTESIAN_POINT('Ctrl Pts',(3.97518802543061,-3.12292436790974,-5.55111512312578E-16));
#59170=CARTESIAN_POINT('Ctrl Pts',(3.9540953692043,-3.14504389598732,-5.72481608916671E-16));
#59171=CARTESIAN_POINT('Ctrl Pts',(3.93279819227414,-3.16697858573548,-5.89160445509899E-16));
#59172=CARTESIAN_POINT('Ctrl Pts',(3.91129869242318,-3.18872508690685,-6.66133814775094E-16));
#59173=CARTESIAN_POINT('Ctrl Pts',(3.89425753665478,-3.20596202341459,-7.27145242239012E-16));
#59174=CARTESIAN_POINT('Ctrl Pts',(3.87708874107993,-3.22308115070843,-4.69465644281958E-16));
#59175=CARTESIAN_POINT('Ctrl Pts',(3.85980494844311,-3.24006967703212,-4.44089209850063E-16));
#59176=CARTESIAN_POINT('Ctrl Pts',(3.75513441850311,-3.34295207620028,-2.9040969657491E-16));
#59177=CARTESIAN_POINT('Ctrl Pts',(3.64615041630408,-3.44114871706017,-1.04632860102231E-16));
#59178=CARTESIAN_POINT('Ctrl Pts',(3.53313742783404,-3.53434970143845,0.));
#59179=CARTESIAN_POINT('Ctrl Pts',(3.4219903426573,-3.62601188902845,1.02905317092383E-16));
#59180=CARTESIAN_POINT('Ctrl Pts',(3.30694556827097,-3.71284232949852,-5.47072034414736E-16));
#59181=CARTESIAN_POINT('Ctrl Pts',(3.18825216084998,-3.79450149497552,-5.55111512312578E-16));
#59182=CARTESIAN_POINT('Ctrl Pts',(3.08078920485239,-3.86843428953528,-5.62390316404158E-16));
#59183=CARTESIAN_POINT('Ctrl Pts',(2.97033484176792,-3.93812777284464,5.67746719143187E-17));
#59184=CARTESIAN_POINT('Ctrl Pts',(2.85706463458441,-4.0032942355399,0.));
#59185=CARTESIAN_POINT('Ctrl Pts',(-5.9170192319132,-0.000147776431128344,
63.5633751922049));
#59186=CARTESIAN_POINT('Ctrl Pts',(-5.91623110189089,0.84993950459726,63.5233521849073));
#59187=CARTESIAN_POINT('Ctrl Pts',(-5.73107037269015,1.70039301271516,63.4833291776097));
#59188=CARTESIAN_POINT('Ctrl Pts',(-5.37589115391287,2.47263111983861,63.4433061703122));
#59189=CARTESIAN_POINT('Ctrl Pts',(-4.96419861988145,3.36774166231843,63.3969150178382));
#59190=CARTESIAN_POINT('Ctrl Pts',(-4.32407929378261,4.15776661567246,63.3505238653642));
#59191=CARTESIAN_POINT('Ctrl Pts',(-3.53382635369325,4.74615479151186,63.3041327128903));
#59192=CARTESIAN_POINT('Ctrl Pts',(-2.7435734136039,5.33454296735125,63.2577415604163));
#59193=CARTESIAN_POINT('Ctrl Pts',(-1.80318685952402,5.72129436567601,63.2113504079422));
#59194=CARTESIAN_POINT('Ctrl Pts',(-0.827631399458168,5.85909972305151,
63.1649592554683));
#59195=CARTESIAN_POINT('Ctrl Pts',(0.147924060607687,5.996905080427,63.1185681029943));
#59196=CARTESIAN_POINT('Ctrl Pts',(1.15864842665952,5.88576439685324,63.0721769505203));
#59197=CARTESIAN_POINT('Ctrl Pts',(2.08095574250639,5.53927791248008,63.0257857980463));
#59198=CARTESIAN_POINT('Ctrl Pts',(3.00326305835326,5.19279142810691,62.9793946455724));
#59199=CARTESIAN_POINT('Ctrl Pts',(3.83715332399518,4.61095914293436,62.9330034930984));
#59200=CARTESIAN_POINT('Ctrl Pts',(4.48067252974842,3.86491443257027,62.8866123406244));
#59201=CARTESIAN_POINT('Ctrl Pts',(5.1241917355017,3.11886972220613,62.8402211881504));
#59202=CARTESIAN_POINT('Ctrl Pts',(5.57733988136629,2.20861258665045,62.7938300356764));
#59203=CARTESIAN_POINT('Ctrl Pts',(5.78470977513812,1.24544089377108,62.7474388832024));
#59204=CARTESIAN_POINT('Ctrl Pts',(5.99207966890992,0.282269200891815,62.7010477307284));
#59205=CARTESIAN_POINT('Ctrl Pts',(5.95367131058902,-0.73381704931112,62.6546565782545));
#59206=CARTESIAN_POINT('Ctrl Pts',(5.67418176459349,-1.6785850372942,62.6082654257805));
#59207=CARTESIAN_POINT('Ctrl Pts',(5.39469221859793,-2.62335302527734,62.5618742733065));
#59208=CARTESIAN_POINT('Ctrl Pts',(4.87412148492771,-3.49680275104061,62.5154831208325));
#59209=CARTESIAN_POINT('Ctrl Pts',(4.17611796055031,-4.1921388959224,62.4690919683585));
#59210=CARTESIAN_POINT('Ctrl Pts',(3.47811443617291,-4.88747504080418,62.4227008158845));
#59211=CARTESIAN_POINT('Ctrl Pts',(2.60267812108833,-5.40469760480448,62.3763096634105));
#59212=CARTESIAN_POINT('Ctrl Pts',(1.65684670001291,-5.68056746832837,62.3299185109365));
#59213=CARTESIAN_POINT('Ctrl Pts',(0.711015278937486,-5.95643733185225,
62.2835273584626));
#59214=CARTESIAN_POINT('Ctrl Pts',(-0.305211248128781,-5.99095449489973,
62.2371362059886));
#59215=CARTESIAN_POINT('Ctrl Pts',(-1.26758151165544,-5.77989842323892,
62.1907450535146));
#59216=CARTESIAN_POINT('Ctrl Pts',(-2.2299517751821,-5.56884235157811,62.1443539010407));
#59217=CARTESIAN_POINT('Ctrl Pts',(-3.13846577516915,-5.112213045209,62.0979627485666));
#59218=CARTESIAN_POINT('Ctrl Pts',(-3.88204168820752,-4.46584154408076,
62.0515715960926));
#59219=CARTESIAN_POINT('Ctrl Pts',(-4.62561760124594,-3.81947004295248,
62.0051804436187));
#59220=CARTESIAN_POINT('Ctrl Pts',(-5.20425542733567,-2.98335634706504,
61.9587892911447));
#59221=CARTESIAN_POINT('Ctrl Pts',(-5.54720658714768,-2.05972995272988,
61.9123981386707));
#59222=CARTESIAN_POINT('Ctrl Pts',(-5.79121887920067,-1.40256292753042,
61.8793904898488));
#59223=CARTESIAN_POINT('Ctrl Pts',(-5.91591649412851,-0.701093229105765,
61.8463828410268));
#59224=CARTESIAN_POINT('Ctrl Pts',(-5.91657547456529,0.000148352692112552,
61.8133751922048));
#59225=CARTESIAN_POINT('Origin',(0.,0.,0.));
#59226=CARTESIAN_POINT('Origin',(0.,0.,79.));
#59227=CARTESIAN_POINT('',(-10.,-1.22464679914735E-15,79.));
#59228=CARTESIAN_POINT('Origin',(0.,0.,79.));
#59229=CARTESIAN_POINT('Origin',(0.,0.,79.));
#59230=CARTESIAN_POINT('',(-10.,-1.22464679914735E-15,91.));
#59231=CARTESIAN_POINT('Origin',(0.,0.,91.));
#59232=CARTESIAN_POINT('',(-10.,-1.22464679914735E-15,79.));
#59233=CARTESIAN_POINT('Origin',(0.,0.,91.));
#59234=CARTESIAN_POINT('Origin',(0.,0.,0.));
#59235=CARTESIAN_POINT('',(0.,0.,0.));
#59236=CARTESIAN_POINT('Origin',(-1.,0.,1.));
#59237=CARTESIAN_POINT('',(-1.,4.89897948556636,0.));
#59238=CARTESIAN_POINT('',(-1.,4.89897948556636,1.));
#59239=CARTESIAN_POINT('',(-1.,4.89897948556636,0.));
#59240=CARTESIAN_POINT('',(-1.,8.94427190999916,0.));
#59241=CARTESIAN_POINT('',(-1.,0.,0.));
#59242=CARTESIAN_POINT('',(-1.,8.94427190999916,1.));
#59243=CARTESIAN_POINT('',(-1.,8.94427190999916,0.));
#59244=CARTESIAN_POINT('',(-1.,0.,1.));
#59245=CARTESIAN_POINT('Origin',(1.,18.,1.));
#59246=CARTESIAN_POINT('',(1.,4.89897948556636,1.));
#59247=CARTESIAN_POINT('',(1.,4.89897948556636,0.));
#59248=CARTESIAN_POINT('',(1.,4.89897948556636,0.));
#59249=CARTESIAN_POINT('',(1.,8.94427190999916,1.));
#59250=CARTESIAN_POINT('',(1.,9.,1.));
#59251=CARTESIAN_POINT('',(1.,8.94427190999916,0.));
#59252=CARTESIAN_POINT('',(1.,8.94427190999916,0.));
#59253=CARTESIAN_POINT('',(1.,9.,0.));
#59254=CARTESIAN_POINT('Origin',(0.,0.,0.));
#59255=CARTESIAN_POINT('Origin',(0.,0.,0.));
#59256=CARTESIAN_POINT('Origin',(0.,0.,0.));
#59257=CARTESIAN_POINT('Origin',(0.,0.,0.));
#59258=CARTESIAN_POINT('Origin',(0.,0.,1.));
#59259=CARTESIAN_POINT('Origin',(0.,0.,0.));
#59260=CARTESIAN_POINT('Origin',(0.,0.,1.));
#59261=CARTESIAN_POINT('Origin',(0.,0.,1.));
#59262=CARTESIAN_POINT('',(0.,0.,0.));
#59263=CARTESIAN_POINT('Origin',(0.,0.,0.));
#59264=CARTESIAN_POINT('',(-6.,-7.34788079488412E-16,8.));
#59265=CARTESIAN_POINT('Origin',(0.,0.,8.));
#59266=CARTESIAN_POINT('',(-6.,-7.34788079488412E-16,0.));
#59267=CARTESIAN_POINT('',(-6.,-7.34788079488412E-16,0.));
#59268=CARTESIAN_POINT('Origin',(0.,0.,0.));
#59269=CARTESIAN_POINT('Origin',(0.,0.,0.));
#59270=CARTESIAN_POINT('',(-7.,-8.57252759403147E-16,8.));
#59271=CARTESIAN_POINT('Origin',(0.,0.,8.));
#59272=CARTESIAN_POINT('',(-7.,-8.57252759403147E-16,0.));
#59273=CARTESIAN_POINT('',(-7.,-8.57252759403147E-16,0.));
#59274=CARTESIAN_POINT('Origin',(0.,0.,0.));
#59275=CARTESIAN_POINT('Origin',(0.,0.,8.));
#59276=CARTESIAN_POINT('Origin',(0.,0.,0.));
#59277=CARTESIAN_POINT('',(0.,0.,0.));
#59278=CARTESIAN_POINT('Origin',(0.,0.,0.));
#59279=CARTESIAN_POINT('',(-6.,-7.34788079488412E-16,2.));
#59280=CARTESIAN_POINT('Origin',(0.,0.,2.));
#59281=CARTESIAN_POINT('',(-6.,-7.34788079488412E-16,0.));
#59282=CARTESIAN_POINT('',(-6.,-7.34788079488412E-16,0.));
#59283=CARTESIAN_POINT('Origin',(0.,0.,0.));
#59284=CARTESIAN_POINT('Origin',(0.,0.,0.));
#59285=CARTESIAN_POINT('',(-10.,-1.22464679914735E-15,2.));
#59286=CARTESIAN_POINT('Origin',(0.,0.,2.));
#59287=CARTESIAN_POINT('',(-10.,-1.22464679914735E-15,0.));
#59288=CARTESIAN_POINT('',(-10.,-1.22464679914735E-15,0.));
#59289=CARTESIAN_POINT('Origin',(0.,0.,0.));
#59290=CARTESIAN_POINT('Origin',(0.,0.,2.));
#59291=CARTESIAN_POINT('Origin',(0.,0.,0.));
#59292=CARTESIAN_POINT('',(0.,0.,0.));
#59293=CARTESIAN_POINT('Origin',(0.,0.,0.));
#59294=CARTESIAN_POINT('',(-2.94578277890271,0.00179111083247481,0.322176117089595));
#59295=CARTESIAN_POINT('',(-2.94467343002877,0.00314729851841336,0.177823882910467));
#59296=CARTESIAN_POINT('',(-2.942,-3.60291088309151E-16,0.));
#59297=CARTESIAN_POINT('',(1.28892185405323,2.64462557919718,0.));
#59298=CARTESIAN_POINT('Ctrl Pts',(-2.94578277890271,0.00179111083247481,
0.322176117089595));
#59299=CARTESIAN_POINT('Ctrl Pts',(-2.94637589714326,0.0927166687183431,
0.317238878916034));
#59300=CARTESIAN_POINT('Ctrl Pts',(-2.94253410879075,0.183587894393493,
0.312301640742474));
#59301=CARTESIAN_POINT('Ctrl Pts',(-2.93409440150521,0.274025695936747,
0.307364402568913));
#59302=CARTESIAN_POINT('Ctrl Pts',(-2.84341104252089,1.24576598806222,0.254314536437722));
#59303=CARTESIAN_POINT('Ctrl Pts',(-2.22189000884716,2.16746671627164,0.20126467030653));
#59304=CARTESIAN_POINT('Ctrl Pts',(-1.35502173669404,2.61657805746752,0.148214804175339));
#59305=CARTESIAN_POINT('Ctrl Pts',(-0.547713942644492,3.03483201575685,
0.0988098694502261));
#59306=CARTESIAN_POINT('Ctrl Pts',(0.472384848283181,3.0432066234576,0.0494049347251131));
#59307=CARTESIAN_POINT('Ctrl Pts',(1.29201581877684,2.64862154577367,3.40875331157512E-17));
#59308=CARTESIAN_POINT('',(-1.28892185405299,2.64462557919729,0.));
#59309=CARTESIAN_POINT('Origin',(0.,0.,0.));
#59310=CARTESIAN_POINT('Ctrl Pts',(-1.28892185405299,2.64462557919729,-1.41553435639707E-14));
#59311=CARTESIAN_POINT('Ctrl Pts',(-2.1671763893535,2.21658711777033,0.0528538148029031));
#59312=CARTESIAN_POINT('Ctrl Pts',(-2.80795602549936,1.32047159410707,0.105707629605821));
#59313=CARTESIAN_POINT('Ctrl Pts',(-2.9249109785407,0.356582248145783,0.158561444408738));
#59314=CARTESIAN_POINT('Ctrl Pts',(-2.93911895702394,0.23948657385823,0.164982257242648));
#59315=CARTESIAN_POINT('Ctrl Pts',(-2.94559633372376,0.121390693875098,
0.171403070076557));
#59316=CARTESIAN_POINT('Ctrl Pts',(-2.94467343002877,0.00314729851841336,
0.177823882910467));
#59317=CARTESIAN_POINT('Origin',(0.,0.,0.));
#59318=CARTESIAN_POINT('',(-2.93831560050017,0.00184555222839333,1.32217611708959));
#59319=CARTESIAN_POINT('',(-2.93760127776231,0.0011368673086444,1.17782388291046));
#59320=CARTESIAN_POINT('',(-2.942,-3.60291088309151E-16,0.));
#59321=CARTESIAN_POINT('Ctrl Pts',(-2.93831560050017,0.00184555222839333,
1.32217611708959));
#59322=CARTESIAN_POINT('Ctrl Pts',(-2.94042418966808,0.372080548742382,
1.30220474236985));
#59323=CARTESIAN_POINT('Ctrl Pts',(-2.87561341710461,0.741603687830221,
1.2822333676501));
#59324=CARTESIAN_POINT('Ctrl Pts',(-2.74052219187739,1.08334315658386,1.26226199293036));
#59325=CARTESIAN_POINT('Ctrl Pts',(-2.38168002330511,1.99110405554696,1.20921212679917));
#59326=CARTESIAN_POINT('Ctrl Pts',(-1.52694572694536,2.70282604358144,1.15616226066798));
#59327=CARTESIAN_POINT('Ctrl Pts',(-0.569210306211631,2.89137544039496,
1.10311239453678));
#59328=CARTESIAN_POINT('Ctrl Pts',(0.388525114522094,3.07992483720848,1.05006252840559));
#59329=CARTESIAN_POINT('Ctrl Pts',(1.4492616596298,2.74530164280104,0.997012662274401));
#59330=CARTESIAN_POINT('Ctrl Pts',(2.12540309125483,2.04127771721126,0.94396279614321));
#59331=CARTESIAN_POINT('Ctrl Pts',(2.80154452287985,1.33725379162148,0.890912930012018));
#59332=CARTESIAN_POINT('Ctrl Pts',(3.0930908410222,0.263829134849373,0.837863063880828));
#59333=CARTESIAN_POINT('Ctrl Pts',(2.86604250647906,-0.685491427036063,
0.784813197749637));
#59334=CARTESIAN_POINT('Ctrl Pts',(2.63899417193593,-1.63481198892151,0.731763331618445));
#59335=CARTESIAN_POINT('Ctrl Pts',(1.8933511847073,-2.46002845592027,0.678713465487253));
#59336=CARTESIAN_POINT('Ctrl Pts',(0.97183346999997,-2.78197492031178,0.625663599356061));
#59337=CARTESIAN_POINT('Ctrl Pts',(0.0503157552926523,-3.10392138470329,
0.57261373322487));
#59338=CARTESIAN_POINT('Ctrl Pts',(-1.04707668689336,-2.92259784648754,
0.519563867093679));
#59339=CARTESIAN_POINT('Ctrl Pts',(-1.81585006583891,-2.3210461493589,0.466514000962488));
#59340=CARTESIAN_POINT('Ctrl Pts',(-2.51307534202467,-1.77547958883907,
0.418401373004857));
#59341=CARTESIAN_POINT('Ctrl Pts',(-2.94000293271358,-0.884264490420376,
0.370288745047226));
#59342=CARTESIAN_POINT('Ctrl Pts',(-2.94578277890271,0.00179111083247481,
0.322176117089595));
#59343=CARTESIAN_POINT('Ctrl Pts',(-2.94467343002877,0.00314729851841336,
0.177823882910467));
#59344=CARTESIAN_POINT('Ctrl Pts',(-2.93799932346391,-0.851946277862307,
0.224256884879474));
#59345=CARTESIAN_POINT('Ctrl Pts',(-2.54431566930391,-1.71475440760266,
0.270689886848481));
#59346=CARTESIAN_POINT('Ctrl Pts',(-1.88854677527079,-2.26279797837909,
0.317122888817489));
#59347=CARTESIAN_POINT('Ctrl Pts',(-1.14209734902272,-2.88662569068338,
0.369976703620406));
#59348=CARTESIAN_POINT('Ctrl Pts',(-0.0560682265897754,-3.10261794703268,
0.422830518423324));
#59349=CARTESIAN_POINT('Ctrl Pts',(0.872963891668672,-2.8142569045846,0.475684333226241));
#59350=CARTESIAN_POINT('Ctrl Pts',(1.80199600992712,-2.52589586213653,0.528538148029158));
#59351=CARTESIAN_POINT('Ctrl Pts',(2.57403112401107,-1.73318152089108,0.581391962832075));
#59352=CARTESIAN_POINT('Ctrl Pts',(2.83696576039216,-0.796977059524136,
0.634245777634992));
#59353=CARTESIAN_POINT('Ctrl Pts',(3.09990039677324,0.139227401842806,0.68709959243791));
#59354=CARTESIAN_POINT('Ctrl Pts',(2.85373455545147,1.21892198333124,0.739953407240827));
#59355=CARTESIAN_POINT('Ctrl Pts',(2.21066027791899,1.94860552630545,0.792807222043744));
#59356=CARTESIAN_POINT('Ctrl Pts',(1.56758600038652,2.67828906927967,0.845661036846661));
#59357=CARTESIAN_POINT('Ctrl Pts',(0.527603286643354,3.05796157373966,0.898514851649578));
#59358=CARTESIAN_POINT('Ctrl Pts',(-0.434365791604633,2.91456720332865,
0.951368666452495));
#59359=CARTESIAN_POINT('Ctrl Pts',(-1.39633486985262,2.77117283291763,1.00422248125541));
#59360=CARTESIAN_POINT('Ctrl Pts',(-2.28029031260542,2.10471158763561,1.05707629605833));
#59361=CARTESIAN_POINT('Ctrl Pts',(-2.68270470090093,1.21931408472001,1.10993011086125));
#59362=CARTESIAN_POINT('Ctrl Pts',(-2.85501286099708,0.840199373321872,
1.13256136821099));
#59363=CARTESIAN_POINT('Ctrl Pts',(-2.9390337672121,0.420944198753331,1.15519262556072));
#59364=CARTESIAN_POINT('Ctrl Pts',(-2.93760127776231,0.0011368673086444,
1.17782388291046));
#59365=CARTESIAN_POINT('Origin',(0.,0.,0.));
#59366=CARTESIAN_POINT('',(-2.93907445095043,-0.00223594544481509,2.3221761170896));
#59367=CARTESIAN_POINT('',(-2.94106450717812,-0.00264273247052857,2.17782388291046));
#59368=CARTESIAN_POINT('',(-2.942,-3.60291088309151E-16,0.));
#59369=CARTESIAN_POINT('Ctrl Pts',(-2.93907445095043,-0.00223594544481509,
2.3221761170896));
#59370=CARTESIAN_POINT('Ctrl Pts',(-2.93451423355693,0.646284517263058,
2.28717060582367));
#59371=CARTESIAN_POINT('Ctrl Pts',(-2.72312957542652,1.29750586897281,2.25216509455774));
#59372=CARTESIAN_POINT('Ctrl Pts',(-2.32830278838925,1.80640429077704,2.2171595832918));
#59373=CARTESIAN_POINT('Ctrl Pts',(-1.72995391588694,2.57762551208695,2.16410971716061));
#59374=CARTESIAN_POINT('Ctrl Pts',(-0.710301786504807,3.02198008474211,
2.11105985102942));
#59375=CARTESIAN_POINT('Ctrl Pts',(0.261950767826724,2.93521227313122,2.05800998489823));
#59376=CARTESIAN_POINT('Ctrl Pts',(1.23420332215825,2.84844446152033,2.00496011876704));
#59377=CARTESIAN_POINT('Ctrl Pts',(2.15905630143918,2.23055426564339,1.95191025263585));
#59378=CARTESIAN_POINT('Ctrl Pts',(2.611382890642,1.36556600713954,1.89886038650466));
#59379=CARTESIAN_POINT('Ctrl Pts',(3.06370947984483,0.500577748635682,1.84581052037347));
#59380=CARTESIAN_POINT('Ctrl Pts',(3.04350967896956,-0.611508572495087,
1.79276065424227));
#59381=CARTESIAN_POINT('Ctrl Pts',(2.56006903828727,-1.45949911536289,1.73971078811108));
#59382=CARTESIAN_POINT('Ctrl Pts',(2.07662839760498,-2.3074896582307,1.68666092197989));
#59383=CARTESIAN_POINT('Ctrl Pts',(1.12994691711567,-2.89138442283555,1.6336110558487));
#59384=CARTESIAN_POINT('Ctrl Pts',(0.155184530430073,-2.94278816759169,
1.58056118971751));
#59385=CARTESIAN_POINT('Ctrl Pts',(-0.819577856255521,-2.99419191234782,
1.52751132358632));
#59386=CARTESIAN_POINT('Ctrl Pts',(-1.82242114913739,-2.51310463725525,
1.47446145745513));
#59387=CARTESIAN_POINT('Ctrl Pts',(-2.39236777518593,-1.7206610947631,1.42141159132393));
#59388=CARTESIAN_POINT('Ctrl Pts',(-2.74774990806646,-1.22654416618201,
1.38833309991249));
#59389=CARTESIAN_POINT('Ctrl Pts',(-2.93482315445378,-0.611372882869942,
1.35525460850104));
#59390=CARTESIAN_POINT('Ctrl Pts',(-2.93831560050017,0.00184555222839333,
1.32217611708959));
#59391=CARTESIAN_POINT('Ctrl Pts',(-2.93760127776231,0.0011368673086444,
1.17782388291046));
#59392=CARTESIAN_POINT('Ctrl Pts',(-2.93568828220805,-0.559488245020752,
1.20804644036364));
#59393=CARTESIAN_POINT('Ctrl Pts',(-2.78137900093947,-1.12109806552238,
1.23826899781682));
#59394=CARTESIAN_POINT('Ctrl Pts',(-2.48142253148132,-1.58940935219029,
1.26849155527));
#59395=CARTESIAN_POINT('Ctrl Pts',(-1.956852639928,-2.40840152563582,1.32134537007292));
#59396=CARTESIAN_POINT('Ctrl Pts',(-0.986839522983141,-2.94205211197772,
1.37419918487583));
#59397=CARTESIAN_POINT('Ctrl Pts',(-0.0142707720111539,-2.94675725529095,
1.42705299967875));
#59398=CARTESIAN_POINT('Ctrl Pts',(0.958297978960832,-2.95146239860418,
1.47990681448167));
#59399=CARTESIAN_POINT('Ctrl Pts',(1.93342236395995,-2.42722209888874,1.53276062928459));
#59400=CARTESIAN_POINT('Ctrl Pts',(2.46590395666548,-1.61336359456041,1.5856144440875));
#59401=CARTESIAN_POINT('Ctrl Pts',(2.99838554937101,-0.799505090232077,
1.63846825889042));
#59402=CARTESIAN_POINT('Ctrl Pts',(3.08822434978297,0.303971618709142,1.69132207369334));
#59403=CARTESIAN_POINT('Ctrl Pts',(2.69439912910768,1.19324786258786,1.74417588849625));
#59404=CARTESIAN_POINT('Ctrl Pts',(2.3005739084324,2.08252410646659,1.79702970329917));
#59405=CARTESIAN_POINT('Ctrl Pts',(1.42308466666986,2.75759988528281,1.84988351810209));
#59406=CARTESIAN_POINT('Ctrl Pts',(0.462563168363892,2.91026618027041,1.90273733290501));
#59407=CARTESIAN_POINT('Ctrl Pts',(-0.497958329942082,3.06293247525801,
1.95559114770792));
#59408=CARTESIAN_POINT('Ctrl Pts',(-1.54151208479149,2.69318928641698,2.00844496251084));
#59409=CARTESIAN_POINT('Ctrl Pts',(-2.19165060625059,1.96984474512453,2.06129877731376));
#59410=CARTESIAN_POINT('Ctrl Pts',(-2.66943043569144,1.43826659653236,2.10014047917933));
#59411=CARTESIAN_POINT('Ctrl Pts',(-2.93474154792488,0.715721704963004,
2.13898218104489));
#59412=CARTESIAN_POINT('Ctrl Pts',(-2.94106450717812,-0.00264273247052857,
2.17782388291046));
#59413=CARTESIAN_POINT('Origin',(0.,0.,0.));
#59414=CARTESIAN_POINT('',(-2.94645640454328,-0.00101572304112452,3.32217611708959));
#59415=CARTESIAN_POINT('',(-2.94656901584595,0.000739931193793274,3.17782388291046));
#59416=CARTESIAN_POINT('',(-2.942,-3.60291088309151E-16,0.));
#59417=CARTESIAN_POINT('Ctrl Pts',(-2.94645640454328,-0.00101572304112452,
3.32217611708959));
#59418=CARTESIAN_POINT('Ctrl Pts',(-2.94234855388754,0.920065526773415,
3.27213646927748));
#59419=CARTESIAN_POINT('Ctrl Pts',(-2.47563861836594,1.8447343524899,3.22209682146536));
#59420=CARTESIAN_POINT('Ctrl Pts',(-1.73034924050614,2.38536824088973,3.17205717365325));
#59421=CARTESIAN_POINT('Ctrl Pts',(-0.94022573937933,2.95852486088202,3.11900730752206));
#59422=CARTESIAN_POINT('Ctrl Pts',(0.163002154399846,3.10005226661288,3.06595744139087));
#59423=CARTESIAN_POINT('Ctrl Pts',(1.07221429851196,2.74489464521787,3.01290757525968));
#59424=CARTESIAN_POINT('Ctrl Pts',(1.98142644262409,2.38973702382286,2.95985770912849));
#59425=CARTESIAN_POINT('Ctrl Pts',(2.69662283706915,1.53789437530197,2.90680784299729));
#59426=CARTESIAN_POINT('Ctrl Pts',(2.88904955483864,0.580932710785723,2.8537579768661));
#59427=CARTESIAN_POINT('Ctrl Pts',(3.08147627260814,-0.376028953730528,
2.80070811073491));
#59428=CARTESIAN_POINT('Ctrl Pts',(2.75113331370206,-1.43810963424215,2.74765824460372));
#59429=CARTESIAN_POINT('Ctrl Pts',(2.0498692464734,-2.11710326668621,2.69460837847253));
#59430=CARTESIAN_POINT('Ctrl Pts',(1.34860517924474,-2.79609689913027,2.64155851234134));
#59431=CARTESIAN_POINT('Ctrl Pts',(0.2764200036935,-3.09200348350679,2.58850864621014));
#59432=CARTESIAN_POINT('Ctrl Pts',(-0.673835537461917,-2.86880387612486,
2.53545878007895));
#59433=CARTESIAN_POINT('Ctrl Pts',(-1.62409107861733,-2.64560426874294,
2.48240891394776));
#59434=CARTESIAN_POINT('Ctrl Pts',(-2.45241698537691,-1.90329846960257,
2.42935904781657));
#59435=CARTESIAN_POINT('Ctrl Pts',(-2.77805713094547,-0.98310163505006,
2.37630918168538));
#59436=CARTESIAN_POINT('Ctrl Pts',(-2.8888202067746,-0.670106345156332,
2.35826482682012));
#59437=CARTESIAN_POINT('Ctrl Pts',(-2.94142511454412,-0.336529973536149,
2.34022047195486));
#59438=CARTESIAN_POINT('Ctrl Pts',(-2.93907445095043,-0.00223594544481509,
2.3221761170896));
#59439=CARTESIAN_POINT('Ctrl Pts',(-2.94106450717812,-0.00264273247052857,
2.17782388291046));
#59440=CARTESIAN_POINT('Ctrl Pts',(-2.94334550968056,-0.261792129742843,
2.19183599584781));
#59441=CARTESIAN_POINT('Ctrl Pts',(-2.91192179745946,-0.520397482770503,
2.20584810878516));
#59442=CARTESIAN_POINT('Ctrl Pts',(-2.84460938087215,-0.769297041196698,
2.21986022172251));
#59443=CARTESIAN_POINT('Ctrl Pts',(-2.59070634596583,-1.70814839248162,
2.27271403652542));
#59444=CARTESIAN_POINT('Ctrl Pts',(-1.82617698808441,-2.50890520130758,
2.32556785132834));
#59445=CARTESIAN_POINT('Ctrl Pts',(-0.900077862744179,-2.80597194921199,
2.37842166613126));
#59446=CARTESIAN_POINT('Ctrl Pts',(0.0260212625960488,-3.1030386971164,
2.43127548093418));
#59447=CARTESIAN_POINT('Ctrl Pts',(1.11369015539508,-2.89641538409926,2.48412929573709));
#59448=CARTESIAN_POINT('Ctrl Pts',(1.86633899573991,-2.28043823425261,2.53698311054001));
#59449=CARTESIAN_POINT('Ctrl Pts',(2.61898783608474,-1.66446108440595,2.58983692534293));
#59450=CARTESIAN_POINT('Ctrl Pts',(3.03661662397538,-0.63913009772978,2.64269074014585));
#59451=CARTESIAN_POINT('Ctrl Pts',(2.92855118796608,0.327425723295819,2.69554455494876));
#59452=CARTESIAN_POINT('Ctrl Pts',(2.82048575195678,1.29398154432143,2.74839836975168));
#59453=CARTESIAN_POINT('Ctrl Pts',(2.18672609204752,2.20176219969646,2.8012521845546));
#59454=CARTESIAN_POINT('Ctrl Pts',(1.31662381963688,2.63630824527895,2.85410599935752));
#59455=CARTESIAN_POINT('Ctrl Pts',(0.446521547226236,3.07085429086145,2.90695981416043));
#59456=CARTESIAN_POINT('Ctrl Pts',(-0.659923337685789,3.03216572665139,
2.95981362896335));
#59457=CARTESIAN_POINT('Ctrl Pts',(-1.49754844237796,2.53790627629345,3.01266744376627));
#59458=CARTESIAN_POINT('Ctrl Pts',(-2.33517354707012,2.04364682593551,3.06552125856918));
#59459=CARTESIAN_POINT('Ctrl Pts',(-2.90397887154242,1.09381648942966,3.1183750733721));
#59460=CARTESIAN_POINT('Ctrl Pts',(-2.94426861939999,0.12207322109005,3.17122888817502));
#59461=CARTESIAN_POINT('Ctrl Pts',(-2.94594437781657,0.0816558184686259,
3.1734272197535));
#59462=CARTESIAN_POINT('Ctrl Pts',(-2.94670583035639,0.0412005075560573,
3.17562555133198));
#59463=CARTESIAN_POINT('Ctrl Pts',(-2.94656901584595,0.000739931193793274,
3.17782388291046));
#59464=CARTESIAN_POINT('Origin',(0.,0.,0.));
#59465=CARTESIAN_POINT('',(-2.94218751408198,0.00271333560157655,4.32217611708959));
#59466=CARTESIAN_POINT('',(-2.93894157525109,0.00211448818579894,4.17782388291047));
#59467=CARTESIAN_POINT('',(-2.942,-3.60291088309151E-16,0.));
#59468=CARTESIAN_POINT('Ctrl Pts',(-2.94218751408198,0.00271333560157655,
4.32217611708959));
#59469=CARTESIAN_POINT('Ctrl Pts',(-2.94425072300269,0.224874109476442,
4.31015219886249));
#59470=CARTESIAN_POINT('Ctrl Pts',(-2.92122841359833,0.446611437489588,
4.29812828063538));
#59471=CARTESIAN_POINT('Ctrl Pts',(-2.87151357587431,0.662193261821331,
4.28610436240827));
#59472=CARTESIAN_POINT('Ctrl Pts',(-2.65217031054445,1.61334634728837,4.23305449627708));
#59473=CARTESIAN_POINT('Ctrl Pts',(-1.91323048328662,2.4446764429101,4.18000463014589));
#59474=CARTESIAN_POINT('Ctrl Pts',(-0.994362148038726,2.77404651207381,
4.1269547640147));
#59475=CARTESIAN_POINT('Ctrl Pts',(-0.0754938127908314,3.10341658123751,
4.0739048978835));
#59476=CARTESIAN_POINT('Ctrl Pts',(1.02330303044713,2.9308266239432,4.02085503175231));
#59477=CARTESIAN_POINT('Ctrl Pts',(1.79694505607989,2.33561096879262,3.96780516562112));
#59478=CARTESIAN_POINT('Ctrl Pts',(2.57058708171265,1.74039531364205,3.91475529948993));
#59479=CARTESIAN_POINT('Ctrl Pts',(3.01907428974022,0.722553960635232,3.86170543335874));
#59480=CARTESIAN_POINT('Ctrl Pts',(2.93625081795067,-0.250042529555778,
3.80865556722755));
#59481=CARTESIAN_POINT('Ctrl Pts',(2.85342734616113,-1.22263901974679,3.75560570109635));
#59482=CARTESIAN_POINT('Ctrl Pts',(2.23929319455449,-2.14999064712199,3.70255583496516));
#59483=CARTESIAN_POINT('Ctrl Pts',(1.37614706260187,-2.60582221104315,3.64950596883397));
#59484=CARTESIAN_POINT('Ctrl Pts',(0.513000930649261,-3.06165377496431,
3.59645610270278));
#59485=CARTESIAN_POINT('Ctrl Pts',(-0.599157181649314,-3.04596527543143,
3.54340623657159));
#59486=CARTESIAN_POINT('Ctrl Pts',(-1.44910218190426,-2.5659682376169,3.4903563704404));
#59487=CARTESIAN_POINT('Ctrl Pts',(-2.29904718215921,-2.08597119980237,
3.43730650430921));
#59488=CARTESIAN_POINT('Ctrl Pts',(-2.88677907037054,-1.14166562370618,
3.38425663817802));
#59489=CARTESIAN_POINT('Ctrl Pts',(-2.94213546023897,-0.16711991853123,
3.33120677204682));
#59490=CARTESIAN_POINT('Ctrl Pts',(-2.94527655805905,-0.111821092192249,
3.32819655372775));
#59491=CARTESIAN_POINT('Ctrl Pts',(-2.94670351913813,-0.0564248990201435,
3.32518633540867));
#59492=CARTESIAN_POINT('Ctrl Pts',(-2.94645640454328,-0.00101572304112452,
3.32217611708959));
#59493=CARTESIAN_POINT('Ctrl Pts',(-2.94656901584595,0.000739931193793274,
3.17782388291046));
#59494=CARTESIAN_POINT('Ctrl Pts',(-2.94341644086314,-0.931580773849932,
3.2284793661349));
#59495=CARTESIAN_POINT('Ctrl Pts',(-2.46331480529716,-1.86669725247251,
3.27913484935933));
#59496=CARTESIAN_POINT('Ctrl Pts',(-1.70249726223018,-2.40522818466485,
3.32979033258377));
#59497=CARTESIAN_POINT('Ctrl Pts',(-0.908661985959945,-2.96713012190678,
3.38264414738669));
#59498=CARTESIAN_POINT('Ctrl Pts',(0.190782737823382,-3.09727779621724,
3.4354979621896));
#59499=CARTESIAN_POINT('Ctrl Pts',(1.0938705148769,-2.73625051267428,3.48835177699252));
#59500=CARTESIAN_POINT('Ctrl Pts',(1.99695829193042,-2.37522322913131,3.54120559179544));
#59501=CARTESIAN_POINT('Ctrl Pts',(2.70368912225412,-1.5230209877349,3.59405940659836));
#59502=CARTESIAN_POINT('Ctrl Pts',(2.89139545991222,-0.568728282942871,
3.64691322140127));
#59503=CARTESIAN_POINT('Ctrl Pts',(3.07910179757031,0.385564421849148,3.69976703620419));
#59504=CARTESIAN_POINT('Ctrl Pts',(2.74778364256282,1.44194759003679,3.75262085100711));
#59505=CARTESIAN_POINT('Ctrl Pts',(2.0487087923059,2.11811516372279,3.80547466581002));
#59506=CARTESIAN_POINT('Ctrl Pts',(1.34963394204897,2.79428273740879,3.85832848061294));
#59507=CARTESIAN_POINT('Ctrl Pts',(0.282802396542619,3.09023471659314,3.91118229541586));
#59508=CARTESIAN_POINT('Ctrl Pts',(-0.664709435881276,2.87085021059064,
3.96403611021878));
#59509=CARTESIAN_POINT('Ctrl Pts',(-1.61222126830517,2.65146570458813,4.0168899250217));
#59510=CARTESIAN_POINT('Ctrl Pts',(-2.4404133876466,1.91674471339877,4.06974373982461));
#59511=CARTESIAN_POINT('Ctrl Pts',(-2.77116345090882,1.00213406940284,4.12259755462753));
#59512=CARTESIAN_POINT('Ctrl Pts',(-2.88636239880838,0.683578774547044,
4.14100633072184));
#59513=CARTESIAN_POINT('Ctrl Pts',(-2.94121657433896,0.343201038228005,
4.15941510681615));
#59514=CARTESIAN_POINT('Ctrl Pts',(-2.93894157525109,0.00211448818579894,
4.17782388291047));
#59515=CARTESIAN_POINT('Origin',(0.,0.,0.));
#59516=CARTESIAN_POINT('',(-2.93713130355353,-0.000163959391183133,5.32217611708959));
#59517=CARTESIAN_POINT('',(-2.93901369524072,-0.00214676294064878,5.17782388291046));
#59518=CARTESIAN_POINT('',(-2.942,-3.60291088309151E-16,0.));
#59519=CARTESIAN_POINT('Ctrl Pts',(-2.93713130355353,-0.000163959391183133,
5.32217611708959));
#59520=CARTESIAN_POINT('Ctrl Pts',(-2.93688283938904,0.501950620212298,
5.2951180623163));
#59521=CARTESIAN_POINT('Ctrl Pts',(-2.81488686979709,1.00417843559043,5.26806000754301));
#59522=CARTESIAN_POINT('Ctrl Pts',(-2.57182512474634,1.43868191764525,5.24100195276971));
#59523=CARTESIAN_POINT('Ctrl Pts',(-2.09527966925843,2.29056693856319,5.18795208663852));
#59524=CARTESIAN_POINT('Ctrl Pts',(-1.15336587844195,2.88212438019234,5.13490222050733));
#59525=CARTESIAN_POINT('Ctrl Pts',(-0.179052733645313,2.94143336674734,
5.08185235437614));
#59526=CARTESIAN_POINT('Ctrl Pts',(0.795260411151313,3.00074235330235,5.02880248824495));
#59527=CARTESIAN_POINT('Ctrl Pts',(1.80197290992809,2.52780288478322,4.97575262211376));
#59528=CARTESIAN_POINT('Ctrl Pts',(2.3783297957712,1.74001078013272,4.92270275598257));
#59529=CARTESIAN_POINT('Ctrl Pts',(2.95468668161432,0.952218675482221,4.86965288985138));
#59530=CARTESIAN_POINT('Ctrl Pts',(3.10068795452377,-0.150426065299655,
4.81660302372019));
#59531=CARTESIAN_POINT('Ctrl Pts',(2.74922129166827,-1.06107135569284,4.763553157589));
#59532=CARTESIAN_POINT('Ctrl Pts',(2.39775462881276,-1.97171664608602,4.7105032914578));
#59533=CARTESIAN_POINT('Ctrl Pts',(1.54882003019229,-2.69036248609052,4.65745342532661));
#59534=CARTESIAN_POINT('Ctrl Pts',(0.592646784285425,-2.88666934745533,
4.60440355919542));
#59535=CARTESIAN_POINT('Ctrl Pts',(-0.363526461621441,-3.08297620882014,
4.55135369306423));
#59536=CARTESIAN_POINT('Ctrl Pts',(-1.4269383548147,-2.75694409154526,4.49830382693304));
#59537=CARTESIAN_POINT('Ctrl Pts',(-2.10877094971039,-2.05843999525165,
4.44525396080185));
#59538=CARTESIAN_POINT('Ctrl Pts',(-2.63606405254913,-1.51825403899565,
4.40422801289776));
#59539=CARTESIAN_POINT('Ctrl Pts',(-2.93514778708967,-0.755305486812967,
4.36320206499368));
#59540=CARTESIAN_POINT('Ctrl Pts',(-2.94218751408198,0.00271333560157655,
4.32217611708959));
#59541=CARTESIAN_POINT('Ctrl Pts',(-2.93894157525109,0.00211448818579894,
4.17782388291047));
#59542=CARTESIAN_POINT('Ctrl Pts',(-2.93468477777351,-0.636099554887777,
4.21226892161907));
#59543=CARTESIAN_POINT('Ctrl Pts',(-2.73041348393046,-1.27679522001876,
4.24671396032768));
#59544=CARTESIAN_POINT('Ctrl Pts',(-2.34719296232994,-1.78165786895326,
4.28115899903628));
#59545=CARTESIAN_POINT('Ctrl Pts',(-1.7591644033058,-2.55633886651094,4.3340128138392));
#59546=CARTESIAN_POINT('Ctrl Pts',(-0.749799278074486,-3.01120056482378,
4.38686662864211));
#59547=CARTESIAN_POINT('Ctrl Pts',(0.220063078064465,-2.93856968720406,
4.43972044344503));
#59548=CARTESIAN_POINT('Ctrl Pts',(1.18992543420341,-2.86593880958434,4.49257425824795));
#59549=CARTESIAN_POINT('Ctrl Pts',(2.12028502125,-2.26581535603204,4.54542807305087));
#59550=CARTESIAN_POINT('Ctrl Pts',(2.58637355360725,-1.41219382731194,4.59828188785378));
#59551=CARTESIAN_POINT('Ctrl Pts',(3.05246208596449,-0.558572298591845,
4.6511357026567));
#59552=CARTESIAN_POINT('Ctrl Pts',(3.0542795636324,0.548547305296054,4.70398951745962));
#59553=CARTESIAN_POINT('Ctrl Pts',(2.59099619255503,1.4036945162104,4.75684333226253));
#59554=CARTESIAN_POINT('Ctrl Pts',(2.12771282147767,2.25884172712474,4.80969714706545));
#59555=CARTESIAN_POINT('Ctrl Pts',(1.19932860165501,2.86201654506552,4.86255096186837));
#59556=CARTESIAN_POINT('Ctrl Pts',(0.229709937944512,2.93783132755223,4.91540477667129));
#59557=CARTESIAN_POINT('Ctrl Pts',(-0.739908725765991,3.01364611003894,
4.9682585914742));
#59558=CARTESIAN_POINT('Ctrl Pts',(-1.75076183336435,2.56210085707158,5.02111240627712));
#59559=CARTESIAN_POINT('Ctrl Pts',(-2.34133069094863,1.78935467706368,5.07396622108004));
#59560=CARTESIAN_POINT('Ctrl Pts',(-2.72815297884642,1.28320633978488,5.10858544169018));
#59561=CARTESIAN_POINT('Ctrl Pts',(-2.93466310894815,0.639254998375354,
5.14320466230032));
#59562=CARTESIAN_POINT('Ctrl Pts',(-2.93901369524072,-0.00214676294064878,
5.17782388291046));
#59563=CARTESIAN_POINT('Origin',(0.,0.,0.));
#59564=CARTESIAN_POINT('',(-2.94279128603782,-0.00266058177182005,6.32217611708959));
#59565=CARTESIAN_POINT('',(-2.94660273288284,-0.000682925830890656,6.17782388291046));
#59566=CARTESIAN_POINT('',(-2.942,-3.60291088309151E-16,0.));
#59567=CARTESIAN_POINT('Ctrl Pts',(-2.94279128603782,-0.00266058177182005,
6.32217611708959));
#59568=CARTESIAN_POINT('Ctrl Pts',(-2.93556455204489,0.77464982053833,6.28008392577012));
#59569=CARTESIAN_POINT('Ctrl Pts',(-2.61900297877672,1.55716311141226,6.23799173445064));
#59570=CARTESIAN_POINT('Ctrl Pts',(-2.06697687324552,2.10040394636479,6.19589954313117));
#59571=CARTESIAN_POINT('Ctrl Pts',(-1.37124424252826,2.78506427569988,6.14284967699998));
#59572=CARTESIAN_POINT('Ctrl Pts',(-0.301494896051831,3.08965930485894,
6.08979981086878));
#59573=CARTESIAN_POINT('Ctrl Pts',(0.65054008701558,2.87417600846268,6.03674994473758));
#59574=CARTESIAN_POINT('Ctrl Pts',(1.60257507008298,2.65869271206642,5.98370007860639));
#59575=CARTESIAN_POINT('Ctrl Pts',(2.43689568974137,1.92313109011485,5.9306502124752));
#59576=CARTESIAN_POINT('Ctrl Pts',(2.76999025698787,1.00560633879706,5.87760034634401));
#59577=CARTESIAN_POINT('Ctrl Pts',(3.10308482423439,0.088081587479254,5.82455048021282));
#59578=CARTESIAN_POINT('Ctrl Pts',(2.93495333906901,-1.01140629320476,5.77150061408163));
#59579=CARTESIAN_POINT('Ctrl Pts',(2.34288070651628,-1.78745632882884,5.71845074795044));
#59580=CARTESIAN_POINT('Ctrl Pts',(1.75080807396356,-2.56350636445291,5.66540088181925));
#59581=CARTESIAN_POINT('Ctrl Pts',(0.734794294023496,-3.01611855501705,
5.61235101568806));
#59582=CARTESIAN_POINT('Ctrl Pts',(-0.238130151719265,-2.93724090998327,
5.55930114955686));
#59583=CARTESIAN_POINT('Ctrl Pts',(-1.21105459746203,-2.8583632649495,5.50625128342567));
#59584=CARTESIAN_POINT('Ctrl Pts',(-2.14088970900749,-2.24799578431781,
5.45320141729448));
#59585=CARTESIAN_POINT('Ctrl Pts',(-2.60021870470055,-1.38670574389861,
5.40015155116329));
#59586=CARTESIAN_POINT('Ctrl Pts',(-2.82526720110472,-0.96471621051031,
5.37415973980539));
#59587=CARTESIAN_POINT('Ctrl Pts',(-2.93736997679693,-0.482492328612542,
5.34816792844749));
#59588=CARTESIAN_POINT('Ctrl Pts',(-2.93713130355353,-0.000163959391183133,
5.32217611708959));
#59589=CARTESIAN_POINT('Ctrl Pts',(-2.93901369524072,-0.00214676294064878,
5.17782388291046));
#59590=CARTESIAN_POINT('Ctrl Pts',(-2.94130523081396,-0.339985126312179,
5.19605847710324));
#59591=CARTESIAN_POINT('Ctrl Pts',(-2.88751110036054,-0.677116152820267,
5.21429307129601));
#59592=CARTESIAN_POINT('Ctrl Pts',(-2.77443876694001,-0.993030257951712,
5.23252766548879));
#59593=CARTESIAN_POINT('Ctrl Pts',(-2.44669337777689,-1.90872190591076,
5.28538148029171));
#59594=CARTESIAN_POINT('Ctrl Pts',(-1.62091799188044,-2.64615809478042,
5.33823529509463));
#59595=CARTESIAN_POINT('Ctrl Pts',(-0.674131559565751,-2.86865233256197,
5.39108910989754));
#59596=CARTESIAN_POINT('Ctrl Pts',(0.272654872748948,-3.09114657034351,
5.44394292470046));
#59597=CARTESIAN_POINT('Ctrl Pts',(1.34045235148189,-2.79869885703692,5.49679673950337));
#59598=CARTESIAN_POINT('Ctrl Pts',(2.04174345790288,-2.1248301618769,5.54965055430629));
#59599=CARTESIAN_POINT('Ctrl Pts',(2.74303456432387,-1.45096146671689,5.60250436910921));
#59600=CARTESIAN_POINT('Ctrl Pts',(3.07781929843291,-0.395671789703455,
5.65535818391213));
#59601=CARTESIAN_POINT('Ctrl Pts',(2.8932471500414,0.559232056921528,5.70821199871505));
#59602=CARTESIAN_POINT('Ctrl Pts',(2.70867500164989,1.5141359035465,5.76106581351796));
#59603=CARTESIAN_POINT('Ctrl Pts',(2.00474597075782,2.36865391978304,5.81391962832088));
#59604=CARTESIAN_POINT('Ctrl Pts',(1.10284840201293,2.73264431766924,5.86677344312379));
#59605=CARTESIAN_POINT('Ctrl Pts',(0.200950833268036,3.09663471555545,5.91962725792671));
#59606=CARTESIAN_POINT('Ctrl Pts',(-0.898915273329681,2.97009749509133,
5.97248107272963));
#59607=CARTESIAN_POINT('Ctrl Pts',(-1.69459113213402,2.4108049401817,6.02533488753255));
#59608=CARTESIAN_POINT('Ctrl Pts',(-2.45979488521509,1.87293168771145,6.07616455265852));
#59609=CARTESIAN_POINT('Ctrl Pts',(-2.94366147355347,0.934814970161849,
6.12699421778449));
#59610=CARTESIAN_POINT('Ctrl Pts',(-2.94660273288284,-0.000682925830890656,
6.17782388291046));
#59611=CARTESIAN_POINT('Origin',(0.,0.,0.));
#59612=CARTESIAN_POINT('',(-2.94613349194407,0.00134377452219305,7.3221761170896));
#59613=CARTESIAN_POINT('',(-2.94097104012875,0.00263417315905663,7.17782388291047));
#59614=CARTESIAN_POINT('',(-2.942,-3.60291088309151E-16,0.));
#59615=CARTESIAN_POINT('Ctrl Pts',(-2.94613349194407,0.00134377452219305,
7.3221761170896));
#59616=CARTESIAN_POINT('Ctrl Pts',(-2.94655901031452,0.076401152092742,
7.31809965535512));
#59617=CARTESIAN_POINT('Ctrl Pts',(-2.94394049027812,0.151428352789515,
7.31402319362065));
#59618=CARTESIAN_POINT('Ctrl Pts',(-2.93818267368556,0.226213855655731,
7.30994673188618));
#59619=CARTESIAN_POINT('Ctrl Pts',(-2.86325215321475,1.19945024888809,7.25689686575499));
#59620=CARTESIAN_POINT('Ctrl Pts',(-2.25666138625707,2.13175354584505,7.2038469996238));
#59621=CARTESIAN_POINT('Ctrl Pts',(-1.39724160877638,2.5945724154744,7.15079713349261));
#59622=CARTESIAN_POINT('Ctrl Pts',(-0.537821831295674,3.05739128510375,
7.09774726736142));
#59623=CARTESIAN_POINT('Ctrl Pts',(0.574426956708044,3.05072572740549,7.04469740123023));
#59624=CARTESIAN_POINT('Ctrl Pts',(1.42823798173304,2.57763969552996,6.99164753509903));
#59625=CARTESIAN_POINT('Ctrl Pts',(2.28204900675803,2.10455366365443,6.93859766896784));
#59626=CARTESIAN_POINT('Ctrl Pts',(2.8774222688043,1.16504715760165,6.88554780283665));
#59627=CARTESIAN_POINT('Ctrl Pts',(2.94068287606827,0.190982603489069,6.83249793670546));
#59628=CARTESIAN_POINT('Ctrl Pts',(3.00394348333225,-0.783081950623512,
6.77944807057427));
#59629=CARTESIAN_POINT('Ctrl Pts',(2.53509143581391,-1.7917045527959,6.72639820444308));
#59630=CARTESIAN_POINT('Ctrl Pts',(1.74964368994405,-2.37125221996219,6.67334833831189));
#59631=CARTESIAN_POINT('Ctrl Pts',(0.964195944074186,-2.95079988712848,
6.62029847218069));
#59632=CARTESIAN_POINT('Ctrl Pts',(-0.137847500147206,-3.10127261928869,
6.5672486060495));
#59633=CARTESIAN_POINT('Ctrl Pts',(-1.04991095384295,-2.75350270045941,
6.51419873991831));
#59634=CARTESIAN_POINT('Ctrl Pts',(-1.96197440753872,-2.40573278163011,
6.46114887378712));
#59635=CARTESIAN_POINT('Ctrl Pts',(-2.68405787070882,-1.55972021181128,
6.40809900765593));
#59636=CARTESIAN_POINT('Ctrl Pts',(-2.88424164481483,-0.604351112146305,
6.35504914152473));
#59637=CARTESIAN_POINT('Ctrl Pts',(-2.92559045225217,-0.407015573289341,
6.34409146671302));
#59638=CARTESIAN_POINT('Ctrl Pts',(-2.94467258987502,-0.205014375890775,
6.33313379190131));
#59639=CARTESIAN_POINT('Ctrl Pts',(-2.94279128603782,-0.00266058177182005,
6.32217611708959));
#59640=CARTESIAN_POINT('Ctrl Pts',(-2.94660273288284,-0.000682925830890656,
6.17782388291046));
#59641=CARTESIAN_POINT('Ctrl Pts',(-2.94671986033404,-0.03793652093653,
6.1798480325874));
#59642=CARTESIAN_POINT('Ctrl Pts',(-2.94607433229542,-0.0751859630926007,
6.18187218226435));
#59643=CARTESIAN_POINT('Ctrl Pts',(-2.94465354469403,-0.11240581138343,
6.1838963319413));
#59644=CARTESIAN_POINT('Ctrl Pts',(-2.90755448743874,-1.08427611868375,
6.23675014674421));
#59645=CARTESIAN_POINT('Ctrl Pts',(-2.3418707619172,-2.03596884392924,6.28960396154713));
#59646=CARTESIAN_POINT('Ctrl Pts',(-1.50587294394191,-2.53297576802774,
6.34245777635005));
#59647=CARTESIAN_POINT('Ctrl Pts',(-0.66987512596661,-3.02998269212625,
6.39531159115297));
#59648=CARTESIAN_POINT('Ctrl Pts',(0.436436784462447,-3.07230381507775,
6.44816540595589));
#59649=CARTESIAN_POINT('Ctrl Pts',(1.30796108255195,-2.64061685430534,6.5010192207588));
#59650=CARTESIAN_POINT('Ctrl Pts',(2.17948538064144,-2.20892989353293,6.55387303556172));
#59651=CARTESIAN_POINT('Ctrl Pts',(2.81622206639138,-1.30323484903661,6.60672685036463));
#59652=CARTESIAN_POINT('Ctrl Pts',(2.9274603714869,-0.337039075013164,6.65958066516755));
#59653=CARTESIAN_POINT('Ctrl Pts',(3.03869867658241,0.629156699010298,6.71243447997047));
#59654=CARTESIAN_POINT('Ctrl Pts',(2.62443860102348,1.65585320256089,6.76528829477339));
#59655=CARTESIAN_POINT('Ctrl Pts',(1.87381619985943,2.27429822447636,6.81814210957631));
#59656=CARTESIAN_POINT('Ctrl Pts',(1.12319379869538,2.89274324639182,6.87099592437922));
#59657=CARTESIAN_POINT('Ctrl Pts',(0.0362090719262038,3.10293678667218,
6.92384973918214));
#59658=CARTESIAN_POINT('Ctrl Pts',(-0.890860363440002,2.80891213418353,
6.97670355398506));
#59659=CARTESIAN_POINT('Ctrl Pts',(-1.81792979880623,2.51488748169487,7.02955736878797));
#59660=CARTESIAN_POINT('Ctrl Pts',(-2.58508394276949,1.7166446364372,7.08241118359089));
#59661=CARTESIAN_POINT('Ctrl Pts',(-2.84206816794824,0.778632193944778,
7.13526499839381));
#59662=CARTESIAN_POINT('Ctrl Pts',(-2.91104434310083,0.526863780986117,
7.1494512932327));
#59663=CARTESIAN_POINT('Ctrl Pts',(-2.943266897151,0.265026097713286,7.16363758807158));
#59664=CARTESIAN_POINT('Ctrl Pts',(-2.94097104012875,0.00263417315905663,
7.17782388291047));
#59665=CARTESIAN_POINT('Origin',(0.,0.,0.));
#59666=CARTESIAN_POINT('',(-2.93863545697552,0.00202987236895366,8.3221761170896));
#59667=CARTESIAN_POINT('',(-2.93764652921007,-0.00116347631119334,8.17782388291046));
#59668=CARTESIAN_POINT('',(-2.942,-3.60291088309151E-16,0.));
#59669=CARTESIAN_POINT('Ctrl Pts',(-2.93863545697552,0.00202987236895366,
8.3221761170896));
#59670=CARTESIAN_POINT('Ctrl Pts',(-2.9408741470766,0.356210246758157,8.30306551880894));
#59671=CARTESIAN_POINT('Ctrl Pts',(-2.88168510873734,0.709667537581135,
8.28395492052829));
#59672=CARTESIAN_POINT('Ctrl Pts',(-2.75773880406503,1.0387332771172,8.26484432224763));
#59673=CARTESIAN_POINT('Ctrl Pts',(-2.41367135134812,1.9521998873394,8.21179445611644));
#59674=CARTESIAN_POINT('Ctrl Pts',(-1.57059473032904,2.67770909277114,8.15874458998524));
#59675=CARTESIAN_POINT('Ctrl Pts',(-0.616045496221141,2.88176648585937,
8.10569472385405));
#59676=CARTESIAN_POINT('Ctrl Pts',(0.338503737886761,3.08582387894761,8.05264485772286));
#59677=CARTESIAN_POINT('Ctrl Pts',(1.40452558508349,2.76842945969235,7.99959499159167));
#59678=CARTESIAN_POINT('Ctrl Pts',(2.09200238369389,2.07547974190444,7.94654512546048));
#59679=CARTESIAN_POINT('Ctrl Pts',(2.77947918230429,1.38253002411653,7.89349525932929));
#59680=CARTESIAN_POINT('Ctrl Pts',(3.08841093232836,0.314025007795969,7.8404453931981));
#59681=CARTESIAN_POINT('Ctrl Pts',(2.87679115035106,-0.638876208430471,
7.78739552706691));
#59682=CARTESIAN_POINT('Ctrl Pts',(2.66517136837375,-1.59177742465692,7.73434566093571));
#59683=CARTESIAN_POINT('Ctrl Pts',(1.93300005439505,-2.42907484078926,7.68129579480452));
#59684=CARTESIAN_POINT('Ctrl Pts',(1.01683398364893,-2.76588842546718,7.62824592867333));
#59685=CARTESIAN_POINT('Ctrl Pts',(0.100667912902824,-3.10270201014509,
7.57519606254214));
#59686=CARTESIAN_POINT('Ctrl Pts',(-0.999492914610703,-2.93903176336861,
7.52214619641095));
#59687=CARTESIAN_POINT('Ctrl Pts',(-1.7779381913755,-2.35011189522649,7.46909633027976));
#59688=CARTESIAN_POINT('Ctrl Pts',(-2.49656611864381,-1.80644585112258,
7.42012292588304));
#59689=CARTESIAN_POINT('Ctrl Pts',(-2.94102144022082,-0.900373338050325,
7.37114952148632));
#59690=CARTESIAN_POINT('Ctrl Pts',(-2.94613349194407,0.00134377452219305,
7.3221761170896));
#59691=CARTESIAN_POINT('Ctrl Pts',(-2.94097104012875,0.00263417315905663,
7.17782388291047));
#59692=CARTESIAN_POINT('Ctrl Pts',(-2.93471323298103,-0.712566314094985,
7.2164914028745));
#59693=CARTESIAN_POINT('Ctrl Pts',(-2.67200379227269,-1.43188449036145,
7.25515892283853));
#59694=CARTESIAN_POINT('Ctrl Pts',(-2.19810644885855,-1.9626379197902,7.29382644280256));
#59695=CARTESIAN_POINT('Ctrl Pts',(-1.55034619819585,-2.68811355130562,
7.34668025760548));
#59696=CARTESIAN_POINT('Ctrl Pts',(-0.50801139047619,-3.0612827746093,7.39953407240839));
#59697=CARTESIAN_POINT('Ctrl Pts',(0.453005883307361,-2.91177012045952,
7.45238788721131));
#59698=CARTESIAN_POINT('Ctrl Pts',(1.41402315709093,-2.76225746630973,7.50524170201423));
#59699=CARTESIAN_POINT('Ctrl Pts',(2.2937228969384,-2.09006293470645,7.55809551681715));
#59700=CARTESIAN_POINT('Ctrl Pts',(2.69046625749842,-1.20208605431325,7.61094933162007));
#59701=CARTESIAN_POINT('Ctrl Pts',(3.08720961805843,-0.31410917392004,7.66380314642299));
#59702=CARTESIAN_POINT('Ctrl Pts',(3.000996599331,0.789650055263082,7.7166569612259));
#59703=CARTESIAN_POINT('Ctrl Pts',(2.47118892410342,1.60525538968118,7.76951077602881));
#59704=CARTESIAN_POINT('Ctrl Pts',(1.94138124887585,2.42086072409927,7.82236459083173));
#59705=CARTESIAN_POINT('Ctrl Pts',(0.967978917148135,2.94831216375233,7.87521840563465));
#59706=CARTESIAN_POINT('Ctrl Pts',(-0.00459803675616453,2.94679460138808,
7.92807222043756));
#59707=CARTESIAN_POINT('Ctrl Pts',(-0.977174990660472,2.94527703902382,
7.98092603524048));
#59708=CARTESIAN_POINT('Ctrl Pts',(-1.94892656674138,2.41479047464224,8.0337798500434));
#59709=CARTESIAN_POINT('Ctrl Pts',(-2.47618640555083,1.59753574284808,8.08663366484632));
#59710=CARTESIAN_POINT('Ctrl Pts',(-2.77941863111983,1.12752465355612,8.11703040420104));
#59711=CARTESIAN_POINT('Ctrl Pts',(-2.935634717328,0.562664672081437,8.14742714355575));
#59712=CARTESIAN_POINT('Ctrl Pts',(-2.93764652921007,-0.00116347631119334,
8.17782388291046));
#59713=CARTESIAN_POINT('Origin',(0.,0.,0.));
#59714=CARTESIAN_POINT('',(-2.93871642317227,-0.00207197768594736,9.3221761170896));
#59715=CARTESIAN_POINT('',(-2.94520105889964,-0.0018935710546995,9.17782388291047));
#59716=CARTESIAN_POINT('',(-2.942,-3.60291088309151E-16,0.));
#59717=CARTESIAN_POINT('Ctrl Pts',(-2.93871642317227,-0.00207197768594736,
9.3221761170896));
#59718=CARTESIAN_POINT('Ctrl Pts',(-2.93462655422571,0.63069516315242,9.28803138226276));
#59719=CARTESIAN_POINT('Ctrl Pts',(-2.73431821504367,1.26582298942305,9.25388664743592));
#59720=CARTESIAN_POINT('Ctrl Pts',(-2.35730441600429,1.76839080033892,9.21974191260908));
#59721=CARTESIAN_POINT('Ctrl Pts',(-1.77154700215763,2.54921850997377,9.16669204647789));
#59722=CARTESIAN_POINT('Ctrl Pts',(-0.759238489877945,3.01005825656821,
9.11364218034669));
#59723=CARTESIAN_POINT('Ctrl Pts',(0.214293837547277,2.93907609354129,9.0605923142155));
#59724=CARTESIAN_POINT('Ctrl Pts',(1.18782616497251,2.86809393051436,9.0075424480843));
#59725=CARTESIAN_POINT('Ctrl Pts',(2.12258230754328,2.26528985786606,8.95449258195312));
#59726=CARTESIAN_POINT('Ctrl Pts',(2.58888343604653,1.40775448392131,8.90144271582193));
#59727=CARTESIAN_POINT('Ctrl Pts',(3.05518456454977,0.550219109976561,8.84839284969073));
#59728=CARTESIAN_POINT('Ctrl Pts',(3.05303067898551,-0.562047565264635,
8.79534298355954));
#59729=CARTESIAN_POINT('Ctrl Pts',(2.58341185471709,-1.41777054608419,8.74229311742835));
#59730=CARTESIAN_POINT('Ctrl Pts',(2.11379303044867,-2.27349352690374,8.68924325129716));
#59731=CARTESIAN_POINT('Ctrl Pts',(1.17670926747611,-2.87267281330165,8.63619338516597));
#59732=CARTESIAN_POINT('Ctrl Pts',(0.202909330970668,-2.93988400040574,
8.58314351903477));
#59733=CARTESIAN_POINT('Ctrl Pts',(-0.770890605534777,-3.00709518750983,
8.53009365290358));
#59734=CARTESIAN_POINT('Ctrl Pts',(-1.7814067155731,-2.54233827532011,8.47704378677239));
#59735=CARTESIAN_POINT('Ctrl Pts',(-2.3641356283849,-1.75924781171891,8.4239939206412));
#59736=CARTESIAN_POINT('Ctrl Pts',(-2.73694321676338,-1.25825659470745,
8.39005465279067));
#59737=CARTESIAN_POINT('Ctrl Pts',(-2.93465967862159,-0.626973072346038,
8.35611538494013));
#59738=CARTESIAN_POINT('Ctrl Pts',(-2.93863545697552,0.00202987236895366,
8.3221761170896));
#59739=CARTESIAN_POINT('Ctrl Pts',(-2.93764652921007,-0.00116347631119334,
8.17782388291046));
#59740=CARTESIAN_POINT('Ctrl Pts',(-2.93913285347321,-0.417719052240401,
8.20028095835866));
#59741=CARTESIAN_POINT('Ctrl Pts',(-2.85645082861081,-0.833711429208547,
8.22273803380687));
#59742=CARTESIAN_POINT('Ctrl Pts',(-2.68670181103504,-1.21047632909238,
8.24519510925507));
#59743=CARTESIAN_POINT('Ctrl Pts',(-2.28718927617178,-2.09721077003196,
8.29804892405799));
#59744=CARTESIAN_POINT('Ctrl Pts',(-1.40539610490722,-2.7666567527044,8.35090273886091));
#59745=CARTESIAN_POINT('Ctrl Pts',(-0.443916927094085,-2.91316963573206,
8.40375655366382));
#59746=CARTESIAN_POINT('Ctrl Pts',(0.517562250719054,-3.05968251875972,
8.45661036846674));
#59747=CARTESIAN_POINT('Ctrl Pts',(1.55872743508076,-2.68326230214263,8.50946418326965));
#59748=CARTESIAN_POINT('Ctrl Pts',(2.20422054240271,-1.95576874020468,8.56231799807257));
#59749=CARTESIAN_POINT('Ctrl Pts',(2.84971364972467,-1.22827517826673,8.61517181287549));
#59750=CARTESIAN_POINT('Ctrl Pts',(3.09953468000683,-0.149708271007917,
8.66802562767841));
#59751=CARTESIAN_POINT('Ctrl Pts',(2.8396244541884,0.787497634210531,8.72087944248132));
#59752=CARTESIAN_POINT('Ctrl Pts',(2.57971422836996,1.72470353942896,8.77373325728424));
#59753=CARTESIAN_POINT('Ctrl Pts',(1.81007274645093,2.52054844260704,8.82658707208716));
#59754=CARTESIAN_POINT('Ctrl Pts',(0.882090263685985,2.8116785611841,8.87944088689007));
#59755=CARTESIAN_POINT('Ctrl Pts',(-0.0458922190789657,3.10280867976116,
8.93229470169299));
#59756=CARTESIAN_POINT('Ctrl Pts',(-1.13221570268984,2.88922401373721,8.98514851649591));
#59757=CARTESIAN_POINT('Ctrl Pts',(-1.88090446966924,2.26843953868958,9.03800233129883));
#59758=CARTESIAN_POINT('Ctrl Pts',(-2.54110799810967,1.72102368459441,9.08460951516938));
#59759=CARTESIAN_POINT('Ctrl Pts',(-2.93876870791001,0.856971595110357,
9.13121669903992));
#59760=CARTESIAN_POINT('Ctrl Pts',(-2.94520105889964,-0.0018935710546995,
9.17782388291047));
#59761=CARTESIAN_POINT('Origin',(0.,0.,0.));
#59762=CARTESIAN_POINT('',(-2.94620168531707,-0.00128244101107317,10.3221761170896));
#59763=CARTESIAN_POINT('',(-2.94330664216,0.0025268841526987,10.1778238829105));
#59764=CARTESIAN_POINT('',(-2.942,-3.60291088309151E-16,0.));
#59765=CARTESIAN_POINT('Ctrl Pts',(-2.94620168531707,-0.00128244101107317,
10.3221761170896));
#59766=CARTESIAN_POINT('Ctrl Pts',(-2.94126630412904,0.904162302447864,
10.2729972457166));
#59767=CARTESIAN_POINT('Ctrl Pts',(-2.49257491833407,1.81383213622128,10.2238183743435));
#59768=CARTESIAN_POINT('Ctrl Pts',(-1.76882298743563,2.35698013813353,10.1746395029705));
#59769=CARTESIAN_POINT('Ctrl Pts',(-0.988102690804116,2.9428807085698,10.1215896368393));
#59770=CARTESIAN_POINT('Ctrl Pts',(0.112683772548088,3.10228885822241,10.0685397707081));
#59771=CARTESIAN_POINT('Ctrl Pts',(1.02753850943148,2.76192953278536,10.0154899045769));
#59772=CARTESIAN_POINT('Ctrl Pts',(1.94239324631488,2.42157020734831,9.96244003844575));
#59773=CARTESIAN_POINT('Ctrl Pts',(2.67131625672946,1.58144340682159,9.90939017231457));
#59774=CARTESIAN_POINT('Ctrl Pts',(2.87924391130981,0.627729744095369,9.85634030618337));
#59775=CARTESIAN_POINT('Ctrl Pts',(3.08717156589015,-0.325983918630861,
9.80329044005218));
#59776=CARTESIAN_POINT('Ctrl Pts',(2.77410386463627,-1.39328444355657,9.75024057392098));
#59777=CARTESIAN_POINT('Ctrl Pts',(2.08394846133389,-2.08356639993563,9.69719070778979));
#59778=CARTESIAN_POINT('Ctrl Pts',(1.39379305803153,-2.77384835631469,9.6441408416586));
#59779=CARTESIAN_POINT('Ctrl Pts',(0.326549952680647,-3.08711174414709,
9.59109097552742));
#59780=CARTESIAN_POINT('Ctrl Pts',(-0.627201817996116,-2.87935895850778,
9.53804110939623));
#59781=CARTESIAN_POINT('Ctrl Pts',(-1.58095358867288,-2.67160617286848,
9.48499124326504));
#59782=CARTESIAN_POINT('Ctrl Pts',(-2.42121402467556,-1.94283721375749,
9.43194137713383));
#59783=CARTESIAN_POINT('Ctrl Pts',(-2.76174108497008,-1.02804489786436,
9.37889151100264));
#59784=CARTESIAN_POINT('Ctrl Pts',(-2.88309311197862,-0.702044662436785,
9.35998637969829));
#59785=CARTESIAN_POINT('Ctrl Pts',(-2.94098088678121,-0.35242016294182,
9.34108124839394));
#59786=CARTESIAN_POINT('Ctrl Pts',(-2.93871642317227,-0.00207197768594736,
9.3221761170896));
#59787=CARTESIAN_POINT('Ctrl Pts',(-2.94520105889964,-0.0018935710546995,
9.17782388291047));
#59788=CARTESIAN_POINT('Ctrl Pts',(-2.94606316897201,-0.117004875110373,
9.18407051384284));
#59789=CARTESIAN_POINT('Ctrl Pts',(-2.93989752914462,-0.232023004939246,
9.19031714477521));
#59790=CARTESIAN_POINT('Ctrl Pts',(-2.92639431994892,-0.346173148702556,
9.19656377570758));
#59791=CARTESIAN_POINT('Ctrl Pts',(-2.81214135290127,-1.3120170769757,9.2494175905105));
#59792=CARTESIAN_POINT('Ctrl Pts',(-2.17258136845806,-2.21572064945068,
9.30227140531341));
#59793=CARTESIAN_POINT('Ctrl Pts',(-1.29971415023778,-2.64468574548728,
9.35512522011633));
#59794=CARTESIAN_POINT('Ctrl Pts',(-0.426846932017496,-3.07365084152388,
9.40797903491925));
#59795=CARTESIAN_POINT('Ctrl Pts',(0.679327519979847,-3.02787746112211,
9.46083284972217));
#59796=CARTESIAN_POINT('Ctrl Pts',(1.51377025947196,-2.528264061812,9.51368666452509));
#59797=CARTESIAN_POINT('Ctrl Pts',(2.34821299896408,-2.02865066250189,9.566540479328));
#59798=CARTESIAN_POINT('Ctrl Pts',(2.91092402595096,-1.07519724428343,9.61939429413091));
#59799=CARTESIAN_POINT('Ctrl Pts',(2.9449899904472,-0.103215894501322,9.67224810893383));
#59800=CARTESIAN_POINT('Ctrl Pts',(2.97905595494345,0.868765455280781,9.72510192373675));
#59801=CARTESIAN_POINT('Ctrl Pts',(2.48447685694907,1.85927473662654,9.77795573853967));
#59802=CARTESIAN_POINT('Ctrl Pts',(1.68705949036834,2.41608150538637,9.83080955334259));
#59803=CARTESIAN_POINT('Ctrl Pts',(0.889642123787608,2.97288827414619,9.8836633681455));
#59804=CARTESIAN_POINT('Ctrl Pts',(-0.210613511379468,3.09599253032006,
9.93651718294842));
#59805=CARTESIAN_POINT('Ctrl Pts',(-1.11137078493627,2.72918935640275,9.98937099775133));
#59806=CARTESIAN_POINT('Ctrl Pts',(-2.01212805849309,2.36238618248543,10.0422248125543));
#59807=CARTESIAN_POINT('Ctrl Pts',(-2.71338697043961,1.50567557847691,10.0950786273572));
#59808=CARTESIAN_POINT('Ctrl Pts',(-2.89497825514053,0.550200388018259,
10.1479324421601));
#59809=CARTESIAN_POINT('Ctrl Pts',(-2.9292111996477,0.370077596184809,10.1578962557436));
#59810=CARTESIAN_POINT('Ctrl Pts',(-2.94497596099191,0.186444863810624,
10.167860069327));
#59811=CARTESIAN_POINT('Ctrl Pts',(-2.94330664216,0.0025268841526987,10.1778238829105));
#59812=CARTESIAN_POINT('Origin',(0.,0.,0.));
#59813=CARTESIAN_POINT('',(-2.94267506677377,0.0026741096853234,11.3221761170896));
#59814=CARTESIAN_POINT('',(-2.93720511247626,7.6518416280307E-5,11.1778238829105));
#59815=CARTESIAN_POINT('',(-2.942,-3.60291088309151E-16,0.));
#59816=CARTESIAN_POINT('Ctrl Pts',(-2.94267506677377,0.0026741096853234,
11.3221761170896));
#59817=CARTESIAN_POINT('Ctrl Pts',(-2.94459362275203,0.208843135527949,
11.3110129753016));
#59818=CARTESIAN_POINT('Ctrl Pts',(-2.92478181403725,0.414645989663669,
11.2998498335136));
#59819=CARTESIAN_POINT('Ctrl Pts',(-2.88187939068302,0.615517107798873,
11.2886866917255));
#59820=CARTESIAN_POINT('Ctrl Pts',(-2.67799701967457,1.57010374022251,11.2356368255943));
#59821=CARTESIAN_POINT('Ctrl Pts',(-1.95264240634497,2.41331337073947,11.1825869594632));
#59822=CARTESIAN_POINT('Ctrl Pts',(-1.0392388969828,2.75754830373552,11.129537093332));
#59823=CARTESIAN_POINT('Ctrl Pts',(-0.125835387620612,3.10178323673157,
11.0764872272008));
#59824=CARTESIAN_POINT('Ctrl Pts',(0.97561701777415,2.94704347220669,11.0234373610696));
#59825=CARTESIAN_POINT('Ctrl Pts',(1.75881431280863,2.3644581505064,10.9703874949384));
#59826=CARTESIAN_POINT('Ctrl Pts',(2.5420116078431,1.78187282880611,10.9173376288072));
#59827=CARTESIAN_POINT('Ctrl Pts',(3.0069537925173,0.771441949930418,10.864287762676));
#59828=CARTESIAN_POINT('Ctrl Pts',(2.93992115485034,-0.202370293521759,
10.8112378965448));
#59829=CARTESIAN_POINT('Ctrl Pts',(2.87288851718338,-1.17618253697395,10.7581880304136));
#59830=CARTESIAN_POINT('Ctrl Pts',(2.27388105717527,-2.11337614500262,10.7051381642824));
#59831=CARTESIAN_POINT('Ctrl Pts',(1.41824419635842,-2.58315186002146,10.6520882981512));
#59832=CARTESIAN_POINT('Ctrl Pts',(0.562607335541579,-3.05292757504029,
10.59903843202));
#59833=CARTESIAN_POINT('Ctrl Pts',(-0.549658926083981,-3.05528539704932,
10.5459885658889));
#59834=CARTESIAN_POINT('Ctrl Pts',(-1.40727978292664,-2.58914150733454,
10.4929386997577));
#59835=CARTESIAN_POINT('Ctrl Pts',(-2.26490063976931,-2.12299761761977,
10.4398888336265));
#59836=CARTESIAN_POINT('Ctrl Pts',(-2.86787609182906,-1.18835201618118,
10.3868389674953));
#59837=CARTESIAN_POINT('Ctrl Pts',(-2.93903675290352,-0.214832719851918,
10.3337891013641));
#59838=CARTESIAN_POINT('Ctrl Pts',(-2.9442292739426,-0.143796007266396,
10.3299181066059));
#59839=CARTESIAN_POINT('Ctrl Pts',(-2.94659016179437,-0.0725523127645525,
10.3260471118478));
#59840=CARTESIAN_POINT('Ctrl Pts',(-2.94620168531707,-0.00128244101107317,
10.3221761170896));
#59841=CARTESIAN_POINT('Ctrl Pts',(-2.94330664216,0.0025268841526987,10.1778238829105));
#59842=CARTESIAN_POINT('Ctrl Pts',(-2.93612093097255,-0.789162192096626,
10.2207138841299));
#59843=CARTESIAN_POINT('Ctrl Pts',(-2.60589249191516,-1.58613672417313,
10.2636038853494));
#59844=CARTESIAN_POINT('Ctrl Pts',(-2.0351025661624,-2.13119147659499,10.3064938865688));
#59845=CARTESIAN_POINT('Ctrl Pts',(-1.33171193502808,-2.80286837384081,
10.3593477013718));
#59846=CARTESIAN_POINT('Ctrl Pts',(-0.263007015304154,-3.09198239142367,
10.4122015161747));
#59847=CARTESIAN_POINT('Ctrl Pts',(0.68308046979022,-2.86653460410006,10.4650553309776));
#59848=CARTESIAN_POINT('Ctrl Pts',(1.62916795488458,-2.64108681677646,10.5179091457805));
#59849=CARTESIAN_POINT('Ctrl Pts',(2.4526380053494,-1.90107722454637,10.5707629605834));
#59850=CARTESIAN_POINT('Ctrl Pts',(2.77752420302081,-0.984367241605259,
10.6236167753863));
#59851=CARTESIAN_POINT('Ctrl Pts',(3.10241040069222,-0.0676572586641361,
10.6764705901893));
#59852=CARTESIAN_POINT('Ctrl Pts',(2.92871274557025,1.02575311498802,10.7293244049922));
#59853=CARTESIAN_POINT('Ctrl Pts',(2.33573525751911,1.79665254612406,10.7821782197951));
#59854=CARTESIAN_POINT('Ctrl Pts',(1.74275776946797,2.5675519772601,10.835032034598));
#59855=CARTESIAN_POINT('Ctrl Pts',(0.730500448487692,3.01594046588001,10.8878858494009));
#59856=CARTESIAN_POINT('Ctrl Pts',(-0.23887689886381,2.93710016715487,10.9407396642038));
#59857=CARTESIAN_POINT('Ctrl Pts',(-1.20825424621531,2.85825986842973,10.9935934790068));
#59858=CARTESIAN_POINT('Ctrl Pts',(-2.13475161993805,2.2521907823595,11.0464472938097));
#59859=CARTESIAN_POINT('Ctrl Pts',(-2.5953640803379,1.3956019687589,11.0993011086126));
#59860=CARTESIAN_POINT('Ctrl Pts',(-2.82346851267095,0.971402187234134,
11.1254753667119));
#59861=CARTESIAN_POINT('Ctrl Pts',(-2.93731807226522,0.48576427202227,11.1516496248112));
#59862=CARTESIAN_POINT('Ctrl Pts',(-2.93720511247626,7.6518416280307E-5,
11.1778238829105));
#59863=CARTESIAN_POINT('Origin',(0.,0.,0.));
#59864=CARTESIAN_POINT('',(-2.93712622074894,0.000100805557199934,12.3221761170896));
#59865=CARTESIAN_POINT('',(-2.9430272628276,-0.00257481030056199,12.1778238829105));
#59866=CARTESIAN_POINT('',(-2.942,-3.60291088309151E-16,0.));
#59867=CARTESIAN_POINT('Ctrl Pts',(-2.93712622074894,0.000100805557199934,
12.3221761170896));
#59868=CARTESIAN_POINT('Ctrl Pts',(-2.93727410781314,0.486244108806712,
12.2959788387554));
#59869=CARTESIAN_POINT('Ctrl Pts',(-2.82330164211032,0.972322158399294,
12.2697815604212));
#59870=CARTESIAN_POINT('Ctrl Pts',(-2.59482855910859,1.3967658648718,12.243584282087));
#59871=CARTESIAN_POINT('Ctrl Pts',(-2.13216727371862,2.2562704867391,12.1905344159558));
#59872=CARTESIAN_POINT('Ctrl Pts',(-1.19997521215115,2.8630321833101,12.1374845498246));
#59873=CARTESIAN_POINT('Ctrl Pts',(-0.226752573949602,2.93814114750192,
12.0844346836934));
#59874=CARTESIAN_POINT('Ctrl Pts',(0.74647006425197,3.01325011169373,12.0313848175622));
#59875=CARTESIAN_POINT('Ctrl Pts',(1.76072327908759,2.55670634350636,11.978334951431));
#59876=CARTESIAN_POINT('Ctrl Pts',(2.349785866942,1.77836905954762,11.9252850852998));
#59877=CARTESIAN_POINT('Ctrl Pts',(2.93884845479638,1.00003177558891,11.8722352191686));
#59878=CARTESIAN_POINT('Ctrl Pts',(3.10272041566954,-0.100099024141179,
11.8191853530375));
#59879=CARTESIAN_POINT('Ctrl Pts',(2.76607481766758,-1.01632683498072,11.7661354869063));
#59880=CARTESIAN_POINT('Ctrl Pts',(2.4294292196656,-1.93255464582029,11.7130856207751));
#59881=CARTESIAN_POINT('Ctrl Pts',(1.59226606278853,-2.66487946776933,11.6600357546439));
#59882=CARTESIAN_POINT('Ctrl Pts',(0.639403663520396,-2.87667396267171,
11.6069858885127));
#59883=CARTESIAN_POINT('Ctrl Pts',(-0.313458735747721,-3.08846845757408,
11.5539360223815));
#59884=CARTESIAN_POINT('Ctrl Pts',(-1.38202037740687,-2.77973262542978,
11.5008861562503));
#59885=CARTESIAN_POINT('Ctrl Pts',(-2.07509613389281,-2.09238289219248,
11.4478362901191));
#59886=CARTESIAN_POINT('Ctrl Pts',(-2.62232980813185,-1.54967032940742,
11.4059495657759));
#59887=CARTESIAN_POINT('Ctrl Pts',(-2.93547619508296,-0.770920396015258,
11.3640628414328));
#59888=CARTESIAN_POINT('Ctrl Pts',(-2.94267506677377,0.0026741096853234,
11.3221761170896));
#59889=CARTESIAN_POINT('Ctrl Pts',(-2.93720511247626,7.6518416280307E-5,
11.1778238829105));
#59890=CARTESIAN_POINT('Ctrl Pts',(-2.93708997197894,-0.494987521734636,
11.2045034396141));
#59891=CARTESIAN_POINT('Ctrl Pts',(-2.81856970692698,-0.990103343131662,
11.2311829963177));
#59892=CARTESIAN_POINT('Ctrl Pts',(-2.58195393144776,-1.42025823729116,
11.2578625530213));
#59893=CARTESIAN_POINT('Ctrl Pts',(-2.11320377508074,-2.27242108860962,
11.3107163678243));
#59894=CARTESIAN_POINT('Ctrl Pts',(-1.18097591526968,-2.86963825011554,
11.3635701826272));
#59895=CARTESIAN_POINT('Ctrl Pts',(-0.210891622840258,-2.93924212819014,
11.4164239974301));
#59896=CARTESIAN_POINT('Ctrl Pts',(0.75919266958915,-3.00884600626475,11.469277812233));
#59897=CARTESIAN_POINT('Ctrl Pts',(1.76713339463694,-2.55083660090805,11.5221316270359));
#59898=CARTESIAN_POINT('Ctrl Pts',(2.35274154615311,-1.77432431694913,11.5749854418389));
#59899=CARTESIAN_POINT('Ctrl Pts',(2.93834969766929,-0.997812032990198,
11.6278392566418));
#59900=CARTESIAN_POINT('Ctrl Pts',(3.10162527565385,0.0972031295709437,
11.6806930714447));
#59901=CARTESIAN_POINT('Ctrl Pts',(2.76802260088771,1.01077714936912,11.7335468862476));
#59902=CARTESIAN_POINT('Ctrl Pts',(2.43441992612157,1.92435116916729,11.7864007010505));
#59903=CARTESIAN_POINT('Ctrl Pts',(1.60393899860469,2.65648404620246,11.8392545158534));
#59904=CARTESIAN_POINT('Ctrl Pts',(0.655747147489709,2.87291058741323,11.8921083306564));
#59905=CARTESIAN_POINT('Ctrl Pts',(-0.292444703625262,3.08933712862399,
11.9449621454593));
#59906=CARTESIAN_POINT('Ctrl Pts',(-1.35834747833835,2.79005733401037,11.9978159602622));
#59907=CARTESIAN_POINT('Ctrl Pts',(-2.05530881073343,2.11171145217178,12.0506697750651));
#59908=CARTESIAN_POINT('Ctrl Pts',(-2.61421830322617,1.56773012217451,12.0930544776802));
#59909=CARTESIAN_POINT('Ctrl Pts',(-2.93586860501076,0.779978635821696,
12.1354391802953));
#59910=CARTESIAN_POINT('Ctrl Pts',(-2.9430272628276,-0.00257481030056199,
12.1778238829105));
#59911=CARTESIAN_POINT('Origin',(0.,0.,0.));
#59912=CARTESIAN_POINT('',(-2.94230384945163,-0.00270653131051041,13.3221761170896));
#59913=CARTESIAN_POINT('',(-2.94542263194624,0.00177224128177641,13.1778238829105));
#59914=CARTESIAN_POINT('',(-2.942,-3.60291088309151E-16,0.));
#59915=CARTESIAN_POINT('Ctrl Pts',(-2.94230384945163,-0.00270653131051041,
13.3221761170896));
#59916=CARTESIAN_POINT('Ctrl Pts',(-2.9352201389254,0.75903152900975,13.2809447022092));
#59917=CARTESIAN_POINT('Ctrl Pts',(-2.63281541581416,1.52575687849258,13.2397132873288));
#59918=CARTESIAN_POINT('Ctrl Pts',(-2.10078289570291,2.06659172493232,13.1984818724484));
#59919=CARTESIAN_POINT('Ctrl Pts',(-1.41625014194664,2.7624498778951,13.1454320063172));
#59920=CARTESIAN_POINT('Ctrl Pts',(-0.351583517635692,3.08436100717369,
13.0923821401861));
#59921=CARTESIAN_POINT('Ctrl Pts',(0.603822270094866,2.88435240540648,13.0393322740549));
#59922=CARTESIAN_POINT('Ctrl Pts',(1.55922805782544,2.68434380363926,12.9862824079237));
#59923=CARTESIAN_POINT('Ctrl Pts',(2.40537300897562,1.96241547082624,12.9332325417925));
#59924=CARTESIAN_POINT('Ctrl Pts',(2.75331015075007,1.05041579682204,12.8801826756613));
#59925=CARTESIAN_POINT('Ctrl Pts',(3.10124729252453,0.138416122817822,12.8271328095301));
#59926=CARTESIAN_POINT('Ctrl Pts',(2.95097662492324,-0.963654892377583,
12.7740829433989));
#59927=CARTESIAN_POINT('Ctrl Pts',(2.37157298102772,-1.7492088863529,12.7210330772677));
#59928=CARTESIAN_POINT('Ctrl Pts',(1.7921693371322,-2.53476288032821,12.6679832111365));
#59929=CARTESIAN_POINT('Ctrl Pts',(0.783632716942436,-3.00379985308343,
12.6149333450053));
#59930=CARTESIAN_POINT('Ctrl Pts',(-0.190443419765153,-2.94071784370837,
12.5618834788741));
#59931=CARTESIAN_POINT('Ctrl Pts',(-1.16451955647273,-2.87763583433331,
12.5088336127429));
#59932=CARTESIAN_POINT('Ctrl Pts',(-2.10413520969813,-2.28243484282798,
12.4557837466118));
#59933=CARTESIAN_POINT('Ctrl Pts',(-2.57737778170459,-1.42871057349352,
12.4027338804806));
#59934=CARTESIAN_POINT('Ctrl Pts',(-2.8169219811687,-0.996575535866305,
12.3758812926836));
#59935=CARTESIAN_POINT('Ctrl Pts',(-2.93697463437708,-0.498203085629071,
12.3490287048866));
#59936=CARTESIAN_POINT('Ctrl Pts',(-2.93712622074894,0.000100805557199934,
12.3221761170896));
#59937=CARTESIAN_POINT('Ctrl Pts',(-2.9430272628276,-0.00257481030056199,
12.1778238829105));
#59938=CARTESIAN_POINT('Ctrl Pts',(-2.94479546661752,-0.195867185023464,
12.1882929950983));
#59939=CARTESIAN_POINT('Ctrl Pts',(-2.92737651745624,-0.388842427018477,
12.1987621072861));
#59940=CARTESIAN_POINT('Ctrl Pts',(-2.88960655205276,-0.577748681561196,
12.2092312194739));
#59941=CARTESIAN_POINT('Ctrl Pts',(-2.69892307089993,-1.53145096439204,
12.2620850342768));
#59942=CARTESIAN_POINT('Ctrl Pts',(-1.98953621851721,-2.38144356099016,
12.3149388490797));
#59943=CARTESIAN_POINT('Ctrl Pts',(-1.08532618196459,-2.73965082509689,
12.3677926638826));
#59944=CARTESIAN_POINT('Ctrl Pts',(-0.181116145411983,-3.09785808920362,
12.4206464786855));
#59945=CARTESIAN_POINT('Ctrl Pts',(0.917917075310514,-2.96428002081899,
12.4735002934884));
#59946=CARTESIAN_POINT('Ctrl Pts',(1.70999495989744,-2.39990349844265,12.5263541082914));
#59947=CARTESIAN_POINT('Ctrl Pts',(2.50207284448437,-1.83552697606631,12.5792079230943));
#59948=CARTESIAN_POINT('Ctrl Pts',(2.98719539293572,-0.840351999698262,
12.6320617378972));
#59949=CARTESIAN_POINT('Ctrl Pts',(2.94387332727614,0.131260800180532,12.6849155527001));
#59950=CARTESIAN_POINT('Ctrl Pts',(2.90055126161656,1.10287360005931,12.737769367503));
#59951=CARTESIAN_POINT('Ctrl Pts',(2.32878458184608,2.05092422344884,12.7906231823059));
#59952=CARTESIAN_POINT('Ctrl Pts',(1.48962111902714,2.54256730224792,12.8434769971089));
#59953=CARTESIAN_POINT('Ctrl Pts',(0.650457656208199,3.034210381047,12.8963308119118));
#59954=CARTESIAN_POINT('Ctrl Pts',(-0.456102589659198,3.06944591525562,
12.9491846267147));
#59955=CARTESIAN_POINT('Ctrl Pts',(-1.32484453286982,2.63218664392115,13.0020384415176));
#59956=CARTESIAN_POINT('Ctrl Pts',(-2.19358647608043,2.19492737258668,13.0548922563205));
#59957=CARTESIAN_POINT('Ctrl Pts',(-2.82451011663427,1.28517329570913,13.1077460711235));
#59958=CARTESIAN_POINT('Ctrl Pts',(-2.92955871082826,0.318284973761263,
13.1605998859264));
#59959=CARTESIAN_POINT('Ctrl Pts',(-2.94096978668171,0.213255143821896,
13.1663412182544));
#59960=CARTESIAN_POINT('Ctrl Pts',(-2.94617567004577,0.107551144246887,
13.1720825505824));
#59961=CARTESIAN_POINT('Ctrl Pts',(-2.94542263194624,0.00177224128177641,
13.1778238829105));
#59962=CARTESIAN_POINT('Origin',(0.,0.,0.));
#59963=CARTESIAN_POINT('',(-2.94640032942472,0.00108073188550471,14.3221761170896));
#59964=CARTESIAN_POINT('',(-2.93776462225576,0.00129977310561086,14.1778238829105));
#59965=CARTESIAN_POINT('',(-2.942,-3.60291088309151E-16,0.));
#59966=CARTESIAN_POINT('Ctrl Pts',(-2.94640032942472,0.00108073188550471,
14.3221761170896));
#59967=CARTESIAN_POINT('Ctrl Pts',(-2.94667898956338,0.0602749409108862,
14.3189604317942));
#59968=CARTESIAN_POINT('Ctrl Pts',(-2.94505040817207,0.119453520431582,
14.3157447464988));
#59969=CARTESIAN_POINT('Ctrl Pts',(-2.94146614700694,0.178513412517928,
14.3125290612034));
#59970=CARTESIAN_POINT('Ctrl Pts',(-2.88233580385349,1.15283741536734,14.2594791950723));
#59971=CARTESIAN_POINT('Ctrl Pts',(-2.29095107408328,2.09485965367689,14.2064293289411));
#59972=CARTESIAN_POINT('Ctrl Pts',(-1.43915344311655,2.57156129610056,14.1533794628099));
#59973=CARTESIAN_POINT('Ctrl Pts',(-0.587355812149814,3.04826293852424,
14.1003295966787));
#59974=CARTESIAN_POINT('Ctrl Pts',(0.524854720013437,3.05964398506203,14.0472797305475));
#59975=CARTESIAN_POINT('Ctrl Pts',(1.3862289649121,2.60047291646642,13.9942298644163));
#59976=CARTESIAN_POINT('Ctrl Pts',(2.24760320981075,2.14130184787082,13.9411799982851));
#59977=CARTESIAN_POINT('Ctrl Pts',(2.85814116744481,1.21157866414187,13.8881301321539));
#59978=CARTESIAN_POINT('Ctrl Pts',(2.93719719893692,0.238668697138423,13.8350802660227));
#59979=CARTESIAN_POINT('Ctrl Pts',(3.01625323042904,-0.734241269865052,
13.7820303998915));
#59980=CARTESIAN_POINT('Ctrl Pts',(2.56382733577916,-1.75033802014301,13.7289805337603));
#59981=CARTESIAN_POINT('Ctrl Pts',(1.78788587098706,-2.3425529331824,13.6759306676291));
#59982=CARTESIAN_POINT('Ctrl Pts',(1.01194440619497,-2.93476784622179,13.622880801498));
#59983=CARTESIAN_POINT('Ctrl Pts',(-0.0875126287393881,-3.10310092202263,
13.5698309353668));
#59984=CARTESIAN_POINT('Ctrl Pts',(-1.00509843823799,-2.77017459050656,
13.5167810692356));
#59985=CARTESIAN_POINT('Ctrl Pts',(-1.92268424773658,-2.43724825899049,
13.4637312031044));
#59986=CARTESIAN_POINT('Ctrl Pts',(-2.65839883179945,-1.60306252015755,
13.4106813369732));
#59987=CARTESIAN_POINT('Ctrl Pts',(-2.87405668223012,-0.65106706241757,
13.357631470842));
#59988=CARTESIAN_POINT('Ctrl Pts',(-2.92210094658066,-0.438981477122014,
13.3458130195912));
#59989=CARTESIAN_POINT('Ctrl Pts',(-2.94433430336091,-0.221048884050304,
13.3339945683404));
#59990=CARTESIAN_POINT('Ctrl Pts',(-2.94230384945163,-0.00270653131051041,
13.3221761170896));
#59991=CARTESIAN_POINT('Ctrl Pts',(-2.94542263194624,0.00177224128177641,
13.1778238829105));
#59992=CARTESIAN_POINT('Ctrl Pts',(-2.93924331811451,-0.866233027778004,
13.2249363653854));
#59993=CARTESIAN_POINT('Ctrl Pts',(-2.53181472316137,-1.73928198328602,
13.2720488478602));
#59994=CARTESIAN_POINT('Ctrl Pts',(-1.85921337766286,-2.28625133811473,
13.3191613303351));
#59995=CARTESIAN_POINT('Ctrl Pts',(-1.10464590246936,-2.89987676102466,
13.372015145138));
#59996=CARTESIAN_POINT('Ctrl Pts',(-0.0163374042482181,-3.10310503982634,
13.4248689599409));
#59997=CARTESIAN_POINT('Ctrl Pts',(0.908830114185135,-2.80314954796603,
13.4777227747439));
#59998=CARTESIAN_POINT('Ctrl Pts',(1.83399763261852,-2.50319405610571,13.5305765895468));
#59999=CARTESIAN_POINT('Ctrl Pts',(2.59602417126411,-1.70005479358336,13.5834304043497));
#60000=CARTESIAN_POINT('Ctrl Pts',(2.84699618048077,-0.760415881633083,
13.6362842191526));
#60001=CARTESIAN_POINT('Ctrl Pts',(3.09796818969742,0.179223030317163,13.6891380339556));
#60002=CARTESIAN_POINT('Ctrl Pts',(2.8378856694852,1.2553615916953,13.7419918487585));
#60003=CARTESIAN_POINT('Ctrl Pts',(2.18549282128288,1.97667414938146,13.7948456635614));
#60004=CARTESIAN_POINT('Ctrl Pts',(1.53309997308057,2.69798670706761,13.8476994783643));
#60005=CARTESIAN_POINT('Ctrl Pts',(0.488396796888163,3.06447326106177,13.9005532931672));
#60006=CARTESIAN_POINT('Ctrl Pts',(-0.47164330555891,2.90880940541545,13.9534071079701));
#60007=CARTESIAN_POINT('Ctrl Pts',(-1.43168340800602,2.75314554976913,14.006260922773));
#60008=CARTESIAN_POINT('Ctrl Pts',(-2.30706043670781,2.07533128448227,14.059114737576));
#60009=CARTESIAN_POINT('Ctrl Pts',(-2.69810913870436,1.18483190383781,14.1119685523789));
#60010=CARTESIAN_POINT('Ctrl Pts',(-2.86052341047112,0.814980763359175,
14.1339203292228));
#60011=CARTESIAN_POINT('Ctrl Pts',(-2.93939151111869,0.408441644783018,
14.1558721060666));
#60012=CARTESIAN_POINT('Ctrl Pts',(-2.93776462225576,0.00129977310561086,
14.1778238829105));
#60013=CARTESIAN_POINT('Origin',(0.,0.,0.));
#60014=CARTESIAN_POINT('',(-2.93898631063874,0.00219869534614975,15.3221761170896));
#60015=CARTESIAN_POINT('',(-2.94070302830747,-0.00260312230465348,15.1778238829105));
#60016=CARTESIAN_POINT('',(-2.942,-3.60291088309151E-16,0.));
#60017=CARTESIAN_POINT('Ctrl Pts',(-2.93898631063874,0.00219869534614975,
15.3221761170896));
#60018=CARTESIAN_POINT('Ctrl Pts',(-2.9413195721644,0.340324726473414,15.303926295248));
#60019=CARTESIAN_POINT('Ctrl Pts',(-2.88747827444888,0.677730458314348,
15.2856764734065));
#60020=CARTESIAN_POINT('Ctrl Pts',(-2.7742287838461,0.993853503951382,15.2674266515649));
#60021=CARTESIAN_POINT('Ctrl Pts',(-2.44502719667123,1.91278221446787,15.2143767854337));
#60022=CARTESIAN_POINT('Ctrl Pts',(-1.61383260128749,2.65187445545,15.1613269193025));
#60023=CARTESIAN_POINT('Ctrl Pts',(-0.662719748881298,2.87139211304889,
15.1082770531713));
#60024=CARTESIAN_POINT('Ctrl Pts',(0.288393103524908,3.09090977064778,15.0552271870401));
#60025=CARTESIAN_POINT('Ctrl Pts',(1.35942421295354,2.79085284486343,15.0021773209089));
#60026=CARTESIAN_POINT('Ctrl Pts',(2.05805331298264,2.10914833365457,14.9491274547778));
#60027=CARTESIAN_POINT('Ctrl Pts',(2.75668241301172,1.42744382244573,14.8960775886466));
#60028=CARTESIAN_POINT('Ctrl Pts',(3.08290950364125,0.364091725812366,14.8430277225154));
#60029=CARTESIAN_POINT('Ctrl Pts',(2.88677796198798,-0.592117497307048,
14.7899778563842));
#60030=CARTESIAN_POINT('Ctrl Pts',(2.69064642033471,-1.54832672042648,14.736927990253));
#60031=CARTESIAN_POINT('Ctrl Pts',(1.97215624639864,-2.39739307003199,14.6838781241218));
#60032=CARTESIAN_POINT('Ctrl Pts',(1.06157541348122,-2.74902669574685,14.6308282579906));
#60033=CARTESIAN_POINT('Ctrl Pts',(0.150994580563778,-3.10066032146171,
14.5777783918594));
#60034=CARTESIAN_POINT('Ctrl Pts',(-0.951676911334983,-2.95486122328588,
14.5247285257282));
#60035=CARTESIAN_POINT('Ctrl Pts',(-1.73957467901604,-2.37864879050332,
14.471678659597));
#60036=CARTESIAN_POINT('Ctrl Pts',(-2.47971301862363,-1.83736420923569,
14.4218444787612));
#60037=CARTESIAN_POINT('Ctrl Pts',(-2.94208187209259,-0.916264917963124,
14.3720102979254));
#60038=CARTESIAN_POINT('Ctrl Pts',(-2.94640032942472,0.00108073188550471,
14.3221761170896));
#60039=CARTESIAN_POINT('Ctrl Pts',(-2.93776462225576,0.00129977310561086,
14.1778238829105));
#60040=CARTESIAN_POINT('Ctrl Pts',(-2.93547441213952,-0.571843515603255,
14.2087259208695));
#60041=CARTESIAN_POINT('Ctrl Pts',(-2.77366839213467,-1.14618127181492,
14.2396279588286));
#60042=CARTESIAN_POINT('Ctrl Pts',(-2.46085834215274,-1.62104774284077,
14.2705299967876));
#60043=CARTESIAN_POINT('Ctrl Pts',(-1.92583846831326,-2.4332435128729,14.3233838115905));
#60044=CARTESIAN_POINT('Ctrl Pts',(-0.949078345342955,-2.95445055693513,
14.3762376263935));
#60045=CARTESIAN_POINT('Ctrl Pts',(0.0234689473096315,-2.94670473125899,
14.4290914411964));
#60046=CARTESIAN_POINT('Ctrl Pts',(0.996016239962246,-2.93895890558285,
14.4819452559993));
#60047=CARTESIAN_POINT('Ctrl Pts',(1.96435070229714,-2.40226021016833,14.5347990708022));
#60048=CARTESIAN_POINT('Ctrl Pts',(2.48636610448465,-1.58164571228254,14.5876528856051));
#60049=CARTESIAN_POINT('Ctrl Pts',(3.00838150667215,-0.761031214396772,
14.6405067004081));
#60050=CARTESIAN_POINT('Ctrl Pts',(3.08407784871226,0.343499085960264,14.693360515211));
#60051=CARTESIAN_POINT('Ctrl Pts',(2.67889493917015,1.22765690223306,14.7462143300139));
#60052=CARTESIAN_POINT('Ctrl Pts',(2.27371202962803,2.11181471850586,14.7990681448168));
#60053=CARTESIAN_POINT('Ctrl Pts',(1.3876498685037,2.77560005069443,14.8519219596197));
#60054=CARTESIAN_POINT('Ctrl Pts',(0.425252150859725,2.91595270416053,14.9047757744226));
#60055=CARTESIAN_POINT('Ctrl Pts',(-0.53714556678425,3.05630535762663,14.9576295892256));
#60056=CARTESIAN_POINT('Ctrl Pts',(-1.57587884094787,2.67322533237025,15.0104834040285));
#60057=CARTESIAN_POINT('Ctrl Pts',(-2.21669990962147,1.94161300865957,15.0633372188314));
#60058=CARTESIAN_POINT('Ctrl Pts',(-2.6793941459007,1.41336445080168,15.1014994401911));
#60059=CARTESIAN_POINT('Ctrl Pts',(-2.93464390538761,0.703414755606144,
15.1396616615508));
#60060=CARTESIAN_POINT('Ctrl Pts',(-2.94070302830747,-0.00260312230465348,
15.1778238829105));
#60061=CARTESIAN_POINT('Origin',(0.,0.,0.));
#60062=CARTESIAN_POINT('',(-2.9383894490365,-0.00188841566858416,16.3221761170896));
#60063=CARTESIAN_POINT('',(-2.94668624203375,0.000515437224130946,16.1778238829105));
#60064=CARTESIAN_POINT('',(-2.942,-3.60291088309151E-16,0.));
#60065=CARTESIAN_POINT('Ctrl Pts',(-2.9383894490365,-0.00188841566858416,
16.3221761170896));
#60066=CARTESIAN_POINT('Ctrl Pts',(-2.93478084744062,0.615099093327396,
16.2888921587018));
#60067=CARTESIAN_POINT('Ctrl Pts',(-2.74519813105489,1.23411540322869,16.2556082003141));
#60068=CARTESIAN_POINT('Ctrl Pts',(-2.38568546251023,1.72991184931602,16.2223242419263));
#60069=CARTESIAN_POINT('Ctrl Pts',(-1.81267372164173,2.52014042690405,16.1692743757951));
#60070=CARTESIAN_POINT('Ctrl Pts',(-0.807975369726903,2.99734375645525,
16.116224509664));
#60071=CARTESIAN_POINT('Ctrl Pts',(0.166580468072483,2.94216605243372,16.0631746435328));
#60072=CARTESIAN_POINT('Ctrl Pts',(1.14113630587187,2.88698834841218,16.0101247774016));
#60073=CARTESIAN_POINT('Ctrl Pts',(2.08554962955581,2.29942961081791,15.9570749112704));
#60074=CARTESIAN_POINT('Ctrl Pts',(2.5657024989119,1.44957263340403,15.9040250451392));
#60075=CARTESIAN_POINT('Ctrl Pts',(3.04585536826799,0.599715655990127,15.850975179008));
#60076=CARTESIAN_POINT('Ctrl Pts',(3.06174778329622,-0.512439561243392,
15.7979253128768));
#60077=CARTESIAN_POINT('Ctrl Pts',(2.60607448653775,-1.375669256418,15.7448754467456));
#60078=CARTESIAN_POINT('Ctrl Pts',(2.15040118977928,-2.23889895159261,15.6918255806144));
#60079=CARTESIAN_POINT('Ctrl Pts',(1.22316218123412,-2.8532031247083,15.6387757144832));
#60080=CARTESIAN_POINT('Ctrl Pts',(0.250580893354547,-2.93620492273994,
15.585725848352));
#60081=CARTESIAN_POINT('Ctrl Pts',(-0.722000394525,-3.01920672077158,15.5326759822209));
#60082=CARTESIAN_POINT('Ctrl Pts',(-1.73992396173896,-2.57090614371921,
15.4796261160897));
#60083=CARTESIAN_POINT('Ctrl Pts',(-2.33528145586295,-1.79737326516761,
15.4265762499585));
#60084=CARTESIAN_POINT('Ctrl Pts',(-2.72582847651777,-1.28994543553831,
15.3917762056688));
#60085=CARTESIAN_POINT('Ctrl Pts',(-2.93453708340038,-0.642563810329421,
15.3569761613792));
#60086=CARTESIAN_POINT('Ctrl Pts',(-2.93898631063874,0.00219869534614975,
15.3221761170896));
#60087=CARTESIAN_POINT('Ctrl Pts',(-2.94070302830747,-0.00260312230465348,
15.1778238829105));
#60088=CARTESIAN_POINT('Ctrl Pts',(-2.94303565380434,-0.274404061986468,
15.1925154763537));
#60089=CARTESIAN_POINT('Ctrl Pts',(-2.90843633003559,-0.54562227641632,
15.2072070697969));
#60090=CARTESIAN_POINT('Ctrl Pts',(-2.8345231637324,-0.805666183339214,
15.2218986632402));
#60091=CARTESIAN_POINT('Ctrl Pts',(-2.56861648598613,-1.74118842946232,
15.2747524780431));
#60092=CARTESIAN_POINT('Ctrl Pts',(-1.79389426731002,-2.53208829954357,
15.327606292846));
#60093=CARTESIAN_POINT('Ctrl Pts',(-0.864066442222231,-2.81726973293956,
15.3804601076489));
#60094=CARTESIAN_POINT('Ctrl Pts',(0.0657613828655833,-3.10245116633556,
15.4333139224518));
#60095=CARTESIAN_POINT('Ctrl Pts',(1.15069481436507,-2.88191416304626,15.4861677372547));
#60096=CARTESIAN_POINT('Ctrl Pts',(1.89539278194,-2.25634788250431,15.5390215520576));
#60097=CARTESIAN_POINT('Ctrl Pts',(2.64009074951493,-1.63078160196237,15.5918753668606));
#60098=CARTESIAN_POINT('Ctrl Pts',(3.0445532531653,-0.600186044167799,15.6447291816635));
#60099=CARTESIAN_POINT('Ctrl Pts',(2.92411745215616,0.364906413629165,15.6975829964664));
#60100=CARTESIAN_POINT('Ctrl Pts',(2.80368165114701,1.32999887142613,15.7504368112693));
#60101=CARTESIAN_POINT('Ctrl Pts',(2.15834754547832,2.22958822922551,15.8032906260722));
#60102=CARTESIAN_POINT('Ctrl Pts',(1.28275117211377,2.6529547668878,15.8561444408751));
#60103=CARTESIAN_POINT('Ctrl Pts',(0.407154798749216,3.07632130455008,15.9089982556781));
#60104=CARTESIAN_POINT('Ctrl Pts',(-0.698703842311192,3.0234650220753,15.961852070481));
#60105=CARTESIAN_POINT('Ctrl Pts',(-1.52992999255096,2.51851817198227,16.0147058852839));
#60106=CARTESIAN_POINT('Ctrl Pts',(-2.36115614279074,2.01357132188925,16.0675597000868));
#60107=CARTESIAN_POINT('Ctrl Pts',(-2.91774980220986,1.05653390417798,16.1204135148897));
#60108=CARTESIAN_POINT('Ctrl Pts',(-2.94559058794027,0.0843543297622131,
16.1732673296926));
#60109=CARTESIAN_POINT('Ctrl Pts',(-2.94639064385726,0.0564169709381923,
16.1747861807653));
#60110=CARTESIAN_POINT('Ctrl Pts',(-2.94675405280721,0.0284671076397201,
16.1763050318379));
#60111=CARTESIAN_POINT('Ctrl Pts',(-2.94668624203375,0.000515437224130946,
16.1778238829105));
#60112=CARTESIAN_POINT('Origin',(0.,0.,0.));
#60113=CARTESIAN_POINT('',(-2.9458984904506,-0.00153267693865478,17.3221761170896));
#60114=CARTESIAN_POINT('',(-2.93922953893335,0.0022355800204151,17.1778238829105));
#60115=CARTESIAN_POINT('',(-2.942,-3.60291088309151E-16,0.));
#60116=CARTESIAN_POINT('Ctrl Pts',(-2.9458984904506,-0.00153267693865478,
17.3221761170896));
#60117=CARTESIAN_POINT('Ctrl Pts',(-2.94027455109819,0.888306186912937,
17.2738580221557));
#60118=CARTESIAN_POINT('Ctrl Pts',(-2.50916352361795,1.78286348468974,17.2255399272217));
#60119=CARTESIAN_POINT('Ctrl Pts',(-1.80683108598698,2.32797155462599,17.1772218322878));
#60120=CARTESIAN_POINT('Ctrl Pts',(-1.03571952111964,2.92646183402729,17.1241719661566));
#60121=CARTESIAN_POINT('Ctrl Pts',(0.0623357253435999,3.10370875724391,
17.0711221000254));
#60122=CARTESIAN_POINT('Ctrl Pts',(0.982592217141216,2.77823733097987,17.0180722338942));
#60123=CARTESIAN_POINT('Ctrl Pts',(1.90284870893879,2.45276590471584,16.965022367763));
#60124=CARTESIAN_POINT('Ctrl Pts',(2.64530644607076,1.6245761289712,16.9119725016318));
#60125=CARTESIAN_POINT('Ctrl Pts',(2.86868029896989,0.674361531182407,16.8589226355006));
#60126=CARTESIAN_POINT('Ctrl Pts',(3.09205415186903,-0.275853066606427,
16.8058727693694));
#60127=CARTESIAN_POINT('Ctrl Pts',(2.79634412053529,-1.34809248643939,16.7528229032383));
#60128=CARTESIAN_POINT('Ctrl Pts',(2.1174790684053,-2.04948103853197,16.6997730371071));
#60129=CARTESIAN_POINT('Ctrl Pts',(1.43861401627531,-2.75086959062454,16.6467231709759));
#60130=CARTESIAN_POINT('Ctrl Pts',(0.376593943349051,-3.08140727497672,
16.5936733048447));
#60131=CARTESIAN_POINT('Ctrl Pts',(-0.580402982021727,-2.88915602051826,
16.5406234387135));
#60132=CARTESIAN_POINT('Ctrl Pts',(-1.53739990739248,-2.69690476605982,
16.4875735725823));
#60133=CARTESIAN_POINT('Ctrl Pts',(-2.3893736852078,-1.98186457279075,16.4345237064511));
#60134=CARTESIAN_POINT('Ctrl Pts',(-2.74469800920436,-1.07271756334381,
16.3814738403199));
#60135=CARTESIAN_POINT('Ctrl Pts',(-2.8770886883768,-0.733977483029354,
16.3617079325765));
#60136=CARTESIAN_POINT('Ctrl Pts',(-2.94053244192803,-0.368290693895058,
16.341942024833));
#60137=CARTESIAN_POINT('Ctrl Pts',(-2.9383894490365,-0.00188841566858416,
16.3221761170896));
#60138=CARTESIAN_POINT('Ctrl Pts',(-2.94668624203375,0.000515437224130946,
16.1778238829105));
#60139=CARTESIAN_POINT('Ctrl Pts',(-2.94439433622497,-0.944210489409022,
16.2291588466408));
#60140=CARTESIAN_POINT('Ctrl Pts',(-2.44950204050612,-1.8910007617774,16.2804938103711));
#60141=CARTESIAN_POINT('Ctrl Pts',(-1.67155253041584,-2.426835738729,16.3318287741014));
#60142=CARTESIAN_POINT('Ctrl Pts',(-0.8705857751193,-2.97852450168421,16.3846825889043));
#60143=CARTESIAN_POINT('Ctrl Pts',(0.230435647515488,-3.09458029647436,
16.4375364037072));
#60144=CARTESIAN_POINT('Ctrl Pts',(1.12882547663905,-2.72201627621926,16.4903902185102));
#60145=CARTESIAN_POINT('Ctrl Pts',(2.0272153057626,-2.34945225596416,16.5432440333131));
#60146=CARTESIAN_POINT('Ctrl Pts',(2.72297354137494,-1.48826842066384,16.596097848116));
#60147=CARTESIAN_POINT('Ctrl Pts',(2.89844232621279,-0.531649928364628,
16.6489516629189));
#60148=CARTESIAN_POINT('Ctrl Pts',(3.07391111105065,0.424968563934609,16.7018054777218));
#60149=CARTESIAN_POINT('Ctrl Pts',(2.72909044511397,1.4770217132327,16.7546592925247));
#60150=CARTESIAN_POINT('Ctrl Pts',(2.02141287935942,2.14418038790392,16.8075131073277));
#60151=CARTESIAN_POINT('Ctrl Pts',(1.31373531360488,2.81133906257512,16.8603669221306));
#60152=CARTESIAN_POINT('Ctrl Pts',(0.243200848032404,3.09360326261943,16.9132207369335));
#60153=CARTESIAN_POINT('Ctrl Pts',(-0.701423490172106,2.86210143987712,
16.9660745517364));
#60154=CARTESIAN_POINT('Ctrl Pts',(-1.6460478283766,2.63059961713482,17.0189283665393));
#60155=CARTESIAN_POINT('Ctrl Pts',(-2.46476203921317,1.88533177160598,17.0717821813422));
#60156=CARTESIAN_POINT('Ctrl Pts',(-2.78377104759162,0.966560044333808,
17.1246359961452));
#60157=CARTESIAN_POINT('Ctrl Pts',(-2.89077950149426,0.658367048391136,
17.1423652917336));
#60158=CARTESIAN_POINT('Ctrl Pts',(-2.94156105341168,0.330651370465482,
17.160094587322));
#60159=CARTESIAN_POINT('Ctrl Pts',(-2.93922953893335,0.0022355800204151,
17.1778238829105));
#60160=CARTESIAN_POINT('Origin',(0.,0.,0.));
#60161=CARTESIAN_POINT('',(-2.94316033587002,0.00260673739485059,18.3221761170896));
#60162=CARTESIAN_POINT('',(-2.93873926947604,-0.00201622880601424,18.1778238829105));
#60163=CARTESIAN_POINT('',(-2.942,-3.60291088309151E-16,0.));
#60164=CARTESIAN_POINT('Ctrl Pts',(-2.94316033587002,0.00260673739485059,
18.3221761170896));
#60165=CARTESIAN_POINT('Ctrl Pts',(-2.94491668517285,0.192797687418137,
18.3118737517407));
#60166=CARTESIAN_POINT('Ctrl Pts',(-2.92806785825349,0.382678731558034,
18.3015713863917));
#60167=CARTESIAN_POINT('Ctrl Pts',(-2.89148654186959,0.56867891698542,18.2912690210428));
#60168=CARTESIAN_POINT('Ctrl Pts',(-2.70311873784196,1.52644779850943,18.2382191549116));
#60169=CARTESIAN_POINT('Ctrl Pts',(-1.99154029026522,2.38131498645116,18.1851692887804));
#60170=CARTESIAN_POINT('Ctrl Pts',(-1.08384206308078,2.74032416234529,18.1321194226492));
#60171=CARTESIAN_POINT('Ctrl Pts',(-0.176143835896361,3.09933333823942,
18.0790695565181));
#60172=CARTESIAN_POINT('Ctrl Pts',(0.927674170895802,2.96248450208593,18.0260196903868));
#60173=CARTESIAN_POINT('Ctrl Pts',(1.72022055624172,2.39268288126949,17.9729698242556));
#60174=CARTESIAN_POINT('Ctrl Pts',(2.51276694158766,1.82288126045303,17.9199199581245));
#60175=CARTESIAN_POINT('Ctrl Pts',(2.99404170548737,0.820126854973603,17.8668700919933));
#60176=CARTESIAN_POINT('Ctrl Pts',(2.9428175484727,-0.154644782769381,17.8138202258621));
#60177=CARTESIAN_POINT('Ctrl Pts',(2.89159339145802,-1.12941642051234,17.7607703597309));
#60178=CARTESIAN_POINT('Ctrl Pts',(2.30787031352896,-2.07620529051882,17.7077204935997));
#60179=CARTESIAN_POINT('Ctrl Pts',(1.45996797292217,-2.55980148653722,17.6546706274685));
#60180=CARTESIAN_POINT('Ctrl Pts',(0.612065632315374,-3.04339768255563,
17.6016207613373));
#60181=CARTESIAN_POINT('Ctrl Pts',(-0.500015970969152,-3.06380120458596,
17.5485708952061));
#60182=CARTESIAN_POINT('Ctrl Pts',(-1.36508691313533,-2.61163317715626,
17.4955210290749));
#60183=CARTESIAN_POINT('Ctrl Pts',(-2.23015785530151,-2.15946514972656,
17.4424711629438));
#60184=CARTESIAN_POINT('Ctrl Pts',(-2.84821813634935,-1.23472557283683,
17.3894212968126));
#60185=CARTESIAN_POINT('Ctrl Pts',(-2.93516433523754,-0.262488966599004,
17.3363714306814));
#60186=CARTESIAN_POINT('Ctrl Pts',(-2.94291948241534,-0.175770535322769,
17.3316396594841));
#60187=CARTESIAN_POINT('Ctrl Pts',(-2.94644924052216,-0.0886742315037942,
17.3269078882868));
#60188=CARTESIAN_POINT('Ctrl Pts',(-2.9458984904506,-0.00153267693865478,
17.3221761170896));
#60189=CARTESIAN_POINT('Ctrl Pts',(-2.93922953893335,0.0022355800204151,
17.1778238829105));
#60190=CARTESIAN_POINT('Ctrl Pts',(-2.9346104425522,-0.648407683513794,
17.212948402125));
#60191=CARTESIAN_POINT('Ctrl Pts',(-2.72152344667222,-1.30179887700645,
17.2480729213394));
#60192=CARTESIAN_POINT('Ctrl Pts',(-2.32418176308124,-1.81157354166827,
17.2831974405539));
#60193=CARTESIAN_POINT('Ctrl Pts',(-1.72627966427209,-2.5786597913827,17.3360512553568));
#60194=CARTESIAN_POINT('Ctrl Pts',(-0.711171660733521,-3.02055668179605,
17.3889050701597));
#60195=CARTESIAN_POINT('Ctrl Pts',(0.257680923198029,-2.9355101952696,17.4417588849627));
#60196=CARTESIAN_POINT('Ctrl Pts',(1.22653350712957,-2.85046370874314,17.4946126997656));
#60197=CARTESIAN_POINT('Ctrl Pts',(2.14913067145408,-2.23847384527686,17.5474665145685));
#60198=CARTESIAN_POINT('Ctrl Pts',(2.60424816996682,-1.37895287589402,17.6003203293714));
#60199=CARTESIAN_POINT('Ctrl Pts',(3.05936566847955,-0.519431906511194,
17.6531741441743));
#60200=CARTESIAN_POINT('Ctrl Pts',(3.04700350118055,0.587620168788174,17.7060279589772));
#60201=CARTESIAN_POINT('Ctrl Pts',(2.57280578318673,1.43676371290232,17.7588817737802));
#60202=CARTESIAN_POINT('Ctrl Pts',(2.09860806519289,2.28590725701647,17.8117355885831));
#60203=CARTESIAN_POINT('Ctrl Pts',(1.16257479650419,2.87714226994538,17.864589403386));
#60204=CARTESIAN_POINT('Ctrl Pts',(0.192064658972456,2.94053238912373,17.9174432181889));
#60205=CARTESIAN_POINT('Ctrl Pts',(-0.778445478559264,3.00392250830208,
17.9702970329918));
#60206=CARTESIAN_POINT('Ctrl Pts',(-1.78343248493401,2.5394677337299,18.0231508477947));
#60207=CARTESIAN_POINT('Ctrl Pts',(-2.36405591431578,1.75922119095369,18.0760046625977));
#60208=CARTESIAN_POINT('Ctrl Pts',(-2.73689954660888,1.25819084947647,18.1099444027019));
#60209=CARTESIAN_POINT('Ctrl Pts',(-2.93475752332708,0.626944267538864,
18.1438841428062));
#60210=CARTESIAN_POINT('Ctrl Pts',(-2.93873926947604,-0.00201622880601424,
18.1778238829105));
#60211=CARTESIAN_POINT('Origin',(0.,0.,0.));
#60212=CARTESIAN_POINT('',(-2.93716369210466,0.00036464873958586,19.3221761170896));
#60213=CARTESIAN_POINT('',(-2.94645753962907,-0.000902846911536883,19.1778238829105));
#60214=CARTESIAN_POINT('',(-2.942,-3.60291088309151E-16,0.));
#60215=CARTESIAN_POINT('Ctrl Pts',(-2.93716369210466,0.00036464873958586,
19.3221761170896));
#60216=CARTESIAN_POINT('Ctrl Pts',(-2.93768143739811,0.470519560834665,
19.2968396151945));
#60217=CARTESIAN_POINT('Ctrl Pts',(-2.83142571131797,0.940453511257854,
19.2715031132994));
#60218=CARTESIAN_POINT('Ctrl Pts',(-2.61714889686116,1.35448210918234,19.2461666114043));
#60219=CARTESIAN_POINT('Ctrl Pts',(-2.16849357857734,2.22138006476051,19.1931167452731));
#60220=CARTESIAN_POINT('Ctrl Pts',(-1.24626864868979,2.84318628438932,19.1400668791419));
#60221=CARTESIAN_POINT('Ctrl Pts',(-0.274392720940246,2.93407545355119,
19.0870170130107));
#60222=CARTESIAN_POINT('Ctrl Pts',(0.697483206809295,3.02496462271307,19.0339671468795));
#60223=CARTESIAN_POINT('Ctrl Pts',(1.71901013242084,2.58493674140802,18.9809172807483));
#60224=CARTESIAN_POINT('Ctrl Pts',(2.32062334974625,1.81625917782929,18.9278674146171));
#60225=CARTESIAN_POINT('Ctrl Pts',(2.92223656707166,1.04758161425057,18.8748175484859));
#60226=CARTESIAN_POINT('Ctrl Pts',(3.10393607611096,-0.0497456316017877,
18.8217676823547));
#60227=CARTESIAN_POINT('Ctrl Pts',(2.78220016595262,-0.971314763096829,
18.7687178162235));
#60228=CARTESIAN_POINT('Ctrl Pts',(2.46046425579428,-1.89288389459188,18.7156679500923));
#60229=CARTESIAN_POINT('Ctrl Pts',(1.63529292643825,-2.63869491172959,18.6626180839611));
#60230=CARTESIAN_POINT('Ctrl Pts',(0.685992217770817,-2.86592128461242,
18.6095682178299));
#60231=CARTESIAN_POINT('Ctrl Pts',(-0.263308490896586,-3.09314765749525,
18.5565183516988));
#60232=CARTESIAN_POINT('Ctrl Pts',(-1.3367385788754,-2.80178938612322,18.5034684855676));
#60233=CARTESIAN_POINT('Ctrl Pts',(-2.04087504262555,-2.12577496288408,
18.4504186194364));
#60234=CARTESIAN_POINT('Ctrl Pts',(-2.60826712539801,-1.58104357723327,
18.4076711186541));
#60235=CARTESIAN_POINT('Ctrl Pts',(-2.93587273339684,-0.786550656032357,
18.3649236178719));
#60236=CARTESIAN_POINT('Ctrl Pts',(-2.94316033587002,0.00260673739485059,
18.3221761170896));
#60237=CARTESIAN_POINT('Ctrl Pts',(-2.93873926947604,-0.00201622880601424,
18.1778238829105));
#60238=CARTESIAN_POINT('Ctrl Pts',(-2.9409582329643,-0.352525860695343,
18.1967379576091));
#60239=CARTESIAN_POINT('Ctrl Pts',(-2.8829659327141,-0.702325513325489,
18.2156520323078));
#60240=CARTESIAN_POINT('Ctrl Pts',(-2.76149291692009,-1.02848258833687,
18.2345661070064));
#60241=CARTESIAN_POINT('Ctrl Pts',(-2.42204663775388,-1.93990151387084,
18.2874199218093));
#60242=CARTESIAN_POINT('Ctrl Pts',(-1.58689422703273,-2.6667010539585,18.3402737366122));
#60243=CARTESIAN_POINT('Ctrl Pts',(-0.637335842913562,-2.87705102284432,
18.3931275514152));
#60244=CARTESIAN_POINT('Ctrl Pts',(0.312222541205624,-3.08740099173015,
18.4459813662181));
#60245=CARTESIAN_POINT('Ctrl Pts',(1.37618689872286,-2.7813013894141,18.498835181021));
#60246=CARTESIAN_POINT('Ctrl Pts',(2.06878987437855,-2.0985061401818,18.5516889958239));
#60247=CARTESIAN_POINT('Ctrl Pts',(2.76139285003424,-1.4157108909495,18.6045428106268));
#60248=CARTESIAN_POINT('Ctrl Pts',(3.08263444382841,-0.356219994800951,
18.6573966254298));
#60249=CARTESIAN_POINT('Ctrl Pts',(2.88584744993387,0.596241612454314,18.7102504402327));
#60250=CARTESIAN_POINT('Ctrl Pts',(2.68906045603933,1.54870321970957,18.7631042550356));
#60251=CARTESIAN_POINT('Ctrl Pts',(1.97424487445611,2.39413553807152,18.8159580698385));
#60252=CARTESIAN_POINT('Ctrl Pts',(1.06775945217669,2.74654497814968,18.8688118846414));
#60253=CARTESIAN_POINT('Ctrl Pts',(0.161274029897288,3.09895441822785,18.9216656994444));
#60254=CARTESIAN_POINT('Ctrl Pts',(-0.936881233078337,2.95834098002222,
18.9745195142473));
#60255=CARTESIAN_POINT('Ctrl Pts',(-1.72532865995951,2.38890363552703,19.0273733290502));
#60256=CARTESIAN_POINT('Ctrl Pts',(-2.47344465061743,1.84859470867852,19.0775235136703));
#60257=CARTESIAN_POINT('Ctrl Pts',(-2.94272737324388,0.922211045366831,
19.1276736982904));
#60258=CARTESIAN_POINT('Ctrl Pts',(-2.94645753962907,-0.000902846911536883,
19.1778238829105));
#60259=CARTESIAN_POINT('Origin',(0.,0.,0.));
#60260=CARTESIAN_POINT('',(-2.94181767770235,-0.00272435142412375,20.3221761170896));
#60261=CARTESIAN_POINT('',(-2.94133845650885,0.002661508174006,20.1778238829105));
#60262=CARTESIAN_POINT('',(-2.942,-3.60291088309151E-16,0.));
#60263=CARTESIAN_POINT('Ctrl Pts',(-2.94181767770235,-0.00272435142412375,
20.3221761170896));
#60264=CARTESIAN_POINT('Ctrl Pts',(-2.93494169159882,0.743426259253046,
20.2818054786483));
#60265=CARTESIAN_POINT('Ctrl Pts',(-2.64630113395455,1.49430940028337,20.241434840207));
#60266=CARTESIAN_POINT('Ctrl Pts',(-2.13403588059313,2.03223546686346,20.2010642017657));
#60267=CARTESIAN_POINT('Ctrl Pts',(-1.46088320915349,2.73910825665216,20.1480143356345));
#60268=CARTESIAN_POINT('Ctrl Pts',(-0.401579583775771,3.07825074195412,
20.0949644695033));
#60269=CARTESIAN_POINT('Ctrl Pts',(0.556945495101902,2.89376948769634,20.0419146033721));
#60270=CARTESIAN_POINT('Ctrl Pts',(1.5154705739796,2.70928823343856,19.9888647372409));
#60271=CARTESIAN_POINT('Ctrl Pts',(2.37321710635726,2.00118323962099,19.9358148711097));
#60272=CARTESIAN_POINT('Ctrl Pts',(2.73590522713548,1.0949487296533,19.8827650049785));
#60273=CARTESIAN_POINT('Ctrl Pts',(3.09859334791368,0.188714219685681,19.8297151388474));
#60274=CARTESIAN_POINT('Ctrl Pts',(2.96622305709255,-0.915649806432031,
19.7766652727162));
#60275=CARTESIAN_POINT('Ctrl Pts',(2.39964093164797,-1.71050095925033,19.723615406585));
#60276=CARTESIAN_POINT('Ctrl Pts',(1.83305880620336,-2.50535211206866,19.6705655404538));
#60277=CARTESIAN_POINT('Ctrl Pts',(0.832264846135248,-2.99069039158755,
19.6175156743226));
#60278=CARTESIAN_POINT('Ctrl Pts',(-0.142706552994196,-2.9434206244044,
19.5644658081914));
#60279=CARTESIAN_POINT('Ctrl Pts',(-1.11767795212364,-2.89615085722124,
19.5114159420602));
#60280=CARTESIAN_POINT('Ctrl Pts',(-2.06682679031441,-2.31627304333605,
19.458366075929));
#60281=CARTESIAN_POINT('Ctrl Pts',(-2.55385835606975,-1.47033929062967,
19.4053162097978));
#60282=CARTESIAN_POINT('Ctrl Pts',(-2.80828469416576,-1.02842167767351,
19.3776028455618));
#60283=CARTESIAN_POINT('Ctrl Pts',(-2.93659737620366,-0.513896332520092,
19.3498894813257));
#60284=CARTESIAN_POINT('Ctrl Pts',(-2.93716369210466,0.00036464873958586,
19.3221761170896));
#60285=CARTESIAN_POINT('Ctrl Pts',(-2.94645753962907,-0.000902846911536883,
19.1778238829105));
#60286=CARTESIAN_POINT('Ctrl Pts',(-2.94665863540772,-0.0506685377110252,
19.1805275130933));
#60287=CARTESIAN_POINT('Ctrl Pts',(-2.94550666757136,-0.100424725376753,
19.1832311432761));
#60288=CARTESIAN_POINT('Ctrl Pts',(-2.94297238022198,-0.150110405910103,
19.1859347734589));
#60289=CARTESIAN_POINT('Ctrl Pts',(-2.89342908281652,-1.12142585206726,
19.2387885882619));
#60290=CARTESIAN_POINT('Ctrl Pts',(-2.31560289721883,-2.06579549359683,
19.2916424030648));
#60291=CARTESIAN_POINT('Ctrl Pts',(-1.47330820404643,-2.55205456458153,
19.3444962178677));
#60292=CARTESIAN_POINT('Ctrl Pts',(-0.63101351087402,-3.03831363556623,
19.3973500326706));
#60293=CARTESIAN_POINT('Ctrl Pts',(0.47574968987309,-3.06646213600607,19.4502038474735));
#60294=CARTESIAN_POINT('Ctrl Pts',(1.34167365068723,-2.62364848631891,19.5030576622764));
#60295=CARTESIAN_POINT('Ctrl Pts',(2.20759761150139,-2.18083483663175,19.5559114770793));
#60296=CARTESIAN_POINT('Ctrl Pts',(2.83268233238255,-1.26705903681756,19.6087652918823));
#60297=CARTESIAN_POINT('Ctrl Pts',(2.93153690758253,-0.299517819492232,
19.6616191066852));
#60298=CARTESIAN_POINT('Ctrl Pts',(3.03039148278251,0.668023397833066,19.7144729214881));
#60299=CARTESIAN_POINT('Ctrl Pts',(2.60301591230135,1.68933003266952,19.767326736291));
#60300=CARTESIAN_POINT('Ctrl Pts',(1.84453430824712,2.29811069150536,19.8201805510939));
#60301=CARTESIAN_POINT('Ctrl Pts',(1.08605270419287,2.90689135034122,19.8730343658968));
#60302=CARTESIAN_POINT('Ctrl Pts',(-0.00353493343442576,3.10314603317647,
19.9258881806998));
#60303=CARTESIAN_POINT('Ctrl Pts',(-0.92676259337782,2.79727200326095,19.9787419955027));
#60304=CARTESIAN_POINT('Ctrl Pts',(-1.8499902533212,2.49139797334544,20.0315958103056));
#60305=CARTESIAN_POINT('Ctrl Pts',(-2.60685793558067,1.68339523067915,20.0844496251085));
#60306=CARTESIAN_POINT('Ctrl Pts',(-2.85180743635457,0.742168384306878,
20.1373034399114));
#60307=CARTESIAN_POINT('Ctrl Pts',(-2.91440438305093,0.501637472647963,
20.1508102542444));
#60308=CARTESIAN_POINT('Ctrl Pts',(-2.94356999338208,0.25240622569323,20.1643170685774));
#60309=CARTESIAN_POINT('Ctrl Pts',(-2.94133845650885,0.002661508174006,
20.1778238829105));
#60310=CARTESIAN_POINT('Origin',(0.,0.,0.));
#60311=CARTESIAN_POINT('',(-2.94661408633091,0.000803455063355558,21.3221761170896));
#60312=CARTESIAN_POINT('',(-2.93750898741464,-0.00097440350457154,21.1778238829105));
#60313=CARTESIAN_POINT('',(-2.942,-3.60291088309151E-16,0.));
#60314=CARTESIAN_POINT('Ctrl Pts',(-2.94661408633091,0.000803455063355558,
21.3221761170896));
#60315=CARTESIAN_POINT('Ctrl Pts',(-2.94677107215841,0.0441441474901623,
21.3198212082333));
#60316=CARTESIAN_POINT('Ctrl Pts',(-2.94589802603797,0.0874783744189961,
21.317466299377));
#60317=CARTESIAN_POINT('Ctrl Pts',(-2.943975270306,0.130765975174579,21.3151113905207));
#60318=CARTESIAN_POINT('Ctrl Pts',(-2.90066067071482,1.10592109384657,21.2620615243895));
#60319=CARTESIAN_POINT('Ctrl Pts',(-2.32463766198353,2.05741428325321,21.2090116582583));
#60320=CARTESIAN_POINT('Ctrl Pts',(-1.48068641588049,2.54787320529567,21.1559617921271));
#60321=CARTESIAN_POINT('Ctrl Pts',(-0.636735169777449,3.03833212733813,
21.1029119259959));
#60322=CARTESIAN_POINT('Ctrl Pts',(0.475144313697323,3.06775678201641,21.0498620598648));
#60323=CARTESIAN_POINT('Ctrl Pts',(1.34385501904681,2.62262155489871,20.9968121937336));
#60324=CARTESIAN_POINT('Ctrl Pts',(2.2125657243963,2.17748632778101,20.9437623276024));
#60325=CARTESIAN_POINT('Ctrl Pts',(2.83810765162053,1.25779121886726,20.8907124614712));
#60326=CARTESIAN_POINT('Ctrl Pts',(2.93293829559698,0.286291960518122,20.83766259534));
#60327=CARTESIAN_POINT('Ctrl Pts',(3.02776893957345,-0.685207297831074,
20.7846127292088));
#60328=CARTESIAN_POINT('Ctrl Pts',(2.59188830030215,-1.70851070561573,20.7315628630776));
#60329=CARTESIAN_POINT('Ctrl Pts',(1.82565738556811,-2.31323696212845,20.6785129969464));
#60330=CARTESIAN_POINT('Ctrl Pts',(1.05942647083414,-2.91796321864112,20.6254631308152));
#60331=CARTESIAN_POINT('Ctrl Pts',(-0.0371547193624712,-3.10411232388192,
20.572413264684));
#60332=CARTESIAN_POINT('Ctrl Pts',(-0.96002132737357,-2.78611722356123,
20.5193633985529));
#60333=CARTESIAN_POINT('Ctrl Pts',(-1.88288793538472,-2.46812212324052,
20.4663135324217));
#60334=CARTESIAN_POINT('Ctrl Pts',(-2.63203996121031,-1.64598281735826,
20.4132636662905));
#60335=CARTESIAN_POINT('Ctrl Pts',(-2.86311511537232,-0.697611617279415,
20.3602138001593));
#60336=CARTESIAN_POINT('Ctrl Pts',(-2.91834342614413,-0.47094536423746,
20.3475345724694));
#60337=CARTESIAN_POINT('Ctrl Pts',(-2.94397722228141,-0.237068266928035,
20.3348553447795));
#60338=CARTESIAN_POINT('Ctrl Pts',(-2.94181767770235,-0.00272435142412375,
20.3221761170896));
#60339=CARTESIAN_POINT('Ctrl Pts',(-2.94133845650885,0.002661508174006,
20.1778238829105));
#60340=CARTESIAN_POINT('Ctrl Pts',(-2.93483771693884,-0.72487536879094,
20.2171708833804));
#60341=CARTESIAN_POINT('Ctrl Pts',(-2.66189196800706,-1.45676970117924,
20.2565178838503));
#60342=CARTESIAN_POINT('Ctrl Pts',(-2.17278956561389,-1.99062931463176,
20.2958648843202));
#60343=CARTESIAN_POINT('Ctrl Pts',(-1.51579087481095,-2.70774921711983,
20.3487186991231));
#60344=CARTESIAN_POINT('Ctrl Pts',(-0.468762173916675,-3.06753807201771,
20.401572513926));
#60345=CARTESIAN_POINT('Ctrl Pts',(0.490261385495665,-2.90572939872311,
20.4544263287289));
#60346=CARTESIAN_POINT('Ctrl Pts',(1.44928494490802,-2.74392072542852,20.5072801435319));
#60347=CARTESIAN_POINT('Ctrl Pts',(2.32030336283847,-2.06051452394146,20.5601339583348));
#60348=CARTESIAN_POINT('Ctrl Pts',(2.70564136917951,-1.16752916284621,20.6129877731377));
#60349=CARTESIAN_POINT('Ctrl Pts',(3.09097937552055,-0.274543801750937,
20.6658415879406));
#60350=CARTESIAN_POINT('Ctrl Pts',(2.99063697027215,0.828020718952537,20.7186954027435));
#60351=CARTESIAN_POINT('Ctrl Pts',(2.4504268392386,1.6367736160664,20.7715492175465));
#60352=CARTESIAN_POINT('Ctrl Pts',(1.91021670820505,2.44552651318024,20.8244030323494));
#60353=CARTESIAN_POINT('Ctrl Pts',(0.930138851386389,2.96046778670446,20.8772568471523));
#60354=CARTESIAN_POINT('Ctrl Pts',(-0.0423388953904588,2.94649401537642,
20.9301106619552));
#60355=CARTESIAN_POINT('Ctrl Pts',(-1.01481664216731,2.93252024404837,20.9829644767581));
#60356=CARTESIAN_POINT('Ctrl Pts',(-1.97969427890232,2.38963142786804,21.035818291561));
#60357=CARTESIAN_POINT('Ctrl Pts',(-2.49644383636957,1.56569081767899,21.088672106364));
#60358=CARTESIAN_POINT('Ctrl Pts',(-2.78698824487709,1.10242706878285,21.1183893652128));
#60359=CARTESIAN_POINT('Ctrl Pts',(-2.93586621539549,0.550314599197934,
21.1481066240616));
#60360=CARTESIAN_POINT('Ctrl Pts',(-2.93750898741464,-0.00097440350457154,
21.1778238829105));
#60361=CARTESIAN_POINT('Origin',(0.,0.,0.));
#60362=CARTESIAN_POINT('',(-2.93936618898165,0.00234662407228609,22.3221761170896));
#60363=CARTESIAN_POINT('',(-2.94488602564283,-0.00204434552984655,22.1778238829105));
#60364=CARTESIAN_POINT('',(-2.942,-3.60291088309151E-16,0.));
#60365=CARTESIAN_POINT('Ctrl Pts',(-2.93936618898165,0.00234662407228609,
22.3221761170896));
#60366=CARTESIAN_POINT('Ctrl Pts',(-2.94175919559491,0.324419742206598,
22.3047870716871));
#60367=CARTESIAN_POINT('Ctrl Pts',(-2.89299512987164,0.645788293098763,
22.2873980262846));
#60368=CARTESIAN_POINT('Ctrl Pts',(-2.78998843935577,0.948712095789747,
22.2700089808822));
#60369=CARTESIAN_POINT('Ctrl Pts',(-2.47573938105466,1.87286099578738,22.216959114751));
#60370=CARTESIAN_POINT('Ctrl Pts',(-1.65664562584339,2.62534170401123,22.1639092486198));
#60371=CARTESIAN_POINT('Ctrl Pts',(-0.709219538526518,2.86026183742134,
22.1108593824886));
#60372=CARTESIAN_POINT('Ctrl Pts',(0.238206548790326,3.09518197083143,22.0578095163574));
#60373=CARTESIAN_POINT('Ctrl Pts',(1.31396496821276,2.81254152942782,22.0047596502262));
#60374=CARTESIAN_POINT('Ctrl Pts',(2.02356245339832,2.14226168561014,21.951709784095));
#60375=CARTESIAN_POINT('Ctrl Pts',(2.7331599385839,1.47198184179245,21.8986599179638));
#60376=CARTESIAN_POINT('Ctrl Pts',(3.07659648953258,0.414062595560654,21.8456100518326));
#60377=CARTESIAN_POINT('Ctrl Pts',(2.89600482043572,-0.54520290942886,21.7925601857014));
#60378=CARTESIAN_POINT('Ctrl Pts',(2.71541315133886,-1.5044684144184,21.7395103195703));
#60379=CARTESIAN_POINT('Ctrl Pts',(2.01079326219644,-2.36508017816566,21.6864604534391));
#60380=CARTESIAN_POINT('Ctrl Pts',(1.10603738031632,-2.73144127628248,21.6334105873079));
#60381=CARTESIAN_POINT('Ctrl Pts',(0.201281498436279,-3.09780237439927,
21.5803607211767));
#60382=CARTESIAN_POINT('Ctrl Pts',(-0.903610376181412,-2.96991280688572,
21.5273108550455));
#60383=CARTESIAN_POINT('Ctrl Pts',(-1.70075321826476,-2.40655949916031,
21.4742609889143));
#60384=CARTESIAN_POINT('Ctrl Pts',(-2.4625105094419,-1.86821371342004,21.4235660316394));
#60385=CARTESIAN_POINT('Ctrl Pts',(-2.94323459680346,-0.932206986069505,
21.3728710743645));
#60386=CARTESIAN_POINT('Ctrl Pts',(-2.94661408633091,0.000803455063355558,
21.3221761170896));
#60387=CARTESIAN_POINT('Ctrl Pts',(-2.93750898741464,-0.00097440350457154,
21.1778238829105));
#60388=CARTESIAN_POINT('Ctrl Pts',(-2.93878797774595,-0.430183871402343,
21.2009604388645));
#60389=CARTESIAN_POINT('Ctrl Pts',(-2.85082038965928,-0.858894195057127,
21.2240969948186));
#60390=CARTESIAN_POINT('Ctrl Pts',(-2.67097820455793,-1.244787128584,21.2472335507727));
#60391=CARTESIAN_POINT('Ctrl Pts',(-2.26014153707957,-2.12633206046017,
21.3000873655756));
#60392=CARTESIAN_POINT('Ctrl Pts',(-1.36984672392337,-2.78442952001476,
21.3529411803785));
#60393=CARTESIAN_POINT('Ctrl Pts',(-0.406569934833748,-2.91861618799067,
21.4057949951814));
#60394=CARTESIAN_POINT('Ctrl Pts',(0.556706854255877,-3.05280285596659,
21.4586488099844));
#60395=CARTESIAN_POINT('Ctrl Pts',(1.59296561927893,-2.66307873236383,21.5115026247873));
#60396=CARTESIAN_POINT('Ctrl Pts',(2.22908836892936,-1.92737765064757,21.5643564395902));
#60397=CARTESIAN_POINT('Ctrl Pts',(2.86521111857982,-1.1916765689313,21.6172102543931));
#60398=CARTESIAN_POINT('Ctrl Pts',(3.10119785285763,-0.109998529101508,
21.670064069196));
#60399=CARTESIAN_POINT('Ctrl Pts',(2.82930562814205,0.823801691716928,21.722917883999));
#60400=CARTESIAN_POINT('Ctrl Pts',(2.55741340342647,1.75760191253534,21.7757716988019));
#60401=CARTESIAN_POINT('Ctrl Pts',(1.77764221971752,2.5435243143424,21.8286255136048));
#60402=CARTESIAN_POINT('Ctrl Pts',(0.846007184985371,2.82274536713198,21.8814793284077));
#60403=CARTESIAN_POINT('Ctrl Pts',(-0.0856278497467812,3.10196641992156,
21.9343331432106));
#60404=CARTESIAN_POINT('Ctrl Pts',(-1.16912673550214,2.87448612369365,21.9871869580135));
#60405=CARTESIAN_POINT('Ctrl Pts',(-1.90980336325705,2.2441636924262,22.0400407728165));
#60406=CARTESIAN_POINT('Ctrl Pts',(-2.55341965804143,1.69644047215729,22.0859684761811));
#60407=CARTESIAN_POINT('Ctrl Pts',(-2.93817544933017,0.844536541703994,
22.1318961795458));
#60408=CARTESIAN_POINT('Ctrl Pts',(-2.94488602564283,-0.00204434552984655,
22.1778238829105));
#60409=CARTESIAN_POINT('Origin',(0.,0.,0.));
#60410=CARTESIAN_POINT('',(-2.93809596128261,-0.00168714029618489,23.3221761170896));
#60411=CARTESIAN_POINT('',(-2.94367738520799,0.0024475330369777,23.1778238829105));
#60412=CARTESIAN_POINT('',(-2.942,-3.60291088309151E-16,0.));
#60413=CARTESIAN_POINT('Ctrl Pts',(-2.93809596128261,-0.00168714029618489,
23.3221761170896));
#60414=CARTESIAN_POINT('Ctrl Pts',(-2.93497421326337,0.599494484093746,
23.2897529351409));
#60415=CARTESIAN_POINT('Ctrl Pts',(-2.75577143026152,1.20238463007766,23.2573297531923));
#60416=CARTESIAN_POINT('Ctrl Pts',(-2.41343846997067,1.69097749367112,23.2249065712436));
#60417=CARTESIAN_POINT('Ctrl Pts',(-1.85332324918586,2.49039890910546,23.1718567051124));
#60418=CARTESIAN_POINT('Ctrl Pts',(-0.856499547571336,2.98384019636719,
23.1188068389812));
#60419=CARTESIAN_POINT('Ctrl Pts',(0.118823245776437,2.94448147705157,23.06575697285));
#60420=CARTESIAN_POINT('Ctrl Pts',(1.09414603912426,2.90512275773594,23.0127071067188));
#60421=CARTESIAN_POINT('Ctrl Pts',(2.04796792420534,2.3329640318429,22.9596572405877));
#60422=CARTESIAN_POINT('Ctrl Pts',(2.54184613269262,1.49100917842654,22.9066073744565));
#60423=CARTESIAN_POINT('Ctrl Pts',(3.0357243411799,0.649054325010205,22.8535575083253));
#60424=CARTESIAN_POINT('Ctrl Pts',(3.06965887307341,-0.462696655929437,
22.8005076421941));
#60425=CARTESIAN_POINT('Ctrl Pts',(2.62805106122367,-1.33320581758324,22.7474577760629));
#60426=CARTESIAN_POINT('Ctrl Pts',(2.18644324937392,-2.20371497923707,22.6944079099317));
#60427=CARTESIAN_POINT('Ctrl Pts',(1.26929309378089,-2.83298232160505,22.6413580438005));
#60428=CARTESIAN_POINT('Ctrl Pts',(0.298186489546595,-2.93175288008531,
22.5883081776693));
#60429=CARTESIAN_POINT('Ctrl Pts',(-0.672920114687705,-3.03052343856557,
22.5352583115381));
#60430=CARTESIAN_POINT('Ctrl Pts',(-1.69798316756328,-2.59879721315811,
22.4822084454069));
#60431=CARTESIAN_POINT('Ctrl Pts',(-2.30581251330558,-1.83502555456867,
22.4291585792757));
#60432=CARTESIAN_POINT('Ctrl Pts',(-2.71440342809815,-1.32160815729808,
22.393497758547));
#60433=CARTESIAN_POINT('Ctrl Pts',(-2.93445869821015,-0.658149191626092,
22.3578369378183));
#60434=CARTESIAN_POINT('Ctrl Pts',(-2.93936618898165,0.00234662407228609,
22.3221761170896));
#60435=CARTESIAN_POINT('Ctrl Pts',(-2.94488602564283,-0.00204434552984655,
22.1778238829105));
#60436=CARTESIAN_POINT('Ctrl Pts',(-2.94589801178521,-0.129712683742034,
22.1847499943487));
#60437=CARTESIAN_POINT('Ctrl Pts',(-2.93831247708221,-0.257259965072063,
22.191676105787));
#60438=CARTESIAN_POINT('Ctrl Pts',(-2.92172066492491,-0.383624713571277,
22.1986022172252));
#60439=CARTESIAN_POINT('Ctrl Pts',(-2.7951069690834,-1.34792612199431,22.2514560320281));
#60440=CARTESIAN_POINT('Ctrl Pts',(-2.14402520764591,-2.24336437253339,
22.304309846831));
#60441=CARTESIAN_POINT('Ctrl Pts',(-1.26573558775814,-2.66111498935963,
22.3571636616339));
#60442=CARTESIAN_POINT('Ctrl Pts',(-0.387445967870374,-3.07886560618586,
22.4100174764369));
#60443=CARTESIAN_POINT('Ctrl Pts',(0.718051510467669,-3.01892858929924,
22.4628712912398));
#60444=CARTESIAN_POINT('Ctrl Pts',(1.5460269824779,-2.50866899653226,22.5157251060427));
#60445=CARTESIAN_POINT('Ctrl Pts',(2.37400245448816,-1.99840940376527,22.5685789208456));
#60446=CARTESIAN_POINT('Ctrl Pts',(2.9244559201706,-1.03782723511788,22.6214327356485));
#60447=CARTESIAN_POINT('Ctrl Pts',(2.9460703853714,-0.0654893056121799,
22.6742865504515));
#60448=CARTESIAN_POINT('Ctrl Pts',(2.96768485057219,0.906848623893493,22.7271403652544));
#60449=CARTESIAN_POINT('Ctrl Pts',(2.46046031529139,1.89094231425748,22.7799941800573));
#60450=CARTESIAN_POINT('Ctrl Pts',(1.65597701930418,2.4374904463912,22.8328479948602));
#60451=CARTESIAN_POINT('Ctrl Pts',(0.851493723316973,2.98403857852492,22.8857018096631));
#60452=CARTESIAN_POINT('Ctrl Pts',(-0.250248333376632,3.09304115242837,
22.9385556244661));
#60453=CARTESIAN_POINT('Ctrl Pts',(-1.14623387467553,2.71473156486203,22.991409439269));
#60454=CARTESIAN_POINT('Ctrl Pts',(-2.04221941597443,2.33642197729568,23.0442632540719));
#60455=CARTESIAN_POINT('Ctrl Pts',(-2.73244844187862,1.47080022825954,23.0971170688748));
#60456=CARTESIAN_POINT('Ctrl Pts',(-2.90178753079562,0.513077665496164,
23.1499708836777));
#60457=CARTESIAN_POINT('Ctrl Pts',(-2.93153373758168,0.344843540830449,
23.1592552167553));
#60458=CARTESIAN_POINT('Ctrl Pts',(-2.94520702688292,0.173767493765761,
23.1685395498329));
#60459=CARTESIAN_POINT('Ctrl Pts',(-2.94367738520799,0.0024475330369777,
23.1778238829105));
#60460=CARTESIAN_POINT('Origin',(0.,0.,0.));
#60461=CARTESIAN_POINT('',(-2.94555278480659,-0.00176380088044714,24.3221761170896));
#60462=CARTESIAN_POINT('',(-2.93722802281203,0.000281837720408654,24.1778238829105));
#60463=CARTESIAN_POINT('',(-2.942,-3.60291088309151E-16,0.));
#60464=CARTESIAN_POINT('Ctrl Pts',(-2.94555278480659,-0.00176380088044714,
24.3221761170896));
#60465=CARTESIAN_POINT('Ctrl Pts',(-2.93937087079276,0.87249287190428,24.2747187985947));
#60466=CARTESIAN_POINT('Ctrl Pts',(-2.525406696364,1.75183148857115,24.2272614800999));
#60467=CARTESIAN_POINT('Ctrl Pts',(-1.84436353069014,2.29835012543712,24.179804161605));
#60468=CARTESIAN_POINT('Ctrl Pts',(-1.08306369508132,2.90927255939407,24.1267542954739));
#60469=CARTESIAN_POINT('Ctrl Pts',(0.0119712680674577,3.10431159537625,
24.0737044293427));
#60470=CARTESIAN_POINT('Ctrl Pts',(0.93738725442356,2.79381374964061,24.0206545632115));
#60471=CARTESIAN_POINT('Ctrl Pts',(1.86280324077969,2.48331590390496,23.9676046970803));
#60472=CARTESIAN_POINT('Ctrl Pts',(2.61860025034316,1.66728117645145,23.9145548309491));
#60473=CARTESIAN_POINT('Ctrl Pts',(2.85736149770633,0.720815790519383,23.8615049648179));
#60474=CARTESIAN_POINT('Ctrl Pts',(3.09612274506951,-0.225649595412714,
23.8084550986867));
#60475=CARTESIAN_POINT('Ctrl Pts',(2.8178482302324,-1.30254563982334,23.7554052325555));
#60476=CARTESIAN_POINT('Ctrl Pts',(2.1504522425905,-2.01485614493296,23.7023553664243));
#60477=CARTESIAN_POINT('Ctrl Pts',(1.48305625494865,-2.72716665004254,23.6493055002931));
#60478=CARTESIAN_POINT('Ctrl Pts',(0.42653879450204,-3.07489161585109,23.596255634162));
#60479=CARTESIAN_POINT('Ctrl Pts',(-0.533451353174756,-2.89819250330834,
23.5432057680308));
#60480=CARTESIAN_POINT('Ctrl Pts',(-1.49344150085158,-2.72149339076559,
23.4901559018996));
#60481=CARTESIAN_POINT('Ctrl Pts',(-2.35690433575861,-2.02037019987151,
23.4371060357684));
#60482=CARTESIAN_POINT('Ctrl Pts',(-2.7269323832346,-1.11710783262096,23.3840561696372));
#60483=CARTESIAN_POINT('Ctrl Pts',(-2.87080553939092,-0.765904164412539,
23.3634294854547));
#60484=CARTESIAN_POINT('Ctrl Pts',(-2.94008192646617,-0.384141383135884,
23.3428028012721));
#60485=CARTESIAN_POINT('Ctrl Pts',(-2.93809596128261,-0.00168714029618489,
23.3221761170896));
#60486=CARTESIAN_POINT('Ctrl Pts',(-2.94367738520799,0.0024475330369777,
23.1778238829105));
#60487=CARTESIAN_POINT('Ctrl Pts',(-2.93649908877625,-0.801522104392271,
23.2213933646358));
#60488=CARTESIAN_POINT('Ctrl Pts',(-2.59451675492149,-1.61086329021898,
23.2649628463611));
#60489=CARTESIAN_POINT('Ctrl Pts',(-2.00764029345905,-2.15708136536191,
23.3085323280865));
#60490=CARTESIAN_POINT('Ctrl Pts',(-1.29570481527567,-2.81969445696598,
23.3613861428894));
#60491=CARTESIAN_POINT('Ctrl Pts',(-0.223384706979118,-3.0950972636835,
23.4142399576923));
#60492=CARTESIAN_POINT('Ctrl Pts',(0.719737744845044,-2.8575508995217,23.4670937724952));
#60493=CARTESIAN_POINT('Ctrl Pts',(1.66286019666921,-2.62000453535991,23.5199475872981));
#60494=CARTESIAN_POINT('Ctrl Pts',(2.47678499202095,-1.8695090003188,23.5728014021011));
#60495=CARTESIAN_POINT('Ctrl Pts',(2.78990372839629,-0.948713207978274,
23.625655216904));
#60496=CARTESIAN_POINT('Ctrl Pts',(3.10302246477162,-0.0279174156377443,
23.6785090317069));
#60497=CARTESIAN_POINT('Ctrl Pts',(2.91533514217051,1.06317863400226,23.7313628465098));
#60498=CARTESIAN_POINT('Ctrl Pts',(2.31253295285098,1.82642024372548,23.7842166613127));
#60499=CARTESIAN_POINT('Ctrl Pts',(1.70973076353145,2.58966185344871,23.8370704761156));
#60500=CARTESIAN_POINT('Ctrl Pts',(0.691813707493536,3.02504902325521,23.8899242909186));
#60501=CARTESIAN_POINT('Ctrl Pts',(-0.276474379915739,2.93379983672406,
23.9427781057215));
#60502=CARTESIAN_POINT('Ctrl Pts',(-1.24476246732499,2.84255065019292,23.9956319205244));
#60503=CARTESIAN_POINT('Ctrl Pts',(-2.16342158610557,2.22466510732416,24.0484857353273));
#60504=CARTESIAN_POINT('Ctrl Pts',(-2.61302545814756,1.36224723152027,24.1013395501302));
#60505=CARTESIAN_POINT('Ctrl Pts',(-2.82989818087518,0.946247894136707,
24.1268343277236));
#60506=CARTESIAN_POINT('Ctrl Pts',(-2.9376334601039,0.473351988907629,24.1523291053171));
#60507=CARTESIAN_POINT('Ctrl Pts',(-2.93722802281203,0.000281837720408654,
24.1778238829105));
#60508=CARTESIAN_POINT('Origin',(0.,0.,0.));
#60509=CARTESIAN_POINT('',(-2.94363848369983,0.00251143626685393,25.3221761170896));
#60510=CARTESIAN_POINT('',(-2.94264856609968,-0.00262420787473867,25.1778238829105));
#60511=CARTESIAN_POINT('',(-2.942,-3.60291088309151E-16,0.));
#60512=CARTESIAN_POINT('Ctrl Pts',(-2.94363848369983,0.00251143626685393,
25.3221761170896));
#60513=CARTESIAN_POINT('Ctrl Pts',(-2.94521862476287,0.176738668532974,
25.3127345281798));
#60514=CARTESIAN_POINT('Ctrl Pts',(-2.93108735667538,0.350709910061776,
25.3032929392699));
#60515=CARTESIAN_POINT('Ctrl Pts',(-2.90033250031881,0.521691019695654,
25.2938513503601));
#60516=CARTESIAN_POINT('Ctrl Pts',(-2.72752885167656,1.48239001471223,25.2408014842289));
#60517=CARTESIAN_POINT('Ctrl Pts',(-2.02991389507056,2.34868971365866,25.1877516180977));
#60518=CARTESIAN_POINT('Ctrl Pts',(-1.12815990441773,2.72237862217966,25.1347017519665));
#60519=CARTESIAN_POINT('Ctrl Pts',(-0.226405913764866,3.09606753070067,
25.0816518858353));
#60520=CARTESIAN_POINT('Ctrl Pts',(0.879487110934829,2.9771456487962,25.0286020197041));
#60521=CARTESIAN_POINT('Ctrl Pts',(1.68117394631541,2.42027773089514,24.9755521535729));
#60522=CARTESIAN_POINT('Ctrl Pts',(2.48286078169597,1.86340981299409,24.9225022874417));
#60523=CARTESIAN_POINT('Ctrl Pts',(2.98034142775742,0.868595859096418,24.8694524213105));
#60524=CARTESIAN_POINT('Ctrl Pts',(2.94493923631214,-0.10687856130158,24.8164025551794));
#60525=CARTESIAN_POINT('Ctrl Pts',(2.90953704486686,-1.08235298169963,24.7633526890482));
#60526=CARTESIAN_POINT('Ctrl Pts',(2.34125201591485,-2.03848786859804,24.710302822917));
#60527=CARTESIAN_POINT('Ctrl Pts',(1.50130740842057,-2.53577723742803,24.6572529567858));
#60528=CARTESIAN_POINT('Ctrl Pts',(0.66136280092637,-3.03306660625799,24.6042030906546));
#60529=CARTESIAN_POINT('Ctrl Pts',(-0.450241385110007,-3.0715104570196,
24.5511532245234));
#60530=CARTESIAN_POINT('Ctrl Pts',(-1.32253468000992,-2.6334373265008,24.4981033583922));
#60531=CARTESIAN_POINT('Ctrl Pts',(-2.1948279749099,-2.19536419598197,24.445053492261));
#60532=CARTESIAN_POINT('Ctrl Pts',(-2.82781037867336,-1.28077408418266,
24.3920036261298));
#60533=CARTESIAN_POINT('Ctrl Pts',(-2.93051922652061,-0.310076112317096,
24.3389537599986));
#60534=CARTESIAN_POINT('Ctrl Pts',(-2.94134685279283,-0.207744569486468,
24.3333612123623));
#60535=CARTESIAN_POINT('Ctrl Pts',(-2.94628128463976,-0.104789472031122,
24.3277686647259));
#60536=CARTESIAN_POINT('Ctrl Pts',(-2.94555278480659,-0.00176380088044714,
24.3221761170896));
#60537=CARTESIAN_POINT('Ctrl Pts',(-2.93722802281203,0.000281837720408654,
24.1778238829105));
#60538=CARTESIAN_POINT('Ctrl Pts',(-2.93679293864966,-0.507380714800876,
24.20518292012));
#60539=CARTESIAN_POINT('Ctrl Pts',(-2.81182371976808,-1.01524392781641,
24.2325419573295));
#60540=CARTESIAN_POINT('Ctrl Pts',(-2.56355212294478,-1.45321026615464,
24.259900994539));
#60541=CARTESIAN_POINT('Ctrl Pts',(-2.08392629039663,-2.2992996792865,24.3127548093419));
#60542=CARTESIAN_POINT('Ctrl Pts',(-1.14412599999694,-2.88452829681116,
24.3656086241448));
#60543=CARTESIAN_POINT('Ctrl Pts',(-0.17322981844223,-2.94170205743451,
24.4184624389477));
#60544=CARTESIAN_POINT('Ctrl Pts',(0.797666363112456,-2.99887581805785,
24.4713162537506));
#60545=CARTESIAN_POINT('Ctrl Pts',(1.7996584358222,-2.52799472177994,24.5241700685536));
#60546=CARTESIAN_POINT('Ctrl Pts',(2.37527333142833,-1.74404591846582,24.5770238833565));
#60547=CARTESIAN_POINT('Ctrl Pts',(2.95088822703446,-0.960097115151713,
24.6298776981594));
#60548=CARTESIAN_POINT('Ctrl Pts',(3.100125945537,0.136919395198534,24.6827315129623));
#60549=CARTESIAN_POINT('Ctrl Pts',(2.75484998282307,1.04614584874751,24.7355853277652));
#60550=CARTESIAN_POINT('Ctrl Pts',(2.40957402010914,1.95537230229652,24.7884391425681));
#60551=CARTESIAN_POINT('Ctrl Pts',(1.56978437617865,2.67680869904419,24.8412929573711));
#60552=CARTESIAN_POINT('Ctrl Pts',(0.618898400893287,2.88107346905344,24.894146772174));
#60553=CARTESIAN_POINT('Ctrl Pts',(-0.331987574392054,3.08533823906269,
24.9470005869769));
#60554=CARTESIAN_POINT('Ctrl Pts',(-1.3939698810323,2.77243138233356,24.9998544017798));
#60555=CARTESIAN_POINT('Ctrl Pts',(-2.08218609597328,2.0852147674634,25.0527082165827));
#60556=CARTESIAN_POINT('Ctrl Pts',(-2.62523507380622,1.54295454145717,25.094413438692));
#60557=CARTESIAN_POINT('Ctrl Pts',(-2.93556705736549,0.767638819576851,
25.1361186608012));
#60558=CARTESIAN_POINT('Ctrl Pts',(-2.94264856609968,-0.00262420787473867,
25.1778238829105));
#60559=CARTESIAN_POINT('Origin',(0.,0.,0.));
#60560=CARTESIAN_POINT('',(-2.93724345526557,0.000625155175501269,26.3221761170896));
#60561=CARTESIAN_POINT('',(-2.94570126337859,0.00159745694066759,26.1778238829105));
#60562=CARTESIAN_POINT('',(-2.942,-3.60291088309151E-16,0.));
#60563=CARTESIAN_POINT('Ctrl Pts',(-2.93724345526557,0.000625155175501269,
26.3221761170896));
#60564=CARTESIAN_POINT('Ctrl Pts',(-2.93810221353313,0.454776386691649,
26.2977003916336));
#60565=CARTESIAN_POINT('Ctrl Pts',(-2.83926083141474,0.9085735093724,26.2732246661775));
#60566=CARTESIAN_POINT('Ctrl Pts',(-2.63878026210633,1.31184178190614,26.2487489407215));
#60567=CARTESIAN_POINT('Ctrl Pts',(-2.20424902082298,2.18590485763848,26.1956990745903));
#60568=CARTESIAN_POINT('Ctrl Pts',(-1.29223400116845,2.82259190792271,26.1426492084591));
#60569=CARTESIAN_POINT('Ctrl Pts',(-0.321960633202111,2.92923735520096,
26.0895993423279));
#60570=CARTESIAN_POINT('Ctrl Pts',(0.648312734764256,3.03588280247922,26.0365494761968));
#60571=CARTESIAN_POINT('Ctrl Pts',(1.67684445104244,2.61248664675148,25.9834996100656));
#60572=CARTESIAN_POINT('Ctrl Pts',(2.29084992130659,1.85367116028875,25.9304497439344));
#60573=CARTESIAN_POINT('Ctrl Pts',(2.90485539157074,1.09485567382602,25.8773998778032));
#60574=CARTESIAN_POINT('Ctrl Pts',(3.10433461582086,0.000620856628295308,
25.824350011672));
#60575=CARTESIAN_POINT('Ctrl Pts',(2.79759309147536,-0.926046989610136,
25.7713001455408));
#60576=CARTESIAN_POINT('Ctrl Pts',(2.49085156712986,-1.85271483584854,25.7182502794096));
#60577=CARTESIAN_POINT('Ctrl Pts',(1.67788929418876,-2.61181571112766,25.6652004132784));
#60578=CARTESIAN_POINT('Ctrl Pts',(0.732400182457275,-2.85441414394849,
25.6121505471472));
#60579=CARTESIAN_POINT('Ctrl Pts',(-0.213088929274242,-3.09701257676932,
25.5591006810161));
#60580=CARTESIAN_POINT('Ctrl Pts',(-1.29110487979616,-2.82310856713184,
25.5060508148848));
#60581=CARTESIAN_POINT('Ctrl Pts',(-2.00611668471787,-2.15860741676972,
25.4530009487536));
#60582=CARTESIAN_POINT('Ctrl Pts',(-2.59387373821273,-1.61237134697007,
25.4093926715323));
#60583=CARTESIAN_POINT('Ctrl Pts',(-2.93634021746692,-0.802199456859896,
25.3657843943109));
#60584=CARTESIAN_POINT('Ctrl Pts',(-2.94363848369983,0.00251143626685393,
25.3221761170896));
#60585=CARTESIAN_POINT('Ctrl Pts',(-2.94264856609968,-0.00262420787473867,
25.1778238829105));
#60586=CARTESIAN_POINT('Ctrl Pts',(-2.94454158698631,-0.208530047137775,
25.1889724756041));
#60587=CARTESIAN_POINT('Ctrl Pts',(-2.92476451808285,-0.414074824008361,
25.2001210682978));
#60588=CARTESIAN_POINT('Ctrl Pts',(-2.88196999784739,-0.61471009119703,
25.2112696609915));
#60589=CARTESIAN_POINT('Ctrl Pts',(-2.67908756153879,-1.56589196197611,
25.2641234757944));
#60590=CARTESIAN_POINT('Ctrl Pts',(-1.95887256567987,-2.40672933052306,
25.3169772905973));
#60591=CARTESIAN_POINT('Ctrl Pts',(-1.05014893306918,-2.75332649409503,
25.3698311054002));
#60592=CARTESIAN_POINT('Ctrl Pts',(-0.141425300458436,-3.09992365766701,
25.4226849202032));
#60593=CARTESIAN_POINT('Ctrl Pts',(0.9558069689041,-2.95228061626393,25.4755387350061));
#60594=CARTESIAN_POINT('Ctrl Pts',(1.74059160347801,-2.37780580254439,25.528392549809));
#60595=CARTESIAN_POINT('Ctrl Pts',(2.52537623805186,-1.8033309888249,25.5812463646119));
#60596=CARTESIAN_POINT('Ctrl Pts',(2.99771323783714,-0.802024402789044,
25.6341001794148));
#60597=CARTESIAN_POINT('Ctrl Pts',(2.94195074047982,0.168953855541036,25.6869539942177));
#60598=CARTESIAN_POINT('Ctrl Pts',(2.88618824312249,1.13993211387114,25.7398078090207));
#60599=CARTESIAN_POINT('Ctrl Pts',(2.30232624862252,2.08058204449547,25.7926616238236));
#60600=CARTESIAN_POINT('Ctrl Pts',(1.45693486800003,2.5614371659515,25.8455154386265));
#60601=CARTESIAN_POINT('Ctrl Pts',(0.61154348737756,3.04229228740752,25.8983692534294));
#60602=CARTESIAN_POINT('Ctrl Pts',(-0.495377279367419,3.06335259969526,
25.9512230682323));
#60603=CARTESIAN_POINT('Ctrl Pts',(-1.35844774583423,2.61500273165246,26.0040768830352));
#60604=CARTESIAN_POINT('Ctrl Pts',(-2.2215182123011,2.16665286360963,26.0569306978382));
#60605=CARTESIAN_POINT('Ctrl Pts',(-2.84073837848977,1.2488928152362,26.1097845126411));
#60606=CARTESIAN_POINT('Ctrl Pts',(-2.93339488062293,0.280738381855969,
26.162638327444));
#60607=CARTESIAN_POINT('Ctrl Pts',(-2.94226866742349,0.188017462826645,
26.1677001792662));
#60608=CARTESIAN_POINT('Ctrl Pts',(-2.94631278858676,0.0948343242288374,
26.1727620310883));
#60609=CARTESIAN_POINT('Ctrl Pts',(-2.94570126337859,0.00159745694066759,
26.1778238829105));
#60610=CARTESIAN_POINT('Origin',(0.,0.,0.));
#60611=CARTESIAN_POINT('',(-2.94133724676478,-0.0027142933295754,27.3221761170896));
#60612=CARTESIAN_POINT('',(-2.9379441153396,0.0014763941512189,27.1778238829104));
#60613=CARTESIAN_POINT('',(-2.942,-3.60291088309151E-16,0.));
#60614=CARTESIAN_POINT('Ctrl Pts',(-2.94133724676478,-0.0027142933295754,
27.3221761170896));
#60615=CARTESIAN_POINT('Ctrl Pts',(-2.93472634309306,0.727831082166025,
27.2826662550874));
#60616=CARTESIAN_POINT('Ctrl Pts',(-2.65946238238259,1.46282296367726,27.2431563930852));
#60617=CARTESIAN_POINT('Ctrl Pts',(-2.16672707396524,1.99734421654923,27.203646531083));
#60618=CARTESIAN_POINT('Ctrl Pts',(-1.50513169435615,2.71504555672481,27.1505966649518));
#60619=CARTESIAN_POINT('Ctrl Pts',(-0.451469932853536,3.07133011774635,
27.0975467988206));
#60620=CARTESIAN_POINT('Ctrl Pts',(0.509922102492116,2.90242477625634,27.0444969326894));
#60621=CARTESIAN_POINT('Ctrl Pts',(1.47131413783779,2.73351943476633,26.9914470665582));
#60622=CARTESIAN_POINT('Ctrl Pts',(2.34043644702647,2.03942419076481,26.938397200427));
#60623=CARTESIAN_POINT('Ctrl Pts',(2.71778006804373,1.13919341385949,26.8853473342958));
#60624=CARTESIAN_POINT('Ctrl Pts',(3.09512368906099,0.238962636954171,26.8322974681646));
#60625=CARTESIAN_POINT('Ctrl Pts',(2.98068862190676,-0.86740367285492,26.7792476020334));
#60626=CARTESIAN_POINT('Ctrl Pts',(2.42707716940252,-1.6713427375023,26.7261977359022));
#60627=CARTESIAN_POINT('Ctrl Pts',(1.87346571689831,-2.47528180214964,26.6731478697711));
#60628=CARTESIAN_POINT('Ctrl Pts',(0.880677879044135,-2.97679362163533,
26.6200980036398));
#60629=CARTESIAN_POINT('Ctrl Pts',(-0.0949321182835713,-2.94534854055591,
26.5670481375087));
#60630=CARTESIAN_POINT('Ctrl Pts',(-1.07054211561136,-2.91390345947649,
26.5139982713775));
#60631=CARTESIAN_POINT('Ctrl Pts',(-2.0289742724127,-2.34950147783184,26.4609484052463));
#60632=CARTESIAN_POINT('Ctrl Pts',(-2.52966661935728,-1.51158093641926,
26.4078985391151));
#60633=CARTESIAN_POINT('Ctrl Pts',(-2.79935351208561,-1.06025351241171,
26.3793243984399));
#60634=CARTESIAN_POINT('Ctrl Pts',(-2.93624089950528,-0.529572864918339,
26.3507502577648));
#60635=CARTESIAN_POINT('Ctrl Pts',(-2.93724345526557,0.000625155175501269,
26.3221761170896));
#60636=CARTESIAN_POINT('Ctrl Pts',(-2.94570126337859,0.00159745694066759,
26.1778238829105));
#60637=CARTESIAN_POINT('Ctrl Pts',(-2.93992748904903,-0.8787074327395,26.2256158458912));
#60638=CARTESIAN_POINT('Ctrl Pts',(-2.51913195498579,-1.76380189917085,
26.273407808872));
#60639=CARTESIAN_POINT('Ctrl Pts',(-1.82977959360776,-2.30987579829058,
26.3211997718528));
#60640=CARTESIAN_POINT('Ctrl Pts',(-1.0674149663818,-2.91378672666985,26.3740535866557));
#60641=CARTESIAN_POINT('Ctrl Pts',(0.0234071261477989,-3.10305976504139,
26.4269074014586));
#60642=CARTESIAN_POINT('Ctrl Pts',(0.944657065598613,-2.79127974110918,
26.4797612162615));
#60643=CARTESIAN_POINT('Ctrl Pts',(1.86590700504943,-2.47949971717697,26.5326150310644));
#60644=CARTESIAN_POINT('Ctrl Pts',(2.61758479142146,-1.66666663094102,26.5854688458673));
#60645=CARTESIAN_POINT('Ctrl Pts',(2.85650173825782,-0.723890450304441,
26.6383226606703));
#60646=CARTESIAN_POINT('Ctrl Pts',(3.09541868509418,0.218885730332135,26.6911764754732));
#60647=CARTESIAN_POINT('Ctrl Pts',(2.82157479239486,1.29160500536933,26.7440302902761));
#60648=CARTESIAN_POINT('Ctrl Pts',(2.15999720281805,2.00450284323323,26.796884105079));
#60649=CARTESIAN_POINT('Ctrl Pts',(1.49841961324124,2.71740068109714,26.8497379198819));
#60650=CARTESIAN_POINT('Ctrl Pts',(0.449108326786933,3.07047708178776,26.9025917346849));
#60651=CARTESIAN_POINT('Ctrl Pts',(-0.508859359581332,2.90253022669505,
26.9554455494878));
#60652=CARTESIAN_POINT('Ctrl Pts',(-1.4668270459496,2.73458337160234,27.0082993642907));
#60653=CARTESIAN_POINT('Ctrl Pts',(-2.33345113223182,2.0456132607263,27.0611531790936));
#60654=CARTESIAN_POINT('Ctrl Pts',(-2.7130626400236,1.15017854093185,27.1140069938965));
#60655=CARTESIAN_POINT('Ctrl Pts',(-2.86584647440086,0.789789176761778,
27.1352792902345));
#60656=CARTESIAN_POINT('Ctrl Pts',(-2.9397413453216,0.395955545015464,27.1565515865725));
#60657=CARTESIAN_POINT('Ctrl Pts',(-2.9379441153396,0.0014763941512189,
27.1778238829104));
#60658=CARTESIAN_POINT('Origin',(0.,0.,0.));
#60659=CARTESIAN_POINT('',(-2.94676864247139,0.000515229547840817,28.3221761170896));
#60660=CARTESIAN_POINT('',(-2.94035116299482,-0.00254728619478539,28.1778238829105));
#60661=CARTESIAN_POINT('',(-2.942,-3.60291088309151E-16,0.));
#60662=CARTESIAN_POINT('Ctrl Pts',(-2.94676864247139,0.000515229547840817,
28.3221761170896));
#60663=CARTESIAN_POINT('Ctrl Pts',(-2.94683491423248,0.0280099856412504,
28.3206819846724));
#60664=CARTESIAN_POINT('Ctrl Pts',(-2.9464835583305,0.0555030051240508,
28.3191878522552));
#60665=CARTESIAN_POINT('Ctrl Pts',(-2.94570938304831,0.0829841132854057,
28.317693719838));
#60666=CARTESIAN_POINT('Ctrl Pts',(-2.9182219297212,1.05871363519171,28.2646438537068));
#60667=CARTESIAN_POINT('Ctrl Pts',(-2.35771228185992,2.01942729218297,28.2115939875756));
#60668=CARTESIAN_POINT('Ctrl Pts',(-1.52182959338531,2.52351437902251,28.1585441214444));
#60669=CARTESIAN_POINT('Ctrl Pts',(-0.685946904910668,3.02760146586206,
28.1054942553132));
#60670=CARTESIAN_POINT('Ctrl Pts',(0.425308824177326,3.07506198254987,28.052444389182));
#60671=CARTESIAN_POINT('Ctrl Pts',(1.30112729920903,2.6440797801295,27.9993945230508));
#60672=CARTESIAN_POINT('Ctrl Pts',(2.17694577424074,2.21309757770913,27.9463446569197));
#60673=CARTESIAN_POINT('Ctrl Pts',(2.81732699521616,1.30367265618058,27.8932947907884));
#60674=CARTESIAN_POINT('Ctrl Pts',(2.92790728721788,0.333839856657492,27.8402449246573));
#60675=CARTESIAN_POINT('Ctrl Pts',(3.03848757921959,-0.635992942865569,
27.7871950585261));
#60676=CARTESIAN_POINT('Ctrl Pts',(2.61926694224765,-1.66623362038317,27.7341451923949));
#60677=CARTESIAN_POINT('Ctrl Pts',(1.86294829021996,-2.28331202431976,27.6810953262637));
#60678=CARTESIAN_POINT('Ctrl Pts',(1.10662963819224,-2.90039042825636,27.6280454601325));
#60679=CARTESIAN_POINT('Ctrl Pts',(0.0132129711087428,-3.10430655861194,
27.5749955940013));
#60680=CARTESIAN_POINT('Ctrl Pts',(-0.914691487938128,-2.80132640267609,
27.5219457278701));
#60681=CARTESIAN_POINT('Ctrl Pts',(-1.84259594698497,-2.49834624674026,
27.4688958617389));
#60682=CARTESIAN_POINT('Ctrl Pts',(-2.6049881979952,-1.68846980451303,27.4158459956077));
#60683=CARTESIAN_POINT('Ctrl Pts',(-2.85141982464256,-0.74397252373459,
27.3627961294765));
#60684=CARTESIAN_POINT('Ctrl Pts',(-2.91431697190524,-0.502906937443884,
27.3492561253476));
#60685=CARTESIAN_POINT('Ctrl Pts',(-2.9436027991731,-0.253071720547933,
27.3357161212186));
#60686=CARTESIAN_POINT('Ctrl Pts',(-2.94133724676478,-0.0027142933295754,
27.3221761170896));
#60687=CARTESIAN_POINT('Ctrl Pts',(-2.9379441153396,0.0014763941512189,
27.1778238829104));
#60688=CARTESIAN_POINT('Ctrl Pts',(-2.93527589132841,-0.58417972821138,
27.2094054013754));
#60689=CARTESIAN_POINT('Ctrl Pts',(-2.76577241378268,-1.17125865882499,
27.2409869198403));
#60690=CARTESIAN_POINT('Ctrl Pts',(-2.43989484316183,-1.65243236443258,
27.2725684383053));
#60691=CARTESIAN_POINT('Ctrl Pts',(-1.89451660920699,-2.45770922128962,
27.3254222531082));
#60692=CARTESIAN_POINT('Ctrl Pts',(-0.911161211996041,-2.96636360629089,
27.3782760679111));
#60693=CARTESIAN_POINT('Ctrl Pts',(0.0612071071330964,-2.94616246238192,
27.431129882714));
#60694=CARTESIAN_POINT('Ctrl Pts',(1.03357542626229,-2.92596131847296,27.4839836975169));
#60695=CARTESIAN_POINT('Ctrl Pts',(1.99495666730963,-2.3769046456537,27.5368375123199));
#60696=CARTESIAN_POINT('Ctrl Pts',(2.5064191879131,-1.54967171335511,27.5896913271228));
#60697=CARTESIAN_POINT('Ctrl Pts',(3.01788170851653,-0.722438781056572,
27.6425451419257));
#60698=CARTESIAN_POINT('Ctrl Pts',(3.07942550867611,0.38297041072131,27.6953989567286));
#60699=CARTESIAN_POINT('Ctrl Pts',(2.66295193186737,1.26186630562661,27.7482527715315));
#60700=CARTESIAN_POINT('Ctrl Pts',(2.24647835505861,2.14076220053196,27.8011065863344));
#60701=CARTESIAN_POINT('Ctrl Pts',(1.35198740128158,2.79314479856472,27.8539604011373));
#60702=CARTESIAN_POINT('Ctrl Pts',(0.387871045182579,2.92115997799177,27.9068142159403));
#60703=CARTESIAN_POINT('Ctrl Pts',(-0.576245310916365,3.04917515741882,
27.9596680307432));
#60704=CARTESIAN_POINT('Ctrl Pts',(-1.60998706933728,2.6528229182401,28.0125218455461));
#60705=CARTESIAN_POINT('Ctrl Pts',(-2.24138541226995,1.91306324996728,28.065375660349));
#60706=CARTESIAN_POINT('Ctrl Pts',(-2.68915896564396,1.38844227334775,28.1028584012028));
#60707=CARTESIAN_POINT('Ctrl Pts',(-2.93458079833888,0.691110419661017,
28.1403411420566));
#60708=CARTESIAN_POINT('Ctrl Pts',(-2.94035116299482,-0.00254728619478539,
28.1778238829105));
#60709=CARTESIAN_POINT('Origin',(0.,0.,0.));
#60710=CARTESIAN_POINT('',(-2.93977218479318,0.00247205850073318,29.3221761170896));
#60711=CARTESIAN_POINT('',(-2.94676321920776,0.000286364410989904,29.1778238829104));
#60712=CARTESIAN_POINT('',(-2.942,-3.60291088309151E-16,0.));
#60713=CARTESIAN_POINT('Ctrl Pts',(-2.93977218479318,0.00247205850073318,
29.3221761170896));
#60714=CARTESIAN_POINT('Ctrl Pts',(-2.94219100511596,0.308495628903927,
29.3056478481262));
#60715=CARTESIAN_POINT('Ctrl Pts',(-2.89823697117032,0.613841578117692,
29.2891195791628));
#60716=CARTESIAN_POINT('Ctrl Pts',(-2.80501362181614,0.903320936247213,
29.2725913101994));
#60717=CARTESIAN_POINT('Ctrl Pts',(-2.50579981942117,1.8324467406818,29.2195414440682));
#60718=CARTESIAN_POINT('Ctrl Pts',(-1.69902253333613,2.59811782328335,29.166491577937));
#60719=CARTESIAN_POINT('Ctrl Pts',(-0.755532623944009,2.84837858905605,
29.1134417118058));
#60720=CARTESIAN_POINT('Ctrl Pts',(0.187957285448161,3.09863935482876,29.0603918456747));
#60721=CARTESIAN_POINT('Ctrl Pts',(1.26815981814739,2.83348980377255,29.0073419795435));
#60722=CARTESIAN_POINT('Ctrl Pts',(1.98853888476605,2.1748110805792,28.9542921134123));
#60723=CARTESIAN_POINT('Ctrl Pts',(2.7089179513847,1.51613235738584,28.9012422472811));
#60724=CARTESIAN_POINT('Ctrl Pts',(3.06947355192275,0.463924462055363,28.8481923811499));
#60725=CARTESIAN_POINT('Ctrl Pts',(2.90446929669537,-0.498144795205691,
28.7951425150187));
#60726=CARTESIAN_POINT('Ctrl Pts',(2.73946504146801,-1.46021405246669,28.7420926488875));
#60727=CARTESIAN_POINT('Ctrl Pts',(2.04890093047521,-2.33214467165833,28.6890427827563));
#60728=CARTESIAN_POINT('Ctrl Pts',(1.15020817940491,-2.71313679648975,28.6359929166252));
#60729=CARTESIAN_POINT('Ctrl Pts',(0.251515428334551,-3.0941289213212,28.582943050494));
#60730=CARTESIAN_POINT('Ctrl Pts',(-0.855305962813357,-2.98418255179246,
28.5298931843628));
#60731=CARTESIAN_POINT('Ctrl Pts',(-1.66148402899086,-2.43383667361739,
28.4768433182316));
#60732=CARTESIAN_POINT('Ctrl Pts',(-2.4449563492249,-1.89899111009379,28.4252875845176));
#60733=CARTESIAN_POINT('Ctrl Pts',(-2.94448190454346,-0.948204112437949,
28.3737318508036));
#60734=CARTESIAN_POINT('Ctrl Pts',(-2.94676864247139,0.000515229547840817,
28.3221761170896));
#60735=CARTESIAN_POINT('Ctrl Pts',(-2.94035116299482,-0.00254728619478539,
28.1778238829105));
#60736=CARTESIAN_POINT('Ctrl Pts',(-2.94271749746822,-0.287005243355917,
28.1931949568596));
#60737=CARTESIAN_POINT('Ctrl Pts',(-2.90478190263403,-0.570845323032888,
28.2085660308087));
#60738=CARTESIAN_POINT('Ctrl Pts',(-2.82397206139089,-0.841903415598018,
28.2239371047578));
#60739=CARTESIAN_POINT('Ctrl Pts',(-2.54610544013462,-1.7739433155234,28.2767909195607));
#60740=CARTESIAN_POINT('Ctrl Pts',(-1.76131727017756,-2.55485601800717,
28.3296447343636));
#60741=CARTESIAN_POINT('Ctrl Pts',(-0.827913232594077,-2.82810523920302,
28.3824985491665));
#60742=CARTESIAN_POINT('Ctrl Pts',(0.10549080498941,-3.10135446039886,28.4353523639694));
#60743=CARTESIAN_POINT('Ctrl Pts',(1.18751071019935,-2.86694020030677,28.4882061787723));
#60744=CARTESIAN_POINT('Ctrl Pts',(1.92413562263573,-2.23188746813457,28.5410599935753));
#60745=CARTESIAN_POINT('Ctrl Pts',(2.66076053507213,-1.59683473596234,28.5939138083782));
#60746=CARTESIAN_POINT('Ctrl Pts',(3.05199045473495,-0.561143531710042,
28.6467676231811));
#60747=CARTESIAN_POINT('Ctrl Pts',(2.91920405654855,0.402327280882647,28.699621437984));
#60748=CARTESIAN_POINT('Ctrl Pts',(2.78641765836215,1.36579809347531,28.7524752527869));
#60749=CARTESIAN_POINT('Ctrl Pts',(2.12961494232652,2.25704851440832,28.8053290675899));
#60750=CARTESIAN_POINT('Ctrl Pts',(1.24866809498787,2.66916607824828,28.8581828823928));
#60751=CARTESIAN_POINT('Ctrl Pts',(0.367721247649218,3.08128364208823,28.9110366971957));
#60752=CARTESIAN_POINT('Ctrl Pts',(-0.737369730992477,3.01426834883514,
28.9638905119986));
#60753=CARTESIAN_POINT('Ctrl Pts',(-1.5620605691078,2.4987169393812,29.0167443268015));
#60754=CARTESIAN_POINT('Ctrl Pts',(-2.38675140722314,1.98316552992725,29.0695981416044));
#60755=CARTESIAN_POINT('Ctrl Pts',(-2.93104210481211,1.01907800427242,29.1224519564074));
#60756=CARTESIAN_POINT('Ctrl Pts',(-2.94642936306387,0.0466215957147753,
29.1753057712103));
#60757=CARTESIAN_POINT('Ctrl Pts',(-2.94667372786,0.0311780314270079,29.176145141777));
#60758=CARTESIAN_POINT('Ctrl Pts',(-2.94678470022545,0.0157323564597679,
29.1769845123437));
#60759=CARTESIAN_POINT('Ctrl Pts',(-2.94676321920776,0.000286364410989904,
29.1778238829104));
#60760=CARTESIAN_POINT('Origin',(0.,0.,0.));
#60761=CARTESIAN_POINT('',(-2.93783810979555,-0.00147013671584123,30.3221761170896));
#60762=CARTESIAN_POINT('',(-2.93953450219412,0.00234327334966803,30.1778238829105));
#60763=CARTESIAN_POINT('',(-2.942,-3.60291088309151E-16,0.));
#60764=CARTESIAN_POINT('Ctrl Pts',(-2.93783810979555,-0.00147013671584123,
30.3221761170896));
#60765=CARTESIAN_POINT('Ctrl Pts',(-2.93520375456558,0.583879716040712,
30.29061371158));
#60766=CARTESIAN_POINT('Ctrl Pts',(-2.7660401693521,1.17063223301724,30.2590513060705));
#60767=CARTESIAN_POINT('Ctrl Pts',(-2.44055613232114,1.65159798299293,30.2274889005609));
#60768=CARTESIAN_POINT('Ctrl Pts',(-1.89348488367694,2.46000178612405,30.1744390344297));
#60769=CARTESIAN_POINT('Ctrl Pts',(-0.904798249272084,2.96955113115784,
30.1213891682985));
#60770=CARTESIAN_POINT('Ctrl Pts',(0.0710347428950288,2.94602175785218,
30.0683393021673));
#60771=CARTESIAN_POINT('Ctrl Pts',(1.04686773506211,2.92249238454653,30.0152894360361));
#60772=CARTESIAN_POINT('Ctrl Pts',(2.00984708499145,2.36588429290148,29.9622395699049));
#60773=CARTESIAN_POINT('Ctrl Pts',(2.51732061765051,1.5320532106909,29.9091897037737));
#60774=CARTESIAN_POINT('Ctrl Pts',(3.02479415030958,0.698222128480303,29.8561398376426));
#60775=CARTESIAN_POINT('Ctrl Pts',(3.07676186569834,-0.412831944295833,
29.8030899715113));
#60776=CARTESIAN_POINT('Ctrl Pts',(2.64933579337382,-1.29039140821108,29.7500401053801));
#60777=CARTESIAN_POINT('Ctrl Pts',(2.22190972104931,-2.16795087212629,29.6969902392489));
#60778=CARTESIAN_POINT('Ctrl Pts',(1.31508986101154,-2.81201572718063,29.6439403731178));
#60779=CARTESIAN_POINT('Ctrl Pts',(0.345713587226916,-2.92652904445579,
29.5908905069866));
#60780=CARTESIAN_POINT('Ctrl Pts',(-0.623662686557708,-3.04104236173095,
29.5378406408554));
#60781=CARTESIAN_POINT('Ctrl Pts',(-1.65559537408919,-2.62600414122694,
29.4847907747242));
#60782=CARTESIAN_POINT('Ctrl Pts',(-2.27573655850254,-1.87219476784112,
29.431740908593));
#60783=CARTESIAN_POINT('Ctrl Pts',(-2.70266593978139,-1.35324299126101,
29.3952193114252));
#60784=CARTESIAN_POINT('Ctrl Pts',(-2.93442745198144,-0.673731214018755,
29.3586977142574));
#60785=CARTESIAN_POINT('Ctrl Pts',(-2.93977218479318,0.00247205850073318,
29.3221761170896));
#60786=CARTESIAN_POINT('Ctrl Pts',(-2.94676321920776,0.000286364410989904,
29.1778238829104));
#60787=CARTESIAN_POINT('Ctrl Pts',(-2.94543207508477,-0.956876924304651,
29.2298383271466));
#60788=CARTESIAN_POINT('Ctrl Pts',(-2.43546913201457,-1.9152578319996,29.2818527713828));
#60789=CARTESIAN_POINT('Ctrl Pts',(-1.64033359579244,-2.44804519141836,
29.333867215619));
#60790=CARTESIAN_POINT('Ctrl Pts',(-0.832366751354701,-2.98943027853342,
29.386721030422));
#60791=CARTESIAN_POINT('Ctrl Pts',(0.270050756435348,-3.09137516130311,
29.4395748452249));
#60792=CARTESIAN_POINT('Ctrl Pts',(1.16359526511913,-2.70733552108051,29.4924286600278));
#60793=CARTESIAN_POINT('Ctrl Pts',(2.05713977380296,-2.32329588085788,29.5452824748307));
#60794=CARTESIAN_POINT('Ctrl Pts',(2.74181128338049,-1.45327171764289,29.5981362896336));
#60795=CARTESIAN_POINT('Ctrl Pts',(2.90501373170058,-0.494484361070186,
29.6509901044365));
#60796=CARTESIAN_POINT('Ctrl Pts',(3.06821618002067,0.464302995502493,29.7038439192394));
#60797=CARTESIAN_POINT('Ctrl Pts',(2.70994956708335,1.51185354543288,29.7566977340424));
#60798=CARTESIAN_POINT('Ctrl Pts',(1.99378537328151,2.16989387989381,29.8095515488453));
#60799=CARTESIAN_POINT('Ctrl Pts',(1.27762117947965,2.82793421435476,29.8624053636482));
#60800=CARTESIAN_POINT('Ctrl Pts',(0.203559404813244,3.09646433334624,29.9152591784511));
#60801=CARTESIAN_POINT('Ctrl Pts',(-0.738022482733161,2.85288316965352,
29.968112993254));
#60802=CARTESIAN_POINT('Ctrl Pts',(-1.67960437027954,2.6093020059608,30.0209668080569));
#60803=CARTESIAN_POINT('Ctrl Pts',(-2.48870637070592,1.85360955958394,30.0738206228599));
#60804=CARTESIAN_POINT('Ctrl Pts',(-2.79592199393075,0.930827464445613,
30.1266744376628));
#60805=CARTESIAN_POINT('Ctrl Pts',(-2.89502495529665,0.633152374345404,
30.1437242527454));
#60806=CARTESIAN_POINT('Ctrl Pts',(-2.94190127783126,0.318089821395596,
30.1607740678279));
#60807=CARTESIAN_POINT('Ctrl Pts',(-2.93953450219412,0.00234327334966803,
30.1778238829105));
#60808=CARTESIAN_POINT('Origin',(0.,0.,0.));
#60809=CARTESIAN_POINT('',(-2.94517042509113,-0.00197354254748233,31.3221761170896));
#60810=CARTESIAN_POINT('',(-2.93848416988746,-0.00187374481244229,31.1778238829104));
#60811=CARTESIAN_POINT('',(-2.942,-3.60291088309151E-16,0.));
#60812=CARTESIAN_POINT('Ctrl Pts',(-2.94517042509113,-0.00197354254748233,
31.3221761170896));
#60813=CARTESIAN_POINT('Ctrl Pts',(-2.93855277029816,0.856718198839958,
31.2755795750338));
#60814=CARTESIAN_POINT('Ctrl Pts',(-2.54130670618931,1.72073915113778,31.2289830329781));
#60815=CARTESIAN_POINT('Ctrl Pts',(-1.88141044101362,2.26812364849925,31.1823864909223));
#60816=CARTESIAN_POINT('Ctrl Pts',(-1.13012274918965,2.89131740979965,31.1293366247911));
#60817=CARTESIAN_POINT('Ctrl Pts',(-0.0383963406818305,3.10409721392047,
31.0762867586599));
#60818=CARTESIAN_POINT('Ctrl Pts',(0.891935521624298,2.80865468822734,31.0232368925287));
#60819=CARTESIAN_POINT('Ctrl Pts',(1.82226738393048,2.5132121625342,30.9701870263976));
#60820=CARTESIAN_POINT('Ctrl Pts',(2.59120470003495,1.70954730702706,30.9171371602664));
#60821=CARTESIAN_POINT('Ctrl Pts',(2.84529048722843,0.767080292879461,30.8640872941352));
#60822=CARTESIAN_POINT('Ctrl Pts',(3.09937627442189,-0.175386721268062,
30.811037428004));
#60823=CARTESIAN_POINT('Ctrl Pts',(2.83861053270447,-1.25665589405602,30.7579875618728));
#60824=CARTESIAN_POINT('Ctrl Pts',(2.18285930359996,-1.97970083424839,30.7049376957416));
#60825=CARTESIAN_POINT('Ctrl Pts',(1.5271080744954,-2.70274577444079,30.6518878296104));
#60826=CARTESIAN_POINT('Ctrl Pts',(0.476371358003699,-3.06756648203756,
30.5988379634792));
#60827=CARTESIAN_POINT('Ctrl Pts',(-0.486359291616223,-2.90646602799606,
30.545788097348));
#60828=CARTESIAN_POINT('Ctrl Pts',(-1.44908994123612,-2.74536557395456,
30.4927382312169));
#60829=CARTESIAN_POINT('Ctrl Pts',(-2.32381452398424,-2.05834395827482,
30.4396883650856));
#60830=CARTESIAN_POINT('Ctrl Pts',(-2.70844888391655,-1.16120401982074,
30.3866384989544));
#60831=CARTESIAN_POINT('Ctrl Pts',(-2.86424222074291,-0.797824043480206,
30.3651510383328));
#60832=CARTESIAN_POINT('Ctrl Pts',(-2.93963156005239,-0.399972142754944,
30.3436635777112));
#60833=CARTESIAN_POINT('Ctrl Pts',(-2.93783810979555,-0.00147013671584123,
30.3221761170896));
#60834=CARTESIAN_POINT('Ctrl Pts',(-2.93953450219412,0.00234327334966803,
30.1778238829105));
#60835=CARTESIAN_POINT('Ctrl Pts',(-2.93456435830457,-0.660713144752601,
30.2136278826308));
#60836=CARTESIAN_POINT('Ctrl Pts',(-2.71243957464638,-1.32678587811968,
30.2494318823512));
#60837=CARTESIAN_POINT('Ctrl Pts',(-2.30078930455155,-1.84119204342544,
30.2852358820715));
#60838=CARTESIAN_POINT('Ctrl Pts',(-1.69311174592427,-2.60055771225837,
30.3380896968744));
#60839=CARTESIAN_POINT('Ctrl Pts',(-0.67242738264646,-3.02941730602445,
30.3909435116774));
#60840=CARTESIAN_POINT('Ctrl Pts',(0.295256498288523,-2.93196916166087,
30.4437973264803));
#60841=CARTESIAN_POINT('Ctrl Pts',(1.26294037922351,-2.83452101729728,30.4966511412832));
#60842=CARTESIAN_POINT('Ctrl Pts',(2.17762377781566,-2.21076513480403,30.5495049560861));
#60843=CARTESIAN_POINT('Ctrl Pts',(2.62169558491961,-1.34548572074361,30.602358770889));
#60844=CARTESIAN_POINT('Ctrl Pts',(3.06576739202355,-0.480206306683199,
30.6552125856919));
#60845=CARTESIAN_POINT('Ctrl Pts',(3.03922760763929,0.626596638944376,30.7080664004949));
#60846=CARTESIAN_POINT('Ctrl Pts',(2.55419333021886,1.46959722256727,30.7609202152978));
#60847=CARTESIAN_POINT('Ctrl Pts',(2.06915905279841,2.31259780619018,30.8137740301007));
#60848=CARTESIAN_POINT('Ctrl Pts',(1.12563028234178,2.8917960278084,30.8666278449037));
#60849=CARTESIAN_POINT('Ctrl Pts',(0.154387873675291,2.94275108515381,30.9194816597066));
#60850=CARTESIAN_POINT('Ctrl Pts',(-0.816854534991167,2.99370614249923,
30.9723354745095));
#60851=CARTESIAN_POINT('Ctrl Pts',(-1.81581058186747,2.51641803557186,31.0251892893124));
#60852=CARTESIAN_POINT('Ctrl Pts',(-2.38639333745911,1.72879912183073,31.0780431041153));
#60853=CARTESIAN_POINT('Ctrl Pts',(-2.74545409105091,1.23316016685073,31.1113033637137));
#60854=CARTESIAN_POINT('Ctrl Pts',(-2.93487769090008,0.614629248581725,
31.1445636233121));
#60855=CARTESIAN_POINT('Ctrl Pts',(-2.93848416988746,-0.00187374481244229,
31.1778238829104));
#60856=CARTESIAN_POINT('Origin',(0.,0.,0.));
#60857=CARTESIAN_POINT('',(-2.94410448200555,0.00238870800367233,32.3221761170895));
#60858=CARTESIAN_POINT('',(-2.94627736789538,-0.00111514688795235,32.1778238829105));
#60859=CARTESIAN_POINT('',(-2.942,-3.60291088309151E-16,0.));
#60860=CARTESIAN_POINT('Ctrl Pts',(-2.94410448200555,0.00238870800367233,
32.3221761170895));
#60861=CARTESIAN_POINT('Ctrl Pts',(-2.94549825313968,0.160667033072669,
32.3135953046188));
#60862=CARTESIAN_POINT('Ctrl Pts',(-2.93384105715144,0.318739746346453,
32.3050144921481));
#60863=CARTESIAN_POINT('Ctrl Pts',(-2.90841493730487,0.474565785638333,
32.2964336796773));
#60864=CARTESIAN_POINT('Ctrl Pts',(-2.75122093514068,1.4379419871783,32.2433838135461));
#60865=CARTESIAN_POINT('Ctrl Pts',(-2.06775311879117,2.31544614106569,32.190333947415));
#60866=CARTESIAN_POINT('Ctrl Pts',(-1.17218075418514,2.70371640745745,32.1372840812838));
#60867=CARTESIAN_POINT('Ctrl Pts',(-0.276608389579133,3.09198667384919,
32.0842342151526));
#60868=CARTESIAN_POINT('Ctrl Pts',(0.831068523283415,2.99102305274535,32.0311843490214));
#60869=CARTESIAN_POINT('Ctrl Pts',(1.64168476217013,2.44723543495411,31.9781344828902));
#60870=CARTESIAN_POINT('Ctrl Pts',(2.45230100105687,1.90344781716287,31.925084616759));
#60871=CARTESIAN_POINT('Ctrl Pts',(2.96585656596776,0.91683620268427,31.8720347506278));
#60872=CARTESIAN_POINT('Ctrl Pts',(2.94628565982781,-0.0590842037233539,
31.8189848844966));
#60873=CARTESIAN_POINT('Ctrl Pts',(2.92671475368787,-1.03500461013098,31.7659350183654));
#60874=CARTESIAN_POINT('Ctrl Pts',(2.37401737649702,-2.0002338084676,31.7128851522342));
#60875=CARTESIAN_POINT('Ctrl Pts',(1.54225162012017,-2.5110854371513,31.659835286103));
#60876=CARTESIAN_POINT('Ctrl Pts',(0.710485863743306,-3.02193706583501,
31.6067854199718));
#60877=CARTESIAN_POINT('Ctrl Pts',(-0.400348271819595,-3.07841112486583,
31.5537355538407));
#60878=CARTESIAN_POINT('Ctrl Pts',(-1.27963428555693,-2.65454821535866,
31.5006856877095));
#60879=CARTESIAN_POINT('Ctrl Pts',(-2.15892029929426,-2.2306853058515,31.4476358215783));
#60880=CARTESIAN_POINT('Ctrl Pts',(-2.80665819120605,-1.32648542780635,
31.3945859554471));
#60881=CARTESIAN_POINT('Ctrl Pts',(-2.92510264959188,-0.357581629543773,
31.3415360893159));
#60882=CARTESIAN_POINT('Ctrl Pts',(-2.93951098896476,-0.239717991723232,
31.3350827652405));
#60883=CARTESIAN_POINT('Ctrl Pts',(-2.94608692810003,-0.120896875558947,
31.328629441165));
#60884=CARTESIAN_POINT('Ctrl Pts',(-2.94517042509113,-0.00197354254748233,
31.3221761170896));
#60885=CARTESIAN_POINT('Ctrl Pts',(-2.93848416988746,-0.00187374481244229,
31.1778238829104));
#60886=CARTESIAN_POINT('Ctrl Pts',(-2.9406087397491,-0.365054477034348,
31.197417438115));
#60887=CARTESIAN_POINT('Ctrl Pts',(-2.87824797656616,-0.727531445198681,
31.2170109933195));
#60888=CARTESIAN_POINT('Ctrl Pts',(-2.74809407102639,-1.06376620622274,
31.2366045485241));
#60889=CARTESIAN_POINT('Ctrl Pts',(-2.39700258469507,-1.9707628999802,31.289458363327));
#60890=CARTESIAN_POINT('Ctrl Pts',(-1.55261014772547,-2.68680656694023,
31.3423121781299));
#60891=CARTESIAN_POINT('Ctrl Pts',(-0.600435577557133,-2.88497776107816,
31.3951659929328));
#60892=CARTESIAN_POINT('Ctrl Pts',(0.351738992611175,-3.08314895521609,
31.4480198077357));
#60893=CARTESIAN_POINT('Ctrl Pts',(1.41169569597818,-2.76344767653195,31.5008736225387));
#60894=CARTESIAN_POINT('Ctrl Pts',(2.09549692613227,-2.07183787910206,31.5537274373416));
#60895=CARTESIAN_POINT('Ctrl Pts',(2.7792981562864,-1.38022808167213,31.6065812521445));
#60896=CARTESIAN_POINT('Ctrl Pts',(3.08694391322754,-0.31670976549634,31.6594350669474));
#60897=CARTESIAN_POINT('Ctrl Pts',(2.8779743548094,0.633153360388591,31.7122888817503));
#60898=CARTESIAN_POINT('Ctrl Pts',(2.66900479639126,1.5830164862735,31.7651426965532));
#60899=CARTESIAN_POINT('Ctrl Pts',(1.94341992261392,2.41922442186759,31.8179965113562));
#60900=CARTESIAN_POINT('Ctrl Pts',(1.03249534685752,2.75999509481983,31.8708503261591));
#60901=CARTESIAN_POINT('Ctrl Pts',(0.121570771101085,3.10076576777208,31.923704140962));
#60902=CARTESIAN_POINT('Ctrl Pts',(-0.97469350663439,2.94609917808244,31.9765579557649));
#60903=CARTESIAN_POINT('Ctrl Pts',(-1.75578316451228,2.36661045462222,32.0294117705678));
#60904=CARTESIAN_POINT('Ctrl Pts',(-2.48687618959725,1.82421412461807,32.078882474682));
#60905=CARTESIAN_POINT('Ctrl Pts',(-2.94185119889749,0.909639842305583,
32.1283531787962));
#60906=CARTESIAN_POINT('Ctrl Pts',(-2.94627736789538,-0.00111514688795235,
32.1778238829105));
#60907=CARTESIAN_POINT('Origin',(0.,0.,0.));
#60908=CARTESIAN_POINT('',(-2.93736495050316,0.000879932274083783,33.3221761170896));
#60909=CARTESIAN_POINT('',(-2.94171210674826,0.00267199037597989,33.1778238829104));
#60910=CARTESIAN_POINT('',(-2.942,-3.60291088309151E-16,0.));
#60911=CARTESIAN_POINT('Ctrl Pts',(-2.93736495050316,0.000879932274083783,
33.3221761170896));
#60912=CARTESIAN_POINT('Ctrl Pts',(-2.93853387350149,0.439014109857465,
33.2985611680727));
#60913=CARTESIAN_POINT('Ctrl Pts',(-2.84680871230498,0.87668310875137,33.2749462190557));
#60914=CARTESIAN_POINT('Ctrl Pts',(-2.65971696032059,1.26885610824061,33.2513312700388));
#60915=CARTESIAN_POINT('Ctrl Pts',(-2.2394241877252,2.14985420433057,33.1982814039076));
#60916=CARTESIAN_POINT('Ctrl Pts',(-1.33785916906647,2.80125447544335,33.1452315377764));
#60917=CARTESIAN_POINT('Ctrl Pts',(-0.36944378833565,2.92362812609551,33.0921816716452));
#60918=CARTESIAN_POINT('Ctrl Pts',(0.598971592395111,3.04600177674767,33.039131805514));
#60919=CARTESIAN_POINT('Ctrl Pts',(1.63423733519791,2.63934880693927,32.9860819393828));
#60920=CARTESIAN_POINT('Ctrl Pts',(2.26047341956974,1.89059515810641,32.9330320732517));
#60921=CARTESIAN_POINT('Ctrl Pts',(2.88670950394163,1.14184150927349,32.8799822071205));
#60922=CARTESIAN_POINT('Ctrl Pts',(3.10391592988244,0.0509871814159728,
32.8269323409893));
#60923=CARTESIAN_POINT('Ctrl Pts',(2.81224954200074,-0.880535431401397,
32.7738824748581));
#60924=CARTESIAN_POINT('Ctrl Pts',(2.52058315411905,-1.81205804421874,32.7208326087269));
#60925=CARTESIAN_POINT('Ctrl Pts',(1.72004395241494,-2.584248941996,32.6677827425957));
#60926=CARTESIAN_POINT('Ctrl Pts',(0.778615340539899,-2.84215556997019,
32.6147328764645));
#60927=CARTESIAN_POINT('Ctrl Pts',(-0.162813271335088,-3.10006219794436,
32.5616830103333));
#60928=CARTESIAN_POINT('Ctrl Pts',(-1.24513129338095,-2.84368455611553,
32.5086331442021));
#60929=CARTESIAN_POINT('Ctrl Pts',(-1.97083021041444,-2.19087161060488,
32.4555832780709));
#60930=CARTESIAN_POINT('Ctrl Pts',(-2.57914737379974,-1.64365111748691,
32.4111142244105));
#60931=CARTESIAN_POINT('Ctrl Pts',(-2.93688142666368,-0.817870137505501,
32.36664517075));
#60932=CARTESIAN_POINT('Ctrl Pts',(-2.94410448200555,0.00238870800367233,
32.3221761170895));
#60933=CARTESIAN_POINT('Ctrl Pts',(-2.94627736789538,-0.00111514688795235,
32.1778238829105));
#60934=CARTESIAN_POINT('Ctrl Pts',(-2.94658005652525,-0.0633981686056019,
32.1812069935992));
#60935=CARTESIAN_POINT('Ctrl Pts',(-2.94477567931027,-0.125663328770047,
32.1845901042879));
#60936=CARTESIAN_POINT('Ctrl Pts',(-2.94080844994758,-0.187790376294515,
32.1879732149766));
#60937=CARTESIAN_POINT('Ctrl Pts',(-2.87882903948476,-1.15839162652036,
32.2408270297795));
#60938=CARTESIAN_POINT('Ctrl Pts',(-2.28895518053886,-2.09528326974124,
32.2936808445824));
#60939=CARTESIAN_POINT('Ctrl Pts',(-1.4405017823663,-2.57071472157287,32.3465346593853));
#60940=CARTESIAN_POINT('Ctrl Pts',(-0.592048384193733,-3.04614617340449,
32.3993884741882));
#60941=CARTESIAN_POINT('Ctrl Pts',(0.514984553205557,-3.06011743384676,
32.4522422889911));
#60942=CARTESIAN_POINT('Ctrl Pts',(1.3751661303974,-2.60624973448819,32.5050961037941));
#60943=CARTESIAN_POINT('Ctrl Pts',(2.23534770758924,-2.15238203512962,32.557949918597));
#60944=CARTESIAN_POINT('Ctrl Pts',(2.84867792457375,-1.23067537597021,32.6108037333999));
#60945=CARTESIAN_POINT('Ctrl Pts',(2.93513255375312,-0.261947431005922,
32.6636575482028));
#60946=CARTESIAN_POINT('Ctrl Pts',(3.0215871829325,0.706780513958397,32.7165113630057));
#60947=CARTESIAN_POINT('Ctrl Pts',(2.58116622430677,1.72252974472756,32.7693651778086));
#60948=CARTESIAN_POINT('Ctrl Pts',(1.81494983884269,2.32154617597773,32.8222189926116));
#60949=CARTESIAN_POINT('Ctrl Pts',(1.04873345337863,2.92056260722789,32.8750728074145));
#60950=CARTESIAN_POINT('Ctrl Pts',(-0.0432783589237744,3.10284623895901,
32.9279266222174));
#60951=CARTESIAN_POINT('Ctrl Pts',(-0.962512796986673,2.78517300725625,
32.9807804370203));
#60952=CARTESIAN_POINT('Ctrl Pts',(-1.88174723504962,2.46749977555347,33.0336342518232));
#60953=CARTESIAN_POINT('Ctrl Pts',(-2.62820429887308,1.64986968041674,33.0864880666261));
#60954=CARTESIAN_POINT('Ctrl Pts',(-2.86107889367498,0.705582829212486,
33.1393418814291));
#60955=CARTESIAN_POINT('Ctrl Pts',(-2.91759629319511,0.476409538426898,
33.1521692152562));
#60956=CARTESIAN_POINT('Ctrl Pts',(-2.94386334938736,0.239776081870586,
33.1649965490833));
#60957=CARTESIAN_POINT('Ctrl Pts',(-2.94171210674826,0.00267199037597989,
33.1778238829104));
#60958=CARTESIAN_POINT('Origin',(0.,0.,0.));
#60959=CARTESIAN_POINT('',(-2.94086681343003,-0.0026768557490095,34.3221761170896));
#60960=CARTESIAN_POINT('',(-2.93739638408601,-0.000779703272701529,34.1778238829104));
#60961=CARTESIAN_POINT('',(-2.942,-3.60291088309151E-16,0.));
#60962=CARTESIAN_POINT('Ctrl Pts',(-2.94086681343003,-0.0026768557490095,
34.3221761170896));
#60963=CARTESIAN_POINT('Ctrl Pts',(-2.93457120391373,0.712243215688969,
34.2835270315264));
#60964=CARTESIAN_POINT('Ctrl Pts',(-2.67230139772352,1.43129977251953,34.2448779459633));
#60965=CARTESIAN_POINT('Ctrl Pts',(-2.19884786976029,1.96192715921988,34.2062288604002));
#60966=CARTESIAN_POINT('Ctrl Pts',(-1.54898394900133,2.69026811269557,34.153178994269));
#60967=CARTESIAN_POINT('Ctrl Pts',(-0.501241431081312,3.06360095642591,
34.1001291281379));
#60968=CARTESIAN_POINT('Ctrl Pts',(0.462764471317297,2.91031599255435,34.0470792620067));
#60969=CARTESIAN_POINT('Ctrl Pts',(1.42677037371591,2.75703102868279,33.9940293958755));
#60970=CARTESIAN_POINT('Ctrl Pts',(2.30703966059311,2.07712825720934,33.9409795297443));
#60971=CARTESIAN_POINT('Ctrl Pts',(2.69893944497945,1.18313820189125,33.8879296636131));
#60972=CARTESIAN_POINT('Ctrl Pts',(3.09083922936579,0.289148146573163,33.8348797974819));
#60973=CARTESIAN_POINT('Ctrl Pts',(2.99436951126127,-0.818929192589566,
33.7818299313507));
#60974=CARTESIAN_POINT('Ctrl Pts',(2.45387447161704,-1.63174452963146,33.7287800652195));
#60975=CARTESIAN_POINT('Ctrl Pts',(1.91337943197281,-2.44455986667332,33.6757301990883));
#60976=CARTESIAN_POINT('Ctrl Pts',(0.928859070788909,-2.96211320159438,
33.6226803329571));
#60977=CARTESIAN_POINT('Ctrl Pts',(-0.0471326924005423,-2.94650108463293,
33.569630466826));
#60978=CARTESIAN_POINT('Ctrl Pts',(-1.02312445559002,-2.93088896767149,
33.5165806006948));
#60979=CARTESIAN_POINT('Ctrl Pts',(-1.99058762078505,-2.38211139882752,
33.4635307345636));
#60980=CARTESIAN_POINT('Ctrl Pts',(-2.50480894011653,-1.55242465387196,
33.4104808684324));
#60981=CARTESIAN_POINT('Ctrl Pts',(-2.79012656703532,-1.09206985282163,
33.3810459513181));
#60982=CARTESIAN_POINT('Ctrl Pts',(-2.93590794326828,-0.545233599152603,
33.3516110342038));
#60983=CARTESIAN_POINT('Ctrl Pts',(-2.93736495050316,0.000879932274083783,
33.3221761170896));
#60984=CARTESIAN_POINT('Ctrl Pts',(-2.94171210674826,0.00267199037597989,
33.1778238829104));
#60985=CARTESIAN_POINT('Ctrl Pts',(-2.93499935772893,-0.737188882927786,
33.2178503638862));
#60986=CARTESIAN_POINT('Ctrl Pts',(-2.65157963682834,-1.4816322954402,33.257876844862));
#60987=CARTESIAN_POINT('Ctrl Pts',(-2.14711625751622,-2.01829416622589,
33.2979033258378));
#60988=CARTESIAN_POINT('Ctrl Pts',(-1.48098690077514,-2.72694070318839,
33.3507571406407));
#60989=CARTESIAN_POINT('Ctrl Pts',(-0.429436061512542,-3.07329016984171,
33.4036109554436));
#60990=CARTESIAN_POINT('Ctrl Pts',(0.527436465104114,-2.89921202053081,
33.4564647702466));
#60991=CARTESIAN_POINT('Ctrl Pts',(1.4843089917208,-2.72513387121991,33.5093185850495));
#60992=CARTESIAN_POINT('Ctrl Pts',(2.34650320569153,-2.03062810594474,33.5621723998524));
#60993=CARTESIAN_POINT('Ctrl Pts',(2.72037264688675,-1.13278074965211,33.6150262146553));
#60994=CARTESIAN_POINT('Ctrl Pts',(3.09424208808199,-0.234933393359419,
33.6678800294583));
#60995=CARTESIAN_POINT('Ctrl Pts',(2.97978675650164,0.866255553950765,33.7207338442612));
#60996=CARTESIAN_POINT('Ctrl Pts',(2.42926278584456,1.66802334576665,33.7735876590641));
#60997=CARTESIAN_POINT('Ctrl Pts',(1.8787388151875,2.46979113758252,33.826441473867));
#60998=CARTESIAN_POINT('Ctrl Pts',(0.892146205453725,2.9721377739041,33.8792952886699));
#60999=CARTESIAN_POINT('Ctrl Pts',(-0.0800728087435554,2.94571008587262,
33.9321491034728));
#61000=CARTESIAN_POINT('Ctrl Pts',(-1.05229182294078,2.91928239784113,33.9850029182758));
#61001=CARTESIAN_POINT('Ctrl Pts',(-2.01013724160151,2.36408038545666,34.0378567330786));
#61002=CARTESIAN_POINT('Ctrl Pts',(-2.51629175002141,1.53358905626203,34.0907105478816));
#61003=CARTESIAN_POINT('Ctrl Pts',(-2.79437200738008,1.07731880930218,34.1197483262245));
#61004=CARTESIAN_POINT('Ctrl Pts',(-2.93611472733982,0.537955751140718,
34.1487861045675));
#61005=CARTESIAN_POINT('Ctrl Pts',(-2.93739638408601,-0.000779703272701529,
34.1778238829104));
#61006=CARTESIAN_POINT('Origin',(0.,0.,0.));
#61007=CARTESIAN_POINT('',(-2.94685781061061,0.00021972601725095,35.3221761170896));
#61008=CARTESIAN_POINT('',(-2.94455392252949,-0.00218017528262053,35.1778238829104));
#61009=CARTESIAN_POINT('',(-2.942,-3.60291088309151E-16,0.));
#61010=CARTESIAN_POINT('Ctrl Pts',(-2.94685781061061,0.00021972601725095,
35.3221761170896));
#61011=CARTESIAN_POINT('Ctrl Pts',(-2.9468702780931,0.0118736808740626,
35.3215427611115));
#61012=CARTESIAN_POINT('Ctrl Pts',(-2.94680715351256,0.0235274968392718,
35.3209094051333));
#61013=CARTESIAN_POINT('Ctrl Pts',(-2.94666802890093,0.0351804054366583,
35.3202760491553));
#61014=CARTESIAN_POINT('Ctrl Pts',(-2.93501495815129,1.01122746665534,35.2672261830241));
#61015=CARTESIAN_POINT('Ctrl Pts',(-2.39016622670584,1.9809086806671,35.2141763168929));
#61016=CARTESIAN_POINT('Ctrl Pts',(-1.56257214446959,2.49849122988862,35.1611264507617));
#61017=CARTESIAN_POINT('Ctrl Pts',(-0.734978062233343,3.01607377911014,
35.1080765846305));
#61018=CARTESIAN_POINT('Ctrl Pts',(0.375361370793731,3.08155766354144,35.0550267184993));
#61019=CARTESIAN_POINT('Ctrl Pts',(1.25805705355367,2.66484194317754,35.0019768523681));
#61020=CARTESIAN_POINT('Ctrl Pts',(2.14075273631365,2.24812622281361,34.9489269862369));
#61021=CARTESIAN_POINT('Ctrl Pts',(2.79580466880647,1.3492108976545,34.8958771201057));
#61022=CARTESIAN_POINT('Ctrl Pts',(2.92210549825361,0.381299868446144,34.8428272539745));
#61023=CARTESIAN_POINT('Ctrl Pts',(3.04840632770075,-0.586611160762127,
34.7897773878434));
#61024=CARTESIAN_POINT('Ctrl Pts',(2.64595605410225,-1.62351789401957,34.7367275217122));
#61025=CARTESIAN_POINT('Ctrl Pts',(1.89974876798349,-2.25278599759881,34.683677655581));
#61026=CARTESIAN_POINT('Ctrl Pts',(1.15354148186467,-2.8820541011781,34.6306277894498));
#61027=CARTESIAN_POINT('Ctrl Pts',(0.0635771832255068,-3.10368357507913,
34.5775779233186));
#61028=CARTESIAN_POINT('Ctrl Pts',(-0.869120853144318,-2.81579812398257,
34.5245280571874));
#61029=CARTESIAN_POINT('Ctrl Pts',(-1.80181888951409,-2.52791267288603,
34.4714781910562));
#61030=CARTESIAN_POINT('Ctrl Pts',(-2.57725066361456,-1.73051229679197,
34.418428324925));
#61031=CARTESIAN_POINT('Ctrl Pts',(-2.83897388886586,-0.790137577134433,
34.3653784587938));
#61032=CARTESIAN_POINT('Ctrl Pts',(-2.91002060417886,-0.534865868133838,
34.3509776782257));
#61033=CARTESIAN_POINT('Ctrl Pts',(-2.94321257892139,-0.269058502882331,
34.3365768976577));
#61034=CARTESIAN_POINT('Ctrl Pts',(-2.94086681343003,-0.0026768557490095,
34.3221761170896));
#61035=CARTESIAN_POINT('Ctrl Pts',(-2.93739638408601,-0.000779703272701529,
34.1778238829104));
#61036=CARTESIAN_POINT('Ctrl Pts',(-2.93844756587532,-0.442636620597825,
34.2016399193704));
#61037=CARTESIAN_POINT('Ctrl Pts',(-2.84501259774457,-0.88407135785061,
34.2254559558304));
#61038=CARTESIAN_POINT('Ctrl Pts',(-2.65481645025957,-1.27889373293584,
34.2492719922903));
#61039=CARTESIAN_POINT('Ctrl Pts',(-2.23272304389876,-2.15510454693423,
34.3021258070933));
#61040=CARTESIAN_POINT('Ctrl Pts',(-1.33407263299811,-2.80174552892622,
34.3549796218961));
#61041=CARTESIAN_POINT('Ctrl Pts',(-0.369156248756929,-2.92358396984159,
34.4078334366991));
#61042=CARTESIAN_POINT('Ctrl Pts',(0.595760135484311,-3.04542241075698,
34.460687251502));
#61043=CARTESIAN_POINT('Ctrl Pts',(1.6269424930661,-2.64245831059566,34.5135410663049));
#61044=CARTESIAN_POINT('Ctrl Pts',(2.25359053533617,-1.89867039365946,34.5663948811079));
#61045=CARTESIAN_POINT('Ctrl Pts',(2.88023857760625,-1.15488247672325,34.6192486959108));
#61046=CARTESIAN_POINT('Ctrl Pts',(3.10235230456463,-0.0702707430121562,
34.6721025107136));
#61047=CARTESIAN_POINT('Ctrl Pts',(2.81852268221,0.859970612622888,34.7249563255166));
#61048=CARTESIAN_POINT('Ctrl Pts',(2.53469305985538,1.79021196825791,34.7778101403195));
#61049=CARTESIAN_POINT('Ctrl Pts',(1.7449200881878,2.56608294581688,34.8306639551225));
#61050=CARTESIAN_POINT('Ctrl Pts',(0.809785327091873,2.83334912934047,34.8835177699254));
#61051=CARTESIAN_POINT('Ctrl Pts',(-0.125349434004051,3.10061531286405,
34.9363715847283));
#61052=CARTESIAN_POINT('Ctrl Pts',(-1.20584598452831,2.85927670235226,34.9892253995312));
#61053=CARTESIAN_POINT('Ctrl Pts',(-1.93838897230708,2.21951971308571,35.0420792143341));
#61054=CARTESIAN_POINT('Ctrl Pts',(-2.56552002213284,1.67182288299433,35.0873274371928));
#61055=CARTESIAN_POINT('Ctrl Pts',(-2.93763258542781,0.832121421151534,
35.1325756600516));
#61056=CARTESIAN_POINT('Ctrl Pts',(-2.94455392252949,-0.00218017528262053,
35.1778238829104));
#61057=CARTESIAN_POINT('Origin',(0.,0.,0.));
#61058=CARTESIAN_POINT('',(-2.9402011249149,0.00257356892240088,36.3221761170896));
#61059=CARTESIAN_POINT('',(-2.94404018584088,0.00235134841817481,36.1778238829104));
#61060=CARTESIAN_POINT('',(-2.942,-3.60291088309151E-16,0.));
#61061=CARTESIAN_POINT('Ctrl Pts',(-2.9402011249149,0.00257356892240088,
36.3221761170896));
#61062=CARTESIAN_POINT('Ctrl Pts',(-2.94261307060905,0.292552802751825,
36.3065086245653));
#61063=CARTESIAN_POINT('Ctrl Pts',(-2.90320504514716,0.581890802336307,
36.290841132041));
#61064=CARTESIAN_POINT('Ctrl Pts',(-2.81930038436528,0.857691968114813,
36.2751736395167));
#61065=CARTESIAN_POINT('Ctrl Pts',(-2.53520061438846,1.79155007595818,36.2221237733855));
#61066=CARTESIAN_POINT('Ctrl Pts',(-1.74095216738676,2.57020998044168,36.1690739072543));
#61067=CARTESIAN_POINT('Ctrl Pts',(-0.801646808582714,2.83574549969904,
36.1160240411231));
#61068=CARTESIAN_POINT('Ctrl Pts',(0.13765855022133,3.1012810189564,36.0629741749919));
#61069=CARTESIAN_POINT('Ctrl Pts',(1.22202082082772,2.85369215298764,36.0099243088607));
#61070=CARTESIAN_POINT('Ctrl Pts',(1.95299182479538,2.20678794802801,35.9568744427296));
#61071=CARTESIAN_POINT('Ctrl Pts',(2.68396282876302,1.55988374306839,35.9038245765984));
#61072=CARTESIAN_POINT('Ctrl Pts',(3.06154256609195,0.513664199117923,35.8507747104672));
#61073=CARTESIAN_POINT('Ctrl Pts',(2.91216916370067,-0.450955541884665,
35.797724844336));
#61074=CARTESIAN_POINT('Ctrl Pts',(2.76279576130938,-1.41557528288728,35.7446749782048));
#61075=CARTESIAN_POINT('Ctrl Pts',(2.0864692191978,-2.29859522094207,35.6916251120736));
#61076=CARTESIAN_POINT('Ctrl Pts',(1.19407618200127,-2.69411807557552,35.6385752459424));
#61077=CARTESIAN_POINT('Ctrl Pts',(0.301683144804796,-3.08964093020895,
35.5855253798112));
#61078=CARTESIAN_POINT('Ctrl Pts',(-0.80677638747653,-2.99766670142119,
35.53247551368));
#61079=CARTESIAN_POINT('Ctrl Pts',(-1.62177744859037,-2.46047313281454,
35.4794256475489));
#61080=CARTESIAN_POINT('Ctrl Pts',(-2.4270483099534,-1.92969305368267,35.4270091373957));
#61081=CARTESIAN_POINT('Ctrl Pts',(-2.94582600236185,-0.964261014983614,
35.3745926272426));
#61082=CARTESIAN_POINT('Ctrl Pts',(-2.94685781061061,0.00021972601725095,
35.3221761170896));
#61083=CARTESIAN_POINT('Ctrl Pts',(-2.94455392252949,-0.00218017528262053,
35.1778238829104));
#61084=CARTESIAN_POINT('Ctrl Pts',(-2.94571730226857,-0.142414577871742,
35.1854294748546));
#61085=CARTESIAN_POINT('Ctrl Pts',(-2.93656297186098,-0.282496418618953,
35.1930350667987));
#61086=CARTESIAN_POINT('Ctrl Pts',(-2.91656773022714,-0.421013348566901,
35.2006406587428));
#61087=CARTESIAN_POINT('Ctrl Pts',(-2.77761407533517,-1.38361405293164,
35.2534944735458));
#61088=CARTESIAN_POINT('Ctrl Pts',(-2.11511734051801,-2.27064009363985,
35.3063482883487));
#61089=CARTESIAN_POINT('Ctrl Pts',(-1.23154939376283,-2.67710770336558,
35.3592021031516));
#61090=CARTESIAN_POINT('Ctrl Pts',(-0.347981447007576,-3.08357531309134,
35.4120559179545));
#61091=CARTESIAN_POINT('Ctrl Pts',(0.756657711685735,-3.00948449183453,
35.4649097327574));
#61092=CARTESIAN_POINT('Ctrl Pts',(1.57803009492198,-2.4886624086851,35.5177635475603));
#61093=CARTESIAN_POINT('Ctrl Pts',(2.39940247815818,-1.9678403255357,35.5706173623633));
#61094=CARTESIAN_POINT('Ctrl Pts',(2.93750808593735,-1.00028698049375,35.6234711771662));
#61095=CARTESIAN_POINT('Ctrl Pts',(2.94666750624564,-0.0277519738104105,
35.6763249919691));
#61096=CARTESIAN_POINT('Ctrl Pts',(2.95582692655392,0.944783032872932,35.729178806772));
#61097=CARTESIAN_POINT('Ctrl Pts',(2.43604015939132,1.92229970119767,35.7820326215749));
#61098=CARTESIAN_POINT('Ctrl Pts',(1.62462290152057,2.4584995408919,35.8348864363779));
#61099=CARTESIAN_POINT('Ctrl Pts',(0.813205643649837,2.99469938058611,35.8877402511808));
#61100=CARTESIAN_POINT('Ctrl Pts',(-0.289842104929023,3.08958239164985,
35.9405940659837));
#61101=CARTESIAN_POINT('Ctrl Pts',(-1.18090893615386,2.69982844831109,35.9934478807866));
#61102=CARTESIAN_POINT('Ctrl Pts',(-2.07197576737872,2.31007450497232,36.0463016955895));
#61103=CARTESIAN_POINT('Ctrl Pts',(-2.75106168124954,1.43568360723102,36.0991555103924));
#61104=CARTESIAN_POINT('Ctrl Pts',(-2.90812079627098,0.475870777375731,
36.1520093251953));
#61105=CARTESIAN_POINT('Ctrl Pts',(-2.93369076761249,0.319608681099053,
36.160614177767));
#61106=CARTESIAN_POINT('Ctrl Pts',(-2.945424215324,0.161082443240333,36.1692190303387));
#61107=CARTESIAN_POINT('Ctrl Pts',(-2.94404018584088,0.00235134841817481,
36.1778238829104));
#61108=CARTESIAN_POINT('Origin',(0.,0.,0.));
#61109=CARTESIAN_POINT('',(-2.93761702632781,-0.00123893643864781,37.3221761170896));
#61110=CARTESIAN_POINT('',(-2.93727713413294,0.00048555243809314,37.1778238829104));
#61111=CARTESIAN_POINT('',(-2.942,-3.60291088309151E-16,0.));
#61112=CARTESIAN_POINT('Ctrl Pts',(-2.93761702632781,-0.00123893643864781,
37.3221761170896));
#61113=CARTESIAN_POINT('Ctrl Pts',(-2.93546619409942,0.568253609984608,
37.2914744880191));
#61114=CARTESIAN_POINT('Ctrl Pts',(-2.77600657644893,1.13885954810213,37.2607728589486));
#61115=CARTESIAN_POINT('Ctrl Pts',(-2.4670317237215,1.61178336717249,37.2300712298781));
#61116=CARTESIAN_POINT('Ctrl Pts',(-1.93314882983744,2.42895646356918,37.177021363747));
#61117=CARTESIAN_POINT('Ctrl Pts',(-0.952858734605018,2.95448034199031,
37.1239714976158));
#61118=CARTESIAN_POINT('Ctrl Pts',(0.0232277563561131,2.94678665544818,
37.0709216314846));
#61119=CARTESIAN_POINT('Ctrl Pts',(0.999314247317216,2.93909296890604,37.0178717653534));
#61120=CARTESIAN_POINT('Ctrl Pts',(1.97119713400707,2.39818171740062,36.9648218992222));
#61121=CARTESIAN_POINT('Ctrl Pts',(2.49213229674678,1.57269383816965,36.911772033091));
#61122=CARTESIAN_POINT('Ctrl Pts',(3.01306745948649,0.747205958938681,36.8587221669598));
#61123=CARTESIAN_POINT('Ctrl Pts',(3.08305489827613,-0.362858548017857,
36.8056723008286));
#61124=CARTESIAN_POINT('Ctrl Pts',(2.6699231391851,-1.24723725369426,36.7526224346974));
#61125=CARTESIAN_POINT('Ctrl Pts',(2.25679138009406,-2.13161595937069,36.6995725685662));
#61126=CARTESIAN_POINT('Ctrl Pts',(1.36054042312233,-2.79030886376693,36.646522702435));
#61127=CARTESIAN_POINT('Ctrl Pts',(0.393149643570355,-2.92053481496036,
36.5934728363039));
#61128=CARTESIAN_POINT('Ctrl Pts',(-0.574241135981621,-3.05076076615379,
36.5404229701727));
#61129=CARTESIAN_POINT('Ctrl Pts',(-1.61277173811382,-2.65251976414439,
36.4873731040414));
#61130=CARTESIAN_POINT('Ctrl Pts',(-2.24506149270394,-1.90887110753806,
36.4343232379103));
#61131=CARTESIAN_POINT('Ctrl Pts',(-2.69061382973445,-1.38484807146129,
36.3969408643033));
#61132=CARTESIAN_POINT('Ctrl Pts',(-2.93444626306201,-0.689312005010758,
36.3595584906965));
#61133=CARTESIAN_POINT('Ctrl Pts',(-2.9402011249149,0.00257356892240088,
36.3221761170896));
#61134=CARTESIAN_POINT('Ctrl Pts',(-2.94404018584088,0.00235134841817481,
36.1778238829104));
#61135=CARTESIAN_POINT('Ctrl Pts',(-2.93692305422064,-0.813895782045558,
36.2220728451417));
#61136=CARTESIAN_POINT('Ctrl Pts',(-2.58293361510877,-1.63556005229609,
36.2663218073729));
#61137=CARTESIAN_POINT('Ctrl Pts',(-1.97984868768892,-2.18261740561111,
36.3105707696041));
#61138=CARTESIAN_POINT('Ctrl Pts',(-1.25948514791341,-2.83605799677329,
36.363424584407));
#61139=CARTESIAN_POINT('Ctrl Pts',(-0.183725752190359,-3.09770441712838,
36.4162783992099));
#61140=CARTESIAN_POINT('Ctrl Pts',(0.756276955239686,-2.84809844254033,
36.4691322140128));
#61141=CARTESIAN_POINT('Ctrl Pts',(1.69627966266973,-2.59849246795229,36.5219860288158));
#61142=CARTESIAN_POINT('Ctrl Pts',(2.50052568180677,-1.83763409842111,36.5748398436187));
#61143=CARTESIAN_POINT('Ctrl Pts',(2.80182559496105,-0.912903545632631,
36.6276936584216));
#61144=CARTESIAN_POINT('Ctrl Pts',(3.10312550811534,0.011827007155906,36.6805474732246));
#61145=CARTESIAN_POINT('Ctrl Pts',(2.90147931528681,1.10042974320177,36.7334012880274));
#61146=CARTESIAN_POINT('Ctrl Pts',(2.28895130441658,1.85588833190484,36.7862551028303));
#61147=CARTESIAN_POINT('Ctrl Pts',(1.67642329354638,2.61134692060786,36.8391089176332));
#61148=CARTESIAN_POINT('Ctrl Pts',(0.653013464634534,3.03366136196813,36.8919627324362));
#61149=CARTESIAN_POINT('Ctrl Pts',(-0.314026516870114,2.93001825100472,
36.9448165472391));
#61150=CARTESIAN_POINT('Ctrl Pts',(-1.28106649837473,2.82637514004131,36.997670362042));
#61151=CARTESIAN_POINT('Ctrl Pts',(-2.19173663247216,2.19677447675427,37.0505241768449));
#61152=CARTESIAN_POINT('Ctrl Pts',(-2.63025817789325,1.32866901980392,37.1033779916479));
#61153=CARTESIAN_POINT('Ctrl Pts',(-2.83614761973355,0.921086428124407,
37.1281932887354));
#61154=CARTESIAN_POINT('Ctrl Pts',(-2.93795761448107,0.460928338712189,
37.1530085858229));
#61155=CARTESIAN_POINT('Ctrl Pts',(-2.93727713413294,0.00048555243809314,
37.1778238829104));
#61156=CARTESIAN_POINT('Origin',(0.,0.,0.));
#61157=CARTESIAN_POINT('',(-2.94471098031246,-0.00212455505907094,38.3221761170895));
#61158=CARTESIAN_POINT('',(-2.9422704459833,-0.00265502083472174,38.1778238829104));
#61159=CARTESIAN_POINT('',(-2.942,-3.60291088309151E-16,0.));
#61160=CARTESIAN_POINT('Ctrl Pts',(-2.94471098031246,-0.00212455505907094,
38.3221761170895));
#61161=CARTESIAN_POINT('Ctrl Pts',(-2.93776546270216,0.841018236135255,
38.2764403514729));
#61162=CARTESIAN_POINT('Ctrl Pts',(-2.55687059036142,1.68958573147536,38.2307045858562));
#61163=CARTESIAN_POINT('Ctrl Pts',(-1.91798197858352,2.23728479977708,38.1849688202396));
#61164=CARTESIAN_POINT('Ctrl Pts',(-1.17692178486893,2.87257234469591,38.1319189541084));
#61165=CARTESIAN_POINT('Ctrl Pts',(-0.0887526147754901,3.10306661066995,
38.0788690879772));
#61166=CARTESIAN_POINT('Ctrl Pts',(0.846259422451992,2.82276424963368,38.025819221846));
#61167=CARTESIAN_POINT('Ctrl Pts',(1.78127145967947,2.54246188859742,37.9727693557148));
#61168=CARTESIAN_POINT('Ctrl Pts',(2.56312636404104,1.75136290055085,37.9197194895836));
#61169=CARTESIAN_POINT('Ctrl Pts',(2.83246497394273,0.813138660625782,37.8666696234524));
#61170=CARTESIAN_POINT('Ctrl Pts',(3.10180358384444,-0.125085579299313,
37.8136197573212));
#61171=CARTESIAN_POINT('Ctrl Pts',(2.8586258992863,-1.21043507110287,37.7605698911901));
#61172=CARTESIAN_POINT('Ctrl Pts',(2.21469458797494,-1.94402216064632,37.7075200250589));
#61173=CARTESIAN_POINT('Ctrl Pts',(1.57076327666364,-2.67760925018972,37.6544701589277));
#61174=CARTESIAN_POINT('Ctrl Pts',(0.526078338599165,-3.05943393747302,
37.6014202927965));
#61175=CARTESIAN_POINT('Ctrl Pts',(-0.439140697634978,-2.9139755699834,
37.5483704266653));
#61176=CARTESIAN_POINT('Ctrl Pts',(-1.40435973386915,-2.76851720249378,
37.4953205605341));
#61177=CARTESIAN_POINT('Ctrl Pts',(-2.29011286827302,-2.09577578023121,
37.4422706944029));
#61178=CARTESIAN_POINT('Ctrl Pts',(-2.68925158920712,-1.20499391191384,
37.3892208282717));
#61179=CARTESIAN_POINT('Ctrl Pts',(-2.85739615593405,-0.829735578305169,
37.366872591211));
#61180=CARTESIAN_POINT('Ctrl Pts',(-2.93918265362425,-0.415782229974393,
37.3445243541503));
#61181=CARTESIAN_POINT('Ctrl Pts',(-2.93761702632781,-0.00123893643864781,
37.3221761170896));
#61182=CARTESIAN_POINT('Ctrl Pts',(-2.93727713413294,0.00048555243809314,
37.1778238829104));
#61183=CARTESIAN_POINT('Ctrl Pts',(-2.93650826724294,-0.519763436495626,
37.2058624006258));
#61184=CARTESIAN_POINT('Ctrl Pts',(-2.80489514815729,-1.04037588308685,
37.2339009183412));
#61185=CARTESIAN_POINT('Ctrl Pts',(-2.54472982091734,-1.48592388881374,
37.2619394360566));
#61186=CARTESIAN_POINT('Ctrl Pts',(-2.05430696177559,-2.32580108986735,
37.3147932508595));
#61187=CARTESIAN_POINT('Ctrl Pts',(-1.10708828674735,-2.89894524136082,
37.3676470656625));
#61188=CARTESIAN_POINT('Ctrl Pts',(-0.13553953614123,-2.94367946988174,
37.4205008804654));
#61189=CARTESIAN_POINT('Ctrl Pts',(0.836009214464838,-2.98841369840265,
37.4733546952683));
#61190=CARTESIAN_POINT('Ctrl Pts',(1.83188804064887,-2.50473800395102,37.5262085100712));
#61191=CARTESIAN_POINT('Ctrl Pts',(2.39741535950944,-1.71348134882026,37.5790623248741));
#61192=CARTESIAN_POINT('Ctrl Pts',(2.96294267837005,-0.922224693689448,
37.631916139677));
#61193=CARTESIAN_POINT('Ctrl Pts',(3.09811848990726,0.176612922120487,37.6847699544799));
#61194=CARTESIAN_POINT('Ctrl Pts',(2.74122568156945,1.08134279025845,37.7376237692829));
#61195=CARTESIAN_POINT('Ctrl Pts',(2.38433287323164,1.9860726583964,37.7904775840858));
#61196=CARTESIAN_POINT('Ctrl Pts',(1.53537144501881,2.6966947788623,37.8433313988887));
#61197=CARTESIAN_POINT('Ctrl Pts',(0.581947704629053,2.88876402096991,37.8961852136916));
#61198=CARTESIAN_POINT('Ctrl Pts',(-0.371476035760709,3.08083326307753,
37.9490390284945));
#61199=CARTESIAN_POINT('Ctrl Pts',(-1.4293620883274,2.75434962682684,38.0018928432975));
#61200=CARTESIAN_POINT('Ctrl Pts',(-2.10872100721019,2.05837548530462,38.0547466581004));
#61201=CARTESIAN_POINT('Ctrl Pts',(-2.636047247822,1.5181523169454,38.0957723997037));
#61202=CARTESIAN_POINT('Ctrl Pts',(-2.93530923507167,0.755309503360123,
38.1367981413071));
#61203=CARTESIAN_POINT('Ctrl Pts',(-2.9422704459833,-0.00265502083472174,
38.1778238829104));
#61204=CARTESIAN_POINT('Origin',(0.,0.,-1.84858989190508));
#61205=CARTESIAN_POINT('',(-2.37393550902653,-0.00171275100589707,38.6514101080949));
#61206=CARTESIAN_POINT('',(-2.37498223974761,0.00116593724452961,38.848589891905));
#61207=CARTESIAN_POINT('',(-2.37175,1.07555357745099E-12,-1.84858989190508));
#61208=CARTESIAN_POINT('',(-2.34668236863844,0.343918483396126,39.62825));
#61209=CARTESIAN_POINT('Ctrl Pts',(-2.37393550902653,-0.00171275100589735,
38.6514101080949));
#61210=CARTESIAN_POINT('Ctrl Pts',(-2.37483094766103,-0.110413451510199,
38.6587242086095));
#61211=CARTESIAN_POINT('Ctrl Pts',(-2.31859051736089,-1.00660760499401,
38.7190881752552));
#61212=CARTESIAN_POINT('Ctrl Pts',(-1.17732869269255,-2.54685292441361,
38.8325020080321));
#61213=CARTESIAN_POINT('Ctrl Pts',(1.50731350036759,-2.36620050995552,38.9916516064257));
#61214=CARTESIAN_POINT('Ctrl Pts',(2.80472045702593,-0.0113602674063951,
39.1508012048193));
#61215=CARTESIAN_POINT('Ctrl Pts',(1.52653968516444,2.35613848946071,39.3099508032129));
#61216=CARTESIAN_POINT('Ctrl Pts',(-1.16086793848797,2.55318010173628,39.4691004016064));
#61217=CARTESIAN_POINT('Ctrl Pts',(-2.23204672396583,1.1261196710573,39.5752001338688));
#61218=CARTESIAN_POINT('Ctrl Pts',(-2.34668236863851,0.343918483395665,
39.62825));
#61219=CARTESIAN_POINT('',(-0.439445221992216,2.33068358199225,39.6282499999999));
#61220=CARTESIAN_POINT('Origin',(0.,0.,39.62825));
#61221=CARTESIAN_POINT('Ctrl Pts',(-2.37498223974761,0.00116593724452945,
38.848589891905));
#61222=CARTESIAN_POINT('Ctrl Pts',(-2.37064629607478,-0.718482336400258,
38.8970613353916));
#61223=CARTESIAN_POINT('Ctrl Pts',(-1.63815568977571,-2.23050835538683,
38.9983865936812));
#61224=CARTESIAN_POINT('Ctrl Pts',(0.931334562612731,-2.64189543289012,
39.1525656667738));
#61225=CARTESIAN_POINT('Ctrl Pts',(2.72641926444476,-0.654580598253606,
39.3111271111825));
#61226=CARTESIAN_POINT('Ctrl Pts',(2.02601511878175,1.93446865908499,39.4696885555913));
#61227=CARTESIAN_POINT('Ctrl Pts',(0.334552217316969,2.47661908313362,39.5753961851971));
#61228=CARTESIAN_POINT('Ctrl Pts',(-0.439445221993938,2.33068358199192,
39.62825));
#61229=CARTESIAN_POINT('Origin',(0.,0.,-1.84858989190508));
#61230=CARTESIAN_POINT('',(-2.36821658130285,-0.000998792486933048,37.6514101080949));
#61231=CARTESIAN_POINT('',(-2.37196802524163,-0.00214039621392242,37.848589891905));
#61232=CARTESIAN_POINT('',(-2.37175,1.07555357745099E-12,-1.84858989190508));
#61233=CARTESIAN_POINT('Ctrl Pts',(-2.36821658130285,-0.000998792486933131,
37.6514101080949));
#61234=CARTESIAN_POINT('Ctrl Pts',(-2.36947874192167,-0.335190857899489,
37.6737583451556));
#61235=CARTESIAN_POINT('Ctrl Pts',(-2.14703253604354,-1.46107782393166,
37.7491564483476));
#61236=CARTESIAN_POINT('Ctrl Pts',(-0.41808470505867,-2.7742369623609,37.8776044176707));
#61237=CARTESIAN_POINT('Ctrl Pts',(2.10849398479986,-1.85079097113315,38.0367540160642));
#61238=CARTESIAN_POINT('Ctrl Pts',(2.69662111602106,0.774135259850986,38.1959036144578));
#61239=CARTESIAN_POINT('Ctrl Pts',(0.805698917428903,2.68741434710406,38.3550532128514));
#61240=CARTESIAN_POINT('Ctrl Pts',(-1.70509856072161,2.15558121155782,38.5068887107304));
#61241=CARTESIAN_POINT('Ctrl Pts',(-2.36833624614658,0.678003059672109,
38.6056743424783));
#61242=CARTESIAN_POINT('Ctrl Pts',(-2.37393550902653,-0.00171275100589735,
38.6514101080949));
#61243=CARTESIAN_POINT('Ctrl Pts',(-2.37196802524163,-0.00214039621392275,
37.848589891905));
#61244=CARTESIAN_POINT('Ctrl Pts',(-2.37358598828088,-0.178310691973696,
37.8604179651045));
#61245=CARTESIAN_POINT('Ctrl Pts',(-2.27532136204516,-1.13991136271545,
37.925099853107));
#61246=CARTESIAN_POINT('Ctrl Pts',(-0.964945338256294,-2.63066900551404,
38.0426355559125));
#61247=CARTESIAN_POINT('Ctrl Pts',(1.68390204706478,-2.23961789871709,38.2011970003212));
#61248=CARTESIAN_POINT('Ctrl Pts',(2.79519402126786,0.196448450834139,38.35975844473));
#61249=CARTESIAN_POINT('Ctrl Pts',(1.35400172213932,2.45320986049924,38.5183198891387));
#61250=CARTESIAN_POINT('Ctrl Pts',(-1.3233434007851,2.46973099698168,38.6768813335475));
#61251=CARTESIAN_POINT('Ctrl Pts',(-2.34354795942612,0.915615981906982,
38.7869713344696));
#61252=CARTESIAN_POINT('Ctrl Pts',(-2.37537425850781,0.066230348892728,
38.8442075205887));
#61253=CARTESIAN_POINT('Ctrl Pts',(-2.37498223974761,0.00116593724452945,
38.848589891905));
#61254=CARTESIAN_POINT('Origin',(0.,0.,-1.84858989190508));
#61255=CARTESIAN_POINT('',(-2.37029980218114,0.00207473218684835,36.6514101080949));
#61256=CARTESIAN_POINT('',(-2.36794257065935,0.000391437457186727,36.848589891905));
#61257=CARTESIAN_POINT('',(-2.37175,1.07555357745099E-12,-1.84858989190508));
#61258=CARTESIAN_POINT('Ctrl Pts',(-2.37029980218114,0.0020747321868483,
36.6514101080949));
#61259=CARTESIAN_POINT('Ctrl Pts',(-2.36566040938742,-0.555702157675974,
36.6887924817018));
#61260=CARTESIAN_POINT('Ctrl Pts',(-1.89013456310209,-1.91214753332761,
36.7792247214399));
#61261=CARTESIAN_POINT('Ctrl Pts',(0.374295901203924,-2.78047924664893,
36.9227068273092));
#61262=CARTESIAN_POINT('Ctrl Pts',(2.54188584736079,-1.18742530783014,37.0818564257028));
#61263=CARTESIAN_POINT('Ctrl Pts',(2.37262067949971,1.49727438051885,37.2410060240964));
#61264=CARTESIAN_POINT('Ctrl Pts',(0.0221143200437823,2.8054724710268,37.40015562249));
#61265=CARTESIAN_POINT('Ctrl Pts',(-2.01580497986092,1.71296397828207,37.5369569838228));
#61266=CARTESIAN_POINT('Ctrl Pts',(-2.36648264644968,0.458108599416178,
37.6207084790244));
#61267=CARTESIAN_POINT('Ctrl Pts',(-2.36821658130285,-0.000998792486933131,
37.6514101080949));
#61268=CARTESIAN_POINT('Ctrl Pts',(-2.36794257065935,0.000391437457186762,
36.848589891905));
#61269=CARTESIAN_POINT('Ctrl Pts',(-2.36732273379814,-0.419017311524687,
36.8766284096204));
#61270=CARTESIAN_POINT('Ctrl Pts',(-2.06121258368243,-1.62987497742847,
36.9575207421387));
#61271=CARTESIAN_POINT('Ctrl Pts',(-0.128881968591299,-2.79909178025225,
37.09126688946));
#61272=CARTESIAN_POINT('Ctrl Pts',(2.27965875812724,-1.62931833193606,37.2498283338687));
#61273=CARTESIAN_POINT('Ctrl Pts',(2.60658251510917,1.02822903240515,37.4083897782775));
#61274=CARTESIAN_POINT('Ctrl Pts',(0.553362663956598,2.74687418626157,37.5669512226862));
#61275=CARTESIAN_POINT('Ctrl Pts',(-1.81428835189544,2.01617231988166,37.7136845938954));
#61276=CARTESIAN_POINT('Ctrl Pts',(-2.36635611090427,0.608907312915311,
37.8075641503016));
#61277=CARTESIAN_POINT('Ctrl Pts',(-2.37196802524163,-0.00214039621392275,
37.848589891905));
#61278=CARTESIAN_POINT('Origin',(0.,0.,-1.84858989190508));
#61279=CARTESIAN_POINT('',(-2.3756662176464,0.000177136364110247,35.6514101080949));
#61280=CARTESIAN_POINT('',(-2.37339473513533,0.00189558484520333,35.848589891905));
#61281=CARTESIAN_POINT('',(-2.37175,1.07555357745099E-12,-1.84858989190508));
#61282=CARTESIAN_POINT('Ctrl Pts',(-2.3756662176464,0.000177136364110169,
35.6514101080949));
#61283=CARTESIAN_POINT('Ctrl Pts',(-2.37483440554125,-0.777357601048919,
35.703826618248));
#61284=CARTESIAN_POINT('Ctrl Pts',(-1.53333569344657,-2.34336521677519,
35.8092929945323));
#61285=CARTESIAN_POINT('Ctrl Pts',(1.13681369625387,-2.5649203784333,35.9678092369478));
#61286=CARTESIAN_POINT('Ctrl Pts',(2.77251472574384,-0.429329754965117,
36.1269588353414));
#61287=CARTESIAN_POINT('Ctrl Pts',(1.859335179167,2.10096039122589,36.2861084337349));
#61288=CARTESIAN_POINT('Ctrl Pts',(-0.763203449633773,2.69975599917453,
36.4452580321285));
#61289=CARTESIAN_POINT('Ctrl Pts',(-2.23290357408391,1.25890136125407,36.5670252569152));
#61290=CARTESIAN_POINT('Ctrl Pts',(-2.37224423868689,0.235847080193127,
36.6357426155706));
#61291=CARTESIAN_POINT('Ctrl Pts',(-2.37029980218114,0.0020747321868483,
36.6514101080949));
#61292=CARTESIAN_POINT('Ctrl Pts',(-2.37339473513533,0.00189558484520345,
35.8485898919049));
#61293=CARTESIAN_POINT('Ctrl Pts',(-2.36765712231437,-0.656137770585933,
35.8928388541362));
#61294=CARTESIAN_POINT('Ctrl Pts',(-1.74141091723484,-2.10975212807994,
35.9899416311704));
#61295=CARTESIAN_POINT('Ctrl Pts',(0.719130113544572,-2.70820542107464,
36.1398982230075));
#61296=CARTESIAN_POINT('Ctrl Pts',(2.66420539827102,-0.86806350611665,36.2984596674162));
#61297=CARTESIAN_POINT('Ctrl Pts',(2.17652250448365,1.76473072150059,36.457021111825));
#61298=CARTESIAN_POINT('Ctrl Pts',(-0.298602167564159,2.78610149950517,
36.6155825562337));
#61299=CARTESIAN_POINT('Ctrl Pts',(-2.11160214823684,1.53266631190897,36.746105482927));
#61300=CARTESIAN_POINT('Ctrl Pts',(-2.36849115300642,0.371586263542998,
36.8237745948175));
#61301=CARTESIAN_POINT('Ctrl Pts',(-2.36794257065935,0.000391437457186762,
36.848589891905));
#61302=CARTESIAN_POINT('Origin',(0.,0.,-1.84858989190508));
#61303=CARTESIAN_POINT('',(-2.37083645980716,-0.00215799885136332,34.6514101080949));
#61304=CARTESIAN_POINT('',(-2.37380889386788,-0.00175759032045419,34.848589891905));
#61305=CARTESIAN_POINT('',(-2.37175,1.07555357745099E-12,-1.84858989190508));
#61306=CARTESIAN_POINT('Ctrl Pts',(-2.37083645980716,-0.00215799885136286,
34.6514101080949));
#61307=CARTESIAN_POINT('Ctrl Pts',(-2.37272754386709,-0.216906697555937,
34.665810888663));
#61308=CARTESIAN_POINT('Ctrl Pts',(-2.24739628056231,-1.22058222879963,
34.7332615353623));
#61309=CARTESIAN_POINT('Ctrl Pts',(-0.827441754243024,-2.68076520187573,
34.8537620481927));
#61310=CARTESIAN_POINT('Ctrl Pts',(1.8086454231506,-2.14475258658905,35.0129116465864));
#61311=CARTESIAN_POINT('Ctrl Pts',(2.78197455612906,0.363014454134983,35.1720612449799));
#61312=CARTESIAN_POINT('Ctrl Pts',(1.19772633632314,2.53704819558261,35.3312108433735));
#61313=CARTESIAN_POINT('Ctrl Pts',(-1.48763826287672,2.37867490914512,35.4903604417671));
#61314=CARTESIAN_POINT('Ctrl Pts',(-2.37136291112883,0.80588756412244,35.5970935300075));
#61315=CARTESIAN_POINT('Ctrl Pts',(-2.37567626854769,0.00957219667382547,
35.6507767521168));
#61316=CARTESIAN_POINT('Ctrl Pts',(-2.3756662176464,0.000177136364110169,
35.6514101080949));
#61317=CARTESIAN_POINT('Ctrl Pts',(-2.37380889386788,-0.00175759032045452,
34.848589891905));
#61318=CARTESIAN_POINT('Ctrl Pts',(-2.37474677486596,-0.114810256650096,
34.8561954838491));
#61319=CARTESIAN_POINT('Ctrl Pts',(-2.31608115217637,-1.01252620627014,
34.9166548905962));
#61320=CARTESIAN_POINT('Ctrl Pts',(-1.17105809706712,-2.54561341065258,
35.0299681121462));
#61321=CARTESIAN_POINT('Ctrl Pts',(1.50052034409269,-2.36642418021518,35.188529556555));
#61322=CARTESIAN_POINT('Ctrl Pts',(2.80193296331482,-0.0263888510821259,
35.3470910009637));
#61323=CARTESIAN_POINT('Ctrl Pts',(1.54482460333755,2.33774285330196,35.5056524453724));
#61324=CARTESIAN_POINT('Ctrl Pts',(-1.12290500001934,2.56721815733726,35.6642138897812));
#61325=CARTESIAN_POINT('Ctrl Pts',(-2.30695019422284,1.04264178315749,35.7785263719587));
#61326=CARTESIAN_POINT('Ctrl Pts',(-2.37451049717692,0.129859716097185,
35.8399850393333));
#61327=CARTESIAN_POINT('Ctrl Pts',(-2.37339473513533,0.00189558484520345,
35.8485898919049));
#61328=CARTESIAN_POINT('Origin',(0.,0.,-1.84858989190508));
#61329=CARTESIAN_POINT('',(-2.36801336551865,0.000709374362088072,33.6514101080949));
#61330=CARTESIAN_POINT('',(-2.36803870630727,-0.000628572818909962,33.848589891905));
#61331=CARTESIAN_POINT('',(-2.37175,1.07555357745099E-12,-1.84858989190508));
#61332=CARTESIAN_POINT('Ctrl Pts',(-2.36801336551865,0.000709374362087983,
33.6514101080949));
#61333=CARTESIAN_POINT('Ctrl Pts',(-2.36683877105606,-0.439550574027366,
33.6808450252092));
#61334=CARTESIAN_POINT('Ctrl Pts',(-2.03750269480847,-1.674913490657,33.7633298084547));
#61335=CARTESIAN_POINT('Ctrl Pts',(-0.0448724219901618,-2.805200240646,
33.8988644578313));
#61336=CARTESIAN_POINT('Ctrl Pts',(2.33619776832739,-1.55349345400542,34.0580140562249));
#61337=CARTESIAN_POINT('Ctrl Pts',(2.56951053574539,1.1264002534988,34.2171636546184));
#61338=CARTESIAN_POINT('Ctrl Pts',(0.440572383654118,2.77075042165889,34.3763132530121));
#61339=CARTESIAN_POINT('Ctrl Pts',(-1.86411244105769,1.94954241988793,34.5210620708375));
#61340=CARTESIAN_POINT('Ctrl Pts',(-2.36576113286264,0.574188595109401,
34.6127610225318));
#61341=CARTESIAN_POINT('Ctrl Pts',(-2.37083645980716,-0.00215799885136286,
34.6514101080949));
#61342=CARTESIAN_POINT('Ctrl Pts',(-2.36803870630727,-0.000628572818910204,
33.848589891905));
#61343=CARTESIAN_POINT('Ctrl Pts',(-2.36888613676592,-0.356840042454167,
33.872405928365));
#61344=CARTESIAN_POINT('Ctrl Pts',(-2.12639782110154,-1.5024792828138,33.9490757796279));
#61345=CARTESIAN_POINT('Ctrl Pts',(-0.351024016063958,-2.77998324516326,
34.0785994456937));
#61346=CARTESIAN_POINT('Ctrl Pts',(2.14289857733639,-1.80541141862616,34.2371608901025));
#61347=CARTESIAN_POINT('Ctrl Pts',(2.68008236242858,0.817730538643591,34.3957223345112));
#61348=CARTESIAN_POINT('Ctrl Pts',(0.770010256154827,2.69418056348283,34.55428377892));
#61349=CARTESIAN_POINT('Ctrl Pts',(-1.71783430240134,2.13849813336335,34.7052396313845));
#61350=CARTESIAN_POINT('Ctrl Pts',(-2.3682291245708,0.670830720808595,34.8033416690462));
#61351=CARTESIAN_POINT('Ctrl Pts',(-2.37380889386788,-0.00175759032045452,
34.848589891905));
#61352=CARTESIAN_POINT('Origin',(0.,0.,-1.84858989190508));
#61353=CARTESIAN_POINT('',(-2.37344656872762,0.00192570299439512,32.6514101080949));
#61354=CARTESIAN_POINT('',(-2.37151790930666,0.002154076539162,32.848589891905));
#61355=CARTESIAN_POINT('',(-2.37175,1.07555357745099E-12,-1.84858989190508));
#61356=CARTESIAN_POINT('Ctrl Pts',(-2.37344656872762,0.00192570299439525,
32.6514101080949));
#61357=CARTESIAN_POINT('Ctrl Pts',(-2.36762356345687,-0.659341773836592,
32.6958791617554));
#61358=CARTESIAN_POINT('Ctrl Pts',(-1.73518620177463,-2.11923842087366,
32.793398081547));
#61359=CARTESIAN_POINT('Ctrl Pts',(0.741276476036008,-2.70585866416802,
32.9439668674699));
#61360=CARTESIAN_POINT('Ctrl Pts',(2.67738679382172,-0.838308941051334,
33.1031164658635));
#61361=CARTESIAN_POINT('Ctrl Pts',(2.15207135460536,1.79993077896479,33.262266064257));
#61362=CARTESIAN_POINT('Ctrl Pts',(-0.351726937875201,2.78342416558279,
33.4214156626506));
#61363=CARTESIAN_POINT('Ctrl Pts',(-2.12889350245117,1.49938279527832,33.5511303439299));
#61364=CARTESIAN_POINT('Ctrl Pts',(-2.36895571532184,0.353919685607108,
33.627795159078));
#61365=CARTESIAN_POINT('Ctrl Pts',(-2.36801336551865,0.000709374362087983,
33.6514101080949));
#61366=CARTESIAN_POINT('Ctrl Pts',(-2.37151790930666,0.00215407653916203,
32.848589891905));
#61367=CARTESIAN_POINT('Ctrl Pts',(-2.36610629731291,-0.594299025520429,
32.8886163728808));
#61368=CARTESIAN_POINT('Ctrl Pts',(-1.83591513178192,-1.9869237846516,32.9814966686595));
#61369=CARTESIAN_POINT('Ctrl Pts',(0.5015298178546,-2.75680839831995,33.1272307792412));
#61370=CARTESIAN_POINT('Ctrl Pts',(2.58675326481436,-1.07714077548725,33.2857922236499));
#61371=CARTESIAN_POINT('Ctrl Pts',(2.30994215059737,1.58609330246939,33.4443536680588));
#61372=CARTESIAN_POINT('Ctrl Pts',(-0.076139789038159,2.80102256966442,
33.6029151124674));
#61373=CARTESIAN_POINT('Ctrl Pts',(-2.04474804530386,1.65994568587728,33.7376605204162));
#61374=CARTESIAN_POINT('Ctrl Pts',(-2.36700547402024,0.433683396591004,
33.8195521135621));
#61375=CARTESIAN_POINT('Ctrl Pts',(-2.36803870630727,-0.000628572818910204,
33.848589891905));
#61376=CARTESIAN_POINT('Origin',(0.,0.,-1.84858989190508));
#61377=CARTESIAN_POINT('',(-2.37430589928956,-0.0015910093592776,31.6514101080949));
#61378=CARTESIAN_POINT('',(-2.37519828256487,-0.000898997154156478,31.848589891905));
#61379=CARTESIAN_POINT('',(-2.37175,1.07555357745099E-12,-1.84858989190508));
#61380=CARTESIAN_POINT('Ctrl Pts',(-2.37430589928956,-0.0015910093592772,
31.6514101080949));
#61381=CARTESIAN_POINT('Ctrl Pts',(-2.37504475585361,-0.0974633462288916,
31.6578634321704));
#61382=CARTESIAN_POINT('Ctrl Pts',(-2.32616367491842,-0.98069910565149,
31.717366622377));
#61383=CARTESIAN_POINT('Ctrl Pts',(-1.21826882213122,-2.52724810839787,
31.8299196787149));
#61384=CARTESIAN_POINT('Ctrl Pts',(1.46829221901895,-2.39066515512857,31.9890692771084));
#61385=CARTESIAN_POINT('Ctrl Pts',(2.80499514663885,-0.0562507929721938,
32.148218875502));
#61386=CARTESIAN_POINT('Ctrl Pts',(1.56295699802168,2.32987710978769,32.3073684738957));
#61387=CARTESIAN_POINT('Ctrl Pts',(-1.11596827534518,2.57405841674206,32.4665180722891));
#61388=CARTESIAN_POINT('Ctrl Pts',(-2.30707249918363,1.04480000964771,32.5811986170223));
#61389=CARTESIAN_POINT('Ctrl Pts',(-2.37457018418897,0.129524825184061,
32.6428292956242));
#61390=CARTESIAN_POINT('Ctrl Pts',(-2.37344656872762,0.00192570299439525,
32.6514101080949));
#61391=CARTESIAN_POINT('Ctrl Pts',(-2.37519828256487,-0.000898997154156859,
31.848589891905));
#61392=CARTESIAN_POINT('Ctrl Pts',(-2.37544230083747,-0.051109655468214,
31.8519730025937));
#61393=CARTESIAN_POINT('Ctrl Pts',(-2.35126215380067,-0.885514299668502,
31.9082099280854));
#61394=CARTESIAN_POINT('Ctrl Pts',(-1.3697471531232,-2.44444624398976,32.0173006683799));
#61395=CARTESIAN_POINT('Ctrl Pts',(1.30762066055104,-2.47823584659426,32.1758621127887));
#61396=CARTESIAN_POINT('Ctrl Pts',(2.79096458522799,-0.249081085688892,
32.3344235571974));
#61397=CARTESIAN_POINT('Ctrl Pts',(1.72580305366397,2.20751636986205,32.4929850016062));
#61398=CARTESIAN_POINT('Ctrl Pts',(-0.915236051531332,2.64837075826291,
32.6515464460149));
#61399=CARTESIAN_POINT('Ctrl Pts',(-2.26482404050824,1.17010253722111,32.7700814094479));
#61400=CARTESIAN_POINT('Ctrl Pts',(-2.37325217502012,0.193300109510363,
32.8357625580779));
#61401=CARTESIAN_POINT('Ctrl Pts',(-2.37151790930666,0.00215407653916203,
32.848589891905));
#61402=CARTESIAN_POINT('Origin',(0.,0.,-1.84858989190508));
#61403=CARTESIAN_POINT('',(-2.36839481200122,-0.00118517904615592,30.6514101080949));
#61404=CARTESIAN_POINT('',(-2.36891564579557,-0.00151055549120149,30.848589891905));
#61405=CARTESIAN_POINT('',(-2.37175,1.07555357745099E-12,-1.84858989190508));
#61406=CARTESIAN_POINT('Ctrl Pts',(-2.36839481200122,-0.00118517904615575,
30.6514101080949));
#61407=CARTESIAN_POINT('Ctrl Pts',(-2.36984063649032,-0.322445251385961,
30.6728975687166));
#61408=CARTESIAN_POINT('Ctrl Pts',(-2.15901428293454,-1.43503844100005,
30.7474348954694));
#61409=CARTESIAN_POINT('Ctrl Pts',(-0.463035703261235,-2.76708508396162,
30.8750220883534));
#61410=CARTESIAN_POINT('Ctrl Pts',(2.07817926003504,-1.88476335053973,31.034171686747));
#61411=CARTESIAN_POINT('Ctrl Pts',(2.70884324499614,0.730294597006095,31.1933212851405));
#61412=CARTESIAN_POINT('Ctrl Pts',(0.849162334591095,2.67396433295012,31.3524708835341));
#61413=CARTESIAN_POINT('Ctrl Pts',(-1.68412356093239,2.18022151201017,31.5051671578522));
#61414=CARTESIAN_POINT('Ctrl Pts',(-2.36897094933856,0.690659887185638,
31.6048135660392));
#61415=CARTESIAN_POINT('Ctrl Pts',(-2.37430589928956,-0.0015910093592772,
31.6514101080949));
#61416=CARTESIAN_POINT('Ctrl Pts',(-2.36891564579557,-0.00151055549120167,
30.848589891905));
#61417=CARTESIAN_POINT('Ctrl Pts',(-2.37062840873568,-0.294295702210565,
30.8681834471096));
#61418=CARTESIAN_POINT('Ctrl Pts',(-2.18474225478032,-1.37477397204726,
30.940630817117));
#61419=CARTESIAN_POINT('Ctrl Pts',(-0.570943356725327,-2.74327329784255,
31.0659320019274));
#61420=CARTESIAN_POINT('Ctrl Pts',(1.99257021690915,-1.97007325598095,31.2244934463362));
#61421=CARTESIAN_POINT('Ctrl Pts',(2.73661388518784,0.602054106075114,31.3830548907449));
#61422=CARTESIAN_POINT('Ctrl Pts',(0.981781195472087,2.62442953562526,31.5416163351537));
#61423=CARTESIAN_POINT('Ctrl Pts',(-1.6129731567046,2.25834827685961,31.6967946688737));
#61424=CARTESIAN_POINT('Ctrl Pts',(-2.37163004112299,0.733323690003802,
31.7991191877908));
#61425=CARTESIAN_POINT('Ctrl Pts',(-2.37519828256487,-0.000898997154156859,
31.848589891905));
#61426=CARTESIAN_POINT('Origin',(0.,0.,-1.84858989190508));
#61427=CARTESIAN_POINT('',(-2.36995400383523,0.0019928976040509,29.6514101080949));
#61428=CARTESIAN_POINT('',(-2.36976239142724,0.00188907497310223,29.848589891905));
#61429=CARTESIAN_POINT('',(-2.37175,1.07555357745099E-12,-1.84858989190508));
#61430=CARTESIAN_POINT('Ctrl Pts',(-2.36995400383523,0.00199289760405105,
29.6514101080949));
#61431=CARTESIAN_POINT('Ctrl Pts',(-2.36564524447228,-0.543141402735341,
29.6879317052627));
#61432=CARTESIAN_POINT('Ctrl Pts',(-1.907411081712,-1.8866583110207,29.7775031685617));
#61433=CARTESIAN_POINT('Ctrl Pts',(0.32913472971066,-2.78618596904008,29.920124497992));
#61434=CARTESIAN_POINT('Ctrl Pts',(2.52228565055847,-1.22851008191401,30.0792740963855));
#61435=CARTESIAN_POINT('Ctrl Pts',(2.39660132461721,1.4585828791058,30.2384236947791));
#61436=CARTESIAN_POINT('Ctrl Pts',(0.067628238422609,2.80474390020647,30.3975732931727));
#61437=CARTESIAN_POINT('Ctrl Pts',(-2.00067933025812,1.73877948815203,30.5352354309446));
#61438=CARTESIAN_POINT('Ctrl Pts',(-2.36627107576156,0.470705885969103,
30.6198477025854));
#61439=CARTESIAN_POINT('Ctrl Pts',(-2.36839481200122,-0.00118517904615575,
30.6514101080949));
#61440=CARTESIAN_POINT('Ctrl Pts',(-2.36976239142724,0.0018890749731023,
29.848589891905));
#61441=CARTESIAN_POINT('Ctrl Pts',(-2.36575561414334,-0.532646635303957,
29.8843938916254));
#61442=CARTESIAN_POINT('Ctrl Pts',(-1.9223422941335,-1.86228449563888,29.9730517061487));
#61443=CARTESIAN_POINT('Ctrl Pts',(0.28075407675448,-2.78795657276624,30.1145633354749));
#61444=CARTESIAN_POINT('Ctrl Pts',(2.49292302707169,-1.27939809455089,30.2731247798837));
#61445=CARTESIAN_POINT('Ctrl Pts',(2.42873635105556,1.39741348222569,30.4316862242924));
#61446=CARTESIAN_POINT('Ctrl Pts',(0.146804643376738,2.79820890927176,30.5902476687012));
#61447=CARTESIAN_POINT('Ctrl Pts',(-1.97063355459528,1.78652468932462,30.7292155579053));
#61448=CARTESIAN_POINT('Ctrl Pts',(-2.3660082132534,0.495495214251002,30.8153296323066));
#61449=CARTESIAN_POINT('Ctrl Pts',(-2.36891564579557,-0.00151055549120167,
30.848589891905));
#61450=CARTESIAN_POINT('Origin',(0.,0.,-1.84858989190508));
#61451=CARTESIAN_POINT('',(-2.37559433303246,0.000415362230552236,28.6514101080949));
#61452=CARTESIAN_POINT('',(-2.37558996096397,0.000230858190189672,28.848589891905));
#61453=CARTESIAN_POINT('',(-2.37175,1.07555357745099E-12,-1.84858989190508));
#61454=CARTESIAN_POINT('Ctrl Pts',(-2.37559433303246,0.000415362230552201,
28.6514101080949));
#61455=CARTESIAN_POINT('Ctrl Pts',(-2.37375083518073,-0.76441301960334,
28.7029658418089));
#61456=CARTESIAN_POINT('Ctrl Pts',(-1.55667585051139,-2.31961727945024,
28.8075714416541));
#61457=CARTESIAN_POINT('Ctrl Pts',(1.09504940571272,-2.58302704659199,28.9652269076305));
#61458=CARTESIAN_POINT('Ctrl Pts',(2.76518410684866,-0.474256027488414,
29.1243765060241));
#61459=CARTESIAN_POINT('Ctrl Pts',(1.89317756819207,2.07051699333089,29.2835261044177));
#61460=CARTESIAN_POINT('Ctrl Pts',(-0.719300701960229,2.71178325544964,
29.4426757028112));
#61461=CARTESIAN_POINT('Ctrl Pts',(-2.22273779394574,1.28494796187104,29.565303704037));
#61462=CARTESIAN_POINT('Ctrl Pts',(-2.37190398245533,0.248699696755391,
29.6348818391316));
#61463=CARTESIAN_POINT('Ctrl Pts',(-2.36995400383523,0.00199289760405105,
29.6514101080949));
#61464=CARTESIAN_POINT('Ctrl Pts',(-2.37558996096397,0.000230858190189351,
28.848589891905));
#61465=CARTESIAN_POINT('Ctrl Pts',(-2.37451683347506,-0.771404774036993,
28.9006043361412));
#61466=CARTESIAN_POINT('Ctrl Pts',(-1.54564963095845,-2.32910717712637,
29.0054725951804));
#61467=CARTESIAN_POINT('Ctrl Pts',(1.10644174224207,-2.57435649712099,29.1631946690224));
#61468=CARTESIAN_POINT('Ctrl Pts',(2.7623251407879,-0.470196256701246,29.3217561134311));
#61469=CARTESIAN_POINT('Ctrl Pts',(1.89585453653854,2.06331293785769,29.4803175578399));
#61470=CARTESIAN_POINT('Ctrl Pts',(-0.701772262303996,2.71275512995654,
29.6388790022487));
#61471=CARTESIAN_POINT('Ctrl Pts',(-2.21673174114633,1.29779949503705,29.761636446937));
#61472=CARTESIAN_POINT('Ctrl Pts',(-2.37167041322091,0.256434239938047,
29.8315400768225));
#61473=CARTESIAN_POINT('Ctrl Pts',(-2.36976239142724,0.0018890749731023,
29.848589891905));
#61474=CARTESIAN_POINT('Origin',(0.,0.,-1.84858989190508));
#61475=CARTESIAN_POINT('',(-2.37121570870644,-0.00218817987852429,27.6514101080949));
#61476=CARTESIAN_POINT('',(-2.37042075827088,-0.00205354385727247,27.848589891905));
#61477=CARTESIAN_POINT('',(-2.37175,1.07555357745099E-12,-1.84858989190508));
#61478=CARTESIAN_POINT('Ctrl Pts',(-2.37121570870644,-0.0021881798785239,
27.6514101080949));
#61479=CARTESIAN_POINT('Ctrl Pts',(-2.37304212744356,-0.204018644870209,
27.6649501122239));
#61480=CARTESIAN_POINT('Ctrl Pts',(-2.25693119590959,-1.19455237637443,
27.7315399824841));
#61481=CARTESIAN_POINT('Ctrl Pts',(-0.870827027847972,-2.66698747877582,
27.8511797188755));
#61482=CARTESIAN_POINT('Ctrl Pts',(1.77360972961834,-2.17381472333333,28.0103293172691));
#61483=CARTESIAN_POINT('Ctrl Pts',(2.7874981175229,0.317830409469884,28.1694789156627));
#61484=CARTESIAN_POINT('Ctrl Pts',(1.23873112821468,2.51728169189892,28.3286285140562));
#61485=CARTESIAN_POINT('Ctrl Pts',(-1.44884954017187,2.40249806125235,28.4877781124498));
#61486=CARTESIAN_POINT('Ctrl Pts',(-2.36530750122204,0.831688918896625,
28.5953719771294));
#61487=CARTESIAN_POINT('Ctrl Pts',(-2.37564775928989,0.0225807897506126,
28.6499159756778));
#61488=CARTESIAN_POINT('Ctrl Pts',(-2.37559433303246,0.000415362230552201,
28.6514101080949));
#61489=CARTESIAN_POINT('Ctrl Pts',(-2.37042075827088,-0.00205354385727267,
27.848589891905));
#61490=CARTESIAN_POINT('Ctrl Pts',(-2.37232842441219,-0.231374808268618,
27.8639609658541));
#61491=CARTESIAN_POINT('Ctrl Pts',(-2.23658719967056,-1.24701197475112,
27.9321858546062));
#61492=CARTESIAN_POINT('Ctrl Pts',(-0.787247754401329,-2.68919424297219,
28.0532645581612));
#61493=CARTESIAN_POINT('Ctrl Pts',(1.82962584537607,-2.12226152233333,28.2118260025699));
#61494=CARTESIAN_POINT('Ctrl Pts',(2.77581846464243,0.382565751988956,28.3703874469787));
#61495=CARTESIAN_POINT('Ctrl Pts',(1.18733596115095,2.53806186264293,28.5289488913874));
#61496=CARTESIAN_POINT('Ctrl Pts',(-1.48533521008643,2.37598485199765,28.6875103357962));
#61497=CARTESIAN_POINT('Ctrl Pts',(-2.36988450532629,0.809206391250685,
28.7940573359687));
#61498=CARTESIAN_POINT('Ctrl Pts',(-2.37560727830038,0.0126829423644369,
28.8477505213383));
#61499=CARTESIAN_POINT('Ctrl Pts',(-2.37558996096397,0.000230858190189351,
28.848589891905));
#61500=CARTESIAN_POINT('Origin',(0.,0.,-1.84858989190508));
#61501=CARTESIAN_POINT('',(-2.36791541979134,0.000503980893847333,26.6514101080949));
#61502=CARTESIAN_POINT('',(-2.36848027041357,0.00119022360032209,26.848589891905));
#61503=CARTESIAN_POINT('',(-2.37175,1.07555357745099E-12,-1.84858989190508));
#61504=CARTESIAN_POINT('Ctrl Pts',(-2.36791541979134,0.000503980893847393,
26.6514101080949));
#61505=CARTESIAN_POINT('Ctrl Pts',(-2.36710719014345,-0.426925371301292,
26.6799842487701));
#61506=CARTESIAN_POINT('Ctrl Pts',(-2.05187220716749,-1.64901827578131,
26.7616082555765));
#61507=CARTESIAN_POINT('Ctrl Pts',(-0.0903796039458558,-2.80410296736195,
26.896282128514));
#61508=CARTESIAN_POINT('Ctrl Pts',(2.3106855433324,-1.59119271121138,27.0554317269076));
#61509=CARTESIAN_POINT('Ctrl Pts',(2.58744764787687,1.08456285842457,27.2145813253012));
#61510=CARTESIAN_POINT('Ctrl Pts',(0.48546854847008,2.76323763234795,27.3737309236948));
#61511=CARTESIAN_POINT('Ctrl Pts',(-1.84601931779875,1.97486971266958,27.5193405179593));
#61512=CARTESIAN_POINT('Ctrl Pts',(-2.36588620130201,0.586755054088587,
27.6119002460927));
#61513=CARTESIAN_POINT('Ctrl Pts',(-2.37121570870644,-0.0021881798785239,
27.6514101080949));
#61514=CARTESIAN_POINT('Ctrl Pts',(-2.36848027041357,0.00119022360032195,
26.848589891905));
#61515=CARTESIAN_POINT('Ctrl Pts',(-2.36632923020358,-0.470947746561001,
26.88017141037));
#61516=CARTESIAN_POINT('Ctrl Pts',(-2.00099020303499,-1.73630730429607,
26.9646067436378));
#61517=CARTESIAN_POINT('Ctrl Pts',(0.0582007337807619,-2.8014527263247,
27.1018958917086));
#61518=CARTESIAN_POINT('Ctrl Pts',(2.38330878115067,-1.47355487069022,27.2604573361174));
#61519=CARTESIAN_POINT('Ctrl Pts',(2.53215294297463,1.19988590150465,27.4190187805261));
#61520=CARTESIAN_POINT('Ctrl Pts',(0.368819578303693,2.77767831505101,27.5775802249349));
#61521=CARTESIAN_POINT('Ctrl Pts',(-1.88893002712957,1.91202293803979,27.7207705953945));
#61522=CARTESIAN_POINT('Ctrl Pts',(-2.3657688675932,0.557151984308005,27.8111071510512));
#61523=CARTESIAN_POINT('Ctrl Pts',(-2.37042075827088,-0.00205354385727267,
27.848589891905));
#61524=CARTESIAN_POINT('Origin',(0.,0.,-1.84858989190508));
#61525=CARTESIAN_POINT('',(-2.37307089521247,0.00202464274905245,25.6514101080949));
#61526=CARTESIAN_POINT('',(-2.37473384480564,0.00128782070115716,25.848589891905));
#61527=CARTESIAN_POINT('',(-2.37175,1.07555357745099E-12,-1.84858989190508));
#61528=CARTESIAN_POINT('Ctrl Pts',(-2.37307089521247,0.00202464274905237,
25.6514101080949));
#61529=CARTESIAN_POINT('Ctrl Pts',(-2.36718725723238,-0.646708552619323,
25.6950183853163));
#61530=CARTESIAN_POINT('Ctrl Pts',(-1.7552402308422,-2.09438973910438,25.7916765286689));
#61531=CARTESIAN_POINT('Ctrl Pts',(0.697277587574235,-2.71752937247129,
25.9413845381526));
#61532=CARTESIAN_POINT('Ctrl Pts',(2.66343320026788,-0.881637971101683,
26.1005341365462));
#61533=CARTESIAN_POINT('Ctrl Pts',(2.18099113692833,1.76477748881203,26.2596837349398));
#61534=CARTESIAN_POINT('Ctrl Pts',(-0.306520859756921,2.78876440147091,
26.4188333333333));
#61535=CARTESIAN_POINT('Ctrl Pts',(-2.11621631635713,1.52539742028699,26.5494087910517));
#61536=CARTESIAN_POINT('Ctrl Pts',(-2.36860772431913,0.366626748857101,
26.6269343826389));
#61537=CARTESIAN_POINT('Ctrl Pts',(-2.36791541979134,0.000503980893847393,
26.6514101080949));
#61538=CARTESIAN_POINT('Ctrl Pts',(-2.37473384480564,0.00128782070115717,
25.848589891905));
#61539=CARTESIAN_POINT('Ctrl Pts',(-2.3700792053546,-0.708386931882113,
25.8963818548858));
#61540=CARTESIAN_POINT('Ctrl Pts',(-1.65568478423942,-2.21103251101488,
25.9970276326695));
#61541=CARTESIAN_POINT('Ctrl Pts',(0.898257358734679,-2.65417754129669,
26.1505272252561));
#61542=CARTESIAN_POINT('Ctrl Pts',(2.71619596155049,-0.688334367659731,
26.3090886696649));
#61543=CARTESIAN_POINT('Ctrl Pts',(2.05390236619762,1.90604558533434,26.4676501140736));
#61544=CARTESIAN_POINT('Ctrl Pts',(-0.483865183409376,2.7599636206894,26.6262115584824));
#61545=CARTESIAN_POINT('Ctrl Pts',(-2.16234346834408,1.42556571001596,26.7531914844262));
#61546=CARTESIAN_POINT('Ctrl Pts',(-2.36992914200068,0.319207193709481,
26.827317595567));
#61547=CARTESIAN_POINT('Ctrl Pts',(-2.36848027041357,0.00119022360032195,
26.848589891905));
#61548=CARTESIAN_POINT('Origin',(0.,0.,-1.84858989190508));
#61549=CARTESIAN_POINT('',(-2.37461414594325,-0.0014219220721963,24.6514101080949));
#61550=CARTESIAN_POINT('',(-2.37227285406081,-0.00211555575218542,24.848589891905));
#61551=CARTESIAN_POINT('',(-2.37175,1.07555357745099E-12,-1.84858989190508));
#61552=CARTESIAN_POINT('Ctrl Pts',(-2.37461414594325,-0.00142192207219587,
24.6514101080949));
#61553=CARTESIAN_POINT('Ctrl Pts',(-2.37520144012387,-0.0844780524433969,
24.6570026557313));
#61554=CARTESIAN_POINT('Ctrl Pts',(-2.33348900523777,-0.95479259564346,
24.7156450694988));
#61555=CARTESIAN_POINT('Ctrl Pts',(-1.25911190801061,-2.50714960213454,
24.8273373493976));
#61556=CARTESIAN_POINT('Ctrl Pts',(1.42931150622999,-2.41417284852102,24.9864869477912));
#61557=CARTESIAN_POINT('Ctrl Pts',(2.80371329149552,-0.101753149675579,
25.1456365461847));
#61558=CARTESIAN_POINT('Ctrl Pts',(1.60055245978652,2.30421217509344,25.3047861445783));
#61559=CARTESIAN_POINT('Ctrl Pts',(-1.07405846611233,2.59182567618851,25.4639357429719));
#61560=CARTESIAN_POINT('Ctrl Pts',(-2.29894274585785,1.07076183898232,25.5794770641441));
#61561=CARTESIAN_POINT('Ctrl Pts',(-2.37434475638383,0.142481283852646,
25.6419685191851));
#61562=CARTESIAN_POINT('Ctrl Pts',(-2.37307089521247,0.00202464274905237,
25.6514101080949));
#61563=CARTESIAN_POINT('Ctrl Pts',(-2.37227285406081,-0.00211555575218592,
24.848589891905));
#61564=CARTESIAN_POINT('Ctrl Pts',(-2.3737989493321,-0.168110516416099,
24.8597384845987));
#61565=CARTESIAN_POINT('Ctrl Pts',(-2.28226874561123,-1.11939179033149,
24.9237408920953));
#61566=CARTESIAN_POINT('Ctrl Pts',(-0.998567672067767,-2.61808848352113,
25.0405971143948));
#61567=CARTESIAN_POINT('Ctrl Pts',(1.65509714933991,-2.26101263364264,25.1991585588037));
#61568=CARTESIAN_POINT('Ctrl Pts',(2.79744787596231,0.16065517271071,25.3577200032123));
#61569=CARTESIAN_POINT('Ctrl Pts',(1.3853730777416,2.43562438374916,25.5162814476211));
#61570=CARTESIAN_POINT('Ctrl Pts',(-1.29172345032858,2.48655891366281,25.6748428920299));
#61571=CARTESIAN_POINT('Ctrl Pts',(-2.33792441559412,0.935961079615963,
25.7856123734578));
#61572=CARTESIAN_POINT('Ctrl Pts',(-2.37522683763784,0.0764525181823475,
25.8435280400829));
#61573=CARTESIAN_POINT('Ctrl Pts',(-2.37473384480564,0.00128782070115717,
25.848589891905));
#61574=CARTESIAN_POINT('Origin',(0.,0.,-1.84858989190508));
#61575=CARTESIAN_POINT('',(-2.36860268394698,-0.00136012066467478,23.6514101080949));
#61576=CARTESIAN_POINT('',(-2.3679029786215,0.000227208911412896,23.848589891905));
#61577=CARTESIAN_POINT('',(-2.37175,1.07555357745099E-12,-1.84858989190508));
#61578=CARTESIAN_POINT('Ctrl Pts',(-2.36860268394698,-0.00136012066467461,
23.651410108095));
#61579=CARTESIAN_POINT('Ctrl Pts',(-2.37020370805452,-0.309682979419102,
23.6720367922775));
#61580=CARTESIAN_POINT('Ctrl Pts',(-2.17071820741675,-1.40899174483152,
23.7457133425912));
#61581=CARTESIAN_POINT('Ctrl Pts',(-0.507869442880617,-2.75920832003777,
23.8724397590362));
#61582=CARTESIAN_POINT('Ctrl Pts',(2.04732629486344,-1.91823277178195,24.0315893574297));
#61583=CARTESIAN_POINT('Ctrl Pts',(2.7203353844948,0.686248730594912,24.1907389558233));
#61584=CARTESIAN_POINT('Ctrl Pts',(0.892434408187573,2.6598350985466,24.3498885542168));
#61585=CARTESIAN_POINT('Ctrl Pts',(-1.6628526585275,2.2047074150282,24.5034456049741));
#61586=CARTESIAN_POINT('Ctrl Pts',(-2.36963047681923,0.703376943895443,
24.6039527896001));
#61587=CARTESIAN_POINT('Ctrl Pts',(-2.37461414594325,-0.00142192207219587,
24.6514101080949));
#61588=CARTESIAN_POINT('Ctrl Pts',(-2.3679029786215,0.000227208911412861,
23.848589891905));
#61589=CARTESIAN_POINT('Ctrl Pts',(-2.36755222713902,-0.409034741783179,
23.8759489291145));
#61590=CARTESIAN_POINT('Ctrl Pts',(-2.07217810476315,-1.6094075389743,23.956161781127));
#61591=CARTESIAN_POINT('Ctrl Pts',(-0.164721108680563,-2.79721140774162,
24.0892284479423));
#61592=CARTESIAN_POINT('Ctrl Pts',(2.25860455255274,-1.6583817951343,24.2477898923511));
#61593=CARTESIAN_POINT('Ctrl Pts',(2.61953714146364,0.99476121141571,24.4063513367598));
#61594=CARTESIAN_POINT('Ctrl Pts',(0.588499322301271,2.73956077700343,24.5649127811686));
#61595=CARTESIAN_POINT('Ctrl Pts',(-1.79932587717851,2.03600208971102,24.7123256328836));
#61596=CARTESIAN_POINT('Ctrl Pts',(-2.36656395931527,0.61884682880159,24.8068846697958));
#61597=CARTESIAN_POINT('Ctrl Pts',(-2.37227285406081,-0.00211555575218592,
24.848589891905));
#61598=CARTESIAN_POINT('Origin',(0.,0.,-1.84858989190508));
#61599=CARTESIAN_POINT('',(-2.36962670248717,0.00189177622211031,22.651410108095));
#61600=CARTESIAN_POINT('',(-2.37310225641301,0.0019731259294458,22.848589891905));
#61601=CARTESIAN_POINT('',(-2.37175,1.07555357745099E-12,-1.84858989190508));
#61602=CARTESIAN_POINT('Ctrl Pts',(-2.36962670248717,0.00189177622211021,
22.651410108095));
#61603=CARTESIAN_POINT('Ctrl Pts',(-2.36567043422174,-0.530579655077376,
22.6870709288237));
#61604=CARTESIAN_POINT('Ctrl Pts',(-1.9243615988136,-1.86111040461567,22.7757816156835));
#61605=CARTESIAN_POINT('Ctrl Pts',(0.283886816331191,-2.79115929317747,
22.9175421686747));
#61606=CARTESIAN_POINT('Ctrl Pts',(2.50202163773962,-1.26927130616756,23.0766917670682));
#61607=CARTESIAN_POINT('Ctrl Pts',(2.41995070706164,1.41950713269408,23.2358413654619));
#61608=CARTESIAN_POINT('Ctrl Pts',(0.113125021193992,2.80327748429537,23.3949909638554));
#61609=CARTESIAN_POINT('Ctrl Pts',(-1.98524427925328,1.76455614662456,23.5335138780665));
#61610=CARTESIAN_POINT('Ctrl Pts',(-2.36608602661693,0.483294032172269,
23.6189869261463));
#61611=CARTESIAN_POINT('Ctrl Pts',(-2.36860268394698,-0.00136012066467461,
23.651410108095));
#61612=CARTESIAN_POINT('Ctrl Pts',(-2.37310225641302,0.00197312592944565,
22.848589891905));
#61613=CARTESIAN_POINT('Ctrl Pts',(-2.36731533440048,-0.646162491872702,
22.8921593736304));
#61614=CARTESIAN_POINT('Ctrl Pts',(-1.7571753397551,-2.09013014137335,22.9885826701586));
#61615=CARTESIAN_POINT('Ctrl Pts',(0.684385634967381,-2.71719359006588,
23.1378597814898));
#61616=CARTESIAN_POINT('Ctrl Pts',(2.65286911563599,-0.902114271336809,
23.2964212258986));
#61617=CARTESIAN_POINT('Ctrl Pts',(2.19894585862139,1.73671005470014,23.4549826703074));
#61618=CARTESIAN_POINT('Ctrl Pts',(-0.262894499289412,2.789697328652,23.6135441147161));
#61619=CARTESIAN_POINT('Ctrl Pts',(-2.10132025508898,1.55318133166961,23.7447465219153));
#61620=CARTESIAN_POINT('Ctrl Pts',(-2.36822982970795,0.381601828584115,
23.8230951143116));
#61621=CARTESIAN_POINT('Ctrl Pts',(-2.3679029786215,0.000227208911412861,
23.848589891905));
#61622=CARTESIAN_POINT('Origin',(0.,0.,-1.84858989190508));
#61623=CARTESIAN_POINT('',(-2.37546973462112,0.000647720784673299,21.651410108095));
#61624=CARTESIAN_POINT('',(-2.37407662519319,-0.00164808854746207,21.848589891905));
#61625=CARTESIAN_POINT('',(-2.37175,1.07555357745099E-12,-1.84858989190508));
#61626=CARTESIAN_POINT('Ctrl Pts',(-2.37546973462112,0.000647720784673306,
21.651410108095));
#61627=CARTESIAN_POINT('Ctrl Pts',(-2.37274529400723,-0.751516627875191,
21.7021050653699));
#61628=CARTESIAN_POINT('Ctrl Pts',(-1.57965287445059,-2.29572849416704,
21.8058498887759));
#61629=CARTESIAN_POINT('Ctrl Pts',(1.05299683804908,-2.60045372645548,21.9626445783133));
#61630=CARTESIAN_POINT('Ctrl Pts',(2.75712554852525,-0.519057447732828,
22.1217941767068));
#61631=CARTESIAN_POINT('Ctrl Pts',(1.92652156513405,2.03952851989154,22.2809437751004));
#61632=CARTESIAN_POINT('Ctrl Pts',(-0.675208582315117,2.72309663705597,
22.440093373494));
#61633=CARTESIAN_POINT('Ctrl Pts',(-2.21231188343661,1.31099872606338,22.5635821511589));
#61634=CARTESIAN_POINT('Ctrl Pts',(-2.37155587088784,0.261537227593486,
22.6340210626925));
#61635=CARTESIAN_POINT('Ctrl Pts',(-2.36962670248717,0.00189177622211021,
22.651410108095));
#61636=CARTESIAN_POINT('Ctrl Pts',(-2.37407662519319,-0.00164808854746259,
21.848589891905));
#61637=CARTESIAN_POINT('Ctrl Pts',(-2.37489245732554,-0.104570379898861,
21.8555160033433));
#61638=CARTESIAN_POINT('Ctrl Pts',(-2.32211136907176,-0.992060131910626,
21.9152959295845));
#61639=CARTESIAN_POINT('Ctrl Pts',(-1.20356513206848,-2.53040622748872,
22.0279296706286));
#61640=CARTESIAN_POINT('Ctrl Pts',(1.47008916186248,-2.38544808357241,22.1864911150373));
#61641=CARTESIAN_POINT('Ctrl Pts',(2.80136517195679,-0.0622725990490076,
22.3450525594461));
#61642=CARTESIAN_POINT('Ctrl Pts',(1.5746386679948,2.31776568455491,22.5036140038548));
#61643=CARTESIAN_POINT('Ctrl Pts',(-1.08993310932985,2.58138926170217,22.6621754482636));
#61644=CARTESIAN_POINT('Ctrl Pts',(-2.30056081128665,1.06313136545322,22.777167410947));
#61645=CARTESIAN_POINT('Ctrl Pts',(-2.37433540652935,0.140086014052276,
22.8393055588275));
#61646=CARTESIAN_POINT('Ctrl Pts',(-2.37310225641302,0.00197312592944565,
22.848589891905));
#61647=CARTESIAN_POINT('Origin',(0.,0.,-1.84858989190508));
#61648=CARTESIAN_POINT('',(-2.37160301736592,-0.00219628840535642,20.651410108095));
#61649=CARTESIAN_POINT('',(-2.3681294836508,-0.000785534163144364,20.848589891905));
#61650=CARTESIAN_POINT('',(-2.37175,1.07555357745099E-12,-1.84858989190508));
#61651=CARTESIAN_POINT('Ctrl Pts',(-2.37160301736592,-0.00219628840535644,
20.651410108095));
#61652=CARTESIAN_POINT('Ctrl Pts',(-2.37334397584842,-0.191117152306352,
20.6640893357849));
#61653=CARTESIAN_POINT('Ctrl Pts',(-2.26621572573114,-1.16853165787267,
20.7298184296059));
#61654=CARTESIAN_POINT('Ctrl Pts',(-0.91398305353419,-2.65250766299173,
20.8485973895582));
#61655=CARTESIAN_POINT('Ctrl Pts',(1.73810712782103,-2.20230459668849,21.0077469879518));
#61656=CARTESIAN_POINT('Ctrl Pts',(2.79228786153128,0.272562695031161,21.1668965863454));
#61657=CARTESIAN_POINT('Ctrl Pts',(1.2794098201712,2.49685250594164,21.326046184739));
#61658=CARTESIAN_POINT('Ctrl Pts',(-1.40967940307629,2.42568874856607,21.4851957831325));
#61659=CARTESIAN_POINT('Ctrl Pts',(-2.35903719972994,0.857509241612945,
21.5936504242512));
#61660=CARTESIAN_POINT('Ctrl Pts',(-2.37559629177148,0.0355876552723523,
21.6490551992387));
#61661=CARTESIAN_POINT('Ctrl Pts',(-2.37546973462112,0.000647720784673306,
21.651410108095));
#61662=CARTESIAN_POINT('Ctrl Pts',(-2.3681294836508,-0.000785534163144468,
20.848589891905));
#61663=CARTESIAN_POINT('Ctrl Pts',(-2.36916056635605,-0.346801018693284,
20.8717264478591));
#61664=CARTESIAN_POINT('Ctrl Pts',(-2.1362394959101,-1.48194260514544,20.9477168186161));
#61665=CARTESIAN_POINT('Ctrl Pts',(-0.386600015079116,-2.7752594710379,
21.0765610041761));
#61666=CARTESIAN_POINT('Ctrl Pts',(2.11959990940443,-1.83270863131529,21.2351224485848));
#61667=CARTESIAN_POINT('Ctrl Pts',(2.69033567115523,0.783338164367446,21.3936838929936));
#61668=CARTESIAN_POINT('Ctrl Pts',(0.804452967251542,2.68409763733083,21.5522453374023));
#61669=CARTESIAN_POINT('Ctrl Pts',(-1.70153384115788,2.1579663888224,21.7038806703728));
#61670=CARTESIAN_POINT('Ctrl Pts',(-2.36866676476808,0.680839409513659,
21.8026621885404));
#61671=CARTESIAN_POINT('Ctrl Pts',(-2.37407662519319,-0.00164808854746259,
21.848589891905));
#61672=CARTESIAN_POINT('Origin',(0.,0.,-1.84858989190508));
#61673=CARTESIAN_POINT('',(-2.36785111718193,0.000293968609762033,19.651410108095));
#61674=CARTESIAN_POINT('',(-2.37121668396496,0.00214562610995388,19.848589891905));
#61675=CARTESIAN_POINT('',(-2.37175,1.07555357745099E-12,-1.84858989190508));
#61676=CARTESIAN_POINT('Ctrl Pts',(-2.36785111718192,0.000293968609762288,
19.651410108095));
#61677=CARTESIAN_POINT('Ctrl Pts',(-2.36739457070405,-0.414287432580937,
19.679123472331));
#61678=CARTESIAN_POINT('Ctrl Pts',(-2.065941122802,-1.62309576599104,19.7598867026983));
#61679=CARTESIAN_POINT('Ctrl Pts',(-0.135862993192047,-2.80226750533537,
19.8936997991968));
#61680=CARTESIAN_POINT('Ctrl Pts',(2.28456502325081,-1.62847308203622,20.0528493975903));
#61681=CARTESIAN_POINT('Ctrl Pts',(2.60470360644785,1.04243994883883,20.211998995984));
#61682=CARTESIAN_POINT('Ctrl Pts',(0.530236912192428,2.75499741221771,20.3711485943775));
#61683=CARTESIAN_POINT('Ctrl Pts',(-1.82759145210684,2.0001243501166,20.5176189650812));
#61684=CARTESIAN_POINT('Ctrl Pts',(-2.36605980865027,0.599327406656931,
20.6110394696537));
#61685=CARTESIAN_POINT('Ctrl Pts',(-2.37160301736592,-0.00219628840535644,
20.651410108095));
#61686=CARTESIAN_POINT('Ctrl Pts',(-2.37121668396496,0.00214562610995377,
19.848589891905));
#61687=CARTESIAN_POINT('Ctrl Pts',(-2.36597598747472,-0.584372248785578,
19.8879368923749));
#61688=CARTESIAN_POINT('Ctrl Pts',(-1.850360793774,-1.96697607918093,19.9801377076478));
#61689=CARTESIAN_POINT('Ctrl Pts',(0.466180705424317,-2.76300565564655,
20.1251923377236));
#61690=CARTESIAN_POINT('Ctrl Pts',(2.57274555864665,-1.11018241460974,20.2837537821323));
#61691=CARTESIAN_POINT('Ctrl Pts',(2.33006666709568,1.55637849835264,20.4423152265411));
#61692=CARTESIAN_POINT('Ctrl Pts',(-0.0402592916836527,2.80176799408478,
20.6008766709498));
#61693=CARTESIAN_POINT('Ctrl Pts',(-2.03332046845351,1.68037126807848,20.7363015594045));
#61694=CARTESIAN_POINT('Ctrl Pts',(-2.36680513132683,0.443646720139554,
20.8188726330562));
#61695=CARTESIAN_POINT('Ctrl Pts',(-2.3681294836508,-0.000785534163144468,
20.848589891905));
#61696=CARTESIAN_POINT('Origin',(0.,0.,-1.84858989190508));
#61697=CARTESIAN_POINT('',(-2.37268542712431,0.00210147159002048,18.651410108095));
#61698=CARTESIAN_POINT('',(-2.37534353148036,-0.000727847436731155,18.848589891905));
#61699=CARTESIAN_POINT('',(-2.37175,1.07555357745099E-12,-1.84858989190508));
#61700=CARTESIAN_POINT('Ctrl Pts',(-2.37268542712431,0.00210147159002057,
18.651410108095));
#61701=CARTESIAN_POINT('Ctrl Pts',(-2.36681038593963,-0.634092970239114,
18.6941576088772));
#61702=CARTESIAN_POINT('Ctrl Pts',(-1.77494844826955,-2.06944727531261,
18.7899549757907));
#61703=CARTESIAN_POINT('Ctrl Pts',(0.653095138640082,-2.7284846827978,18.9388022088353));
#61704=CARTESIAN_POINT('Ctrl Pts',(2.64877844972125,-0.924734907240888,
19.0979518072289));
#61705=CARTESIAN_POINT('Ctrl Pts',(2.20933676661749,1.7291596155502,19.2571014056225));
#61706=CARTESIAN_POINT('Ctrl Pts',(-0.261234089078342,2.79337048654149,
19.416251004016));
#61707=CARTESIAN_POINT('Ctrl Pts',(-2.10325227673128,1.55139759182543,19.5476872381736));
#61708=CARTESIAN_POINT('Ctrl Pts',(-2.36826850752845,0.379318412104361,
19.6260736061998));
#61709=CARTESIAN_POINT('Ctrl Pts',(-2.36785111718192,0.000293968609762288,
19.651410108095));
#61710=CARTESIAN_POINT('Ctrl Pts',(-2.37534353148036,-0.000727847436731129,
18.848589891905));
#61711=CARTESIAN_POINT('Ctrl Pts',(-2.37550564871799,-0.0408474181895097,
18.8512935220879));
#61712=CARTESIAN_POINT('Ctrl Pts',(-2.35642199299718,-0.865115184557848,
18.9068509670736));
#61713=CARTESIAN_POINT('Ctrl Pts',(-1.40094218755544,-2.42670263740165,
19.0152622268623));
#61714=CARTESIAN_POINT('Ctrl Pts',(1.27577326591705,-2.49478000577529,19.1738236712711));
#61715=CARTESIAN_POINT('Ctrl Pts',(2.7875455501625,-0.284806090198347,19.3323851156798));
#61716=CARTESIAN_POINT('Ctrl Pts',(1.75393439181258,2.18523199053596,19.4909465600886));
#61717=CARTESIAN_POINT('Ctrl Pts',(-0.88124182797927,2.65987547525528,19.6495080044973));
#61718=CARTESIAN_POINT('Ctrl Pts',(-2.25749629369168,1.19063929439144,19.7687224484361));
#61719=CARTESIAN_POINT('Ctrl Pts',(-2.37301568042272,0.203482143368676,
19.835083077572));
#61720=CARTESIAN_POINT('Ctrl Pts',(-2.37121668396496,0.00214562610995377,
19.848589891905));
#61721=CARTESIAN_POINT('Origin',(0.,0.,-1.84858989190508));
#61722=CARTESIAN_POINT('',(-2.37489284321081,-0.00123559705226072,17.651410108095));
#61723=CARTESIAN_POINT('',(-2.36912129924534,-0.00162542170875829,17.848589891905));
#61724=CARTESIAN_POINT('',(-2.37175,1.07555357745099E-12,-1.84858989190508));
#61725=CARTESIAN_POINT('Ctrl Pts',(-2.37489284321081,-0.00123559705226036,
17.651410108095));
#61726=CARTESIAN_POINT('Ctrl Pts',(-2.3753368409954,-0.0714864407096927,
17.6561418792922));
#61727=CARTESIAN_POINT('Ctrl Pts',(-2.34058824250688,-0.928903408008142,
17.7139235166207));
#61728=CARTESIAN_POINT('Ctrl Pts',(-1.29962352880245,-2.48639108101694,
17.8247550200804));
#61729=CARTESIAN_POINT('Ctrl Pts',(1.38995452278499,-2.43704500347595,17.9839046184738));
#61730=CARTESIAN_POINT('Ctrl Pts',(2.80169335019333,-0.147228719548932,
18.1430542168675));
#61731=CARTESIAN_POINT('Ctrl Pts',(1.63772657118694,2.27794064944762,18.302203815261));
#61732=CARTESIAN_POINT('Ctrl Pts',(-1.0318659076804,2.60891062954338,18.4613534136547));
#61733=CARTESIAN_POINT('Ctrl Pts',(-2.2905754966375,1.09673789523524,18.5777555112659));
#61734=CARTESIAN_POINT('Ctrl Pts',(-2.37410134196417,0.155427571425982,
18.641107742746));
#61735=CARTESIAN_POINT('Ctrl Pts',(-2.37268542712431,0.00210147159002057,
18.651410108095));
#61736=CARTESIAN_POINT('Ctrl Pts',(-2.36912129924534,-0.0016254217087585,
17.848589891905));
#61737=CARTESIAN_POINT('Ctrl Pts',(-2.37091015942674,-0.284195516689885,
17.8675039666037));
#61738=CARTESIAN_POINT('Ctrl Pts',(-2.19351504650125,-1.35421254674421,
17.9392718561053));
#61739=CARTESIAN_POINT('Ctrl Pts',(-0.606031153241877,-2.7357359054823,
18.0638935604098));
#61740=CARTESIAN_POINT('Ctrl Pts',(1.96717496328582,-1.9954316242523,18.2224550048186));
#61741=CARTESIAN_POINT('Ctrl Pts',(2.7441002692833,0.566955390982473,18.3810164492273));
#61742=CARTESIAN_POINT('Ctrl Pts',(1.01531319693132,2.61164006237112,18.5395778936361));
#61743=CARTESIAN_POINT('Ctrl Pts',(-1.59529820733317,2.27736397432732,18.6954357078619));
#61744=CARTESIAN_POINT('Ctrl Pts',(-2.37233638595852,0.743458207631327,
18.7984397072849));
#61745=CARTESIAN_POINT('Ctrl Pts',(-2.37534353148036,-0.000727847436731129,
18.848589891905));
#61746=CARTESIAN_POINT('Origin',(0.,0.,-1.84858989190508));
#61747=CARTESIAN_POINT('',(-2.36883928475605,-0.0015223826853693,16.651410108095));
#61748=CARTESIAN_POINT('',(-2.36951653941713,0.0018022559201944,16.848589891905));
#61749=CARTESIAN_POINT('',(-2.37175,1.07555357745099E-12,-1.84858989190508));
#61750=CARTESIAN_POINT('Ctrl Pts',(-2.36883928475605,-0.00152238268536945,
16.651410108095));
#61751=CARTESIAN_POINT('Ctrl Pts',(-2.37056689977668,-0.296904640803646,
16.6711760158384));
#61752=CARTESIAN_POINT('Ctrl Pts',(-2.18214828101389,-1.38294063098053,
16.743991789713));
#61753=CARTESIAN_POINT('Ctrl Pts',(-0.552569484305025,-2.75060518602588,
16.8698574297189));
#61754=CARTESIAN_POINT('Ctrl Pts',(2.01593436473937,-1.95119721233924,17.0290070281124));
#61755=CARTESIAN_POINT('Ctrl Pts',(2.73111138732539,0.642022207091869,17.188156626506));
#61756=CARTESIAN_POINT('Ctrl Pts',(0.935471545677604,2.64500565436165,17.3473062248996));
#61757=CARTESIAN_POINT('Ctrl Pts',(-1.64122679092401,2.22907771841236,17.5017240520959));
#61758=CARTESIAN_POINT('Ctrl Pts',(-2.37035899611375,0.716125152553366,
17.603092013161));
#61759=CARTESIAN_POINT('Ctrl Pts',(-2.37489284321081,-0.00123559705226036,
17.651410108095));
#61760=CARTESIAN_POINT('Ctrl Pts',(-2.36951653941713,0.00180225592019443,
16.848589891905));
#61761=CARTESIAN_POINT('Ctrl Pts',(-2.36579276584773,-0.522726350568018,
16.8837144111195));
#61762=CARTESIAN_POINT('Ctrl Pts',(-1.93551536846003,-1.84209105910571,
16.9716927451369));
#61763=CARTESIAN_POINT('Ctrl Pts',(0.245024140396729,-2.79132367773206,
17.1125248939573));
#61764=CARTESIAN_POINT('Ctrl Pts',(2.47633259500592,-1.31122140851802,17.271086338366));
#61765=CARTESIAN_POINT('Ctrl Pts',(2.44643459674846,1.3661926903175,17.4296477827748));
#61766=CARTESIAN_POINT('Ctrl Pts',(0.182630818693805,2.79609919124984,17.5882092271835));
#61767=CARTESIAN_POINT('Ctrl Pts',(-1.9580065820238,1.80680355351091,17.7278565968936));
#61768=CARTESIAN_POINT('Ctrl Pts',(-2.36591133784849,0.505423204125703,
17.8146501518008));
#61769=CARTESIAN_POINT('Ctrl Pts',(-2.36912129924534,-0.0016254217087585,
17.848589891905));
#61770=CARTESIAN_POINT('Origin',(0.,0.,-1.84858989190508));
#61771=CARTESIAN_POINT('',(-2.36932045623978,0.00177252062842899,15.651410108095));
#61772=CARTESIAN_POINT('',(-2.37552790433159,0.000415529653166168,15.848589891905));
#61773=CARTESIAN_POINT('',(-2.37175,1.07555357745099E-12,-1.84858989190508));
#61774=CARTESIAN_POINT('Ctrl Pts',(-2.36932045623978,0.00177252062842921,
15.651410108095));
#61775=CARTESIAN_POINT('Ctrl Pts',(-2.3657336259535,-0.518015199574277,
15.6862101523846));
#61776=CARTESIAN_POINT('Ctrl Pts',(-1.94098877146081,-1.83550765140878,
15.7740600628054));
#61777=CARTESIAN_POINT('Ctrl Pts',(0.238564168873022,-2.7953978360347,15.9149598393574));
#61778=CARTESIAN_POINT('Ctrl Pts',(2.48109896001892,-1.30969839084066,16.074109437751));
#61779=CARTESIAN_POINT('Ctrl Pts',(2.4426630300295,1.38005769665789,16.2332590361446));
#61780=CARTESIAN_POINT('Ctrl Pts',(0.158592023455111,2.80107309695302,16.3924086345381));
#61781=CARTESIAN_POINT('Ctrl Pts',(-1.96949605169442,1.79029139008163,16.5317923251883));
#61782=CARTESIAN_POINT('Ctrl Pts',(-2.36593014103228,0.495873988647358,
16.6181261497072));
#61783=CARTESIAN_POINT('Ctrl Pts',(-2.36883928475605,-0.00152238268536945,
16.651410108095));
#61784=CARTESIAN_POINT('Ctrl Pts',(-2.37552790433159,0.000415529653166134,
15.848589891905));
#61785=CARTESIAN_POINT('Ctrl Pts',(-2.37368024029323,-0.761193483430817,
15.8999248556353));
#61786=CARTESIAN_POINT('Ctrl Pts',(-1.56394205346637,-2.31032295076223,
16.0041136341686));
#61787=CARTESIAN_POINT('Ctrl Pts',(1.07337977774581,-2.5883161622899,16.1611562275048));
#61788=CARTESIAN_POINT('Ctrl Pts',(2.75607650988087,-0.505536324043674,
16.3197176719135));
#61789=CARTESIAN_POINT('Ctrl Pts',(1.92212503357044,2.03886244228653,16.4782791163223));
#61790=CARTESIAN_POINT('Ctrl Pts',(-0.666970940652513,2.72152061678207,
16.636840560731));
#61791=CARTESIAN_POINT('Ctrl Pts',(-2.20841342965836,1.31836001741498,16.7602774859253));
#61792=CARTESIAN_POINT('Ctrl Pts',(-2.37139613474805,0.26656097481449,16.8308605963166));
#61793=CARTESIAN_POINT('Ctrl Pts',(-2.36951653941713,0.00180225592019443,
16.848589891905));
#61794=CARTESIAN_POINT('Origin',(0.,0.,-1.84858989190508));
#61795=CARTESIAN_POINT('',(-2.37529741037155,0.000871252838594932,14.651410108095));
#61796=CARTESIAN_POINT('',(-2.37070442127403,-0.00209855721355318,14.848589891905));
#61797=CARTESIAN_POINT('',(-2.37175,1.07555357745099E-12,-1.84858989190508));
#61798=CARTESIAN_POINT('Ctrl Pts',(-2.37529741037155,0.000871252838595101,
14.651410108095));
#61799=CARTESIAN_POINT('Ctrl Pts',(-2.37181600276552,-0.73866462242614,
14.7012442889308));
#61800=CARTESIAN_POINT('Ctrl Pts',(-1.60226833365963,-2.27170433151576,
14.8041283358978));
#61801=CARTESIAN_POINT('Ctrl Pts',(1.01066706572481,-2.61719582886661,14.960062248996));
#61802=CARTESIAN_POINT('Ctrl Pts',(2.74834116840978,-0.563722224505545,
15.1192118473896));
#61803=CARTESIAN_POINT('Ctrl Pts',(1.95935839934075,2.00800313428798,15.2783614457831));
#61804=CARTESIAN_POINT('Ctrl Pts',(-0.630938711931175,2.73369315508602,
15.4375110441767));
#61805=CARTESIAN_POINT('Ctrl Pts',(-2.20162297148963,1.3370520367252,15.5618605982807));
#61806=CARTESIAN_POINT('Ctrl Pts',(-2.37120145998666,0.274359337190549,
15.6331602862534));
#61807=CARTESIAN_POINT('Ctrl Pts',(-2.36932045623978,0.00177252062842921,
15.651410108095));
#61808=CARTESIAN_POINT('Ctrl Pts',(-2.37070442127403,-0.00209855721355335,
14.848589891905));
#61809=CARTESIAN_POINT('Ctrl Pts',(-2.37258491227423,-0.221216123050188,
14.8632814853483));
#61810=CARTESIAN_POINT('Ctrl Pts',(-2.2443457179653,-1.22646135653919,14.9308268935944));
#61811=CARTESIAN_POINT('Ctrl Pts',(-0.821625189105414,-2.678890955577,15.0512261166435));
#61812=CARTESIAN_POINT('Ctrl Pts',(1.80229479678065,-2.14552048900545,15.2097875610522));
#61813=CARTESIAN_POINT('Ctrl Pts',(2.78049052387073,0.346982924521951,15.368349005461));
#61814=CARTESIAN_POINT('Ctrl Pts',(1.21974494421116,2.52264681917943,15.5269104498698));
#61815=CARTESIAN_POINT('Ctrl Pts',(-1.45478282458735,2.394813486794,15.6854718942785));
#61816=CARTESIAN_POINT('Ctrl Pts',(-2.36509470132286,0.82957372331575,15.7926983749569));
#61817=CARTESIAN_POINT('Ctrl Pts',(-2.37558257129349,0.0229493074598575,
15.8470710408324));
#61818=CARTESIAN_POINT('Ctrl Pts',(-2.37552790433159,0.000415529653166134,
15.848589891905));
#61819=CARTESIAN_POINT('Origin',(0.,0.,-1.84858989190508));
#61820=CARTESIAN_POINT('',(-2.3719949540914,-0.00218192237732729,13.651410108095));
#61821=CARTESIAN_POINT('',(-2.36833556860473,0.00104783714029014,13.848589891905));
#61822=CARTESIAN_POINT('',(-2.37175,1.07555357745099E-12,-1.84858989190508));
#61823=CARTESIAN_POINT('Ctrl Pts',(-2.3719949540914,-0.00218192237732709,
13.651410108095));
#61824=CARTESIAN_POINT('Ctrl Pts',(-2.37363184364254,-0.178202818064253,
13.6632285593458));
#61825=CARTESIAN_POINT('Ctrl Pts',(-2.27525263091362,-1.14252130340604,
13.7280968767278));
#61826=CARTESIAN_POINT('Ctrl Pts',(-0.956898470366649,-2.63732956639619,
13.846015060241));
#61827=CARTESIAN_POINT('Ctrl Pts',(1.70214696396934,-2.23021470657591,14.0051646586345));
#61828=CARTESIAN_POINT('Ctrl Pts',(2.79634252716041,0.227223227623548,14.1643142570281));
#61829=CARTESIAN_POINT('Ctrl Pts',(1.31975170355224,2.47576601587237,14.3234638554217));
#61830=CARTESIAN_POINT('Ctrl Pts',(-1.37013816353632,2.4482408658461,14.4826134538153));
#61831=CARTESIAN_POINT('Ctrl Pts',(-2.35254974335426,0.883348319972068,
14.591928871373));
#61832=CARTESIAN_POINT('Ctrl Pts',(-2.37552205761282,0.0485918052708133,
14.6481944227996));
#61833=CARTESIAN_POINT('Ctrl Pts',(-2.37529741037155,0.000871252838595101,
14.651410108095));
#61834=CARTESIAN_POINT('Ctrl Pts',(-2.36833556860473,0.0010478371402901,
13.848589891905));
#61835=CARTESIAN_POINT('Ctrl Pts',(-2.36648927158143,-0.461002671016135,
13.8794919298641));
#61836=CARTESIAN_POINT('Ctrl Pts',(-2.01294080374263,-1.71593888244227,
13.9632477826261));
#61837=CARTESIAN_POINT('Ctrl Pts',(0.022316198533973,-2.80196836001547,
14.099857450191));
#61838=CARTESIAN_POINT('Ctrl Pts',(2.36424066594685,-1.50395836934669,14.2584188945997));
#61839=CARTESIAN_POINT('Ctrl Pts',(2.5473128609508,1.16735679707592,14.4169803390085));
#61840=CARTESIAN_POINT('Ctrl Pts',(0.404364597205185,2.77272681232246,14.5755417834172));
#61841=CARTESIAN_POINT('Ctrl Pts',(-1.87505217600518,1.93208845330377,14.7194116343828));
#61842=CARTESIAN_POINT('Ctrl Pts',(-2.36581974255682,0.567071361866622,
14.8104276705453));
#61843=CARTESIAN_POINT('Ctrl Pts',(-2.37070442127403,-0.00209855721355335,
14.848589891905));
#61844=CARTESIAN_POINT('Origin',(0.,0.,-1.84858989190508));
#61845=CARTESIAN_POINT('',(-2.36782090892634,8.12663433023876E-5,12.651410108095));
#61846=CARTESIAN_POINT('',(-2.3745092207065,0.00142872646625845,12.848589891905));
#61847=CARTESIAN_POINT('',(-2.37175,1.07555357745099E-12,-1.84858989190508));
#61848=CARTESIAN_POINT('Ctrl Pts',(-2.36782090892634,8.126634330273E-5,
12.651410108095));
#61849=CARTESIAN_POINT('Ctrl Pts',(-2.3676987046513,-0.401636019150047,
12.6782626958919));
#61850=CARTESIAN_POINT('Ctrl Pts',(-2.07971230686784,-1.59714884508751,
12.7581651498201));
#61851=CARTESIAN_POINT('Ctrl Pts',(-0.181310616086829,-2.79969433775756,
12.8911174698795));
#61852=CARTESIAN_POINT('Ctrl Pts',(2.25784308439087,-1.66532475230686,13.0502670682731));
#61853=CARTESIAN_POINT('Ctrl Pts',(2.62127386877248,1.00004261372609,13.2094166666667));
#61854=CARTESIAN_POINT('Ctrl Pts',(0.574865689414601,2.74603193053384,13.3685662650602));
#61855=CARTESIAN_POINT('Ctrl Pts',(-1.80882641908756,2.02530207859848,13.515897412203));
#61856=CARTESIAN_POINT('Ctrl Pts',(-2.366284284329,0.611907895625466,13.6101786932146));
#61857=CARTESIAN_POINT('Ctrl Pts',(-2.3719949540914,-0.00218192237732709,
13.651410108095));
#61858=CARTESIAN_POINT('Ctrl Pts',(-2.3745092207065,0.00142872646625845,
12.848589891905));
#61859=CARTESIAN_POINT('Ctrl Pts',(-2.36952764776996,-0.698330449908164,
12.8957023743799));
#61860=CARTESIAN_POINT('Ctrl Pts',(-1.67258769039563,-2.19175214238388,
12.9956686716578));
#61861=CARTESIAN_POINT('Ctrl Pts',(0.864190157080086,-2.66546432646371,
13.1484887837385));
#61862=CARTESIAN_POINT('Ctrl Pts',(2.70715729817405,-0.723065741262676,
13.3070502281472));
#61863=CARTESIAN_POINT('Ctrl Pts',(2.07814568976501,1.87958378247841,13.465611672556));
#61864=CARTESIAN_POINT('Ctrl Pts',(-0.448477109148286,2.76593437843611,
13.6241731169647));
#61865=CARTESIAN_POINT('Ctrl Pts',(-2.15298049765028,1.44611826026627,13.7518325234144));
#61866=CARTESIAN_POINT('Ctrl Pts',(-2.3696471164158,0.329273103676635,13.8266381150612));
#61867=CARTESIAN_POINT('Ctrl Pts',(-2.36833556860473,0.0010478371402901,
13.848589891905));
#61868=CARTESIAN_POINT('Origin',(0.,0.,-1.84858989190508));
#61869=CARTESIAN_POINT('',(-2.37229421808997,0.00215578506045859,11.651410108095));
#61870=CARTESIAN_POINT('',(-2.37257814772649,-0.00207573294591201,11.848589891905));
#61871=CARTESIAN_POINT('',(-2.37175,1.07555357745099E-12,-1.84858989190508));
#61872=CARTESIAN_POINT('Ctrl Pts',(-2.37229421808997,0.00215578506045873,
11.651410108095));
#61873=CARTESIAN_POINT('Ctrl Pts',(-2.36649070893558,-0.621492334890488,
11.6932968324381));
#61874=CARTESIAN_POINT('Ctrl Pts',(-1.79431307440946,-2.04441564917251,
11.7882334229125));
#61875=CARTESIAN_POINT('Ctrl Pts',(0.608740760399282,-2.7387217111284,11.9362198795181));
#61876=CARTESIAN_POINT('Ctrl Pts',(2.63342640009004,-0.967588404067735,
12.0953694779116));
#61877=CARTESIAN_POINT('Ctrl Pts',(2.23710078159852,1.69308653569416,12.2545190763052));
#61878=CARTESIAN_POINT('Ctrl Pts',(-0.21587854772131,2.79724120822844,12.4136686746988));
#61879=CARTESIAN_POINT('Ctrl Pts',(-2.08999848010885,1.57738079894681,12.5459656852954));
#61880=CARTESIAN_POINT('Ctrl Pts',(-2.36794013093322,0.391995059504984,
12.6252128297608));
#61881=CARTESIAN_POINT('Ctrl Pts',(-2.36782090892634,8.126634330273E-5,
12.651410108095));
#61882=CARTESIAN_POINT('Ctrl Pts',(-2.37257814772649,-0.00207573294591234,
11.848589891905));
#61883=CARTESIAN_POINT('Ctrl Pts',(-2.3740036192897,-0.157902106076437,
11.8590590040928));
#61884=CARTESIAN_POINT('Ctrl Pts',(-2.28906614944607,-1.0988790069114,11.9223819310836));
#61885=CARTESIAN_POINT('Ctrl Pts',(-1.03201708332093,-2.60508453662804,
12.0385586728772));
#61886=CARTESIAN_POINT('Ctrl Pts',(1.6260033530305,-2.28202493395194,12.197120117286));
#61887=CARTESIAN_POINT('Ctrl Pts',(2.7992760290567,0.124813526483961,12.3556815616948));
#61888=CARTESIAN_POINT('Ctrl Pts',(1.41645384406812,2.41768137083226,12.5142430061035));
#61889=CARTESIAN_POINT('Ctrl Pts',(-1.25977076144102,2.50289878578082,12.6728044505123));
#61890=CARTESIAN_POINT('Ctrl Pts',(-2.33228417027533,0.956398728600941,
12.7842534124461));
#61891=CARTESIAN_POINT('Ctrl Pts',(-2.37511629688339,0.0867044277261085,
12.842848559577));
#61892=CARTESIAN_POINT('Ctrl Pts',(-2.3745092207065,0.00142872646625845,
12.848589891905));
#61893=CARTESIAN_POINT('Origin',(0.,0.,-1.84858989190508));
#61894=CARTESIAN_POINT('',(-2.37513726959577,-0.00103386453644136,10.651410108095));
#61895=CARTESIAN_POINT('',(-2.36788450901277,6.16867972168256E-5,10.848589891905));
#61896=CARTESIAN_POINT('',(-2.37175,1.07555357745099E-12,-1.84858989190508));
#61897=CARTESIAN_POINT('Ctrl Pts',(-2.37513726959577,-0.00103386453644157,
10.651410108095));
#61898=CARTESIAN_POINT('Ctrl Pts',(-2.37545044739491,-0.0584894452066465,
10.6552811028531));
#61899=CARTESIAN_POINT('Ctrl Pts',(-2.34746382585173,-0.903032024338962,
10.7122019637425));
#61900=CARTESIAN_POINT('Ctrl Pts',(-1.33979301969774,-2.46497800978969,
10.8221726907631));
#61901=CARTESIAN_POINT('Ctrl Pts',(1.35023162953112,-2.4592755988281,10.9813222891566));
#61902=CARTESIAN_POINT('Ctrl Pts',(2.79893585448806,-0.192665531008406,
11.1404718875502));
#61903=CARTESIAN_POINT('Ctrl Pts',(1.67446954602361,2.25106944891023,11.2996214859438));
#61904=CARTESIAN_POINT('Ctrl Pts',(-0.989401707370339,2.62530877914012,
11.4587710843374));
#61905=CARTESIAN_POINT('Ctrl Pts',(-2.2819681016055,1.12272726704564,11.5760339583877));
#61906=CARTESIAN_POINT('Ctrl Pts',(-2.37384089896737,0.168362918657281,
11.6402469663069));
#61907=CARTESIAN_POINT('Ctrl Pts',(-2.37229421808997,0.00215578506045873,
11.651410108095));
#61908=CARTESIAN_POINT('Ctrl Pts',(-2.36788450901277,6.16867972165827E-5,
10.848589891905));
#61909=CARTESIAN_POINT('Ctrl Pts',(-2.367791686282,-0.399043730343822,10.8752694486087));
#61910=CARTESIAN_POINT('Ctrl Pts',(-2.08295912267226,-1.58892555039052,
10.9548028201152));
#61911=CARTESIAN_POINT('Ctrl Pts',(-0.200533038930914,-2.79487230540894,
11.0871900064247));
#61912=CARTESIAN_POINT('Ctrl Pts',(2.23717948448735,-1.68717297792302,11.2457514508335));
#61913=CARTESIAN_POINT('Ctrl Pts',(2.63206274630088,0.961129753352717,11.4043128952422));
#61914=CARTESIAN_POINT('Ctrl Pts',(0.623538130558561,2.73179884013891,11.562874339651));
#61915=CARTESIAN_POINT('Ctrl Pts',(-1.78414908989376,2.05577833064682,11.7109666718719));
#61916=CARTESIAN_POINT('Ctrl Pts',(-2.36680705776116,0.628794809487644,
11.8062051892899));
#61917=CARTESIAN_POINT('Ctrl Pts',(-2.37257814772649,-0.00207573294591234,
11.848589891905));
#61918=CARTESIAN_POINT('Origin',(0.,0.,-1.84858989190508));
#61919=CARTESIAN_POINT('',(-2.36910288125725,-0.0016703647433169,9.65141010809496));
#61920=CARTESIAN_POINT('',(-2.37280337475969,0.00203709636048592,9.84858989190502));
#61921=CARTESIAN_POINT('',(-2.37175,1.07555357745099E-12,-1.84858989190508));
#61922=CARTESIAN_POINT('Ctrl Pts',(-2.36910288125725,-0.0016703647433166,
9.65141010809496));
#61923=CARTESIAN_POINT('Ctrl Pts',(-2.37092842223778,-0.284110306409195,
9.67031523939932));
#61924=CARTESIAN_POINT('Ctrl Pts',(-2.19330740190733,-1.35688708086049,
9.74227023683487));
#61925=CARTESIAN_POINT('Ctrl Pts',(-0.597124060110883,-2.74127794672745,
9.86727510040159));
#61926=CARTESIAN_POINT('Ctrl Pts',(1.98401173368511,-1.98364799422109,10.0264246987952));
#61927=CARTESIAN_POINT('Ctrl Pts',(2.74116841667201,0.597626669265515,10.1855742971888));
#61928=CARTESIAN_POINT('Ctrl Pts',(0.978262417402176,2.6294799042921,10.3447238955823));
#61929=CARTESIAN_POINT('Ctrl Pts',(-1.6192440991928,2.25332728858875,10.5000024992177));
#61930=CARTESIAN_POINT('Ctrl Pts',(-2.37115851693319,0.728907865680533,
10.6022312367219));
#61931=CARTESIAN_POINT('Ctrl Pts',(-2.37513726959577,-0.00103386453644157,
10.651410108095));
#61932=CARTESIAN_POINT('Ctrl Pts',(-2.37280337475968,0.00203709636048583,
9.84858989190502));
#61933=CARTESIAN_POINT('Ctrl Pts',(-2.36701047519887,-0.636198310368005,
9.8914798931245));
#61934=CARTESIAN_POINT('Ctrl Pts',(-1.77272462907463,-2.07044996200305,
9.9872237091469));
#61935=CARTESIAN_POINT('Ctrl Pts',(0.649528893544149,-2.72573603265175,
10.1358213399722));
#61936=CARTESIAN_POINT('Ctrl Pts',(2.64109764832668,-0.936017048588331,
10.294382784381));
#61937=CARTESIAN_POINT('Ctrl Pts',(2.22100851147896,1.70840448816513,10.4529442287897));
#61938=CARTESIAN_POINT('Ctrl Pts',(-0.22714373294823,2.79283555330906,10.6115056731985));
#61939=CARTESIAN_POINT('Ctrl Pts',(-2.09085765599782,1.57368542285565,10.7433875609036));
#61940=CARTESIAN_POINT('Ctrl Pts',(-2.36797557372347,0.391608229833928,
10.8224156338057));
#61941=CARTESIAN_POINT('Ctrl Pts',(-2.36788450901277,6.16867972165827E-5,
10.848589891905));
#61942=CARTESIAN_POINT('Origin',(0.,0.,-1.84858989190508));
#61943=CARTESIAN_POINT('',(-2.36903760879731,0.00163642073173795,8.65141010809496));
#61944=CARTESIAN_POINT('',(-2.37433059532467,-0.00152653879847225,8.84858989190501));
#61945=CARTESIAN_POINT('',(-2.37175,1.07555357745099E-12,-1.84858989190508));
#61946=CARTESIAN_POINT('Ctrl Pts',(-2.36903760879731,0.00163642073173823,
8.65141010809496));
#61947=CARTESIAN_POINT('Ctrl Pts',(-2.36583245845381,-0.505446425674836,
8.6853493759455));
#61948=CARTESIAN_POINT('Ctrl Pts',(-1.95729525761598,-1.80985376099157,
8.77233850992723));
#61949=CARTESIAN_POINT('Ctrl Pts',(0.19317871866267,-2.79890048180234,8.91237751004016));
#61950=CARTESIAN_POINT('Ctrl Pts',(2.4595231253557,-1.34978069337877,9.07152710843373));
#61951=CARTESIAN_POINT('Ctrl Pts',(2.46473231443179,1.34024495618274,9.23067670682731));
#61952=CARTESIAN_POINT('Ctrl Pts',(0.204017275877662,2.79813131849115,9.38982630522089));
#61953=CARTESIAN_POINT('Ctrl Pts',(-1.95343190101933,1.81598178609972,9.53007077231009));
#61954=CARTESIAN_POINT('Ctrl Pts',(-2.36580575458343,0.50844706091372,9.61726537326812));
#61955=CARTESIAN_POINT('Ctrl Pts',(-2.36910288125725,-0.0016703647433166,
9.65141010809496));
#61956=CARTESIAN_POINT('Ctrl Pts',(-2.37433059532467,-0.00152653879847217,
8.84858989190501));
#61957=CARTESIAN_POINT('Ctrl Pts',(-2.37502560197468,-0.094325735057865,
8.85483652283741));
#61958=CARTESIAN_POINT('Ctrl Pts',(-2.32799838253791,-0.971604165542515,
8.91393696857272));
#61959=CARTESIAN_POINT('Ctrl Pts',(-1.23587473403734,-2.51478395593197,
9.02589122911094));
#61960=CARTESIAN_POINT('Ctrl Pts',(1.43941682598108,-2.40408067758287,9.1844526735197));
#61961=CARTESIAN_POINT('Ctrl Pts',(2.8003378439175,-0.0981461317030541,
9.34301411792845));
#61962=CARTESIAN_POINT('Ctrl Pts',(1.60419442889238,2.29740830884616,9.5015755623372));
#61963=CARTESIAN_POINT('Ctrl Pts',(-1.05678242634981,2.59513691480873,9.66013700674596));
#61964=CARTESIAN_POINT('Ctrl Pts',(-2.29402384393756,1.08362978939683,9.77580844993522));
#61965=CARTESIAN_POINT('Ctrl Pts',(-2.37414912830807,0.150306120239738,
9.83862607832158));
#61966=CARTESIAN_POINT('Ctrl Pts',(-2.37280337475968,0.00203709636048583,
9.84858989190502));
#61967=CARTESIAN_POINT('Origin',(0.,0.,-1.84858989190508));
#61968=CARTESIAN_POINT('',(-2.37508229419387,0.00108330972966132,7.65141010809496));
#61969=CARTESIAN_POINT('',(-2.36824036561998,-0.000937958850331377,7.84858989190501));
#61970=CARTESIAN_POINT('',(-2.37175,1.07555357745099E-12,-1.84858989190508));
#61971=CARTESIAN_POINT('Ctrl Pts',(-2.37508229419387,0.00108330972966112,
7.65141010809496));
#61972=CARTESIAN_POINT('Ctrl Pts',(-2.3709611151748,-0.725853319007325,
7.70038351249169));
#61973=CARTESIAN_POINT('Ctrl Pts',(-1.62452387639323,-2.24755017347193,
7.8024067830196));
#61974=CARTESIAN_POINT('Ctrl Pts',(0.968071232182813,-2.63324894641536,
7.95747991967872));
#61975=CARTESIAN_POINT('Ctrl Pts',(2.73883327901741,-0.608238599666532,
8.11662951807229));
#61976=CARTESIAN_POINT('Ctrl Pts',(1.99167942641439,1.9759491356751,8.27577911646587));
#61977=CARTESIAN_POINT('Ctrl Pts',(-0.586502744988177,2.74357001997377,
8.43492871485943));
#61978=CARTESIAN_POINT('Ctrl Pts',(-2.19066818915132,1.36310617154104,8.56013904540247));
#61979=CARTESIAN_POINT('Ctrl Pts',(-2.37084237196762,0.287165755523453,
8.63229950981431));
#61980=CARTESIAN_POINT('Ctrl Pts',(-2.36903760879731,0.00163642073173823,
8.65141010809496));
#61981=CARTESIAN_POINT('Ctrl Pts',(-2.36824036561998,-0.000937958850331759,
7.84858989190501));
#61982=CARTESIAN_POINT('Ctrl Pts',(-2.3694385945702,-0.336752264496505,
7.87104696735324));
#61983=CARTESIAN_POINT('Ctrl Pts',(-2.14590544977689,-1.46139918005804,
7.94635785760438));
#61984=CARTESIAN_POINT('Ctrl Pts',(-0.422112596148098,-2.77008044277018,
8.07452256265844));
#61985=CARTESIAN_POINT('Ctrl Pts',(2.09595354186346,-1.85970520609983,8.23308400706718));
#61986=CARTESIAN_POINT('Ctrl Pts',(2.70014765665469,0.748817291137776,8.39164545147595));
#61987=CARTESIAN_POINT('Ctrl Pts',(0.838763715722044,2.67357441123917,8.55020689588469));
#61988=CARTESIAN_POINT('Ctrl Pts',(-1.68501465022418,2.17736829258185,8.70252170936105));
#61989=CARTESIAN_POINT('Ctrl Pts',(-2.36914503160584,0.690864167473078,
8.80198270803449));
#61990=CARTESIAN_POINT('Ctrl Pts',(-2.37433059532467,-0.00152653879847217,
8.84858989190501));
#61991=CARTESIAN_POINT('Origin',(0.,0.,-1.84858989190508));
#61992=CARTESIAN_POINT('',(-2.37238791048953,-0.00214487927112815,6.65141010809495));
#61993=CARTESIAN_POINT('',(-2.37092048416906,0.00212358946080196,6.84858989190502));
#61994=CARTESIAN_POINT('',(-2.37175,1.07555357745099E-12,-1.84858989190508));
#61995=CARTESIAN_POINT('Ctrl Pts',(-2.37238791048953,-0.00214487927112778,
6.65141010809496));
#61996=CARTESIAN_POINT('Ctrl Pts',(-2.37390455983555,-0.165276290284716,
6.66236778290668));
#61997=CARTESIAN_POINT('Ctrl Pts',(-2.28404464566905,-1.11652245665044,
6.72637532384959));
#61998=CARTESIAN_POINT('Ctrl Pts',(-0.999561980729776,-2.62145718466985,
6.84343273092369));
#61999=CARTESIAN_POINT('Ctrl Pts',(1.66573870468711,-2.25753770557323,7.00258232931727));
#62000=CARTESIAN_POINT('Ctrl Pts',(2.79966104700711,0.181823943001463,7.16173192771085));
#62001=CARTESIAN_POINT('Ctrl Pts',(1.35974615823274,2.45402777277456,7.32088152610442));
#62002=CARTESIAN_POINT('Ctrl Pts',(-1.33023623090505,2.47014847617812,7.48003112449799));
#62003=CARTESIAN_POINT('Ctrl Pts',(-2.34584281991666,0.909205872162835,
7.59020731849484));
#62004=CARTESIAN_POINT('Ctrl Pts',(-2.37542533402904,0.0615922612091321,
7.6473336463605));
#62005=CARTESIAN_POINT('Ctrl Pts',(-2.37508229419387,0.00108330972966112,
7.65141010809496));
#62006=CARTESIAN_POINT('Ctrl Pts',(-2.37092048416906,0.00212358946080219,
6.84858989190502));
#62007=CARTESIAN_POINT('Ctrl Pts',(-2.36587563233299,-0.574449067114922,
6.88725741186907));
#62008=CARTESIAN_POINT('Ctrl Pts',(-1.86459843703705,-1.94698367018192,
6.97877874663604));
#62009=CARTESIAN_POINT('Ctrl Pts',(0.430755120614024,-2.76874966894979,
7.12315389620592));
#62010=CARTESIAN_POINT('Ctrl Pts',(2.55831581876159,-1.14304193917764,7.28171534061469));
#62011=CARTESIAN_POINT('Ctrl Pts',(2.34980895897243,1.52640838558285,7.44027678502343));
#62012=CARTESIAN_POINT('Ctrl Pts',(-0.00437219018642784,2.80205381589964,
7.59883822943218));
#62013=CARTESIAN_POINT('Ctrl Pts',(-2.02170346853928,1.70077735243487,7.73494259839271));
#62014=CARTESIAN_POINT('Ctrl Pts',(-2.36661850469818,0.453602969412513,
7.81819315255032));
#62015=CARTESIAN_POINT('Ctrl Pts',(-2.36824036561998,-0.000937958850331759,
7.84858989190501));
#62016=CARTESIAN_POINT('Origin',(0.,0.,-1.84858989190508));
#62017=CARTESIAN_POINT('',(-2.36782500652722,-0.000132179022545951,5.65141010809495));
#62018=CARTESIAN_POINT('',(-2.37546058182015,-0.000550553819199384,5.84858989190501));
#62019=CARTESIAN_POINT('',(-2.37175,1.07555357745099E-12,-1.84858989190508));
#62020=CARTESIAN_POINT('Ctrl Pts',(-2.36782500652722,-0.000132179022545899,
5.65141010809495));
#62021=CARTESIAN_POINT('Ctrl Pts',(-2.36801741756233,-0.388970489593967,
5.67740191945286));
#62022=CARTESIAN_POINT('Ctrl Pts',(-2.09318863810404,-1.57118029724025,
5.75644359694196));
#62023=CARTESIAN_POINT('Ctrl Pts',(-0.226710508403585,-2.79638414202316,
5.88853514056225));
#62024=CARTESIAN_POINT('Ctrl Pts',(2.23052676138529,-1.70173802070743,6.04768473895582));
#62025=CARTESIAN_POINT('Ctrl Pts',(2.63715407267815,0.957382014315266,6.2068343373494));
#62026=CARTESIAN_POINT('Ctrl Pts',(0.619343131473575,2.7363435474871,6.36598393574298));
#62027=CARTESIAN_POINT('Ctrl Pts',(-1.78972184470636,2.05039854636853,6.51417585932482));
#62028=CARTESIAN_POINT('Ctrl Pts',(-2.366561939603,0.624498882346401,6.60931791677548));
#62029=CARTESIAN_POINT('Ctrl Pts',(-2.37238791048953,-0.00214487927112778,
6.65141010809496));
#62030=CARTESIAN_POINT('Ctrl Pts',(-2.37546058182015,-0.000550553819199696,
5.84858989190501));
#62031=CARTESIAN_POINT('Ctrl Pts',(-2.37555500637229,-0.0305832574876921,
5.85061404158198));
#62032=CARTESIAN_POINT('Ctrl Pts',(-2.36144599049303,-0.84472755400906,
5.90549200606186));
#62033=CARTESIAN_POINT('Ctrl Pts',(-1.43190741113937,-2.40856095400742,
6.01322378534467));
#62034=CARTESIAN_POINT('Ctrl Pts',(1.24371659317073,-2.5109149207244,6.17178522975341));
#62035=CARTESIAN_POINT('Ctrl Pts',(2.78366924554423,-0.320484375057478,
6.33034667416217));
#62036=CARTESIAN_POINT('Ctrl Pts',(1.7817780141982,2.16258914529891,6.48890811857092));
#62037=CARTESIAN_POINT('Ctrl Pts',(-0.847103045334166,2.67094386572056,
6.64746956297967));
#62038=CARTESIAN_POINT('Ctrl Pts',(-2.25001273100393,1.21118166807022,6.76736348742437));
#62039=CARTESIAN_POINT('Ctrl Pts',(-2.37277133355458,0.213655896415416,
6.83440359706615));
#62040=CARTESIAN_POINT('Ctrl Pts',(-2.37092048416906,0.00212358946080219,
6.84858989190502));
#62041=CARTESIAN_POINT('Origin',(0.,0.,-1.84858989190508));
#62042=CARTESIAN_POINT('',(-2.37190116809107,0.00218740778883247,4.65141010809495));
#62043=CARTESIAN_POINT('',(-2.36934253286443,-0.00173065431709335,4.84858989190501));
#62044=CARTESIAN_POINT('',(-2.37175,1.07555357745099E-12,-1.84858989190508));
#62045=CARTESIAN_POINT('Ctrl Pts',(-2.37190116809107,0.00218740778883234,
4.65141010809495));
#62046=CARTESIAN_POINT('Ctrl Pts',(-2.36622595650251,-0.608904074897115,
4.69243605599904));
#62047=CARTESIAN_POINT('Ctrl Pts',(-1.81333638750516,-2.01929938386188,
4.78651187003434));
#62048=CARTESIAN_POINT('Ctrl Pts',(0.564226129275921,-2.74823776254792,
4.9336375502008));
#62049=CARTESIAN_POINT('Ctrl Pts',(2.61738109284993,-1.01018718025988,5.09278714859438));
#62050=CARTESIAN_POINT('Ctrl Pts',(2.26427587290829,1.65656774558932,5.25193674698795));
#62051=CARTESIAN_POINT('Ctrl Pts',(-0.170466175671311,2.80037554755443,
5.41108634538153));
#62052=CARTESIAN_POINT('Ctrl Pts',(-2.07645202982422,1.60334443212033,5.54424413241719));
#62053=CARTESIAN_POINT('Ctrl Pts',(-2.36762470235237,0.404657166379961,
5.62435205332167));
#62054=CARTESIAN_POINT('Ctrl Pts',(-2.36782500652722,-0.000132179022545899,
5.65141010809495));
#62055=CARTESIAN_POINT('Ctrl Pts',(-2.36934253286443,-0.00173065431709328,
4.84858989190501));
#62056=CARTESIAN_POINT('Ctrl Pts',(-2.37118989843079,-0.274085561974275,
4.86682448609781));
#62057=CARTESIAN_POINT('Ctrl Pts',(-2.20212096045125,-1.33365068797172,
4.93791289509353));
#62058=CARTESIAN_POINT('Ctrl Pts',(-0.641019536282537,-2.72774974243608,
5.06185511889216));
#62059=CARTESIAN_POINT('Ctrl Pts',(1.94145701387202,-2.02046266150336,5.2204165633009));
#62060=CARTESIAN_POINT('Ctrl Pts',(2.75113651059875,0.531763672408809,5.37897800770967));
#62061=CARTESIAN_POINT('Ctrl Pts',(1.04867864620236,2.59842217513736,5.5375394521184));
#62062=CARTESIAN_POINT('Ctrl Pts',(-1.57739889422249,2.29629762498076,5.69407674685021));
#62063=CARTESIAN_POINT('Ctrl Pts',(-2.37308942892567,0.753619104515225,
5.79776022677906));
#62064=CARTESIAN_POINT('Ctrl Pts',(-2.37546058182015,-0.000550553819199696,
5.84858989190501));
#62065=CARTESIAN_POINT('Origin',(0.,0.,-1.84858989190508));
#62066=CARTESIAN_POINT('',(-2.37534261640908,-0.000818844704635749,3.65141010809495));
#62067=CARTESIAN_POINT('',(-2.36928439194487,0.0017046354039639,3.84858989190501));
#62068=CARTESIAN_POINT('',(-2.37175,1.07555357745099E-12,-1.84858989190508));
#62069=CARTESIAN_POINT('Ctrl Pts',(-2.37534261640908,-0.000818844704635778,
3.65141010809495));
#62070=CARTESIAN_POINT('Ctrl Pts',(-2.37554183260228,-0.045488019799339,
3.65442032641404));
#62071=CARTESIAN_POINT('Ctrl Pts',(-2.35411815018044,-0.877178853768313,
3.71048041086432));
#62072=CARTESIAN_POINT('Ctrl Pts',(-1.37960980571773,-2.44291602421381,
3.81959036144579));
#62073=CARTESIAN_POINT('Ctrl Pts',(1.31015328351832,-2.48085878298404,3.97873995983935));
#62074=CARTESIAN_POINT('Ctrl Pts',(2.79544153036393,-0.238051622317477,
4.13788955823294));
#62075=CARTESIAN_POINT('Ctrl Pts',(1.71077171156123,2.22360564722096,4.2970391566265));
#62076=CARTESIAN_POINT('Ctrl Pts',(-0.946677043995799,2.64101580821315,
4.45618875502009));
#62077=CARTESIAN_POINT('Ctrl Pts',(-2.27311787854369,1.14872896002257,4.57431240550956));
#62078=CARTESIAN_POINT('Ctrl Pts',(-2.37356446372587,0.181286597264478,
4.63938618986785));
#62079=CARTESIAN_POINT('Ctrl Pts',(-2.37190116809107,0.00218740778883234,
4.65141010809495));
#62080=CARTESIAN_POINT('Ctrl Pts',(-2.36928439194487,0.00170463540396366,
3.84858989190501));
#62081=CARTESIAN_POINT('Ctrl Pts',(-2.36585269261901,-0.512803915466465,
3.88303493061364));
#62082=CARTESIAN_POINT('Ctrl Pts',(-1.94848825283823,-1.82186493092716,
3.97033378412518));
#62083=CARTESIAN_POINT('Ctrl Pts',(0.20925401019493,-2.79423289347191,4.11048645243965));
#62084=CARTESIAN_POINT('Ctrl Pts',(2.45933594484265,-1.34282962940415,4.2690478968484));
#62085=CARTESIAN_POINT('Ctrl Pts',(2.46373152879142,1.33474778785059,4.42760934125715));
#62086=CARTESIAN_POINT('Ctrl Pts',(0.218427035218096,2.79353080054729,4.58617078566591));
#62087=CARTESIAN_POINT('Ctrl Pts',(-1.94518171864127,1.82705282789237,4.72649763588185));
#62088=CARTESIAN_POINT('Ctrl Pts',(-2.36583522387729,0.515347737049405,
4.81397067129489));
#62089=CARTESIAN_POINT('Ctrl Pts',(-2.36934253286443,-0.00173065431709328,
4.84858989190501));
#62090=CARTESIAN_POINT('Origin',(0.,0.,-1.84858989190508));
#62091=CARTESIAN_POINT('',(-2.36939151225074,-0.00180255051221435,2.65141010809495));
#62092=CARTESIAN_POINT('',(-2.37543340018105,0.000596509793510114,2.84858989190501));
#62093=CARTESIAN_POINT('',(-2.37175,1.07555357745099E-12,-1.84858989190508));
#62094=CARTESIAN_POINT('Ctrl Pts',(-2.36939151225074,-0.00180255051221455,
2.65141010809495));
#62095=CARTESIAN_POINT('Ctrl Pts',(-2.37128654501027,-0.271300123974492,
2.66945446296022));
#62096=CARTESIAN_POINT('Ctrl Pts',(-2.2041984741782,-1.33083306058644,2.74054868395668));
#62097=CARTESIAN_POINT('Ctrl Pts',(-0.641521429760122,-2.73122899507208,
2.86469277108434));
#62098=CARTESIAN_POINT('Ctrl Pts',(1.95156679945169,-2.01557660741595,3.02384236947791));
#62099=CARTESIAN_POINT('Ctrl Pts',(2.75050382812508,0.553073821547345,3.18299196787149));
#62100=CARTESIAN_POINT('Ctrl Pts',(1.02079575688963,2.61326192654012,3.34214156626506));
#62101=CARTESIAN_POINT('Ctrl Pts',(-1.59690279772098,2.27745090552783,3.49828094633955));
#62102=CARTESIAN_POINT('Ctrl Pts',(-2.37203099343379,0.741728556467104,
3.60137046028285));
#62103=CARTESIAN_POINT('Ctrl Pts',(-2.37534261640908,-0.000818844704635778,
3.65141010809495));
#62104=CARTESIAN_POINT('Ctrl Pts',(-2.37543340018105,0.000596509793510109,
2.84858989190501));
#62105=CARTESIAN_POINT('Ctrl Pts',(-2.37289189110074,-0.75101179482527,
2.89924537512947));
#62106=CARTESIAN_POINT('Ctrl Pts',(-1.58200873350162,-2.29145202362107,
3.00275467315685));
#62107=CARTESIAN_POINT('Ctrl Pts',(1.04014173421655,-2.60185124395797,3.15911778598714));
#62108=CARTESIAN_POINT('Ctrl Pts',(2.74937577244265,-0.540793460784857,
3.31767923039589));
#62109=CARTESIAN_POINT('Ctrl Pts',(1.94808022437453,2.01407749008101,3.47624067480464));
#62110=CARTESIAN_POINT('Ctrl Pts',(-0.632060208719933,2.72983966543523,
3.6348021192134));
#62111=CARTESIAN_POINT('Ctrl Pts',(-2.19993069937822,1.33892162353352,3.75891852491352));
#62112=CARTESIAN_POINT('Ctrl Pts',(-2.37111842630456,0.276678131346021,
3.83018111581072));
#62113=CARTESIAN_POINT('Ctrl Pts',(-2.36928439194487,0.00170463540396366,
3.84858989190501));
#62114=CARTESIAN_POINT('Origin',(0.,0.,-1.84858989190508));
#62115=CARTESIAN_POINT('',(-2.36877975033525,0.00148782749813889,1.65141010809495));
#62116=CARTESIAN_POINT('',(-2.37099583443225,-0.00213048971222318,1.84858989190501));
#62117=CARTESIAN_POINT('',(-2.37175,1.07555357745099E-12,-1.84858989190508));
#62118=CARTESIAN_POINT('Ctrl Pts',(-2.36877975033525,0.00148782749813899,
1.65141010809495));
#62119=CARTESIAN_POINT('Ctrl Pts',(-2.36596424764654,-0.492870032272385,
1.68448859950641));
#62120=CARTESIAN_POINT('Ctrl Pts',(-1.97328459846742,-1.78415699276091,
1.77061695704905));
#62121=CARTESIAN_POINT('Ctrl Pts',(0.147742963738231,-2.80166329463351,
1.90979518072289));
#62122=CARTESIAN_POINT('Ctrl Pts',(2.43729952527864,-1.38950924165797,2.06894477911646));
#62123=CARTESIAN_POINT('Ctrl Pts',(2.48615290161395,1.30008022007748,2.22809437751004));
#62124=CARTESIAN_POINT('Ctrl Pts',(0.249388740897356,2.79445248935483,2.38724397590361));
#62125=CARTESIAN_POINT('Ctrl Pts',(-1.93704908267542,1.8416239542747,2.52834921943192));
#62126=CARTESIAN_POINT('Ctrl Pts',(-2.36571520511157,0.521014719177456,
2.61640459682903));
#62127=CARTESIAN_POINT('Ctrl Pts',(-2.36939151225074,-0.00180255051221455,
2.65141010809495));
#62128=CARTESIAN_POINT('Ctrl Pts',(-2.37099583443225,-0.00213048971222356,
1.84858989190501));
#62129=CARTESIAN_POINT('Ctrl Pts',(-2.37283470856056,-0.211048770807267,
1.86260200484238));
#62130=CARTESIAN_POINT('Ctrl Pts',(-2.25194621232616,-1.20591570523556,
1.92946793258267));
#62131=CARTESIAN_POINT('Ctrl Pts',(-0.855867697802383,-2.66814781527329,
2.04918767512588));
#62132=CARTESIAN_POINT('Ctrl Pts',(1.77466802262196,-2.16842771739956,2.20774911953463));
#62133=CARTESIAN_POINT('Ctrl Pts',(2.78470651107863,0.311343289720562,2.36631056394338));
#62134=CARTESIAN_POINT('Ctrl Pts',(1.25195381897505,2.50681790160282,2.52487200835213));
#62135=CARTESIAN_POINT('Ctrl Pts',(-1.42399178516171,2.41324930660116,2.68343345276089));
#62136=CARTESIAN_POINT('Ctrl Pts',(-2.36017099633076,0.849952732330805,
2.79133941394518));
#62137=CARTESIAN_POINT('Ctrl Pts',(-2.37554369583539,0.0332145832082634,
2.84639156032655));
#62138=CARTESIAN_POINT('Ctrl Pts',(-2.37543340018105,0.000596509793510109,
2.84858989190501));
#62139=CARTESIAN_POINT('Origin',(0.,0.,-1.84858989190508));
#62140=CARTESIAN_POINT('',(-2.37479956011642,0.00144393851757992,0.651410108094952));
#62141=CARTESIAN_POINT('',(-2.36820388529326,0.000916507492466495,0.848589891905012));
#62142=CARTESIAN_POINT('',(-2.37175,1.07555357745099E-12,-1.84858989190508));
#62143=CARTESIAN_POINT('Ctrl Pts',(-2.37479956011642,0.00144393851757997,
0.651410108094952));
#62144=CARTESIAN_POINT('Ctrl Pts',(-2.37014002571856,-0.712866861030972,
0.699522736052592));
#62145=CARTESIAN_POINT('Ctrl Pts',(-1.64646945403367,-2.22353554076285,
0.800685230141422));
#62146=CARTESIAN_POINT('Ctrl Pts',(0.92524708272242,-2.64846350983462,0.954897590361446));
#62147=CARTESIAN_POINT('Ctrl Pts',(2.72859047663099,-0.652671033011881,
1.11404718875502));
#62148=CARTESIAN_POINT('Ctrl Pts',(2.02348342694992,1.94341489122264,1.27319678714859));
#62149=CARTESIAN_POINT('Ctrl Pts',(-0.541916200030843,2.75270370291815,
1.43234638554217));
#62150=CARTESIAN_POINT('Ctrl Pts',(-2.17944386261456,1.38916365493018,1.55841749252429));
#62151=CARTESIAN_POINT('Ctrl Pts',(-2.37047963013088,0.299959905330106,
1.63143873337521));
#62152=CARTESIAN_POINT('Ctrl Pts',(-2.36877975033525,0.00148782749813899,
1.65141010809495));
#62153=CARTESIAN_POINT('Ctrl Pts',(-2.36820388529326,0.000916507492466252,
0.848589891905012));
#62154=CARTESIAN_POINT('Ctrl Pts',(-2.36666168705901,-0.451042231517807,
0.878812449358213));
#62155=CARTESIAN_POINT('Ctrl Pts',(-2.02471011777409,-1.69557760792411,
0.961888821614331));
#62156=CARTESIAN_POINT('Ctrl Pts',(-0.0135649315166644,-2.80200471609095,
1.09781900867337));
#62157=CARTESIAN_POINT('Ctrl Pts',(2.34478101694196,-1.53412545281777,1.25638045308212));
#62158=CARTESIAN_POINT('Ctrl Pts',(2.56205685808127,1.13464159452892,1.41494189749087));
#62159=CARTESIAN_POINT('Ctrl Pts',(0.439842266833678,2.76731764321101,1.57350334189962));
#62160=CARTESIAN_POINT('Ctrl Pts',(-1.86096804286685,1.95211388693732,1.718052673371));
#62161=CARTESIAN_POINT('Ctrl Pts',(-2.36589845897007,0.576992846277577,
1.80974819003947));
#62162=CARTESIAN_POINT('Ctrl Pts',(-2.37099583443225,-0.00213048971222356,
1.84858989190501));
#62163=CARTESIAN_POINT('Origin',(0.,0.,39.5));
#62164=CARTESIAN_POINT('',(-2.86973666310952,0.00133538653572275,39.1339652973708));
#62165=CARTESIAN_POINT('Ctrl Pts',(-0.439445221993938,2.33068358199192,
39.62825));
#62166=CARTESIAN_POINT('Ctrl Pts',(-0.35949827194111,2.34930793730339,39.6247609417367));
#62167=CARTESIAN_POINT('Ctrl Pts',(-0.278745636135806,2.3634061787771,39.6212861115939));
#62168=CARTESIAN_POINT('Ctrl Pts',(-0.197512062256915,2.37316448853009,
39.6178207830088));
#62169=CARTESIAN_POINT('Ctrl Pts',(-0.114123930084006,2.38318161795837,
39.6142635435044));
#62170=CARTESIAN_POINT('Ctrl Pts',(-0.0302282552652829,2.38862557677138,
39.6107163162615));
#62171=CARTESIAN_POINT('Ctrl Pts',(0.0538390324598612,2.38964547677812,
39.6071739885661));
#62172=CARTESIAN_POINT('Ctrl Pts',(0.0937642650950609,2.39012984764502,
39.6054916664508));
#62173=CARTESIAN_POINT('Ctrl Pts',(0.133728353022446,2.38961562430752,39.6038104494234));
#62174=CARTESIAN_POINT('Ctrl Pts',(0.173695695523468,2.3881147884205,39.6021297898218));
#62175=CARTESIAN_POINT('Ctrl Pts',(0.19786577786694,2.38720716422776,39.6011134179937));
#62176=CARTESIAN_POINT('Ctrl Pts',(0.222037051875367,2.38593866964451,39.6000972500259));
#62177=CARTESIAN_POINT('Ctrl Pts',(0.246201620501372,2.38431151277149,39.5990811647941));
#62178=CARTESIAN_POINT('Ctrl Pts',(0.262023069244234,2.38324615218255,39.598415895711));
#62179=CARTESIAN_POINT('Ctrl Pts',(0.27784241249069,2.38202687571003,39.5977506295992));
#62180=CARTESIAN_POINT('Ctrl Pts',(0.293641126549649,2.38065591301966,39.5970860183969));
#62181=CARTESIAN_POINT('Ctrl Pts',(0.379384271840456,2.37321539268935,39.5934790251521));
#62182=CARTESIAN_POINT('Ctrl Pts',(0.46463251786987,2.36130457094966,39.5898865577667));
#62183=CARTESIAN_POINT('Ctrl Pts',(0.549033644812378,2.34508734810305,39.5863033810857));
#62184=CARTESIAN_POINT('Ctrl Pts',(0.634178650960569,2.32872719286576,39.5826886236578));
#62185=CARTESIAN_POINT('Ctrl Pts',(0.718462490380905,2.30798424275509,39.5790833214255));
#62186=CARTESIAN_POINT('Ctrl Pts',(0.801522760414795,2.28297369408067,39.5754820995882));
#62187=CARTESIAN_POINT('Ctrl Pts',(0.853315250286197,2.26737828861944,39.5732365465042));
#62188=CARTESIAN_POINT('Ctrl Pts',(0.904631926849359,2.25012252017408,39.5709925799533));
#62189=CARTESIAN_POINT('Ctrl Pts',(0.955382243535092,2.23122440392206,39.5687488968205));
#62190=CARTESIAN_POINT('Ctrl Pts',(0.967602035670815,2.226674066753,39.5682086570094));
#62191=CARTESIAN_POINT('Ctrl Pts',(0.979786008270006,2.22202953927781,39.5676685642798));
#62192=CARTESIAN_POINT('Ctrl Pts',(0.991925279191415,2.21729426385562,39.5671289419076));
#62193=CARTESIAN_POINT('Ctrl Pts',(1.07366759536826,2.18540829778312,39.5634952819579));
#62194=CARTESIAN_POINT('Ctrl Pts',(1.15348638596816,2.14937373494847,39.5598783986484));
#62195=CARTESIAN_POINT('Ctrl Pts',(1.23102268640763,2.10933916676248,39.5562729770003));
#62196=CARTESIAN_POINT('Ctrl Pts',(1.30816316025863,2.06950897699608,39.5526859612052));
#62197=CARTESIAN_POINT('Ctrl Pts',(1.38304533569878,2.02571923323226,39.5491102903455));
#62198=CARTESIAN_POINT('Ctrl Pts',(1.45530281679409,1.97806672561256,39.545540730427));
#62199=CARTESIAN_POINT('Ctrl Pts',(1.51549908373607,1.938368371537,39.5425670012233));
#62200=CARTESIAN_POINT('Ctrl Pts',(1.57387380072491,1.89598823770892,39.5395975131496));
#62201=CARTESIAN_POINT('Ctrl Pts',(1.63020107000193,1.85095785631656,39.5366292400351));
#62202=CARTESIAN_POINT('Ctrl Pts',(1.65836470464044,1.82844266562037,39.5351451034778));
#62203=CARTESIAN_POINT('Ctrl Pts',(1.68601623605506,1.80526457576384,39.5336612706603));
#62204=CARTESIAN_POINT('Ctrl Pts',(1.71312572787294,1.78142555846922,39.5321773633112));
#62205=CARTESIAN_POINT('Ctrl Pts',(1.72751481855975,1.76877235994964,39.531389739642));
#62206=CARTESIAN_POINT('Ctrl Pts',(1.74175118247484,1.75593294056428,39.5306020949754));
#62207=CARTESIAN_POINT('Ctrl Pts',(1.75583018857345,1.74290745007241,39.5298143727475));
#62208=CARTESIAN_POINT('Ctrl Pts',(1.76643953526031,1.73309198842499,39.5292207784164));
#62209=CARTESIAN_POINT('Ctrl Pts',(1.77695982507892,1.72317043557429,39.528627119114));
#62210=CARTESIAN_POINT('Ctrl Pts',(1.7873768489527,1.71315495102162,39.5280340756501));
#62211=CARTESIAN_POINT('Ctrl Pts',(1.78918047975628,1.71142084378803,39.5279313945511));
#62212=CARTESIAN_POINT('Ctrl Pts',(1.79098110660068,1.70968383682676,39.5278287268096));
#62213=CARTESIAN_POINT('Ctrl Pts',(1.79277872129701,1.70794393308359,39.5277260723057));
#62214=CARTESIAN_POINT('Ctrl Pts',(1.85277206005579,1.64987663151762,39.5243000954034));
#62215=CARTESIAN_POINT('Ctrl Pts',(1.90941274940707,1.58858667736653,39.520888862746));
#62216=CARTESIAN_POINT('Ctrl Pts',(1.96268106277255,1.52446609117959,39.5174879201237));
#62217=CARTESIAN_POINT('Ctrl Pts',(2.01751082142157,1.45846594882589,39.5139872862313));
#62218=CARTESIAN_POINT('Ctrl Pts',(2.06876803124024,1.38946620854916,39.5104975544758));
#62219=CARTESIAN_POINT('Ctrl Pts',(2.11639781840586,1.31785082822935,39.5070138673568));
#62220=CARTESIAN_POINT('Ctrl Pts',(2.16250504721347,1.24852474211716,39.5036415415783));
#62221=CARTESIAN_POINT('Ctrl Pts',(2.20521314151012,1.17674668031166,39.5002748801611));
#62222=CARTESIAN_POINT('Ctrl Pts',(2.24443824676613,1.10283631226475,39.4969094767047));
#62223=CARTESIAN_POINT('Ctrl Pts',(2.26159923031564,1.07050052624423,39.4954371126925));
#62224=CARTESIAN_POINT('Ctrl Pts',(2.27809309201077,1.03775630392964,39.4939649894619));
#62225=CARTESIAN_POINT('Ctrl Pts',(2.29391059165361,1.00462924829656,39.4924927380198));
#62226=CARTESIAN_POINT('Ctrl Pts',(2.30309923797525,0.985385195521925,39.4916374828845));
#62227=CARTESIAN_POINT('Ctrl Pts',(2.31205961051446,0.966011939145637,39.4907821844824));
#62228=CARTESIAN_POINT('Ctrl Pts',(2.32078967559046,0.946514421244772,39.4899267704768));
#62229=CARTESIAN_POINT('Ctrl Pts',(2.32610779088639,0.934637070127862,39.4894056758151));
#62230=CARTESIAN_POINT('Ctrl Pts',(2.33133644269386,0.922722526711712,39.4888849296127));
#62231=CARTESIAN_POINT('Ctrl Pts',(2.33647546709348,0.91077224977599,39.4883645221385));
#62232=CARTESIAN_POINT('Ctrl Pts',(2.37171749020212,0.828820520581163,39.4847957100827));
#62233=CARTESIAN_POINT('Ctrl Pts',(2.40274873420275,0.745189063562941,39.4812427358572));
#62234=CARTESIAN_POINT('Ctrl Pts',(2.42951278311371,0.660283828018607,39.4777005656353));
#62235=CARTESIAN_POINT('Ctrl Pts',(2.45657092467005,0.574445624319474,39.4741194728193));
#62236=CARTESIAN_POINT('Ctrl Pts',(2.47926798471156,0.487304592098544,39.4705494227476));
#62237=CARTESIAN_POINT('Ctrl Pts',(2.4975005543187,0.399252281737089,39.466985213823));
#62238=CARTESIAN_POINT('Ctrl Pts',(2.51456467077104,0.316842895112961,39.4636494209282));
#62239=CARTESIAN_POINT('Ctrl Pts',(2.52771800895694,0.233634393127452,39.4603187444982));
#62240=CARTESIAN_POINT('Ctrl Pts',(2.53683582034357,0.149936742873024,39.456988920265));
#62241=CARTESIAN_POINT('Ctrl Pts',(2.54025499961356,0.118550124027614,39.4557402361776));
#62242=CARTESIAN_POINT('Ctrl Pts',(2.54310627315112,0.0870946671010823,
39.4544916719303));
#62243=CARTESIAN_POINT('Ctrl Pts',(2.54538154276705,0.0555866479532388,
39.4532430026497));
#62244=CARTESIAN_POINT('Ctrl Pts',(2.54664021905131,0.038156451466729,39.4525522403772));
#62245=CARTESIAN_POINT('Ctrl Pts',(2.54772260641032,0.0207101698921403,
39.4518614459615));
#62246=CARTESIAN_POINT('Ctrl Pts',(2.54862721938394,0.00325056775144827,
39.4511705813326));
#62247=CARTESIAN_POINT('Ctrl Pts',(2.54933098872424,-0.010332625325178,
39.4506331035844));
#62248=CARTESIAN_POINT('Ctrl Pts',(2.5499270655201,-0.0239235062956236,
39.4500955982875));
#62249=CARTESIAN_POINT('Ctrl Pts',(2.55041445808122,-0.0375069511551507,
39.4495585933208));
#62250=CARTESIAN_POINT('Ctrl Pts',(2.55382119554076,-0.132451425329508,
39.4458050790458));
#62251=CARTESIAN_POINT('Ctrl Pts',(2.55193263779309,-0.227203514255775,
39.4420691827466));
#62252=CARTESIAN_POINT('Ctrl Pts',(2.54463766231788,-0.321313299306112,
39.438345057077));
#62253=CARTESIAN_POINT('Ctrl Pts',(2.53776293446409,-0.410001624962419,
39.4348354701623));
#62254=CARTESIAN_POINT('Ctrl Pts',(2.52608656691972,-0.49812058693239,39.4313363367793));
#62255=CARTESIAN_POINT('Ctrl Pts',(2.50946448834332,-0.58530043370155,39.4278427630424));
#62256=CARTESIAN_POINT('Ctrl Pts',(2.50844839154163,-0.590629680766924,
39.4276292031627));
#62257=CARTESIAN_POINT('Ctrl Pts',(2.50741379735189,-0.595955417977466,
39.4274156640583));
#62258=CARTESIAN_POINT('Ctrl Pts',(2.50636066643785,-0.601277560448006,
39.4272021446113));
#62259=CARTESIAN_POINT('Ctrl Pts',(2.48918927936352,-0.688055535729271,
39.4237206922828));
#62260=CARTESIAN_POINT('Ctrl Pts',(2.46709408631404,-0.773878867566709,
39.4202444659784));
#62261=CARTESIAN_POINT('Ctrl Pts',(2.44034445210713,-0.858488994856188,
39.4167686198238));
#62262=CARTESIAN_POINT('Ctrl Pts',(2.42991429939784,-0.891479971164706,
39.4154133262932));
#62263=CARTESIAN_POINT('Ctrl Pts',(2.4187759588216,-0.924286351580536,39.414058090559));
#62264=CARTESIAN_POINT('Ctrl Pts',(2.40694340479929,-0.956892111550784,
39.4127026253509));
#62265=CARTESIAN_POINT('Ctrl Pts',(2.40229670837332,-0.969696538053649,
39.412170328154));
#62266=CARTESIAN_POINT('Ctrl Pts',(2.3975419341509,-0.982472644162397,39.4116378858603));
#62267=CARTESIAN_POINT('Ctrl Pts',(2.39268328644656,-0.995210568908195,
39.4111056518565));
#62268=CARTESIAN_POINT('Ctrl Pts',(2.35996373150917,-1.08099148036135,39.4075214323809));
#62269=CARTESIAN_POINT('Ctrl Pts',(2.322603485436,-1.16487755966247,39.403953527741));
#62270=CARTESIAN_POINT('Ctrl Pts',(2.28096449592765,-1.24660346235937,39.4003968590742));
#62271=CARTESIAN_POINT('Ctrl Pts',(2.23962237867528,-1.32774668633636,39.3968655482814));
#62272=CARTESIAN_POINT('Ctrl Pts',(2.19406163443676,-1.40676116498233,39.3933453138153));
#62273=CARTESIAN_POINT('Ctrl Pts',(2.14458115370232,-1.48337508521838,39.3898311846722));
#62274=CARTESIAN_POINT('Ctrl Pts',(2.09480630236801,-1.56044479903855,39.3862961491781));
#62275=CARTESIAN_POINT('Ctrl Pts',(2.0410643829371,-1.63508610297419,39.3827672918671));
#62276=CARTESIAN_POINT('Ctrl Pts',(1.98361248698335,-1.70699845916664,39.3792395524859));
#62277=CARTESIAN_POINT('Ctrl Pts',(1.9625644077349,-1.73334427329434,39.3779471297237));
#62278=CARTESIAN_POINT('Ctrl Pts',(1.9410179635923,-1.75932351900642,39.3766548570096));
#62279=CARTESIAN_POINT('Ctrl Pts',(1.91898445265148,-1.78492029350601,39.3753624855173));
#62280=CARTESIAN_POINT('Ctrl Pts',(1.90153877300993,-1.80518729176045,39.3743392124178));
#62281=CARTESIAN_POINT('Ctrl Pts',(1.88378772994283,-1.82521450164685,39.3733158773928));
#62282=CARTESIAN_POINT('Ctrl Pts',(1.86573664953228,-1.84499370935962,39.3722923569303));
#62283=CARTESIAN_POINT('Ctrl Pts',(1.8558141241398,-1.85586617163386,39.3717297364362));
#62284=CARTESIAN_POINT('Ctrl Pts',(1.84580621851311,-1.86665785434142,39.3711673608424));
#62285=CARTESIAN_POINT('Ctrl Pts',(1.83571834843321,-1.87736320670582,39.3706054437992));
#62286=CARTESIAN_POINT('Ctrl Pts',(1.76931159753876,-1.94783473955369,39.3669064384777));
#62287=CARTESIAN_POINT('Ctrl Pts',(1.69938786401867,-2.01462936439108,39.3632241072661));
#62288=CARTESIAN_POINT('Ctrl Pts',(1.62628672313842,-2.07743563507174,39.3595528525232));
#62289=CARTESIAN_POINT('Ctrl Pts',(1.5561772364533,-2.13767156771253,39.3560318433787));
#62290=CARTESIAN_POINT('Ctrl Pts',(1.48314412877673,-2.19423950466426,39.3525210226485));
#62291=CARTESIAN_POINT('Ctrl Pts',(1.4074450694785,-2.24683343290341,39.3490154521977));
#62292=CARTESIAN_POINT('Ctrl Pts',(1.33294635267627,-2.29859339137222,39.3455654687677));
#62293=CARTESIAN_POINT('Ctrl Pts',(1.25586490058951,-2.34650500808928,39.3421205704323));
#62294=CARTESIAN_POINT('Ctrl Pts',(1.1764163541384,-2.39023657739772,39.3386760502602));
#62295=CARTESIAN_POINT('Ctrl Pts',(1.14538583397869,-2.40731698230954,39.3373307109505));
#62296=CARTESIAN_POINT('Ctrl Pts',(1.11399394443605,-2.42375924272401,39.3359854293288));
#62297=CARTESIAN_POINT('Ctrl Pts',(1.08225259103083,-2.43954157402997,39.3346399249504));
#62298=CARTESIAN_POINT('Ctrl Pts',(1.06959621101295,-2.44583453766092,39.3341034256238));
#62299=CARTESIAN_POINT('Ctrl Pts',(1.05688426487745,-2.45202256581224,39.3335668908812));
#62300=CARTESIAN_POINT('Ctrl Pts',(1.04411748830536,-2.45810422120353,39.333030302944));
#62301=CARTESIAN_POINT('Ctrl Pts',(1.03064152771505,-2.46452370758792,39.3324639079849));
#62302=CARTESIAN_POINT('Ctrl Pts',(1.01711168853891,-2.47082119733044,39.331897757558));
#62303=CARTESIAN_POINT('Ctrl Pts',(1.00353479362675,-2.47699284501023,39.3313320696118));
#62304=CARTESIAN_POINT('Ctrl Pts',(0.966236089675615,-2.49394771290812,
39.329778000926));
#62305=CARTESIAN_POINT('Ctrl Pts',(0.928568841452935,-2.50995937495487,
39.3282268550137));
#62306=CARTESIAN_POINT('Ctrl Pts',(0.890556248926717,-2.52500318502184,
39.3266782169168));
#62307=CARTESIAN_POINT('Ctrl Pts',(0.807484702358906,-2.55787946326236,
39.3232938710138));
#62308=CARTESIAN_POINT('Ctrl Pts',(0.722765621710362,-2.58613669789995,
39.3199215020314));
#62309=CARTESIAN_POINT('Ctrl Pts',(0.636767319997115,-2.60991109724267,
39.3165567790635));
#62310=CARTESIAN_POINT('Ctrl Pts',(0.548522341733229,-2.63430659472855,
39.313104153846));
#62311=CARTESIAN_POINT('Ctrl Pts',(0.458929686032447,-2.65398210684791,
39.3096595793604));
#62312=CARTESIAN_POINT('Ctrl Pts',(0.368364879289187,-2.66903506839446,
39.3062183763255));
#62313=CARTESIAN_POINT('Ctrl Pts',(0.279383636592277,-2.68382482252575,
39.3028373441848));
#62314=CARTESIAN_POINT('Ctrl Pts',(0.189463090880913,-2.69415207285719,
39.2994595666231));
#62315=CARTESIAN_POINT('Ctrl Pts',(0.0989502335548338,-2.70006284797304,
39.2960806055499));
#62316=CARTESIAN_POINT('Ctrl Pts',(0.0775500298275637,-2.70146034878565,
39.2952817084927));
#62317=CARTESIAN_POINT('Ctrl Pts',(0.0561167062046726,-2.70261076645142,
39.2944827452768));
#62318=CARTESIAN_POINT('Ctrl Pts',(0.034654851265937,-2.70351433839264,
39.2936836572451));
#62319=CARTESIAN_POINT('Ctrl Pts',(0.0205332261909928,-2.70410887713211,
39.293157867577));
#62320=CARTESIAN_POINT('Ctrl Pts',(0.00640799301672085,-2.70459615835869,
39.2926323494521));
#62321=CARTESIAN_POINT('Ctrl Pts',(-0.00771643634287458,-2.70497657694664,
39.2921072000306));
#62322=CARTESIAN_POINT('Ctrl Pts',(-0.101719698230375,-2.70750840228552,
39.2886121378697));
#62323=CARTESIAN_POINT('Ctrl Pts',(-0.195729688081459,-2.70531291032107,
39.2851317795577));
#62324=CARTESIAN_POINT('Ctrl Pts',(-0.289352720535745,-2.698514854272,39.2816614070979));
#62325=CARTESIAN_POINT('Ctrl Pts',(-0.384132024040294,-2.69163284029931,
39.2781481745523));
#62326=CARTESIAN_POINT('Ctrl Pts',(-0.478515698146043,-2.68003388100711,
39.2746451760382));
#62327=CARTESIAN_POINT('Ctrl Pts',(-0.572104351374966,-2.66379465585476,
39.2711475165855));
#62328=CARTESIAN_POINT('Ctrl Pts',(-0.665368031458597,-2.64761181907741,
39.2676620022525));
#62329=CARTESIAN_POINT('Ctrl Pts',(-0.757843174723416,-2.62682077567727,
39.2641817899669));
#62330=CARTESIAN_POINT('Ctrl Pts',(-0.849129039468325,-2.60144632891952,
39.260702035573));
#62331=CARTESIAN_POINT('Ctrl Pts',(-0.887145207993385,-2.59087909327063,
39.2592528853696));
#62332=CARTESIAN_POINT('Ctrl Pts',(-0.924954967966171,-2.57951634574702,
39.2578038145793));
#62333=CARTESIAN_POINT('Ctrl Pts',(-0.962528474832794,-2.56735731546274,
39.2563544733274));
#62334=CARTESIAN_POINT('Ctrl Pts',(-0.978426001934737,-2.56221277268254,
39.2557412502415));
#62335=CARTESIAN_POINT('Ctrl Pts',(-0.994281227046726,-2.55692566296293,
39.2551279787381));
#62336=CARTESIAN_POINT('Ctrl Pts',(-1.01009184853142,-2.55149584746549,
39.2545146323168));
#62337=CARTESIAN_POINT('Ctrl Pts',(-1.02476184723976,-2.54645775415517,
39.2539455344343));
#62338=CARTESIAN_POINT('Ctrl Pts',(-1.03938588141779,-2.5412993580478,39.2533766649479));
#62339=CARTESIAN_POINT('Ctrl Pts',(-1.0539555861852,-2.5360234172864,39.2528082630797));
#62340=CARTESIAN_POINT('Ctrl Pts',(-1.14426394783588,-2.50332120581856,
39.2492851003049));
#62341=CARTESIAN_POINT('Ctrl Pts',(-1.23256614389459,-2.46607951371862,
39.2457767692827));
#62342=CARTESIAN_POINT('Ctrl Pts',(-1.31846265596223,-2.42437923432781,
39.242278438605));
#62343=CARTESIAN_POINT('Ctrl Pts',(-1.40300647890962,-2.38333564649392,
39.2388351992661));
#62344=CARTESIAN_POINT('Ctrl Pts',(-1.48522069962827,-2.33797256204044,
39.235401647783));
#62345=CARTESIAN_POINT('Ctrl Pts',(-1.56471216223979,-2.28831887886664,
39.2319731774254));
#62346=CARTESIAN_POINT('Ctrl Pts',(-1.60971511361838,-2.26020815834111,
39.2300321981083));
#62347=CARTESIAN_POINT('Ctrl Pts',(-1.653845098157,-2.23072140038903,39.2280928473407));
#62348=CARTESIAN_POINT('Ctrl Pts',(-1.69702733238731,-2.19985722057624,
39.2261542892225));
#62349=CARTESIAN_POINT('Ctrl Pts',(-1.73923615147419,-2.16968878197637,
39.2242594301361));
#62350=CARTESIAN_POINT('Ctrl Pts',(-1.78053947778623,-2.13820426438569,
39.2223653283661));
#62351=CARTESIAN_POINT('Ctrl Pts',(-1.82091439461048,-2.1054636261719,39.2204712032763));
#62352=CARTESIAN_POINT('Ctrl Pts',(-1.8498018668194,-2.08203833267543,39.2191159934036));
#62353=CARTESIAN_POINT('Ctrl Pts',(-1.87821401254732,-2.05796992890122,
39.2177607715932));
#62354=CARTESIAN_POINT('Ctrl Pts',(-1.90614139306952,-2.0332792648442,39.2164052519267));
#62355=CARTESIAN_POINT('Ctrl Pts',(-1.91596398111765,-2.02459509120772,
39.2159284900168));
#62356=CARTESIAN_POINT('Ctrl Pts',(-1.92572742236068,-2.01583317561599,
39.2154516504522));
#62357=CARTESIAN_POINT('Ctrl Pts',(-1.93542869344419,-2.00699675843135,
39.2149748479154));
#62358=CARTESIAN_POINT('Ctrl Pts',(-2.00468455990689,-1.94391494953425,
39.2115710287112));
#62359=CARTESIAN_POINT('Ctrl Pts',(-2.07052139305739,-1.87727179191439,
39.2081815447992));
#62360=CARTESIAN_POINT('Ctrl Pts',(-2.13285384149172,-1.80747796902504,
39.2048020558727));
#62361=CARTESIAN_POINT('Ctrl Pts',(-2.19655932242106,-1.73614675767774,
39.2013481250105));
#62362=CARTESIAN_POINT('Ctrl Pts',(-2.25660484514008,-1.66152391967282,
39.197904634314));
#62363=CARTESIAN_POINT('Ctrl Pts',(-2.31286801647662,-1.58400136238957,
39.1944669502929));
#62364=CARTESIAN_POINT('Ctrl Pts',(-2.36972346584143,-1.50566273117583,
39.1909930780395));
#62365=CARTESIAN_POINT('Ctrl Pts',(-2.42271702573988,-1.42436223090701,
39.1875251353579));
#62366=CARTESIAN_POINT('Ctrl Pts',(-2.47168306438995,-1.34046815016254,
39.1840583408827));
#62367=CARTESIAN_POINT('Ctrl Pts',(-2.49987230981729,-1.29217118971394,
39.1820625429173));
#62368=CARTESIAN_POINT('Ctrl Pts',(-2.52672599489418,-1.24301406482777,
39.180067125489));
#62369=CARTESIAN_POINT('Ctrl Pts',(-2.5522056678096,-1.19306325792156,39.1780711763405));
#62370=CARTESIAN_POINT('Ctrl Pts',(-2.56042357732412,-1.17695272099689,
39.1774274267306));
#62371=CARTESIAN_POINT('Ctrl Pts',(-2.56849851456185,-1.16075960512442,
39.176783621809));
#62372=CARTESIAN_POINT('Ctrl Pts',(-2.57642906806209,-1.14448609784345,
39.1761397309685));
#62373=CARTESIAN_POINT('Ctrl Pts',(-2.58202630645732,-1.13300055654104,
39.1756852846887));
#62374=CARTESIAN_POINT('Ctrl Pts',(-2.58755084539627,-1.12147647157377,
39.1752308557641));
#62375=CARTESIAN_POINT('Ctrl Pts',(-2.59299833616596,-1.10992317430216,
39.174776766792));
#62376=CARTESIAN_POINT('Ctrl Pts',(-2.63494544068166,-1.02095976185379,
39.1712801628739));
#62377=CARTESIAN_POINT('Ctrl Pts',(-2.67239555551184,-0.930128022481478,
39.1677982025641));
#62378=CARTESIAN_POINT('Ctrl Pts',(-2.70522126537772,-0.837829477144926,
39.1643261716253));
#62379=CARTESIAN_POINT('Ctrl Pts',(-2.73808241364883,-0.745431286948738,
39.1608503923063));
#62380=CARTESIAN_POINT('Ctrl Pts',(-2.76630961610753,-0.651562246339273,
39.1573845638093));
#62381=CARTESIAN_POINT('Ctrl Pts',(-2.78973122846687,-0.556596849324899,
39.153923956612));
#62382=CARTESIAN_POINT('Ctrl Pts',(-2.81265859587411,-0.463635420584731,
39.1505363754563));
#62383=CARTESIAN_POINT('Ctrl Pts',(-2.83098131139472,-0.369622551783345,
39.1471537975648));
#62384=CARTESIAN_POINT('Ctrl Pts',(-2.84449142099832,-0.274895379555267,
39.14377178655));
#62385=CARTESIAN_POINT('Ctrl Pts',(-2.85412274004531,-0.207364645540725,
39.1413607604326));
#62386=CARTESIAN_POINT('Ctrl Pts',(-2.86130723538155,-0.139470568128866,
39.1389500224146));
#62387=CARTESIAN_POINT('Ctrl Pts',(-2.86595331455768,-0.0713343506542745,
39.1365379651471));
#62388=CARTESIAN_POINT('Ctrl Pts',(-2.86760682598113,-0.0470850837618877,
39.1356795285827));
#62389=CARTESIAN_POINT('Ctrl Pts',(-2.86893661989062,-0.02283541425464,
39.1348219958471));
#62390=CARTESIAN_POINT('Ctrl Pts',(-2.86994055756815,0.00140893619034663,
39.1339652973708));
#62391=CARTESIAN_POINT('',(0.260859905888426,2.92566825966708,39.058));
#62392=CARTESIAN_POINT('Ctrl Pts',(0.260722923797069,2.92490787419814,39.058));
#62393=CARTESIAN_POINT('Ctrl Pts',(0.162848360265034,2.92110708545298,39.0703773556647));
#62394=CARTESIAN_POINT('Ctrl Pts',(0.0654427185948832,2.91266301593948,
39.0827988569344));
#62395=CARTESIAN_POINT('Ctrl Pts',(-0.0311162990840133,2.89958345814013,
39.0952840450831));
#62396=CARTESIAN_POINT('Ctrl Pts',(-0.129313155017022,2.88628204431298,
39.1079810075358));
#62397=CARTESIAN_POINT('Ctrl Pts',(-0.226635485341331,2.86818645239439,
39.1207438357102));
#62398=CARTESIAN_POINT('Ctrl Pts',(-0.32266288795503,2.84525380804573,39.133593082222));
#62399=CARTESIAN_POINT('Ctrl Pts',(-0.412969691932927,2.82368732013164,
39.1456768661673));
#62400=CARTESIAN_POINT('Ctrl Pts',(-0.502131726890962,2.79784231531796,
39.1578370788154));
#62401=CARTESIAN_POINT('Ctrl Pts',(-0.589768635260519,2.76764452465773,
39.1700908141378));
#62402=CARTESIAN_POINT('Ctrl Pts',(-0.617754478167129,2.75800120609176,
39.1740039041604));
#62403=CARTESIAN_POINT('Ctrl Pts',(-0.6455845199527,2.7479137292182,39.1779265313547));
#62404=CARTESIAN_POINT('Ctrl Pts',(-0.67324554731687,2.73737892024034,39.1818592523898));
#62405=CARTESIAN_POINT('Ctrl Pts',(-0.693406364060657,2.72970059541034,
39.1847256270565));
#62406=CARTESIAN_POINT('Ctrl Pts',(-0.713477387242329,2.7217846284664,39.1875973638378));
#62407=CARTESIAN_POINT('Ctrl Pts',(-0.733453348713622,2.71362967314459,
39.1904746782677));
#62408=CARTESIAN_POINT('Ctrl Pts',(-0.749161208632885,2.70721712093644,
39.1927372202773));
#62409=CARTESIAN_POINT('Ctrl Pts',(-0.764811862045415,2.70065600518691,
39.1950034483465));
#62410=CARTESIAN_POINT('Ctrl Pts',(-0.780383183738797,2.69395435536418,
39.1972706037194));
#62411=CARTESIAN_POINT('Ctrl Pts',(-0.863899019700987,2.65801046451841,
39.2094303535436));
#62412=CARTESIAN_POINT('Ctrl Pts',(-0.945263791906173,2.61797609039484,
39.2216352057428));
#62413=CARTESIAN_POINT('Ctrl Pts',(-1.02414462749053,2.57382342820898,39.2339041184484));
#62414=CARTESIAN_POINT('Ctrl Pts',(-1.06217855473277,2.55253436441183,39.2398198130493));
#62415=CARTESIAN_POINT('Ctrl Pts',(-1.09963454861993,2.53028724262747,39.245750400908));
#62416=CARTESIAN_POINT('Ctrl Pts',(-1.13647239878871,2.50707567377056,39.2516980071986));
#62417=CARTESIAN_POINT('Ctrl Pts',(-1.21477794615272,2.45773526448529,39.2643407255971));
#62418=CARTESIAN_POINT('Ctrl Pts',(-1.29029332358275,2.40403849832711,39.2770603421731));
#62419=CARTESIAN_POINT('Ctrl Pts',(-1.36280597910661,2.34631276383115,39.289877269102));
#62420=CARTESIAN_POINT('Ctrl Pts',(-1.43780473366327,2.28660790042783,39.3031336248369));
#62421=CARTESIAN_POINT('Ctrl Pts',(-1.50959208190557,2.22259204721685,39.3164940778875));
#62422=CARTESIAN_POINT('Ctrl Pts',(-1.57787834130925,2.15460693677166,39.3299812127298));
#62423=CARTESIAN_POINT('Ctrl Pts',(-1.59002758401102,2.14251127339636,39.3323807946659));
#62424=CARTESIAN_POINT('Ctrl Pts',(-1.60206585076167,2.13028993909883,39.3347843866167));
#62425=CARTESIAN_POINT('Ctrl Pts',(-1.61399130943753,2.11794483308677,39.3371921157736));
#62426=CARTESIAN_POINT('Ctrl Pts',(-1.62247302820951,2.10916464942671,39.3389045598937));
#62427=CARTESIAN_POINT('Ctrl Pts',(-1.63089629603585,2.10032323235738,39.3406188236418));
#62428=CARTESIAN_POINT('Ctrl Pts',(-1.63925448160622,2.09142789834082,39.3423336976597));
#62429=CARTESIAN_POINT('Ctrl Pts',(-1.70075807351381,2.02597170708621,39.3549525741946));
#62430=CARTESIAN_POINT('Ctrl Pts',(-1.75883748111895,1.95749928194615,39.3676238420838));
#62431=CARTESIAN_POINT('Ctrl Pts',(-1.81332493160888,1.88633203750824,39.380369171064));
#62432=CARTESIAN_POINT('Ctrl Pts',(-1.86759709574965,1.81544598325444,39.3930641417448));
#62433=CARTESIAN_POINT('Ctrl Pts',(-1.918305926586,1.74188536506989,39.4058325894245));
#62434=CARTESIAN_POINT('Ctrl Pts',(-1.96523749898236,1.66594995450098,39.4186959279941));
#62435=CARTESIAN_POINT('Ctrl Pts',(-2.01136571686395,1.59131437370118,39.4313390774547));
#62436=CARTESIAN_POINT('Ctrl Pts',(-2.05384502137649,1.51438370651053,39.4440738970063));
#62437=CARTESIAN_POINT('Ctrl Pts',(-2.09242267521999,1.43543935198141,39.4569207195948));
#62438=CARTESIAN_POINT('Ctrl Pts',(-2.11318763556892,1.39294645186315,39.4638357010694));
#62439=CARTESIAN_POINT('Ctrl Pts',(-2.13282130912474,1.34987015428585,39.4707831329688));
#62440=CARTESIAN_POINT('Ctrl Pts',(-2.15127797244486,1.30625529672902,39.4777661862196));
#62441=CARTESIAN_POINT('Ctrl Pts',(-2.15677341232959,1.29326904760979,39.4798453783621));
#62442=CARTESIAN_POINT('Ctrl Pts',(-2.16216519449366,1.28023327496112,39.4819280131221));
#62443=CARTESIAN_POINT('Ctrl Pts',(-2.16744975458983,1.26715483776717,39.4840132729464));
#62444=CARTESIAN_POINT('Ctrl Pts',(-2.19936788078035,1.18816260357277,39.4966079989029));
#62445=CARTESIAN_POINT('Ctrl Pts',(-2.22727542829756,1.10787312475877,39.5092572977189));
#62446=CARTESIAN_POINT('Ctrl Pts',(-2.25099555335962,1.02655503037711,39.5219833174302));
#62447=CARTESIAN_POINT('Ctrl Pts',(-2.27436406309063,0.946442354963575,
39.5345206929575));
#62448=CARTESIAN_POINT('Ctrl Pts',(-2.29366844569015,0.865330512105231,
39.5471325316936));
#62449=CARTESIAN_POINT('Ctrl Pts',(-2.30868993862032,0.783477908782109,
39.5598400112676));
#62450=CARTESIAN_POINT('Ctrl Pts',(-2.32326996787289,0.704030855390139,
39.5721740332437));
#62451=CARTESIAN_POINT('Ctrl Pts',(-2.33381505358564,0.623885304742978,
39.5845981571237));
#62452=CARTESIAN_POINT('Ctrl Pts',(-2.34007838345357,0.543289558251172,
39.5971317477171));
#62453=CARTESIAN_POINT('Ctrl Pts',(-2.345223193426,0.477086786078833,39.6074270607909));
#62454=CARTESIAN_POINT('Ctrl Pts',(-2.34747816613177,0.410580313554983,
39.6177962340149));
#62455=CARTESIAN_POINT('Ctrl Pts',(-2.34668236863851,0.343918483395665,
39.62825));
#62456=CARTESIAN_POINT('',(-2.14344942214843,2.01149700971877,39.058));
#62457=CARTESIAN_POINT('Origin',(0.,0.,39.058));
#62458=CARTESIAN_POINT('Ctrl Pts',(-2.86994055756815,0.00140893619034663,
39.1339652973708));
#62459=CARTESIAN_POINT('Ctrl Pts',(-2.87320577914358,0.0802616159190132,
39.1311789587253));
#62460=CARTESIAN_POINT('Ctrl Pts',(-2.87302560073353,0.159057577103706,
39.1284014445519));
#62461=CARTESIAN_POINT('Ctrl Pts',(-2.86931315923603,0.237604716866276,
39.125630361528));
#62462=CARTESIAN_POINT('Ctrl Pts',(-2.86480590834164,0.33296828453044,39.1222660077877));
#62463=CARTESIAN_POINT('Ctrl Pts',(-2.85509398930959,0.427965500006218,
39.1189111337089));
#62464=CARTESIAN_POINT('Ctrl Pts',(-2.8404520930183,0.522299278433487,39.1155614561975));
#62465=CARTESIAN_POINT('Ctrl Pts',(-2.82552036226947,0.618500381895329,
39.1121454722498));
#62466=CARTESIAN_POINT('Ctrl Pts',(-2.80546129783727,0.71401229537241,39.1087348926365));
#62467=CARTESIAN_POINT('Ctrl Pts',(-2.78051144060668,0.808516432443364,
39.1053251748457));
#62468=CARTESIAN_POINT('Ctrl Pts',(-2.76597047184241,0.863594170666203,
39.1033379650819));
#62469=CARTESIAN_POINT('Ctrl Pts',(-2.74976727234159,0.918329478376449,
39.1013510480489));
#62470=CARTESIAN_POINT('Ctrl Pts',(-2.73194088190628,0.972657121596614,
39.0993635245144));
#62471=CARTESIAN_POINT('Ctrl Pts',(-2.72568217604983,0.991731130999871,
39.098665720591));
#62472=CARTESIAN_POINT('Ctrl Pts',(-2.71922333763423,1.01075486961467,39.0979678419068));
#62473=CARTESIAN_POINT('Ctrl Pts',(-2.71256590131154,1.02972544345301,39.0972698495451));
#62474=CARTESIAN_POINT('Ctrl Pts',(-2.70786090595029,1.04313247546704,39.0967765589351));
#62475=CARTESIAN_POINT('Ctrl Pts',(-2.70306010139198,1.05650330826665,39.0962835663674));
#62476=CARTESIAN_POINT('Ctrl Pts',(-2.69816441448398,1.06983707108187,39.0957908567459));
#62477=CARTESIAN_POINT('Ctrl Pts',(-2.66407853481969,1.16267246748952,39.0923604002682));
#62478=CARTESIAN_POINT('Ctrl Pts',(-2.6253979559053,1.25371035778419,39.0889436904178));
#62479=CARTESIAN_POINT('Ctrl Pts',(-2.58240965705905,1.34263826608692,39.0855362733872));
#62480=CARTESIAN_POINT('Ctrl Pts',(-2.53890424253589,1.4326359077062,39.0820878677897));
#62481=CARTESIAN_POINT('Ctrl Pts',(-2.49098647195779,1.5204733357728,39.0786489799275));
#62482=CARTESIAN_POINT('Ctrl Pts',(-2.43890099522592,1.60581543086489,39.0752149933246));
#62483=CARTESIAN_POINT('Ctrl Pts',(-2.38699542910386,1.6908627422796,39.0717928681975));
#62484=CARTESIAN_POINT('Ctrl Pts',(-2.33095040623944,1.77343274680066,39.0683756105289));
#62485=CARTESIAN_POINT('Ctrl Pts',(-2.27096264380004,1.85317031961247,39.0649586515155));
#62486=CARTESIAN_POINT('Ctrl Pts',(-2.23024681086646,1.90729105292729,39.0626394396184));
#62487=CARTESIAN_POINT('Ctrl Pts',(-2.18771369495367,1.96010644704108,39.0603203653064));
#62488=CARTESIAN_POINT('Ctrl Pts',(-2.14341454569435,2.01149633185867,39.058));
#62489=CARTESIAN_POINT('',(-2.,-2.44929359829471E-16,40.));
#62490=CARTESIAN_POINT('',(-2.5,-3.06161699786838E-16,39.5));
#62491=CARTESIAN_POINT('Origin',(0.,0.,40.));
#62492=CARTESIAN_POINT('Ctrl Pts',(1.70810875200399,-2.39535560853235,-0.329233991005384));
#62493=CARTESIAN_POINT('Ctrl Pts',(2.5065338081197,-1.82600514494664,-0.276184124874192));
#62494=CARTESIAN_POINT('Ctrl Pts',(3.47517087235694,0.164164634797699,-0.170084392611809));
#62495=CARTESIAN_POINT('Ctrl Pts',(1.73627755672406,3.01873330702807,-0.0109347942182355));
#62496=CARTESIAN_POINT('Ctrl Pts',(-1.60036897517342,3.08916744448106,0.148214804175339));
#62497=CARTESIAN_POINT('Ctrl Pts',(-3.46493207619462,0.324065259852807,
0.307364402568913));
#62498=CARTESIAN_POINT('Ctrl Pts',(-2.14446912907937,-2.7412743082718,0.466514000962488));
#62499=CARTESIAN_POINT('Ctrl Pts',(1.14770819747867,-3.28524492291903,0.625663599356061));
#62500=CARTESIAN_POINT('Ctrl Pts',(3.38463715916455,-0.809595521922738,
0.784813197749637));
#62501=CARTESIAN_POINT('Ctrl Pts',(2.5099982047375,2.41067844839361,0.943962796143209));
#62502=CARTESIAN_POINT('Ctrl Pts',(-0.672211430585623,3.41454803161592,
1.10311239453679));
#62503=CARTESIAN_POINT('Ctrl Pts',(-3.23641431966485,1.27938206751248,1.26226199293036));
#62504=CARTESIAN_POINT('Ctrl Pts',(-2.82526444201928,-2.03201736216267,
1.42141159132393));
#62505=CARTESIAN_POINT('Ctrl Pts',(0.183265436626373,-3.47527918744039,
1.58056118971751));
#62506=CARTESIAN_POINT('Ctrl Pts',(3.02330987809428,-1.72359489362586,1.73971078811108));
#62507=CARTESIAN_POINT('Ctrl Pts',(3.0839092807201,1.61266406976645,1.89886038650466));
#62508=CARTESIAN_POINT('Ctrl Pts',(0.309350342877327,3.46633465739727,2.05800998489823));
#62509=CARTESIAN_POINT('Ctrl Pts',(-2.74960604526907,2.1332709394318,2.2171595832918));
#62510=CARTESIAN_POINT('Ctrl Pts',(-3.2807428921365,-1.16099267046222,2.37630918168538));
#62511=CARTESIAN_POINT('Ctrl Pts',(-0.795765171857732,-3.3879100678833,
2.53545878007895));
#62512=CARTESIAN_POINT('Ctrl Pts',(2.42079035479599,-2.50019031475376,2.69460837847253));
#62513=CARTESIAN_POINT('Ctrl Pts',(3.41181923151422,0.686051726781072,2.8537579768661));
#62514=CARTESIAN_POINT('Ctrl Pts',(1.26623004817903,3.24157967234375,3.01290757525968));
#62515=CARTESIAN_POINT('Ctrl Pts',(-2.04345363315851,2.81699745515115,3.17205717365325));
#62516=CARTESIAN_POINT('Ctrl Pts',(-3.47451095858186,-0.197360047609994,
3.33120677204682));
#62517=CARTESIAN_POINT('Ctrl Pts',(-1.7113152939479,-3.03027677589855,3.4903563704404));
#62518=CARTESIAN_POINT('Ctrl Pts',(1.62515904294783,-3.07734227449719,3.64950596883397));
#62519=CARTESIAN_POINT('Ctrl Pts',(3.46756149776779,-0.295287392371581,
3.80865556722755));
#62520=CARTESIAN_POINT('Ctrl Pts',(2.12209987368507,2.75823666664889,3.96780516562112));
#62521=CARTESIAN_POINT('Ctrl Pts',(-1.1742906560288,3.27600653853182,4.1269547640147));
#62522=CARTESIAN_POINT('Ctrl Pts',(-3.39111013780228,0.782016251666639,
4.28610436240827));
#62523=CARTESIAN_POINT('Ctrl Pts',(-2.49035024800795,-2.4309119742704,4.44525396080185));
#62524=CARTESIAN_POINT('Ctrl Pts',(0.69988543157182,-3.40900832609501,4.60440355919542));
#62525=CARTESIAN_POINT('Ctrl Pts',(3.24668922743323,-1.25307080608154,4.763553157589));
#62526=CARTESIAN_POINT('Ctrl Pts',(2.80868540870487,2.0548634162641,4.92270275598256));
#62527=CARTESIAN_POINT('Ctrl Pts',(-0.211452087625477,3.47368182182148,
5.08185235437615));
#62528=CARTESIAN_POINT('Ctrl Pts',(-3.03719346007492,1.69900949693403,5.24100195276971));
#62529=CARTESIAN_POINT('Ctrl Pts',(-3.07072482055295,-1.63762830368612,
5.4001515511633));
#62530=CARTESIAN_POINT('Ctrl Pts',(-0.281219485916566,-3.46873074558119,
5.55930114955686));
#62531=CARTESIAN_POINT('Ctrl Pts',(2.76682185390363,-2.11089417388877,5.71845074795045));
#62532=CARTESIAN_POINT('Ctrl Pts',(3.27121630939976,1.18756946816326,5.87760034634401));
#62533=CARTESIAN_POINT('Ctrl Pts',(0.768254450424601,3.394254334018,6.03674994473758));
#62534=CARTESIAN_POINT('Ctrl Pts',(-2.44099358900468,2.48046924654082,6.19589954313117));
#62535=CARTESIAN_POINT('Ctrl Pts',(-3.40614133387891,-0.713707641992457,
6.35504914152473));
#62536=CARTESIAN_POINT('Ctrl Pts',(-1.23989094436864,-3.25174535144891,
6.51419873991831));
#62537=CARTESIAN_POINT('Ctrl Pts',(2.06623938829558,-2.80032715496828,6.67334833831189));
#62538=CARTESIAN_POINT('Ctrl Pts',(3.47279553085058,0.225540651548871,6.83249793670546));
#62539=CARTESIAN_POINT('Ctrl Pts',(1.68667574471175,3.04406016970723,6.99164753509903));
#62540=CARTESIAN_POINT('Ctrl Pts',(-1.65007061929938,3.06405684280202,7.15079713349261));
#62541=CARTESIAN_POINT('Ctrl Pts',(-3.46984292017243,0.267146951931126,
7.30994673188618));
#62542=CARTESIAN_POINT('Ctrl Pts',(-2.09965374212423,-2.77536151659212,
7.46909633027976));
#62543=CARTESIAN_POINT('Ctrl Pts',(1.20082874041637,-3.26637225692158,7.62824592867333));
#62544=CARTESIAN_POINT('Ctrl Pts',(3.39734268235243,-0.754480008524603,
7.78739552706691));
#62545=CARTESIAN_POINT('Ctrl Pts',(2.47054743228023,2.45103504043708,7.94654512546048));
#62546=CARTESIAN_POINT('Ctrl Pts',(-0.727518109309972,3.40321829820288,
8.10569472385404));
#62547=CARTESIAN_POINT('Ctrl Pts',(-3.2567479723672,1.22669068190765,8.26484432224764));
#62548=CARTESIAN_POINT('Ctrl Pts',(-2.79192282561145,-2.07758136313038,
8.42399392064119));
#62549=CARTESIAN_POINT('Ctrl Pts',(0.239625504503551,-3.47185209969956,
8.58314351903478));
#62550=CARTESIAN_POINT('Ctrl Pts',(3.05087679342124,-1.67431424050583,8.74229311742835));
#62551=CARTESIAN_POINT('Ctrl Pts',(3.05733845011404,1.66248578521777,8.90144271582193));
#62552=CARTESIAN_POINT('Ctrl Pts',(0.253070022401753,3.47089800316265,9.06059231421549));
#62553=CARTESIAN_POINT('Ctrl Pts',(-2.78385551443731,2.08837876337934,9.21974191260909));
#62554=CARTESIAN_POINT('Ctrl Pts',(-3.26147446067824,-1.21406825464651,
9.37889151100263));
#62555=CARTESIAN_POINT('Ctrl Pts',(-0.740693152670185,-3.40037513197947,
9.53804110939624));
#62556=CARTESIAN_POINT('Ctrl Pts',(2.46103616338236,-2.46058496848232,9.69719070778978));
#62557=CARTESIAN_POINT('Ctrl Pts',(3.40023926714405,0.741316606294871,9.85634030618338));
#62558=CARTESIAN_POINT('Ctrl Pts',(1.21347023590029,3.26169700787503,10.0154899045769));
#62559=CARTESIAN_POINT('Ctrl Pts',(-2.08888915415634,2.78347255891718,10.1746395029705));
#62560=CARTESIAN_POINT('Ctrl Pts',(-3.47085154388881,-0.253706414742628,
10.3337891013641));
#62561=CARTESIAN_POINT('Ctrl Pts',(-1.66192518770954,-3.05764321905834,
10.4929386997577));
#62562=CARTESIAN_POINT('Ctrl Pts',(1.67487359716716,-3.05056975303127,10.6520882981512));
#62563=CARTESIAN_POINT('Ctrl Pts',(3.47189597719149,-0.238988928945294,
10.8112378965448));
#62564=CARTESIAN_POINT('Ctrl Pts',(2.07706942316891,2.79230370768181,10.9703874949384));
#62565=CARTESIAN_POINT('Ctrl Pts',(-1.22728779301538,3.25652300125645,11.129537093332));
#62566=CARTESIAN_POINT('Ctrl Pts',(-3.40335163300419,0.7268941097055,11.2886866917255));
#62567=CARTESIAN_POINT('Ctrl Pts',(-2.45058201906605,-2.47099679328547,
11.4478362901191));
#62568=CARTESIAN_POINT('Ctrl Pts',(0.75510290591141,-3.39720428971839,11.6069858885127));
#62569=CARTESIAN_POINT('Ctrl Pts',(3.2665923765427,-1.20022982387123,11.7661354869063));
#62570=CARTESIAN_POINT('Ctrl Pts',(2.77497649392323,2.10016257531898,11.9252850852998));
#62571=CARTESIAN_POINT('Ctrl Pts',(-0.267783150583668,3.46979387988111,
12.0844346836934));
#62572=CARTESIAN_POINT('Ctrl Pts',(-3.06435933528609,1.6495087901681,12.243584282087));
#62573=CARTESIAN_POINT('Ctrl Pts',(-3.04375086292351,-1.6872338513227,12.4027338804806));
#62574=CARTESIAN_POINT('Ctrl Pts',(-0.224903903247275,-3.47283682583864,
12.5618834788741));
#62575=CARTESIAN_POINT('Ctrl Pts',(2.80070595732196,-2.06572590757297,12.7210330772677));
#62576=CARTESIAN_POINT('Ctrl Pts',(3.25151796012581,1.24048713801321,12.8801826756613));
#62577=CARTESIAN_POINT('Ctrl Pts',(0.71308310667526,3.40627213645228,13.0393322740549));
#62578=CARTESIAN_POINT('Ctrl Pts',(-2.48091676625765,2.4405387486165,13.1984818724484));
#62579=CARTESIAN_POINT('Ctrl Pts',(-3.39411341586236,-0.768876781324591,
13.357631470842));
#62580=CARTESIAN_POINT('Ctrl Pts',(-1.18696966367366,-3.27143399782347,
13.5167810692356));
#62581=CARTESIAN_POINT('Ctrl Pts',(2.11140144112928,-2.76643477042095,13.6759306676291));
#62582=CARTESIAN_POINT('Ctrl Pts',(3.46867912507889,0.281855480412862,13.8350802660227));
#62583=CARTESIAN_POINT('Ctrl Pts',(1.63706525217668,3.07102503159981,13.9942298644163));
#62584=CARTESIAN_POINT('Ctrl Pts',(-1.69956634431306,3.03688189198646,14.1533794628099));
#62585=CARTESIAN_POINT('Ctrl Pts',(-3.4737205336237,0.210815177057792,14.3125290612034));
#62586=CARTESIAN_POINT('Ctrl Pts',(-2.05434840323376,-2.80906212511005,
14.471678659597));
#62587=CARTESIAN_POINT('Ctrl Pts',(1.25366607246256,-3.24645941963753,14.6308282579906));
#62588=CARTESIAN_POINT('Ctrl Pts',(3.40913659427078,-0.699260370820959,
14.7899778563842));
#62589=CARTESIAN_POINT('Ctrl Pts',(2.4304553223822,2.49079591907906,14.9491274547778));
#62590=CARTESIAN_POINT('Ctrl Pts',(-0.782638005903754,3.39096669643213,
15.1082770531713));
#62591=CARTESIAN_POINT('Ctrl Pts',(-3.27622179205498,1.17368997348573,15.2674266515649));
#62592=CARTESIAN_POINT('Ctrl Pts',(-2.75784752895294,-2.12260556666684,
15.4265762499585));
#62593=CARTESIAN_POINT('Ctrl Pts',(0.295923172689008,-3.46750729782397,
15.585725848352));
#62594=CARTESIAN_POINT('Ctrl Pts',(3.07764019832444,-1.6245947784769,15.7448754467456));
#62595=CARTESIAN_POINT('Ctrl Pts',(3.02996295323977,1.71187087322363,15.9040250451392));
#62596=CARTESIAN_POINT('Ctrl Pts',(0.196722982187926,3.47454708600645,16.0631746435328));
#62597=CARTESIAN_POINT('Ctrl Pts',(-2.81737207355656,2.04293709735284,16.2223242419263));
#62598=CARTESIAN_POINT('Ctrl Pts',(-3.2413474630231,-1.26682437952171,16.3814738403199));
#62599=CARTESIAN_POINT('Ctrl Pts',(-0.68542612957718,-3.41194495932888,
16.5406234387135));
#62600=CARTESIAN_POINT('Ctrl Pts',(2.50063408920154,-2.42033190627238,16.6997730371071));
#62601=CARTESIAN_POINT('Ctrl Pts',(3.38776418320275,0.796386353226517,16.8589226355006));
#62602=CARTESIAN_POINT('Ctrl Pts',(1.16039097180682,3.28095568046051,17.0180722338942));
#62603=CARTESIAN_POINT('Ctrl Pts',(-2.13377476758282,2.74921491081068,17.1772218322878));
#62604=CARTESIAN_POINT('Ctrl Pts',(-3.46627841739718,-0.309985995947102,
17.3363714306813));
#62605=CARTESIAN_POINT('Ctrl Pts',(-1.61209757425368,-3.08420472661629,
17.495521029075));
#62606=CARTESIAN_POINT('Ctrl Pts',(1.7241472355999,-3.0229941605253,17.6546706274685));
#62607=CARTESIAN_POINT('Ctrl Pts',(3.47531646938709,-0.182627550505842,
17.8138202258621));
#62608=CARTESIAN_POINT('Ctrl Pts',(2.03149217768794,2.82563566593247,17.9729698242556));
#62609=CARTESIAN_POINT('Ctrl Pts',(-1.27996184268848,3.2361821743929,18.1321194226493));
#62610=CARTESIAN_POINT('Ctrl Pts',(-3.4146971854187,0.671580610567688,18.2912690210428));
#62611=CARTESIAN_POINT('Ctrl Pts',(-2.41016866685424,-2.5104311147512,18.4504186194364));
#62612=CARTESIAN_POINT('Ctrl Pts',(0.810121597082249,-3.38450592886727,
18.6095682178299));
#62613=CARTESIAN_POINT('Ctrl Pts',(3.28563558515027,-1.1470728774542,18.7687178162235));
#62614=CARTESIAN_POINT('Ctrl Pts',(2.74053705803234,2.14490886010299,18.9278674146171));
#62615=CARTESIAN_POINT('Ctrl Pts',(-0.324043718802237,3.46499250401812,
19.0870170130107));
#62616=CARTESIAN_POINT('Ctrl Pts',(-3.09071850846487,1.59957384513173,19.2461666114042));
#62617=CARTESIAN_POINT('Ctrl Pts',(-3.01597562850516,-1.73639522945087,
19.4053162097978));
#62618=CARTESIAN_POINT('Ctrl Pts',(-0.168529113932866,-3.47602867110644,
19.5644658081914));
#62619=CARTESIAN_POINT('Ctrl Pts',(2.83385276627145,-2.02001383254979,19.723615406585));
#62620=CARTESIAN_POINT('Ctrl Pts',(3.23096363873481,1.29307824580353,19.8827650049785));
#62621=CARTESIAN_POINT('Ctrl Pts',(0.657724041601946,3.41739322725609,20.0419146033721));
#62622=CARTESIAN_POINT('Ctrl Pts',(-2.52018683453118,2.3999657713502,20.2010642017657));
#62623=CARTESIAN_POINT('Ctrl Pts',(-3.38119198703589,-0.823843511476016,
20.3602138001593));
#62624=CARTESIAN_POINT('Ctrl Pts',(-1.13373590955914,-3.29026142912276,
20.5193633985529));
#62625=CARTESIAN_POINT('Ctrl Pts',(2.1560076610309,-2.73181411340027,20.6785129969464));
#62626=CARTESIAN_POINT('Ctrl Pts',(3.46364957884472,0.338096109953581,20.83766259534));
#62627=CARTESIAN_POINT('Ctrl Pts',(1.58702379717214,3.09718143669468,20.9968121937336));
#62628=CARTESIAN_POINT('Ctrl Pts',(-1.74861465325227,3.00890747265985,21.1559617921271));
#62629=CARTESIAN_POINT('Ctrl Pts',(-3.47668367944616,0.154427904439827,
21.3151113905207));
#62630=CARTESIAN_POINT('Ctrl Pts',(-2.00850225079915,-2.84202323937219,
21.4742609889143));
#62631=CARTESIAN_POINT('Ctrl Pts',(1.3061733730541,-3.22569194191282,21.6334105873079));
#62632=CARTESIAN_POINT('Ctrl Pts',(3.42003304048126,-0.643856650671137,
21.7925601857014));
#62633=CARTESIAN_POINT('Ctrl Pts',(2.38972338763523,2.52990108802421,21.951709784095));
#62634=CARTESIAN_POINT('Ctrl Pts',(-0.837551870632141,3.37782241223505,
22.1108593824886));
#62635=CARTESIAN_POINT('Ctrl Pts',(-3.29483313626591,1.12038028756356,22.2700089808822));
#62636=CARTESIAN_POINT('Ctrl Pts',(-2.72304622043883,-2.16707098775067,
22.4291585792757));
#62637=CARTESIAN_POINT('Ctrl Pts',(0.352142938187871,-3.46224966397303,
22.5883081776693));
#62638=CARTESIAN_POINT('Ctrl Pts',(3.10359340496692,-1.57444763686911,22.7474577760629));
#62639=CARTESIAN_POINT('Ctrl Pts',(3.00178980928638,1.76080530594988,22.9066073744565));
#62640=CARTESIAN_POINT('Ctrl Pts',(0.140324154043218,3.47728148362897,23.06575697285));
#62641=CARTESIAN_POINT('Ctrl Pts',(-2.8501469508005,1.99695762184366,23.2249065712436));
#62642=CARTESIAN_POINT('Ctrl Pts',(-3.22036717066564,-1.31924700897744,
23.3840561696372));
#62643=CARTESIAN_POINT('Ctrl Pts',(-0.629978665944583,-3.42261658165964,
23.5432057680308));
#62644=CARTESIAN_POINT('Ctrl Pts',(2.53957371539527,-2.37944168423399,23.7023553664243));
#62645=CARTESIAN_POINT('Ctrl Pts',(3.37439725990662,0.851246448997968,23.8615049648179));
#62646=CARTESIAN_POINT('Ctrl Pts',(1.10700623121625,3.29935063135843,24.0206545632115));
#62647=CARTESIAN_POINT('Ctrl Pts',(-2.17809865823012,2.7142335234119,24.179804161605));
#62648=CARTESIAN_POINT('Ctrl Pts',(-3.46079278243677,-0.366183972383433,
24.3389537599987));
#62649=CARTESIAN_POINT('Ctrl Pts',(-1.56184557114644,-3.10995430778124,
24.4981033583922));
#62650=CARTESIAN_POINT('Ctrl Pts',(1.77296698696289,-2.99462275549635,24.6572529567858));
#62651=CARTESIAN_POINT('Ctrl Pts',(3.47782207381884,-0.126218094801235,
24.8164025551794));
#62652=CARTESIAN_POINT('Ctrl Pts',(1.98538013563459,2.85822376689167,24.9755521535729));
#62653=CARTESIAN_POINT('Ctrl Pts',(-1.33229893846449,3.21498941260517,25.1347017519665));
#62654=CARTESIAN_POINT('Ctrl Pts',(-3.42514380828257,0.616090315765816,
25.2938513503601));
#62655=CARTESIAN_POINT('Ctrl Pts',(-2.36912083031805,-2.54920455749435,
25.4530009487536));
#62656=CARTESIAN_POINT('Ctrl Pts',(0.864927021247645,-3.37091658640681,
25.6121505471473));
#62657=CARTESIAN_POINT('Ctrl Pts',(3.30381384007098,-1.0936139605694,25.7713001455407));
#62658=CARTESIAN_POINT('Ctrl Pts',(2.70537616732062,2.18909049102374,25.9304497439344));
#62659=CARTESIAN_POINT('Ctrl Pts',(-0.380218981513895,3.45927895820695,
26.0895993423279));
#62660=CARTESIAN_POINT('Ctrl Pts',(-3.11626404047753,1.54921780735424,26.2487489407215));
#62661=CARTESIAN_POINT('Ctrl Pts',(-2.98740642921401,-1.78509949618719,
26.4078985391151));
#62662=CARTESIAN_POINT('Ctrl Pts',(-0.112109958810153,-3.47830544112107,
26.5670481375086));
#62663=CARTESIAN_POINT('Ctrl Pts',(2.86625355475253,-1.97376998266397,26.7261977359023));
#62664=CARTESIAN_POINT('Ctrl Pts',(3.20955875621522,1.34532894676326,26.8853473342958));
#62665=CARTESIAN_POINT('Ctrl Pts',(0.602191828648999,3.42761467876791,27.0444969326894));
#62666=CARTESIAN_POINT('Ctrl Pts',(-2.55879345585885,2.3587609957032,27.203646531083));
#62667=CARTESIAN_POINT('Ctrl Pts',(-3.36738044900546,-0.878593362285773,
27.3627961294765));
#62668=CARTESIAN_POINT('Ctrl Pts',(-1.08020369597472,-3.30822268896751,
27.5219457278701));
#62669=CARTESIAN_POINT('Ctrl Pts',(2.20004630527573,-2.69647429790079,27.6810953262637));
#62670=CARTESIAN_POINT('Ctrl Pts',(3.45770821619155,0.394247734652099,27.8402449246573));
#62671=CARTESIAN_POINT('Ctrl Pts',(1.53656455326529,3.12252249923767,27.9993945230509));
#62672=CARTESIAN_POINT('Ctrl Pts',(-1.79720263399863,2.98014094917425,28.1585441214444));
#62673=CARTESIAN_POINT('Ctrl Pts',(-3.47873157758249,0.0979999782004309,
28.317693719838));
#62674=CARTESIAN_POINT('Ctrl Pts',(-1.96212735396128,-2.87423618226371,
28.4768433182315));
#62675=CARTESIAN_POINT('Ctrl Pts',(1.35833681948244,-3.20407529084994,28.6359929166252));
#62676=CARTESIAN_POINT('Ctrl Pts',(3.43002915246079,-0.588283433275092,
28.7951425150187));
#62677=CARTESIAN_POINT('Ctrl Pts',(2.34836235084664,2.56834025271633,28.9542921134123));
#62678=CARTESIAN_POINT('Ctrl Pts',(-0.892245247251056,3.36378890588496,
29.1134417118058));
#62679=CARTESIAN_POINT('Ctrl Pts',(-3.31257710550631,1.06677565808014,29.2725913101995));
#62680=CARTESIAN_POINT('Ctrl Pts',(-2.68752806162076,-2.21096592072287,
29.431740908593));
#62681=CARTESIAN_POINT('Ctrl Pts',(0.408270000973746,-3.45608058223499,
29.5908905069866));
#62682=CARTESIAN_POINT('Ctrl Pts',(3.1287295810871,-1.52388601707194,29.7500401053801));
#62683=CARTESIAN_POINT('Ctrl Pts',(2.97282643492082,1.80927620125641,29.9091897037738));
#62684=CARTESIAN_POINT('Ctrl Pts',(0.0838883851327475,3.47910047619161,
30.0683393021673));
#62685=CARTESIAN_POINT('Ctrl Pts',(-2.8821715180818,1.95045244109027,30.2274889005609));
#62686=CARTESIAN_POINT('Ctrl Pts',(-3.19853910673239,-1.37132234259506,
30.3866384989544));
#62687=CARTESIAN_POINT('Ctrl Pts',(-0.57436535848797,-3.43238718963432,
30.5457880973481));
#62688=CARTESIAN_POINT('Ctrl Pts',(2.57784479098707,-2.33792506684404,30.7049376957416));
#62689=CARTESIAN_POINT('Ctrl Pts',(3.36014201613933,0.905882451520032,30.8640872941352));
#62690=CARTESIAN_POINT('Ctrl Pts',(1.053330067826,3.31687701804131,31.0232368925287));
#62691=CARTESIAN_POINT('Ctrl Pts',(-2.22184915769754,2.67853760567881,31.1823864909223));
#62692=CARTESIAN_POINT('Ctrl Pts',(-3.45439608311781,-0.422285549761243,
31.3415360893159));
#62693=CARTESIAN_POINT('Ctrl Pts',(-1.51118240738248,-3.13488518389664,
31.5006856877095));
#62694=CARTESIAN_POINT('Ctrl Pts',(1.82131999930616,-2.9654630068042,31.659835286103));
#62695=CARTESIAN_POINT('Ctrl Pts',(3.47941213087869,-0.0697754117944455,
31.8189848844967));
#62696=CARTESIAN_POINT('Ctrl Pts',(1.93874543614596,2.89005943164153,31.9781344828902));
#62697=CARTESIAN_POINT('Ctrl Pts',(-1.38428530244174,3.19295029495303,32.1372840812838));
#62698=CARTESIAN_POINT('Ctrl Pts',(-3.43468875149016,0.560437833290886,
32.2964336796773));
#62699=CARTESIAN_POINT('Ctrl Pts',(-2.32744931542688,-2.58730691428671,
32.4555832780709));
#62700=CARTESIAN_POINT('Ctrl Pts',(0.919504750710926,-3.35643983977321,
32.6147328764645));
#62701=CARTESIAN_POINT('Ctrl Pts',(3.32112235582321,-1.03986714644137,32.7738824748581));
#62702=CARTESIAN_POINT('Ctrl Pts',(2.66950307800085,2.2326958371308,32.9330320732517));
#62703=CARTESIAN_POINT('Ctrl Pts',(-0.436294150407741,3.45265474655611,
33.0921816716452));
#62704=CARTESIAN_POINT('Ctrl Pts',(-3.14098920638393,1.49845393321781,33.2513312700388));
#62705=CARTESIAN_POINT('Ctrl Pts',(-2.95805078598005,-1.83333382998357,
33.4104808684324));
#62706=CARTESIAN_POINT('Ctrl Pts',(-0.0556612903949957,-3.47966653651546,
33.569630466826));
#62707=CARTESIAN_POINT('Ctrl Pts',(2.89789979315677,-1.92700653175223,33.7287800652195));
#62708=CARTESIAN_POINT('Ctrl Pts',(3.18730894747029,1.39722548573591,33.8879296636131));
#62709=CARTESIAN_POINT('Ctrl Pts',(0.546501086838704,3.43693380015624,34.0470792620067));
#62710=CARTESIAN_POINT('Ctrl Pts',(-2.59672646692132,2.31693526896525,34.2062288604002));
#62711=CARTESIAN_POINT('Ctrl Pts',(-3.35268243771507,-0.93311192069785,
34.3653784587938));
#62712=CARTESIAN_POINT('Ctrl Pts',(-1.02638711541363,-3.32531304898012,
34.5245280571874));
#62713=CARTESIAN_POINT('Ctrl Pts',(2.2435057805037,-2.66042462727713,34.683677655581));
#62714=CARTESIAN_POINT('Ctrl Pts',(3.45085660129929,0.450295572495346,34.8428272539745));
#62715=CARTESIAN_POINT('Ctrl Pts',(1.48570080382082,3.14704154797274,35.0019768523681));
#62716=CARTESIAN_POINT('Ctrl Pts',(-1.84531749526043,2.95058989467884,35.1611264507617));
#62717=CARTESIAN_POINT('Ctrl Pts',(-3.47986368959678,0.0415462526435041,
35.3202760491553));
#62718=CARTESIAN_POINT('Ctrl Pts',(-1.91523591975808,-2.90569247263341,
35.4794256475488));
#62719=CARTESIAN_POINT('Ctrl Pts',(1.41014267708635,-3.18161515899672,35.6385752459424));
#62720=CARTESIAN_POINT('Ctrl Pts',(3.43912230342089,-0.532555344832574,
35.797724844336));
#62721=CARTESIAN_POINT('Ctrl Pts',(2.30638309143408,2.60610328701889,35.9568744427296));
#62722=CARTESIAN_POINT('Ctrl Pts',(-0.946703720385058,3.34886988492517,
36.1160240411231));
#62723=CARTESIAN_POINT('Ctrl Pts',(-3.32944906139014,1.01289017147471,36.2751736395167));
#62724=CARTESIAN_POINT('Ctrl Pts',(-2.65130234024599,-2.25427876213499,
36.4343232379102));
#62725=CARTESIAN_POINT('Ctrl Pts',(0.464289466150589,-3.44900176816319,
36.5934728363039));
#62726=CARTESIAN_POINT('Ctrl Pts',(3.15304233706577,-1.47292305497444,36.7526224346974));
#62727=CARTESIAN_POINT('Ctrl Pts',(2.94308002069685,1.85727046589526,36.911772033091));
#62728=CARTESIAN_POINT('Ctrl Pts',(0.0274313606274201,3.48000422041144,
37.0709216314846));
#62729=CARTESIAN_POINT('Ctrl Pts',(-2.91343892506985,1.90343258514806,37.2300712298781));
#62730=CARTESIAN_POINT('Ctrl Pts',(-3.17586600267692,-1.4230343579686,37.3892208282717));
#62731=CARTESIAN_POINT('Ctrl Pts',(-0.518606599465324,-3.44125862475635,
37.5483704266653));
#62732=CARTESIAN_POINT('Ctrl Pts',(2.61544821472821,-2.29578456290637,37.7075200250589));
#62733=CARTESIAN_POINT('Ctrl Pts',(3.34498126840255,0.960263912504391,37.8666696234524));
#62734=CARTESIAN_POINT('Ctrl Pts',(0.999416555317858,3.33356087664399,38.025819221846));
#62735=CARTESIAN_POINT('Ctrl Pts',(-2.26509095496236,2.64207807872185,38.1849688202396));
#62736=CARTESIAN_POINT('Ctrl Pts',(-3.44694460696967,-0.478164392868984,
38.3441184186332));
#62737=CARTESIAN_POINT('Ctrl Pts',(-1.46039886746108,-3.15920366970597,
38.5032680170267));
#62738=CARTESIAN_POINT('Ctrl Pts',(1.86972333428146,-2.93511622232055,38.6624176154203));
#62739=CARTESIAN_POINT('Ctrl Pts',(3.47907139646688,-0.0140916651033557,
38.8215672138139));
#62740=CARTESIAN_POINT('Ctrl Pts',(1.89357215294747,2.92263494718828,38.9807168122074));
#62741=CARTESIAN_POINT('Ctrl Pts',(-1.43998038369654,3.16705211734282,39.1398664106011));
#62742=CARTESIAN_POINT('Ctrl Pts',(-2.7687072675905,1.39687744165701,39.2459661428634));
#62743=CARTESIAN_POINT('Ctrl Pts',(-2.91090525077878,0.426608275808765,
39.2990160089946));
#62744=CARTESIAN_POINT('Ctrl Pts',(1.59774743137961,-2.24059110187415,-0.219489327336922));
#62745=CARTESIAN_POINT('Ctrl Pts',(2.34458605102921,-1.70802650978855,-0.166439461205731));
#62746=CARTESIAN_POINT('Ctrl Pts',(3.25063923968512,0.153557917939087,-0.0603397289433482));
#62747=CARTESIAN_POINT('Ctrl Pts',(1.62409624279688,2.82369221612243,0.0988098694502261));
#62748=CARTESIAN_POINT('Ctrl Pts',(-1.49696874765322,2.88957558687682,0.2579594678438));
#62749=CARTESIAN_POINT('Ctrl Pts',(-3.2410619746254,0.30312732483917,0.417109066237375));
#62750=CARTESIAN_POINT('Ctrl Pts',(-2.00591445868996,-2.56415991055002,
0.576258664630948));
#62751=CARTESIAN_POINT('Ctrl Pts',(1.07355449255992,-3.0729844518909,0.735408263024524));
#62752=CARTESIAN_POINT('Ctrl Pts',(3.16595493165337,-0.757287358952449,
0.894557861418096));
#62753=CARTESIAN_POINT('Ctrl Pts',(2.34782661214163,2.25492392933661,1.05370745981167));
#62754=CARTESIAN_POINT('Ctrl Pts',(-0.628779687067362,3.19393325538333,
1.21285705820524));
#62755=CARTESIAN_POINT('Ctrl Pts',(-3.02730880575264,1.19672088192463,1.37200665659882));
#62756=CARTESIAN_POINT('Ctrl Pts',(-2.64272342139147,-1.90072822769928,
1.53115625499239));
#62757=CARTESIAN_POINT('Ctrl Pts',(0.171424612330327,-3.25074055650477,
1.69030585338597));
#62758=CARTESIAN_POINT('Ctrl Pts',(2.8279730938224,-1.61223300963656,1.84945545177954));
#62759=CARTESIAN_POINT('Ctrl Pts',(2.88465715435138,1.50846945320346,2.00860505017312));
#62760=CARTESIAN_POINT('Ctrl Pts',(0.289363142217337,3.24237393471646,2.16775464856669));
#62761=CARTESIAN_POINT('Ctrl Pts',(-2.57195333199973,1.99543978679069,2.32690424696027));
#62762=CARTESIAN_POINT('Ctrl Pts',(-3.06877329840881,-1.08598065252297,
2.48605384535384));
#62763=CARTESIAN_POINT('Ctrl Pts',(-0.74435059115853,-3.16901637694623,
2.64520344374742));
#62764=CARTESIAN_POINT('Ctrl Pts',(2.26438250301455,-2.33865241230782,2.80435304214099));
#62765=CARTESIAN_POINT('Ctrl Pts',(3.19138076371783,0.641725758369828,2.96350264053456));
#62766=CARTESIAN_POINT('Ctrl Pts',(1.18441861774923,3.03214042374254,3.12265223892814));
#62767=CARTESIAN_POINT('Ctrl Pts',(-1.91142559845319,2.63499056654934,3.28180183732171));
#62768=CARTESIAN_POINT('Ctrl Pts',(-3.25002196309905,-0.184608567080839,
3.44095143571529));
#62769=CARTESIAN_POINT('Ctrl Pts',(-1.60074679787117,-2.8344898586703,3.60010103410886));
#62770=CARTESIAN_POINT('Ctrl Pts',(1.52015712313799,-2.87851444399281,3.75925063250244));
#62771=CARTESIAN_POINT('Ctrl Pts',(3.24352150863317,-0.276208802353544,
3.91840023089601));
#62772=CARTESIAN_POINT('Ctrl Pts',(1.98499048631045,2.58002632683958,4.07754982928958));
#62773=CARTESIAN_POINT('Ctrl Pts',(-1.0984194520178,3.06434296175893,4.23669942768315));
#62774=CARTESIAN_POINT('Ctrl Pts',(-3.17200968957183,0.731489992034621,
4.39584902607674));
#62775=CARTESIAN_POINT('Ctrl Pts',(-2.32944811466034,-2.27385016220058,
4.5549986244703));
#62776=CARTESIAN_POINT('Ctrl Pts',(0.654665664139852,-3.18875147157931,
4.71414822286388));
#62777=CARTESIAN_POINT('Ctrl Pts',(3.03691984923879,-1.17210959747432,4.87329782125745));
#62778=CARTESIAN_POINT('Ctrl Pts',(2.62721556343934,1.92209819270584,5.03244741965103));
#62779=CARTESIAN_POINT('Ctrl Pts',(-0.197790116974089,3.2492463970658,5.19159701804461));
#62780=CARTESIAN_POINT('Ctrl Pts',(-2.84095965420498,1.58923608138611,5.35074661643817));
#62781=CARTESIAN_POINT('Ctrl Pts',(-2.8723245453524,-1.53182074191662,5.50989621483176));
#62782=CARTESIAN_POINT('Ctrl Pts',(-0.263049826745572,-3.24461521106184,
5.66904581322532));
#62783=CARTESIAN_POINT('Ctrl Pts',(2.58805682306418,-1.97450878949499,5.82819541161891));
#62784=CARTESIAN_POINT('Ctrl Pts',(3.05986223049256,1.11084031688059,5.98734501001246));
#62785=CARTESIAN_POINT('Ctrl Pts',(0.718617344107592,3.1749507385077,6.14649460840606));
#62786=CARTESIAN_POINT('Ctrl Pts',(-2.28328040136243,2.3202055270938,6.30564420679962));
#62787=CARTESIAN_POINT('Ctrl Pts',(-3.18606971642545,-0.667594818193805,
6.4647938051932));
#62788=CARTESIAN_POINT('Ctrl Pts',(-1.15978128982235,-3.04164929585589,
6.62394340358677));
#62789=CARTESIAN_POINT('Ctrl Pts',(1.93273916042609,-2.61939733850326,6.78309300198035));
#62790=CARTESIAN_POINT('Ctrl Pts',(3.24841736956942,0.210968415366401,6.94224260037392));
#62791=CARTESIAN_POINT('Ctrl Pts',(1.57769921588541,2.84738270406301,7.1013921987675));
#62792=CARTESIAN_POINT('Ctrl Pts',(-1.54345915650127,2.86608738726072,7.26054179716106));
#62793=CARTESIAN_POINT('Ctrl Pts',(-3.24565552778308,0.249886522593035,
7.41969139555465));
#62794=CARTESIAN_POINT('Ctrl Pts',(-1.96399460475218,-2.5960447360758,7.57884099394821));
#62795=CARTESIAN_POINT('Ctrl Pts',(1.12324290433852,-3.0553311534195,7.7379905923418));
#62796=CARTESIAN_POINT('Ctrl Pts',(3.17783954790743,-0.705732872238579,
7.89714019073536));
#62797=CARTESIAN_POINT('Ctrl Pts',(2.31092476365828,2.29267307218309,8.05628978912895));
#62798=CARTESIAN_POINT('Ctrl Pts',(-0.680512987869373,3.18333553879317,
8.21543938752251));
#62799=CARTESIAN_POINT('Ctrl Pts',(-3.04632869622369,1.14743389951957,8.3745889859161));
#62800=CARTESIAN_POINT('Ctrl Pts',(-2.61153601490394,-1.94334832751677,
8.53373858430965));
#62801=CARTESIAN_POINT('Ctrl Pts',(0.22414324255659,-3.24753489373382,8.69288818270324));
#62802=CARTESIAN_POINT('Ctrl Pts',(2.85375890406606,-1.56613639146347,8.8520377810968));
#62803=CARTESIAN_POINT('Ctrl Pts',(2.85980307155329,1.55507217553943,9.0111873794904));
#62804=CARTESIAN_POINT('Ctrl Pts',(0.236719106893722,3.24664244160548,9.17033697788396));
#62805=CARTESIAN_POINT('Ctrl Pts',(-2.60398993466071,1.95344810511779,9.32948657627754));
#62806=CARTESIAN_POINT('Ctrl Pts',(-3.050749804979,-1.13562701034412,9.48863617467111));
#62807=CARTESIAN_POINT('Ctrl Pts',(-0.69283678848375,-3.1806760702288,9.64778577306469));
#62808=CARTESIAN_POINT('Ctrl Pts',(2.30202802014995,-2.30160597706191,9.80693537145825));
#62809=CARTESIAN_POINT('Ctrl Pts',(3.18054898365337,0.693419960618418,9.96608496985184));
#62810=CARTESIAN_POINT('Ctrl Pts',(1.13506762973426,3.05095797334739,10.1252345682454));
#62811=CARTESIAN_POINT('Ctrl Pts',(-1.9539255194228,2.60363172198968,10.284384166639));
#62812=CARTESIAN_POINT('Ctrl Pts',(-3.2465989840766,-0.237314381770985,
10.4435337650326));
#62813=CARTESIAN_POINT('Ctrl Pts',(-1.55454779837227,-2.86008814930212,
10.6026833634261));
#62814=CARTESIAN_POINT('Ctrl Pts',(1.56665960795514,-2.85347170163021,10.7618329618197));
#62815=CARTESIAN_POINT('Ctrl Pts',(3.24757593629035,-0.223547796299663,
10.9209825602133));
#62816=CARTESIAN_POINT('Ctrl Pts',(1.94286946412048,2.61189228809128,11.0801321586069));
#62817=CARTESIAN_POINT('Ctrl Pts',(-1.1479924311337,3.04611826055101,11.2392817570004));
#62818=CARTESIAN_POINT('Ctrl Pts',(-3.18346025880061,0.679929305030804,
11.398431355394));
#62819=CARTESIAN_POINT('Ctrl Pts',(-2.2922493206328,-2.3113450913399,11.5575809537876));
#62820=CARTESIAN_POINT('Ctrl Pts',(0.706315524074037,-3.17771009685506,
11.7167305521812));
#62821=CARTESIAN_POINT('Ctrl Pts',(3.05553705105848,-1.12268268393673,11.8758801505747));
#62822=CARTESIAN_POINT('Ctrl Pts',(2.59568458981499,1.9644705621107,12.0350297489683));
#62823=CARTESIAN_POINT('Ctrl Pts',(-0.250481616296216,3.24560965599688,
12.1941793473619));
#62824=CARTESIAN_POINT('Ctrl Pts',(-2.86637033563197,1.54293362728653,12.3533289457555));
#62825=CARTESIAN_POINT('Ctrl Pts',(-2.84709338166566,-1.57822126309276,
12.512478544149));
#62826=CARTESIAN_POINT('Ctrl Pts',(-0.210372807527127,-3.24845599647828,
12.6716281425426));
#62827=CARTESIAN_POINT('Ctrl Pts',(2.61975166634493,-1.9322588558176,12.8307777409362));
#62828=CARTESIAN_POINT('Ctrl Pts',(3.04143659634136,1.16033896325084,12.9899273393297));
#62829=CARTESIAN_POINT('Ctrl Pts',(0.66701063425504,3.1861920678128,13.1490769377233));
#62830=CARTESIAN_POINT('Ctrl Pts',(-2.3206241324531,2.28285494832214,13.3082265361169));
#62831=CARTESIAN_POINT('Ctrl Pts',(-3.1748189251083,-0.719199466057081,
13.4673761345105));
#62832=CARTESIAN_POINT('Ctrl Pts',(-1.11027926590465,-3.06006585401438,
13.626525732904));
#62833=CARTESIAN_POINT('Ctrl Pts',(1.97498328207596,-2.58769474913928,13.7856753312976));
#62834=CARTESIAN_POINT('Ctrl Pts',(3.24456692577273,0.263644729483094,13.9448249296912));
#62835=CARTESIAN_POINT('Ctrl Pts',(1.53129406930187,2.87260535969066,14.1039745280848));
#62836=CARTESIAN_POINT('Ctrl Pts',(-1.58975695072081,2.84066821660634,14.2631241264783));
#62837=CARTESIAN_POINT('Ctrl Pts',(-3.24928260768908,0.197194357352772,
14.4222737248719));
#62838=CARTESIAN_POINT('Ctrl Pts',(-1.9216164547924,-2.62756794010615,14.5814233232655));
#62839=CARTESIAN_POINT('Ctrl Pts',(1.17266640354997,-3.03670488938056,14.7405729216591));
#62840=CARTESIAN_POINT('Ctrl Pts',(3.18887145231711,-0.654080988715819,
14.8997225200526));
#62841=CARTESIAN_POINT('Ctrl Pts',(2.27342301470172,2.32986499081536,15.0588721184462));
#62842=CARTESIAN_POINT('Ctrl Pts',(-0.732071574579563,3.17187551598343,
15.2180217168398));
#62843=CARTESIAN_POINT('Ctrl Pts',(-3.06454430769971,1.09785757971964,15.3771713152334));
#62844=CARTESIAN_POINT('Ctrl Pts',(-2.57966233142462,-1.98546350634593,
15.5363209136269));
#62845=CARTESIAN_POINT('Ctrl Pts',(0.276803504750348,-3.24347081056088,
15.6954705120205));
#62846=CARTESIAN_POINT('Ctrl Pts',(2.87879311888926,-1.51962931593148,15.8546201104141));
#62847=CARTESIAN_POINT('Ctrl Pts',(2.83419631216968,1.60126648103505,16.0137697088077));
#62848=CARTESIAN_POINT('Ctrl Pts',(0.18401266261032,3.25005575632197,16.1729193072012));
#62849=CARTESIAN_POINT('Ctrl Pts',(-2.63534098076865,1.91094243615129,16.3320689055948));
#62850=CARTESIAN_POINT('Ctrl Pts',(-3.03192321752246,-1.1849745491996,16.4912185039884));
#62851=CARTESIAN_POINT('Ctrl Pts',(-0.64114058115313,-3.19149836822788,
16.650368102382));
#62852=CARTESIAN_POINT('Ctrl Pts',(2.33906751438082,-2.26395367496133,16.8095177007755));
#62853=CARTESIAN_POINT('Ctrl Pts',(3.1688799179103,0.744931637848302,16.9686672991691));
#62854=CARTESIAN_POINT('Ctrl Pts',(1.08541782976375,3.06897233842756,17.1278168975627));
#62855=CARTESIAN_POINT('Ctrl Pts',(-1.99591106248259,2.57158746883364,17.2869664959562));
#62856=CARTESIAN_POINT('Ctrl Pts',(-3.24232132839643,-0.289957725587986,
17.4461160943498));
#62857=CARTESIAN_POINT('Ctrl Pts',(-1.50793955910327,-2.8849335114165,17.6052656927434));
#62858=CARTESIAN_POINT('Ctrl Pts',(1.6127496646616,-2.82767777484218,17.764415291137));
#62859=CARTESIAN_POINT('Ctrl Pts',(3.25077542965584,-0.17082794018687,17.9235648895305));
#62860=CARTESIAN_POINT('Ctrl Pts',(1.90023697552094,2.64307066043752,18.0827144879241));
#62861=CARTESIAN_POINT('Ctrl Pts',(-1.19726319768579,3.02709165944306,18.2418640863177));
#62862=CARTESIAN_POINT('Ctrl Pts',(-3.19407277232272,0.628189624483898,
18.4010136847113));
#62863=CARTESIAN_POINT('Ctrl Pts',(-2.25444708490623,-2.34823155173427,
18.5601632831048));
#62864=CARTESIAN_POINT('Ctrl Pts',(0.757779444268192,-3.16583218017745,
18.7193128814984));
#62865=CARTESIAN_POINT('Ctrl Pts',(3.0733498733406,-1.07296022071643,18.878462479892));
#62866=CARTESIAN_POINT('Ctrl Pts',(2.56347029422739,2.00632577858539,19.0376120782856));
#62867=CARTESIAN_POINT('Ctrl Pts',(-0.303107175560938,3.24111849819258,
19.1967616766791));
#62868=CARTESIAN_POINT('Ctrl Pts',(-2.89102643624049,1.49622499115646,19.3559112750727));
#62869=CARTESIAN_POINT('Ctrl Pts',(-2.82111271187761,-1.62420631266014,
19.5150608734663));
#62870=CARTESIAN_POINT('Ctrl Pts',(-0.15764040701926,-3.25144161584941,
19.6742104718599));
#62871=CARTESIAN_POINT('Ctrl Pts',(2.65075685193123,-1.88950024904527,19.8333600702534));
#62872=CARTESIAN_POINT('Ctrl Pts',(3.02221029463916,1.20953214681529,19.992509668647));
#62873=CARTESIAN_POINT('Ctrl Pts',(0.615228331798773,3.19659462224329,20.1516592670406));
#62874=CARTESIAN_POINT('Ctrl Pts',(-2.35735695209384,2.24490340095456,20.3108088654341));
#62875=CARTESIAN_POINT('Ctrl Pts',(-3.16273235293131,-0.770614782445889,
20.4699584638278));
#62876=CARTESIAN_POINT('Ctrl Pts',(-1.06048495755082,-3.07767684041242,
20.6291080622213));
#62877=CARTESIAN_POINT('Ctrl Pts',(2.01670748329427,-2.55531094116301,20.7882576606149));
#62878=CARTESIAN_POINT('Ctrl Pts',(3.23986233974024,0.316251638312774,20.9474072590085));
#62879=CARTESIAN_POINT('Ctrl Pts',(1.4844858048385,2.89707179311033,21.106556857402));
#62880=CARTESIAN_POINT('Ctrl Pts',(-1.63563623652694,2.81450123129526,21.2657064557956));
#62881=CARTESIAN_POINT('Ctrl Pts',(-3.25205430394149,0.14445028009062,21.4248560541892));
#62882=CARTESIAN_POINT('Ctrl Pts',(-1.8787324333827,-2.65839942878388,21.5840056525828));
#62883=CARTESIAN_POINT('Ctrl Pts',(1.2217811947191,-3.01727920342704,21.7431552509763));
#62884=CARTESIAN_POINT('Ctrl Pts',(3.19906387649592,-0.602256916358366,
21.9023048493699));
#62885=CARTESIAN_POINT('Ctrl Pts',(2.23532278013483,2.36644356531332,22.0614544477634));
#62886=CARTESIAN_POINT('Ctrl Pts',(-0.783437441193132,3.15958048717536,
22.2206040461571));
#62887=CARTESIAN_POINT('Ctrl Pts',(-3.08195316844857,1.04799224553065,22.3797536445506));
#62888=CARTESIAN_POINT('Ctrl Pts',(-2.54710954389172,-2.02705600579221,
22.5389032429442));
#62889=CARTESIAN_POINT('Ctrl Pts',(0.329390897568978,-3.23855287370784,
22.6980528413378));
#62890=CARTESIAN_POINT('Ctrl Pts',(2.90306948255782,-1.47272219330192,22.8572024397313));
#62891=CARTESIAN_POINT('Ctrl Pts',(2.80784344187814,1.64703924819794,23.0163520381249));
#62892=CARTESIAN_POINT('Ctrl Pts',(0.131257776426808,3.2526134838511,23.1755016365185));
#62893=CARTESIAN_POINT('Ctrl Pts',(-2.66599826524709,1.86793370570319,23.3346512349121));
#62894=CARTESIAN_POINT('Ctrl Pts',(-3.01229846694121,-1.23401013985552,
23.4938008333056));
#62895=CARTESIAN_POINT('Ctrl Pts',(-0.589275591589926,-3.20148049445235,
23.6529504316992));
#62896=CARTESIAN_POINT('Ctrl Pts',(2.37549124188466,-2.22570538008331,23.8121000300928));
#62897=CARTESIAN_POINT('Ctrl Pts',(3.15637663476935,0.796247209530284,23.9712496284864));
#62898=CARTESIAN_POINT('Ctrl Pts',(1.03548229020669,3.08617878708782,24.1303992268799));
#62899=CARTESIAN_POINT('Ctrl Pts',(-2.03737117580815,2.53886623735648,24.2895488252735));
#62900=CARTESIAN_POINT('Ctrl Pts',(-3.23719012164088,-0.3425247371407,24.4486984236671));
#62901=CARTESIAN_POINT('Ctrl Pts',(-1.46093435010116,-2.90901940589901,
24.6078480220607));
#62902=CARTESIAN_POINT('Ctrl Pts',(1.65841516005192,-2.80113945317124,24.7669976204542));
#62903=CARTESIAN_POINT('Ctrl Pts',(3.25311914637773,-0.118063113092684,
24.9261472188478));
#62904=CARTESIAN_POINT('Ctrl Pts',(1.85710424368523,2.67355323629226,25.0852968172414));
#62905=CARTESIAN_POINT('Ctrl Pts',(-1.24621878101377,3.00726816713295,25.244446415635));
#62906=CARTESIAN_POINT('Ctrl Pts',(-3.20384443635041,0.576284571083659,
25.4035960140285));
#62907=CARTESIAN_POINT('Ctrl Pts',(-2.21605135904132,-2.38449983294058,
25.5627456124222));
#62908=CARTESIAN_POINT('Ctrl Pts',(0.80904387668984,-3.1531208484283,25.7218952108157));
#62909=CARTESIAN_POINT('Ctrl Pts',(3.09035362680328,-1.02295529741349,25.8810448092093));
#62910=CARTESIAN_POINT('Ctrl Pts',(2.53058115718985,2.04765282361984,26.0401944076028));
#62911=CARTESIAN_POINT('Ctrl Pts',(-0.355652940928235,3.2357741059616,26.1993440059964));
#62912=CARTESIAN_POINT('Ctrl Pts',(-2.9149214652359,1.44912246918937,26.3584936043899));
#62913=CARTESIAN_POINT('Ctrl Pts',(-2.79438937547971,-1.66976378491353,
26.5176432027836));
#62914=CARTESIAN_POINT('Ctrl Pts',(-0.104866507188719,-3.25357128320136,
26.6767928011771));
#62915=CARTESIAN_POINT('Ctrl Pts',(2.68106421761248,-1.84624422551311,26.8359423995708));
#62916=CARTESIAN_POINT('Ctrl Pts',(3.00218838676911,1.25840691731703,26.9950919979642));
#62917=CARTESIAN_POINT('Ctrl Pts',(0.563284068589358,3.20615566329458,27.1542415963579));
#62918=CARTESIAN_POINT('Ctrl Pts',(-2.39346919025677,2.20636087585285,27.3133911947514));
#62919=CARTESIAN_POINT('Ctrl Pts',(-3.14981318172185,-0.821827232119886,
27.472540793145));
#62920=CARTESIAN_POINT('Ctrl Pts',(-1.0104114732658,-3.09447761890361,27.6316903915386));
#62921=CARTESIAN_POINT('Ctrl Pts',(2.0579007800566,-2.52225443971164,27.7908399899321));
#62922=CARTESIAN_POINT('Ctrl Pts',(3.23430484996867,0.368775292924697,27.9499895883257));
#62923=CARTESIAN_POINT('Ctrl Pts',(1.43728674491509,2.92077556345809,28.1091391867193));
#62924=CARTESIAN_POINT('Ctrl Pts',(-1.68108493605638,2.78759331986695,28.2682887851129));
#62925=CARTESIAN_POINT('Ctrl Pts',(-3.25396988688269,0.0916681758473751,
28.4274383835065));
#62926=CARTESIAN_POINT('Ctrl Pts',(-1.83535382987383,-2.68853108562466,
28.5865879819));
#62927=CARTESIAN_POINT('Ctrl Pts',(1.27057434822587,-2.99705920943062,28.7457375802936));
#62928=CARTESIAN_POINT('Ctrl Pts',(3.20841413725675,-0.550274298012868,
28.9048871786872));
#62929=CARTESIAN_POINT('Ctrl Pts',(2.19663408996178,2.40239916625452,29.0640367770808));
#62930=CARTESIAN_POINT('Ctrl Pts',(-0.83459706548745,3.14645368907319,29.2231863754743));
#62931=CARTESIAN_POINT('Ctrl Pts',(-3.09855069553404,0.997851024155426,
29.3823359738679));
#62932=CARTESIAN_POINT('Ctrl Pts',(-2.51388622192681,-2.06811487650207,
29.5414855722615));
#62933=CARTESIAN_POINT('Ctrl Pts',(0.381891577219384,-3.23278237783669,
29.700635170655));
#62934=CARTESIAN_POINT('Ctrl Pts',(2.92658160424422,-1.42542737201929,29.8597847690487));
#62935=CARTESIAN_POINT('Ctrl Pts',(2.78075139815295,1.6923784272062,30.0189343674421));
#62936=CARTESIAN_POINT('Ctrl Pts',(0.078468336229367,3.25431495086323,30.1780839658358));
#62937=CARTESIAN_POINT('Ctrl Pts',(-2.6959537174715,1.82443323595418,30.3372335642293));
#62938=CARTESIAN_POINT('Ctrl Pts',(-2.99188071951124,-1.28272087354164,
30.4963831626229));
#62939=CARTESIAN_POINT('Ctrl Pts',(-0.53725547341239,-3.21061982107676,
30.6555327610165));
#62940=CARTESIAN_POINT('Ctrl Pts',(2.41128961400306,-2.18687116140927,30.81468235941));
#62941=CARTESIAN_POINT('Ctrl Pts',(3.14304242575827,0.847353166682053,30.9738319578037));
#62942=CARTESIAN_POINT('Ctrl Pts',(0.985274156747698,3.10257278967758,31.1329815561972));
#62943=CARTESIAN_POINT('Ctrl Pts',(-2.078294944897,2.50547664152315,31.2921311545908));
#62944=CARTESIAN_POINT('Ctrl Pts',(-3.2312067146159,-0.395001578001435,
31.4512807529843));
#62945=CARTESIAN_POINT('Ctrl Pts',(-1.41354454563206,-2.93233949206372,
31.610430351378));
#62946=CARTESIAN_POINT('Ctrl Pts',(1.70364407254376,-2.77386372291233,31.7695799497715));
#62947=CARTESIAN_POINT('Ctrl Pts',(3.25460646946541,-0.065267205520362,
31.9287295481651));
#62948=CARTESIAN_POINT('Ctrl Pts',(1.81348262343787,2.70333199102358,32.0878791465587));
#62949=CARTESIAN_POINT('Ctrl Pts',(-1.29484629340955,2.98665300221604,32.2470287449522));
#62950=CARTESIAN_POINT('Ctrl Pts',(-3.21277267846304,0.524227808995236,
32.4061783433458));
#62951=CARTESIAN_POINT('Ctrl Pts',(-2.17707225083119,-2.42014038722208,
32.5653279417394));
#62952=CARTESIAN_POINT('Ctrl Pts',(0.860095325819289,-3.13957944790481,
32.724477540133));
#62953=CARTESIAN_POINT('Ctrl Pts',(3.10654383515604,-0.972681077978029,
32.8836271385265));
#62954=CARTESIAN_POINT('Ctrl Pts',(2.49702583686903,2.08844081774213,33.0427767369201));
#62955=CARTESIAN_POINT('Ctrl Pts',(-0.408105079563564,3.22957788623167,
33.2019263353136));
#62956=CARTESIAN_POINT('Ctrl Pts',(-2.93804913217808,1.40163846126938,33.3610759337073));
#62957=CARTESIAN_POINT('Ctrl Pts',(-2.76693040747283,-1.71488168670816,
33.5202255321008));
#62958=CARTESIAN_POINT('Ctrl Pts',(-0.0520650009267163,-3.25484443789231,
33.6793751304944));
#62959=CARTESIAN_POINT('Ctrl Pts',(2.71066578488031,-1.80250217250329,33.838524728888));
#62960=CARTESIAN_POINT('Ctrl Pts',(2.98137614356199,1.30695040832354,33.9976743272815));
#62961=CARTESIAN_POINT('Ctrl Pts',(0.511191519110511,3.21487267399046,34.1568239256752));
#62962=CARTESIAN_POINT('Ctrl Pts',(-2.42895134027704,2.16723751946073,34.3159735240686));
#62963=CARTESIAN_POINT('Ctrl Pts',(-3.13606481250469,-0.872823333254088,
34.4751231224623));
#62964=CARTESIAN_POINT('Ctrl Pts',(-0.960071995023433,-3.11046376661199,
34.6342727208558));
#62965=CARTESIAN_POINT('Ctrl Pts',(2.09855232805267,-2.48853394704777,34.7934223192495));
#62966=CARTESIAN_POINT('Ctrl Pts',(3.22789591957588,0.421201866375226,34.9525719176429));
#62967=CARTESIAN_POINT('Ctrl Pts',(1.38970931465493,2.94371043050936,35.1117215160366));
#62968=CARTESIAN_POINT('Ctrl Pts',(-1.72609108446586,2.7599515661676,35.2708711144301));
#62969=CARTESIAN_POINT('Ctrl Pts',(-3.25502885286523,0.0388619391867563,
35.4300207128238));
#62970=CARTESIAN_POINT('Ctrl Pts',(-1.79149206260406,-2.7179549774465,35.5891703112173));
#62971=CARTESIAN_POINT('Ctrl Pts',(1.31903301680886,-2.97605023214225,35.7483199096108));
#62972=CARTESIAN_POINT('Ctrl Pts',(3.21691977752854,-0.498146814876754,
35.9074695080045));
#62973=CARTESIAN_POINT('Ctrl Pts',(2.15736712067839,2.43772232175455,36.066619106398));
#62974=CARTESIAN_POINT('Ctrl Pts',(-0.885536963467963,3.13249858967495,
36.2257687047916));
#62975=CARTESIAN_POINT('Ctrl Pts',(-3.11433255025735,0.947447091904948,
36.3849183031851));
#62976=CARTESIAN_POINT('Ctrl Pts',(-2.48000105319356,-2.10862926472869,
36.5440679015787));
#62977=CARTESIAN_POINT('Ctrl Pts',(0.434291611168368,-3.22616092765844,
36.7032174999723));
#62978=CARTESIAN_POINT('Ctrl Pts',(2.94932350716411,-1.37775713925967,36.8623670983659));
#62979=CARTESIAN_POINT('Ctrl Pts',(2.75292690696447,1.73727177076979,37.0215166967595));
#62980=CARTESIAN_POINT('Ctrl Pts',(0.0256590137662085,3.25516030394989,
37.180666295153));
#62981=CARTESIAN_POINT('Ctrl Pts',(-2.72520092971278,1.78045134430509,37.3398158935466));
#62982=CARTESIAN_POINT('Ctrl Pts',(-2.97067253020624,-1.33109176306352,
37.4989654919402));
#62983=CARTESIAN_POINT('Ctrl Pts',(-0.485099301329773,-3.21891807062454,
37.6581150903338));
#62984=CARTESIAN_POINT('Ctrl Pts',(2.44646347141876,-2.14745336564863,37.8172646887273));
#62985=CARTESIAN_POINT('Ctrl Pts',(3.12886121760872,0.898221028286588,37.9764142871209));
#62986=CARTESIAN_POINT('Ctrl Pts',(0.934844009354873,3.11817870013068,38.1355638855145));
#62987=CARTESIAN_POINT('Ctrl Pts',(-2.1187428791559,2.47137277344305,38.2947134839081));
#62988=CARTESIAN_POINT('Ctrl Pts',(-3.22423668014841,-0.447270075507296,
38.4538630823016));
#62989=CARTESIAN_POINT('Ctrl Pts',(-1.36604214253824,-2.95508675460852,
38.6130126806952));
#62990=CARTESIAN_POINT('Ctrl Pts',(1.74892005631017,-2.74547765153221,38.7721622790888));
#62991=CARTESIAN_POINT('Ctrl Pts',(3.25428774998656,-0.0131811992043684,
38.9313118774823));
#62992=CARTESIAN_POINT('Ctrl Pts',(1.77122799701979,2.73380279461243,39.0904614758759));
#62993=CARTESIAN_POINT('Ctrl Pts',(-1.34694290196035,2.96242811214064,39.2496110742695));
#62994=CARTESIAN_POINT('Ctrl Pts',(-2.58982041971561,1.30662485145711,39.3557108065319));
#62995=CARTESIAN_POINT('Ctrl Pts',(-2.72283095673202,0.399045011671065,
39.4087606726631));
#62996=CARTESIAN_POINT('Ctrl Pts',(1.48738611075523,-2.08582659521596,-0.109744663668461));
#62997=CARTESIAN_POINT('Ctrl Pts',(2.18263829393873,-1.59004787463046,-0.0566947975372698));
#62998=CARTESIAN_POINT('Ctrl Pts',(3.0261076070133,0.142951201080473,0.0494049347251129));
#62999=CARTESIAN_POINT('Ctrl Pts',(1.5119149288697,2.6286511252168,0.208554533118687));
#63000=CARTESIAN_POINT('Ctrl Pts',(-1.39356852013302,2.68998372927258,0.367704131512261));
#63001=CARTESIAN_POINT('Ctrl Pts',(-3.01719187305616,0.282189389825537,
0.526853729905836));
#63002=CARTESIAN_POINT('Ctrl Pts',(-1.86735978830055,-2.38704551282824,
0.68600332829941));
#63003=CARTESIAN_POINT('Ctrl Pts',(0.999400787641171,-2.86072398086276,
0.845152926692984));
#63004=CARTESIAN_POINT('Ctrl Pts',(2.94727270414218,-0.704979195982167,
1.00430252508656));
#63005=CARTESIAN_POINT('Ctrl Pts',(2.18565501954578,2.09916941027963,1.16345212348013));
#63006=CARTESIAN_POINT('Ctrl Pts',(-0.585347943549101,2.97331847915074,
1.32260172187371));
#63007=CARTESIAN_POINT('Ctrl Pts',(-2.81820329184044,1.11405969633679,1.48175132026728));
#63008=CARTESIAN_POINT('Ctrl Pts',(-2.46018240076365,-1.7694390932359,1.64090091866086));
#63009=CARTESIAN_POINT('Ctrl Pts',(0.159583788034279,-3.02620192556914,
1.80005051705443));
#63010=CARTESIAN_POINT('Ctrl Pts',(2.63263630955052,-1.50087112564727,1.95920011544801));
#63011=CARTESIAN_POINT('Ctrl Pts',(2.68540502798266,1.40427483664047,2.11834971384158));
#63012=CARTESIAN_POINT('Ctrl Pts',(0.269375941557349,3.01841321203564,2.27749931223515));
#63013=CARTESIAN_POINT('Ctrl Pts',(-2.39430061873041,1.85760863414959,2.43664891062873));
#63014=CARTESIAN_POINT('Ctrl Pts',(-2.85680370468111,-1.01096863458373,
2.5957985090223));
#63015=CARTESIAN_POINT('Ctrl Pts',(-0.69293601045933,-2.95012268600915,
2.75494810741588));
#63016=CARTESIAN_POINT('Ctrl Pts',(2.10797465123312,-2.17711450986188,2.91409770580944));
#63017=CARTESIAN_POINT('Ctrl Pts',(2.97094229592146,0.597399789958587,3.07324730420303));
#63018=CARTESIAN_POINT('Ctrl Pts',(1.10260718731943,2.82270117514133,3.23239690259659));
#63019=CARTESIAN_POINT('Ctrl Pts',(-1.77939756374786,2.45298367794754,3.39154650099018));
#63020=CARTESIAN_POINT('Ctrl Pts',(-3.02553296761625,-0.171857086551683,
3.55069609938375));
#63021=CARTESIAN_POINT('Ctrl Pts',(-1.49017830179445,-2.63870294144206,
3.70984569777733));
#63022=CARTESIAN_POINT('Ctrl Pts',(1.41515520332815,-2.67968661348843,3.86899529617089));
#63023=CARTESIAN_POINT('Ctrl Pts',(3.01948151949855,-0.25713021233551,4.02814489456448));
#63024=CARTESIAN_POINT('Ctrl Pts',(1.84788109893584,2.40181598703027,4.18729449295804));
#63025=CARTESIAN_POINT('Ctrl Pts',(-1.0225482480068,2.85267938498604,4.34644409135163));
#63026=CARTESIAN_POINT('Ctrl Pts',(-2.95290924134139,0.680963732402603,
4.50559368974519));
#63027=CARTESIAN_POINT('Ctrl Pts',(-2.16854598131273,-2.11678835013076,
4.66474328813878));
#63028=CARTESIAN_POINT('Ctrl Pts',(0.60944589670789,-2.96849461706362,4.82389288653233));
#63029=CARTESIAN_POINT('Ctrl Pts',(2.82715047104436,-1.0911483888671,4.98304248492593));
#63030=CARTESIAN_POINT('Ctrl Pts',(2.44574571817382,1.78933296914758,5.14219208331948));
#63031=CARTESIAN_POINT('Ctrl Pts',(-0.184128146322703,3.02481097231012,
5.30134168171307));
#63032=CARTESIAN_POINT('Ctrl Pts',(-2.64472584833504,1.47946266583818,5.46049128010663));
#63033=CARTESIAN_POINT('Ctrl Pts',(-2.67392427015187,-1.42601318014711,
5.61964087850022));
#63034=CARTESIAN_POINT('Ctrl Pts',(-0.244880167574575,-3.0204996765425,
5.77879047689378));
#63035=CARTESIAN_POINT('Ctrl Pts',(2.40929179222473,-1.83812340510121,5.93794007528737));
#63036=CARTESIAN_POINT('Ctrl Pts',(2.84850815158536,1.03411116559793,6.09708967368094));
#63037=CARTESIAN_POINT('Ctrl Pts',(0.668980237790581,2.9556471429974,6.25623927207451));
#63038=CARTESIAN_POINT('Ctrl Pts',(-2.12556721372019,2.15994180764678,6.41538887046809));
#63039=CARTESIAN_POINT('Ctrl Pts',(-2.96599809897198,-0.621481994395149,
6.57453846886165));
#63040=CARTESIAN_POINT('Ctrl Pts',(-1.07967163527606,-2.83155324026287,
6.73368806725523));
#63041=CARTESIAN_POINT('Ctrl Pts',(1.7992389325566,-2.43846752203824,6.89283766564881));
#63042=CARTESIAN_POINT('Ctrl Pts',(3.02403920828826,0.196396179183931,7.05198726404238));
#63043=CARTESIAN_POINT('Ctrl Pts',(1.46872268705907,2.65070523841879,7.21113686243596));
#63044=CARTESIAN_POINT('Ctrl Pts',(-1.43684769370316,2.66811793171942,7.37028646082953));
#63045=CARTESIAN_POINT('Ctrl Pts',(-3.02146813539374,0.232626093254943,
7.52943605922311));
#63046=CARTESIAN_POINT('Ctrl Pts',(-1.82833546738012,-2.41672795555947,
7.68858565761668));
#63047=CARTESIAN_POINT('Ctrl Pts',(1.04565706826066,-2.84429004991743,7.84773525601024));
#63048=CARTESIAN_POINT('Ctrl Pts',(2.95833641346242,-0.656985735952557,
8.00688485440384));
#63049=CARTESIAN_POINT('Ctrl Pts',(2.15130209503633,2.13431110392909,8.16603445279739));
#63050=CARTESIAN_POINT('Ctrl Pts',(-0.633507866428774,2.96345277938347,
8.32518405119099));
#63051=CARTESIAN_POINT('Ctrl Pts',(-2.83590942008017,1.0681771171315,8.48433364958454));
#63052=CARTESIAN_POINT('Ctrl Pts',(-2.43114920419642,-1.80911529190317,
8.64348324797814));
#63053=CARTESIAN_POINT('Ctrl Pts',(0.20866098060963,-3.02321768776808,8.80263284637168));
#63054=CARTESIAN_POINT('Ctrl Pts',(2.65664101471088,-1.45795854242112,8.96178244476528));
#63055=CARTESIAN_POINT('Ctrl Pts',(2.66226769299254,1.44765856586108,9.12093204315885));
#63056=CARTESIAN_POINT('Ctrl Pts',(0.220368191385691,3.02238688004832,9.28008164155242));
#63057=CARTESIAN_POINT('Ctrl Pts',(-2.4241243548841,1.81851744685623,9.439231239946));
#63058=CARTESIAN_POINT('Ctrl Pts',(-2.84002514927976,-1.05718576604174,
9.59838083833957));
#63059=CARTESIAN_POINT('Ctrl Pts',(-0.644980424297316,-2.96097700847812,
9.75753043673315));
#63060=CARTESIAN_POINT('Ctrl Pts',(2.14301987691753,-2.1426269856415,9.91668003512672));
#63061=CARTESIAN_POINT('Ctrl Pts',(2.96085870016269,0.645523314941969,10.0758296335203));
#63062=CARTESIAN_POINT('Ctrl Pts',(1.05666502356821,2.84021893881974,10.2349792319139));
#63063=CARTESIAN_POINT('Ctrl Pts',(-1.81896188468925,2.42379088506218,10.3941288303075));
#63064=CARTESIAN_POINT('Ctrl Pts',(-3.0223464242644,-0.220922348799343,
10.553278428701));
#63065=CARTESIAN_POINT('Ctrl Pts',(-1.447170409035,-2.66253307954591,10.7124280270946));
#63066=CARTESIAN_POINT('Ctrl Pts',(1.45844561874313,-2.65637365022915,10.8715776254882));
#63067=CARTESIAN_POINT('Ctrl Pts',(3.02325589538921,-0.208106663654035,
11.0307272238817));
#63068=CARTESIAN_POINT('Ctrl Pts',(1.80866950507204,2.43148086850076,11.1898768222753));
#63069=CARTESIAN_POINT('Ctrl Pts',(-1.06869706925202,2.83571351984556,11.3490264206689));
#63070=CARTESIAN_POINT('Ctrl Pts',(-2.96356888459703,0.632964500356112,
11.5081760190625));
#63071=CARTESIAN_POINT('Ctrl Pts',(-2.13391662219954,-2.15169338939434,
11.667325617456));
#63072=CARTESIAN_POINT('Ctrl Pts',(0.657528142236659,-2.95821590399173,
11.8264752158496));
#63073=CARTESIAN_POINT('Ctrl Pts',(2.84448172557426,-1.04513554400223,11.9856248142432));
#63074=CARTESIAN_POINT('Ctrl Pts',(2.41639268570676,1.82877854890243,12.1447744126368));
#63075=CARTESIAN_POINT('Ctrl Pts',(-0.233180082008765,3.02142543211266,
12.3039240110303));
#63076=CARTESIAN_POINT('Ctrl Pts',(-2.66838133597785,1.43635846440497,12.4630736094239));
#63077=CARTESIAN_POINT('Ctrl Pts',(-2.65043590040781,-1.46920867486283,
12.6222232078175));
#63078=CARTESIAN_POINT('Ctrl Pts',(-0.195841711806975,-3.02407516711792,
12.7813728062111));
#63079=CARTESIAN_POINT('Ctrl Pts',(2.43879737536789,-1.79879180406223,12.9405224046046));
#63080=CARTESIAN_POINT('Ctrl Pts',(2.83135523255693,1.08019078848846,13.0996720029982));
#63081=CARTESIAN_POINT('Ctrl Pts',(0.620938161834819,2.96611199917332,13.2588216013918));
#63082=CARTESIAN_POINT('Ctrl Pts',(-2.16033149864856,2.12517114802777,13.4179711997854));
#63083=CARTESIAN_POINT('Ctrl Pts',(-2.95552443435423,-0.669522150789567,
13.5771207981789));
#63084=CARTESIAN_POINT('Ctrl Pts',(-1.03358886813565,-2.84869771020528,
13.7362703965725));
#63085=CARTESIAN_POINT('Ctrl Pts',(1.83856512302265,-2.4089547278576,13.8954199949661));
#63086=CARTESIAN_POINT('Ctrl Pts',(3.02045472646657,0.245433978553323,14.0545695933596));
#63087=CARTESIAN_POINT('Ctrl Pts',(1.42552288642705,2.67418568778151,14.2137191917532));
#63088=CARTESIAN_POINT('Ctrl Pts',(-1.47994755712857,2.64445454122622,14.3728687901468));
#63089=CARTESIAN_POINT('Ctrl Pts',(-3.02484468175446,0.183573537647755,
14.5320183885404));
#63090=CARTESIAN_POINT('Ctrl Pts',(-1.78888450635103,-2.44607375510225,
14.6911679869339));
#63091=CARTESIAN_POINT('Ctrl Pts',(1.09166673463739,-2.82695035912358,14.8503175853276));
#63092=CARTESIAN_POINT('Ctrl Pts',(2.96860631036345,-0.608901606610685,
15.0094671837211));
#63093=CARTESIAN_POINT('Ctrl Pts',(2.11639070702123,2.16893406255168,15.1686167821147));
#63094=CARTESIAN_POINT('Ctrl Pts',(-0.681505143255366,2.95278433553472,
15.3277663805082));
#63095=CARTESIAN_POINT('Ctrl Pts',(-2.85286682334445,1.02202518595354,15.4869159789018));
#63096=CARTESIAN_POINT('Ctrl Pts',(-2.4014771338963,-1.84832144602502,15.6460655772954));
#63097=CARTESIAN_POINT('Ctrl Pts',(0.257683836811684,-3.01943432329778,
15.805215175689));
#63098=CARTESIAN_POINT('Ctrl Pts',(2.67994603945409,-1.41466385338607,15.9643647740825));
#63099=CARTESIAN_POINT('Ctrl Pts',(2.63842967109959,1.49066208884647,16.1235143724761));
#63100=CARTESIAN_POINT('Ctrl Pts',(0.171302343032715,3.02556442663749,16.2826639708697));
#63101=CARTESIAN_POINT('Ctrl Pts',(-2.45330988798075,1.77894777494975,16.4418135692633));
#63102=CARTESIAN_POINT('Ctrl Pts',(-2.82249897202182,-1.10312471887749,
16.6009631676568));
#63103=CARTESIAN_POINT('Ctrl Pts',(-0.596855032729077,-2.97105177712688,
16.7601127660504));
#63104=CARTESIAN_POINT('Ctrl Pts',(2.1775009395601,-2.10757544365029,16.919262364444));
#63105=CARTESIAN_POINT('Ctrl Pts',(2.94999565261784,0.693476922470085,17.0784119628376));
#63106=CARTESIAN_POINT('Ctrl Pts',(1.01044468772068,2.85698899639461,17.2375615612311));
#63107=CARTESIAN_POINT('Ctrl Pts',(-1.85804735738235,2.3939600268566,17.3967111596247));
#63108=CARTESIAN_POINT('Ctrl Pts',(-3.01836423939567,-0.269929455228868,
17.5558607580183));
#63109=CARTESIAN_POINT('Ctrl Pts',(-1.40378154395286,-2.68566229621672,
17.7150103564118));
#63110=CARTESIAN_POINT('Ctrl Pts',(1.50135209372329,-2.63236138915906,17.8741599548054));
#63111=CARTESIAN_POINT('Ctrl Pts',(3.02623438992458,-0.159028329867903,
18.033309553199));
#63112=CARTESIAN_POINT('Ctrl Pts',(1.76898177335394,2.46050565494257,18.1924591515926));
#63113=CARTESIAN_POINT('Ctrl Pts',(-1.1145645526831,2.81800114449322,18.3516087499861));
#63114=CARTESIAN_POINT('Ctrl Pts',(-2.97344835922673,0.584798638400112,
18.5107583483797));
#63115=CARTESIAN_POINT('Ctrl Pts',(-2.09872550295822,-2.18603198871735,
18.6699079467733));
#63116=CARTESIAN_POINT('Ctrl Pts',(0.705437291454138,-2.94715843148763,
18.8290575451669));
#63117=CARTESIAN_POINT('Ctrl Pts',(2.86106416153093,-0.99884756397866,18.9882071435604));
#63118=CARTESIAN_POINT('Ctrl Pts',(2.38640353042244,1.86774269706779,19.147356741954));
#63119=CARTESIAN_POINT('Ctrl Pts',(-0.282170632319641,3.01724449236703,
19.3065063403476));
#63120=CARTESIAN_POINT('Ctrl Pts',(-2.6913343640161,1.39287613718119,19.4656559387412));
#63121=CARTESIAN_POINT('Ctrl Pts',(-2.62624979525007,-1.51201739586941,
19.6248055371347));
#63122=CARTESIAN_POINT('Ctrl Pts',(-0.146751700105655,-3.02685456059239,
19.7839551355284));
#63123=CARTESIAN_POINT('Ctrl Pts',(2.46766093759102,-1.75898666554075,19.9431047339219));
#63124=CARTESIAN_POINT('Ctrl Pts',(2.8134569505435,1.12598604782707,20.1022543323155));
#63125=CARTESIAN_POINT('Ctrl Pts',(0.572732621995603,2.9757960172305,20.261403930709));
#63126=CARTESIAN_POINT('Ctrl Pts',(-2.19452706965651,2.08984103055892,20.4205535291026));
#63127=CARTESIAN_POINT('Ctrl Pts',(-2.94427271882673,-0.717386053415761,
20.5797031274962));
#63128=CARTESIAN_POINT('Ctrl Pts',(-0.987234005542506,-2.86509225170207,
20.7388527258898));
#63129=CARTESIAN_POINT('Ctrl Pts',(1.87740730555765,-2.37880776892575,20.8980023242833));
#63130=CARTESIAN_POINT('Ctrl Pts',(3.01607510063576,0.294407166671968,21.057151922677));
#63131=CARTESIAN_POINT('Ctrl Pts',(1.38194781250485,2.69696214952598,21.2163015210705));
#63132=CARTESIAN_POINT('Ctrl Pts',(-1.52265781980161,2.62009498993066,21.3754511194641));
#63133=CARTESIAN_POINT('Ctrl Pts',(-3.02742492843683,0.134472655741415,
21.5346007178576));
#63134=CARTESIAN_POINT('Ctrl Pts',(-1.74896261596624,-2.47477561819557,
21.6937503162512));
#63135=CARTESIAN_POINT('Ctrl Pts',(1.13738901638409,-2.80886646494126,21.8528999146448));
#63136=CARTESIAN_POINT('Ctrl Pts',(2.97809471251059,-0.560657182045595,
22.0120495130384));
#63137=CARTESIAN_POINT('Ctrl Pts',(2.08092217263444,2.20298604260242,22.1711991114319));
#63138=CARTESIAN_POINT('Ctrl Pts',(-0.729323011754126,2.94133856211567,
22.3303487098256));
#63139=CARTESIAN_POINT('Ctrl Pts',(-2.86907320063122,0.975604203497742,
22.489498308219));
#63140=CARTESIAN_POINT('Ctrl Pts',(-2.37117286734461,-1.88704102383374,
22.6486479066127));
#63141=CARTESIAN_POINT('Ctrl Pts',(0.306638856950085,-3.01485608344266,
22.8077975050062));
#63142=CARTESIAN_POINT('Ctrl Pts',(2.70254556014871,-1.37099674973474,22.9669471033998));
#63143=CARTESIAN_POINT('Ctrl Pts',(2.61389707446989,1.53327319044601,23.1260967017934));
#63144=CARTESIAN_POINT('Ctrl Pts',(0.1221913988104,3.02794548407324,23.2852463001869));
#63145=CARTESIAN_POINT('Ctrl Pts',(-2.48184957969368,1.73890978956272,23.4443958985805));
#63146=CARTESIAN_POINT('Ctrl Pts',(-2.80422976321679,-1.1487732707336,23.6035454969741));
#63147=CARTESIAN_POINT('Ctrl Pts',(-0.548572517235271,-2.98034440724506,
23.7626950953677));
#63148=CARTESIAN_POINT('Ctrl Pts',(2.21140876837405,-2.07196907593263,23.9218446937612));
#63149=CARTESIAN_POINT('Ctrl Pts',(2.93835600963208,0.741247970062597,24.0809942921549));
#63150=CARTESIAN_POINT('Ctrl Pts',(0.963958349197132,2.87300694281721,24.2401438905484));
#63151=CARTESIAN_POINT('Ctrl Pts',(-1.89664369338618,2.36349895130105,24.399293488942));
#63152=CARTESIAN_POINT('Ctrl Pts',(-3.013587460845,-0.318865501897966,24.5584430873356));
#63153=CARTESIAN_POINT('Ctrl Pts',(-1.36002312905589,-2.70808450401678,
24.7175926857291));
#63154=CARTESIAN_POINT('Ctrl Pts',(1.54386333314095,-2.60765615084613,24.8767422841227));
#63155=CARTESIAN_POINT('Ctrl Pts',(3.02841621893663,-0.109908131384133,
25.0358918825163));
#63156=CARTESIAN_POINT('Ctrl Pts',(1.72882835173588,2.48888270569285,25.1950414809098));
#63157=CARTESIAN_POINT('Ctrl Pts',(-1.16013862356305,2.79954692166073,25.3541910793034));
#63158=CARTESIAN_POINT('Ctrl Pts',(-2.98254506441825,0.536478826401498,
25.513340677697));
#63159=CARTESIAN_POINT('Ctrl Pts',(-2.0629818877646,-2.2197951083868,25.6724902760906));
#63160=CARTESIAN_POINT('Ctrl Pts',(0.753160732132038,-2.93532511044979,
25.8316398744841));
#63161=CARTESIAN_POINT('Ctrl Pts',(2.87689341353558,-0.952296634257589,
25.9907894728777));
#63162=CARTESIAN_POINT('Ctrl Pts',(2.35578614705909,1.90621515621594,26.1499390712713));
#63163=CARTESIAN_POINT('Ctrl Pts',(-0.331086900342577,3.01226925371626,
26.3090886696649));
#63164=CARTESIAN_POINT('Ctrl Pts',(-2.71357888999427,1.3490271310245,26.4682382680584));
#63165=CARTESIAN_POINT('Ctrl Pts',(-2.60137232174541,-1.55442807363986,
26.6273878664521));
#63166=CARTESIAN_POINT('Ctrl Pts',(-0.0976230555672867,-3.02883712528166,
26.7865374648456));
#63167=CARTESIAN_POINT('Ctrl Pts',(2.49587488047244,-1.71871846836224,26.9456870632392));
#63168=CARTESIAN_POINT('Ctrl Pts',(2.79481801732299,1.1714848878708,27.1048366616327));
#63169=CARTESIAN_POINT('Ctrl Pts',(0.524376308529718,2.98469664782127,27.2639862600263));
#63170=CARTESIAN_POINT('Ctrl Pts',(-2.22814492465468,2.05396075600249,27.4231358584199));
#63171=CARTESIAN_POINT('Ctrl Pts',(-2.93224591443823,-0.76506110195399,
27.5822854568135));
#63172=CARTESIAN_POINT('Ctrl Pts',(-0.940619250556885,-2.88073254883971,
27.741435055207));
#63173=CARTESIAN_POINT('Ctrl Pts',(1.91575525483747,-2.34803458152248,27.9005846536006));
#63174=CARTESIAN_POINT('Ctrl Pts',(3.01090148374579,0.343302851197289,28.0597342519942));
#63175=CARTESIAN_POINT('Ctrl Pts',(1.33800893656488,2.7190286276785,28.2188838503878));
#63176=CARTESIAN_POINT('Ctrl Pts',(-1.56496723811412,2.59504569055965,28.3780334487813));
#63177=CARTESIAN_POINT('Ctrl Pts',(-3.02920819618289,0.0853363734943193,
28.5371830471749));
#63178=CARTESIAN_POINT('Ctrl Pts',(-1.70858030578638,-2.5028259889856,28.6963326455685));
#63179=CARTESIAN_POINT('Ctrl Pts',(1.1828118769693,-2.79004312801131,28.8554822439621));
#63180=CARTESIAN_POINT('Ctrl Pts',(2.98679912205271,-0.51226516275064,29.0146318423556));
#63181=CARTESIAN_POINT('Ctrl Pts',(2.04490582907692,2.23645807979271,29.1737814407492));
#63182=CARTESIAN_POINT('Ctrl Pts',(-0.776948883723837,2.92911847226141,
29.3329310391428));
#63183=CARTESIAN_POINT('Ctrl Pts',(-2.88452428556178,0.928926390230714,
29.4920806375363));
#63184=CARTESIAN_POINT('Ctrl Pts',(-2.34024438223286,-1.92526383228128,
29.65123023593));
#63185=CARTESIAN_POINT('Ctrl Pts',(0.355513153465022,-3.00948417343838,
29.8103798343235));
#63186=CARTESIAN_POINT('Ctrl Pts',(2.72443362740134,-1.32696872696665,29.9695294327171));
#63187=CARTESIAN_POINT('Ctrl Pts',(2.58867636138508,1.575480653156,30.1286790311106));
#63188=CARTESIAN_POINT('Ctrl Pts',(0.0730482873259879,3.02952942553484,
30.2878286295043));
#63189=CARTESIAN_POINT('Ctrl Pts',(-2.50973591686119,1.69841403081809,30.4469782278978));
#63190=CARTESIAN_POINT('Ctrl Pts',(-2.78522233229009,-1.19411940448822,
30.6061278262914));
#63191=CARTESIAN_POINT('Ctrl Pts',(-0.500145588336814,-2.98885245251919,
30.7652774246849));
#63192=CARTESIAN_POINT('Ctrl Pts',(2.24473443701905,-2.0358172559745,30.9244270230786));
#63193=CARTESIAN_POINT('Ctrl Pts',(2.92594283537721,0.788823881844076,31.0835766214721));
#63194=CARTESIAN_POINT('Ctrl Pts',(0.917218245669399,2.88826856131385,31.2427262198657));
#63195=CARTESIAN_POINT('Ctrl Pts',(-1.93474073209646,2.33241567736749,31.4018758182592));
#63196=CARTESIAN_POINT('Ctrl Pts',(-3.00801734611399,-0.367717606241629,
31.5610254166528));
#63197=CARTESIAN_POINT('Ctrl Pts',(-1.31590668388164,-2.72979380023079,
31.7201750150464));
#63198=CARTESIAN_POINT('Ctrl Pts',(1.58596814578136,-2.58226443902045,31.8793246134399));
#63199=CARTESIAN_POINT('Ctrl Pts',(3.02980080805213,-0.0607589992462767,
32.0384742118336));
#63200=CARTESIAN_POINT('Ctrl Pts',(1.68821981072978,2.51660455040564,32.1976238102271));
#63201=CARTESIAN_POINT('Ctrl Pts',(-1.20540728437737,2.78035570947905,32.3567734086207));
#63202=CARTESIAN_POINT('Ctrl Pts',(-2.99085660543591,0.488017784699585,
32.5159230070143));
#63203=CARTESIAN_POINT('Ctrl Pts',(-2.02669518623548,-2.25297386015744,
32.6750726054078));
#63204=CARTESIAN_POINT('Ctrl Pts',(0.800685900927647,-2.92271905603642,
32.8342222038014));
#63205=CARTESIAN_POINT('Ctrl Pts',(2.89196531448888,-0.905495009514679,
32.993371802195));
#63206=CARTESIAN_POINT('Ctrl Pts',(2.32454859573719,1.94418579835346,33.1525214005885));
#63207=CARTESIAN_POINT('Ctrl Pts',(-0.379916008719381,3.00650102590723,
33.3116709989822));
#63208=CARTESIAN_POINT('Ctrl Pts',(-2.73510905797225,1.30482298932096,33.4708205973757));
#63209=CARTESIAN_POINT('Ctrl Pts',(-2.5758100289656,-1.59642954343275,33.6299701957693));
#63210=CARTESIAN_POINT('Ctrl Pts',(-0.0484687114584423,-3.03002233926915,
33.7891197941628));
#63211=CARTESIAN_POINT('Ctrl Pts',(2.52343177660385,-1.67799781325436,33.9482693925565));
#63212=CARTESIAN_POINT('Ctrl Pts',(2.77544333965369,1.21667533091117,34.10741899095));
#63213=CARTESIAN_POINT('Ctrl Pts',(0.475881951382315,2.99281154782468,34.2665685893436));
#63214=CARTESIAN_POINT('Ctrl Pts',(-2.26117621363277,2.01753976995621,34.4257181877372));
#63215=CARTESIAN_POINT('Ctrl Pts',(-2.91944718729431,-0.812534745810323,
34.5848677861307));
#63216=CARTESIAN_POINT('Ctrl Pts',(-0.893756874633229,-2.89561448424386,
34.7440173845244));
#63217=CARTESIAN_POINT('Ctrl Pts',(1.95359887560164,-2.31664326681841,34.9031669829178));
#63218=CARTESIAN_POINT('Ctrl Pts',(3.00493523785246,0.392108160255101,35.0623165813115));
#63219=CARTESIAN_POINT('Ctrl Pts',(1.29371782548904,2.74037931304599,35.221466179705));
#63220=CARTESIAN_POINT('Ctrl Pts',(-1.60686467367129,2.56931323765636,35.3806157780986));
#63221=CARTESIAN_POINT('Ctrl Pts',(-3.03019401613369,0.0361776257300149,
35.5397653764922));
#63222=CARTESIAN_POINT('Ctrl Pts',(-1.66774820545003,-2.5302174822596,35.6989149748858));
#63223=CARTESIAN_POINT('Ctrl Pts',(1.22792335653137,-2.77048530528777,35.8580645732793));
#63224=CARTESIAN_POINT('Ctrl Pts',(2.99471725163619,-0.463738284920935,
36.0172141716729));
#63225=CARTESIAN_POINT('Ctrl Pts',(2.00835114992269,2.26934135649022,36.1763637700665));
#63226=CARTESIAN_POINT('Ctrl Pts',(-0.824370206550868,2.91612729442474,
36.3355133684601));
#63227=CARTESIAN_POINT('Ctrl Pts',(-2.89921603912457,0.882004012335179,
36.4946629668536));
#63228=CARTESIAN_POINT('Ctrl Pts',(-2.30869976614112,-1.96297976732238,
36.6538125652472));
#63229=CARTESIAN_POINT('Ctrl Pts',(0.404293756186146,-3.00332008715369,
36.8129621636408));
#63230=CARTESIAN_POINT('Ctrl Pts',(2.74560467726245,-1.28259122354491,36.9721117620343));
#63231=CARTESIAN_POINT('Ctrl Pts',(2.56277379323208,1.61727307564432,37.1312613604279));
#63232=CARTESIAN_POINT('Ctrl Pts',(0.0238866669049971,3.03031638748835,
37.2904109588215));
#63233=CARTESIAN_POINT('Ctrl Pts',(-2.53696293435572,1.65747010346212,37.4495605572151));
#63234=CARTESIAN_POINT('Ctrl Pts',(-2.76547905773556,-1.23914916815844,
37.6087101556087));
#63235=CARTESIAN_POINT('Ctrl Pts',(-0.451592003194222,-2.99657751649272,
37.7678597540022));
#63236=CARTESIAN_POINT('Ctrl Pts',(2.27747872810931,-1.99912216839089,37.9270093523958));
#63237=CARTESIAN_POINT('Ctrl Pts',(2.91274116681489,0.836178144068786,38.0861589507893));
#63238=CARTESIAN_POINT('Ctrl Pts',(0.870271463391887,2.90279652361737,38.245308549183));
#63239=CARTESIAN_POINT('Ctrl Pts',(-1.97239480334944,2.30066746816425,38.4044581475765));
#63240=CARTESIAN_POINT('Ctrl Pts',(-3.00152875332717,-0.416375758145608,
38.5636077459701));
#63241=CARTESIAN_POINT('Ctrl Pts',(-1.27168541761539,-2.75096983951106,
38.7227573443637));
#63242=CARTESIAN_POINT('Ctrl Pts',(1.62811677833888,-2.55583908074386,38.8819069427572));
#63243=CARTESIAN_POINT('Ctrl Pts',(3.02950410350625,-0.0122707333053821,
39.0410565411509));
#63244=CARTESIAN_POINT('Ctrl Pts',(1.64888384109211,2.54497064203657,39.2002061395443));
#63245=CARTESIAN_POINT('Ctrl Pts',(-1.25390542022416,2.75780410693846,39.359355737938));
#63246=CARTESIAN_POINT('Ctrl Pts',(-2.41093357184072,1.21637226125721,39.4654554702004));
#63247=CARTESIAN_POINT('Ctrl Pts',(-2.53475666268526,0.371481747533365,
39.5185053363315));
#63248=CARTESIAN_POINT('Ctrl Pts',(1.37702479013085,-1.93106208855777,0.));
#63249=CARTESIAN_POINT('Ctrl Pts',(2.02069053684824,-1.47206923947237,0.0530498661311914));
#63250=CARTESIAN_POINT('Ctrl Pts',(2.80157597434148,0.132344484221863,0.159149598393574));
#63251=CARTESIAN_POINT('Ctrl Pts',(1.39973361494253,2.43361003431117,0.318299196787148));
#63252=CARTESIAN_POINT('Ctrl Pts',(-1.29016829261282,2.49039187166835,0.477448795180722));
#63253=CARTESIAN_POINT('Ctrl Pts',(-2.79332177148693,0.2612514548119,0.636598393574298));
#63254=CARTESIAN_POINT('Ctrl Pts',(-1.72880511791114,-2.20993111510645,
0.79574799196787));
#63255=CARTESIAN_POINT('Ctrl Pts',(0.92524708272242,-2.64846350983462,0.954897590361446));
#63256=CARTESIAN_POINT('Ctrl Pts',(2.72859047663099,-0.652671033011881,
1.11404718875502));
#63257=CARTESIAN_POINT('Ctrl Pts',(2.02348342694992,1.94341489122264,1.27319678714859));
#63258=CARTESIAN_POINT('Ctrl Pts',(-0.541916200030843,2.75270370291815,
1.43234638554217));
#63259=CARTESIAN_POINT('Ctrl Pts',(-2.60909777792823,1.03139851074894,1.59149598393574));
#63260=CARTESIAN_POINT('Ctrl Pts',(-2.27764138013584,-1.63814995877251,
1.75064558232932));
#63261=CARTESIAN_POINT('Ctrl Pts',(0.147742963738231,-2.80166329463351,
1.90979518072289));
#63262=CARTESIAN_POINT('Ctrl Pts',(2.43729952527864,-1.38950924165797,2.06894477911646));
#63263=CARTESIAN_POINT('Ctrl Pts',(2.48615290161395,1.30008022007748,2.22809437751004));
#63264=CARTESIAN_POINT('Ctrl Pts',(0.249388740897356,2.79445248935483,2.38724397590361));
#63265=CARTESIAN_POINT('Ctrl Pts',(-2.21664790546107,1.71977748150848,2.54639357429719));
#63266=CARTESIAN_POINT('Ctrl Pts',(-2.64483411095343,-0.935956616644485,
2.70554317269076));
#63267=CARTESIAN_POINT('Ctrl Pts',(-0.641521429760122,-2.73122899507208,
2.86469277108434));
#63268=CARTESIAN_POINT('Ctrl Pts',(1.95156679945169,-2.01557660741595,3.02384236947791));
#63269=CARTESIAN_POINT('Ctrl Pts',(2.75050382812508,0.553073821547345,3.18299196787149));
#63270=CARTESIAN_POINT('Ctrl Pts',(1.02079575688963,2.61326192654012,3.34214156626506));
#63271=CARTESIAN_POINT('Ctrl Pts',(-1.64736952904253,2.27097678934574,3.50129116465863));
#63272=CARTESIAN_POINT('Ctrl Pts',(-2.80104397213344,-0.15910560602253,
3.66044076305221));
#63273=CARTESIAN_POINT('Ctrl Pts',(-1.37960980571773,-2.44291602421381,
3.81959036144579));
#63274=CARTESIAN_POINT('Ctrl Pts',(1.31015328351832,-2.48085878298404,3.97873995983935));
#63275=CARTESIAN_POINT('Ctrl Pts',(2.79544153036393,-0.238051622317477,
4.13788955823294));
#63276=CARTESIAN_POINT('Ctrl Pts',(1.71077171156123,2.22360564722096,4.2970391566265));
#63277=CARTESIAN_POINT('Ctrl Pts',(-0.946677043995799,2.64101580821315,
4.45618875502009));
#63278=CARTESIAN_POINT('Ctrl Pts',(-2.73380879311094,0.630437472770587,
4.61533835341365));
#63279=CARTESIAN_POINT('Ctrl Pts',(-2.00764384796512,-1.95972653806095,
4.77448795180724));
#63280=CARTESIAN_POINT('Ctrl Pts',(0.564226129275921,-2.74823776254792,
4.9336375502008));
#63281=CARTESIAN_POINT('Ctrl Pts',(2.61738109284993,-1.01018718025988,5.09278714859438));
#63282=CARTESIAN_POINT('Ctrl Pts',(2.26427587290829,1.65656774558932,5.25193674698795));
#63283=CARTESIAN_POINT('Ctrl Pts',(-0.170466175671311,2.80037554755443,
5.41108634538153));
#63284=CARTESIAN_POINT('Ctrl Pts',(-2.4484920424651,1.36968925029025,5.5702359437751));
#63285=CARTESIAN_POINT('Ctrl Pts',(-2.47552399495132,-1.3202056183776,5.72938554216868));
#63286=CARTESIAN_POINT('Ctrl Pts',(-0.226710508403585,-2.79638414202316,
5.88853514056225));
#63287=CARTESIAN_POINT('Ctrl Pts',(2.23052676138529,-1.70173802070743,6.04768473895582));
#63288=CARTESIAN_POINT('Ctrl Pts',(2.63715407267815,0.957382014315266,6.2068343373494));
#63289=CARTESIAN_POINT('Ctrl Pts',(0.619343131473575,2.7363435474871,6.36598393574298));
#63290=CARTESIAN_POINT('Ctrl Pts',(-1.96785402607795,1.99967808819976,6.52513353413654));
#63291=CARTESIAN_POINT('Ctrl Pts',(-2.74592648151851,-0.575369170596496,
6.68428313253012));
#63292=CARTESIAN_POINT('Ctrl Pts',(-0.999561980729776,-2.62145718466985,
6.84343273092369));
#63293=CARTESIAN_POINT('Ctrl Pts',(1.66573870468711,-2.25753770557323,7.00258232931727));
#63294=CARTESIAN_POINT('Ctrl Pts',(2.79966104700711,0.181823943001463,7.16173192771085));
#63295=CARTESIAN_POINT('Ctrl Pts',(1.35974615823274,2.45402777277456,7.32088152610442));
#63296=CARTESIAN_POINT('Ctrl Pts',(-1.33023623090505,2.47014847617812,7.48003112449799));
#63297=CARTESIAN_POINT('Ctrl Pts',(-2.79728074300439,0.21536566391685,7.63918072289157));
#63298=CARTESIAN_POINT('Ctrl Pts',(-1.69267633000806,-2.23741117504315,
7.79833032128514));
#63299=CARTESIAN_POINT('Ctrl Pts',(0.968071232182813,-2.63324894641536,
7.95747991967872));
#63300=CARTESIAN_POINT('Ctrl Pts',(2.73883327901741,-0.608238599666532,
8.11662951807229));
#63301=CARTESIAN_POINT('Ctrl Pts',(1.99167942641439,1.9759491356751,8.27577911646587));
#63302=CARTESIAN_POINT('Ctrl Pts',(-0.586502744988177,2.74357001997377,
8.43492871485943));
#63303=CARTESIAN_POINT('Ctrl Pts',(-2.62549014393666,0.988920334743421,
8.59407831325302));
#63304=CARTESIAN_POINT('Ctrl Pts',(-2.25076239348891,-1.67488225628956,
8.75322791164658));
#63305=CARTESIAN_POINT('Ctrl Pts',(0.19317871866267,-2.79890048180234,8.91237751004016));
#63306=CARTESIAN_POINT('Ctrl Pts',(2.4595231253557,-1.34978069337877,9.07152710843373));
#63307=CARTESIAN_POINT('Ctrl Pts',(2.46473231443179,1.34024495618274,9.23067670682731));
#63308=CARTESIAN_POINT('Ctrl Pts',(0.204017275877662,2.79813131849115,9.38982630522089));
#63309=CARTESIAN_POINT('Ctrl Pts',(-2.2442587751075,1.68358678859467,9.54897590361444));
#63310=CARTESIAN_POINT('Ctrl Pts',(-2.62930049358051,-0.978744521739348,
9.70812550200804));
#63311=CARTESIAN_POINT('Ctrl Pts',(-0.597124060110883,-2.74127794672745,
9.86727510040159));
#63312=CARTESIAN_POINT('Ctrl Pts',(1.98401173368511,-1.98364799422109,10.0264246987952));
#63313=CARTESIAN_POINT('Ctrl Pts',(2.74116841667201,0.597626669265515,10.1855742971888));
#63314=CARTESIAN_POINT('Ctrl Pts',(0.978262417402176,2.6294799042921,10.3447238955823));
#63315=CARTESIAN_POINT('Ctrl Pts',(-1.68399824995572,2.24395004813468,10.5038734939759));
#63316=CARTESIAN_POINT('Ctrl Pts',(-2.79809386445219,-0.204530315827701,
10.6630230923695));
#63317=CARTESIAN_POINT('Ctrl Pts',(-1.33979301969774,-2.46497800978969,
10.8221726907631));
#63318=CARTESIAN_POINT('Ctrl Pts',(1.35023162953112,-2.4592755988281,10.9813222891566));
#63319=CARTESIAN_POINT('Ctrl Pts',(2.79893585448806,-0.192665531008406,
11.1404718875502));
#63320=CARTESIAN_POINT('Ctrl Pts',(1.67446954602361,2.25106944891023,11.2996214859438));
#63321=CARTESIAN_POINT('Ctrl Pts',(-0.989401707370339,2.62530877914012,
11.4587710843374));
#63322=CARTESIAN_POINT('Ctrl Pts',(-2.74367751039345,0.585999695681418,
11.6179206827309));
#63323=CARTESIAN_POINT('Ctrl Pts',(-1.97558392376629,-1.99204168744878,
11.7770702811245));
#63324=CARTESIAN_POINT('Ctrl Pts',(0.608740760399282,-2.7387217111284,11.9362198795181));
#63325=CARTESIAN_POINT('Ctrl Pts',(2.63342640009004,-0.967588404067735,
12.0953694779116));
#63326=CARTESIAN_POINT('Ctrl Pts',(2.23710078159852,1.69308653569416,12.2545190763052));
#63327=CARTESIAN_POINT('Ctrl Pts',(-0.21587854772131,2.79724120822844,12.4136686746988));
#63328=CARTESIAN_POINT('Ctrl Pts',(-2.47039233632374,1.3297833015234,12.5728182730924));
#63329=CARTESIAN_POINT('Ctrl Pts',(-2.45377841914996,-1.36019608663289,
12.7319678714859));
#63330=CARTESIAN_POINT('Ctrl Pts',(-0.181310616086829,-2.79969433775756,
12.8911174698795));
#63331=CARTESIAN_POINT('Ctrl Pts',(2.25784308439087,-1.66532475230686,13.0502670682731));
#63332=CARTESIAN_POINT('Ctrl Pts',(2.62127386877248,1.00004261372609,13.2094166666667));
#63333=CARTESIAN_POINT('Ctrl Pts',(0.574865689414601,2.74603193053384,13.3685662650602));
#63334=CARTESIAN_POINT('Ctrl Pts',(-2.00003886484401,1.96748734773341,13.5277158634538));
#63335=CARTESIAN_POINT('Ctrl Pts',(-2.73622994360017,-0.619844835522055,
13.6868654618474));
#63336=CARTESIAN_POINT('Ctrl Pts',(-0.956898470366649,-2.63732956639619,
13.846015060241));
#63337=CARTESIAN_POINT('Ctrl Pts',(1.70214696396934,-2.23021470657591,14.0051646586345));
#63338=CARTESIAN_POINT('Ctrl Pts',(2.79634252716041,0.227223227623548,14.1643142570281));
#63339=CARTESIAN_POINT('Ctrl Pts',(1.31975170355224,2.47576601587237,14.3234638554217));
#63340=CARTESIAN_POINT('Ctrl Pts',(-1.37013816353632,2.4482408658461,14.4826134538153));
#63341=CARTESIAN_POINT('Ctrl Pts',(-2.80040675581984,0.16995271794274,14.6417630522088));
#63342=CARTESIAN_POINT('Ctrl Pts',(-1.65615255790967,-2.26457957009835,
14.8009126506024));
#63343=CARTESIAN_POINT('Ctrl Pts',(1.01066706572481,-2.61719582886661,14.960062248996));
#63344=CARTESIAN_POINT('Ctrl Pts',(2.74834116840978,-0.563722224505545,
15.1192118473896));
#63345=CARTESIAN_POINT('Ctrl Pts',(1.95935839934075,2.00800313428798,15.2783614457831));
#63346=CARTESIAN_POINT('Ctrl Pts',(-0.630938711931175,2.73369315508602,
15.4375110441767));
#63347=CARTESIAN_POINT('Ctrl Pts',(-2.64118933898918,0.946192792187444,
15.5966606425703));
#63348=CARTESIAN_POINT('Ctrl Pts',(-2.22329193636798,-1.71117938570411,
15.7558102409639));
#63349=CARTESIAN_POINT('Ctrl Pts',(0.238564168873022,-2.7953978360347,15.9149598393574));
#63350=CARTESIAN_POINT('Ctrl Pts',(2.48109896001892,-1.30969839084066,16.074109437751));
#63351=CARTESIAN_POINT('Ctrl Pts',(2.4426630300295,1.38005769665789,16.2332590361446));
#63352=CARTESIAN_POINT('Ctrl Pts',(0.158592023455111,2.80107309695302,16.3924086345381));
#63353=CARTESIAN_POINT('Ctrl Pts',(-2.27127879519284,1.6469531137482,16.5515582329318));
#63354=CARTESIAN_POINT('Ctrl Pts',(-2.61307472652118,-1.02127488855538,
16.7107078313253));
#63355=CARTESIAN_POINT('Ctrl Pts',(-0.552569484305025,-2.75060518602588,
16.8698574297189));
#63356=CARTESIAN_POINT('Ctrl Pts',(2.01593436473937,-1.95119721233924,17.0290070281124));
#63357=CARTESIAN_POINT('Ctrl Pts',(2.73111138732539,0.642022207091869,17.188156626506));
#63358=CARTESIAN_POINT('Ctrl Pts',(0.935471545677604,2.64500565436165,17.3473062248996));
#63359=CARTESIAN_POINT('Ctrl Pts',(-1.72018365228211,2.21633258487957,17.5064558232932));
#63360=CARTESIAN_POINT('Ctrl Pts',(-2.79440715039491,-0.249901184869753,
17.6656054216867));
#63361=CARTESIAN_POINT('Ctrl Pts',(-1.29962352880245,-2.48639108101694,
17.8247550200804));
#63362=CARTESIAN_POINT('Ctrl Pts',(1.38995452278499,-2.43704500347595,17.9839046184738));
#63363=CARTESIAN_POINT('Ctrl Pts',(2.80169335019333,-0.147228719548932,
18.1430542168675));
#63364=CARTESIAN_POINT('Ctrl Pts',(1.63772657118694,2.27794064944762,18.302203815261));
#63365=CARTESIAN_POINT('Ctrl Pts',(-1.0318659076804,2.60891062954338,18.4613534136547));
#63366=CARTESIAN_POINT('Ctrl Pts',(-2.75282394613075,0.541407652316326,
18.6205030120482));
#63367=CARTESIAN_POINT('Ctrl Pts',(-1.94300392101022,-2.02383242570043,
18.7796526104418));
#63368=CARTESIAN_POINT('Ctrl Pts',(0.653095138640082,-2.7284846827978,18.9388022088353));
#63369=CARTESIAN_POINT('Ctrl Pts',(2.64877844972125,-0.924734907240888,
19.0979518072289));
#63370=CARTESIAN_POINT('Ctrl Pts',(2.20933676661749,1.7291596155502,19.2571014056225));
#63371=CARTESIAN_POINT('Ctrl Pts',(-0.261234089078342,2.79337048654149,
19.416251004016));
#63372=CARTESIAN_POINT('Ctrl Pts',(-2.49164229179172,1.28952728320592,19.5754006024097));
#63373=CARTESIAN_POINT('Ctrl Pts',(-2.43138687862253,-1.39982847907868,
19.7345502008032));
#63374=CARTESIAN_POINT('Ctrl Pts',(-0.135862993192047,-2.80226750533537,
19.8936997991968));
#63375=CARTESIAN_POINT('Ctrl Pts',(2.28456502325081,-1.62847308203622,20.0528493975903));
#63376=CARTESIAN_POINT('Ctrl Pts',(2.60470360644785,1.04243994883883,20.211998995984));
#63377=CARTESIAN_POINT('Ctrl Pts',(0.530236912192428,2.75499741221771,20.3711485943775));
#63378=CARTESIAN_POINT('Ctrl Pts',(-2.03169718721918,1.93477866016328,20.5302981927711));
#63379=CARTESIAN_POINT('Ctrl Pts',(-2.72581308472214,-0.664157324385632,
20.6894477911646));
#63380=CARTESIAN_POINT('Ctrl Pts',(-0.91398305353419,-2.65250766299173,
20.8485973895582));
#63381=CARTESIAN_POINT('Ctrl Pts',(1.73810712782103,-2.20230459668849,21.0077469879518));
#63382=CARTESIAN_POINT('Ctrl Pts',(2.79228786153128,0.272562695031161,21.1668965863454));
#63383=CARTESIAN_POINT('Ctrl Pts',(1.2794098201712,2.49685250594164,21.326046184739));
#63384=CARTESIAN_POINT('Ctrl Pts',(-1.40967940307629,2.42568874856607,21.4851957831325));
#63385=CARTESIAN_POINT('Ctrl Pts',(-2.80279555293216,0.12449503139221,21.6443453815261));
#63386=CARTESIAN_POINT('Ctrl Pts',(-1.61919279854979,-2.29115180760726,
21.8034949799196));
#63387=CARTESIAN_POINT('Ctrl Pts',(1.05299683804908,-2.60045372645548,21.9626445783133));
#63388=CARTESIAN_POINT('Ctrl Pts',(2.75712554852525,-0.519057447732828,
22.1217941767068));
#63389=CARTESIAN_POINT('Ctrl Pts',(1.92652156513405,2.03952851989154,22.2809437751004));
#63390=CARTESIAN_POINT('Ctrl Pts',(-0.675208582315117,2.72309663705597,
22.440093373494));
#63391=CARTESIAN_POINT('Ctrl Pts',(-2.65619323281388,0.903216161464837,
22.5992429718876));
#63392=CARTESIAN_POINT('Ctrl Pts',(-2.1952361907975,-1.74702604187528,22.7583925702811));
#63393=CARTESIAN_POINT('Ctrl Pts',(0.283886816331191,-2.79115929317747,
22.9175421686747));
#63394=CARTESIAN_POINT('Ctrl Pts',(2.50202163773962,-1.26927130616756,23.0766917670682));
#63395=CARTESIAN_POINT('Ctrl Pts',(2.41995070706164,1.41950713269408,23.2358413654619));
#63396=CARTESIAN_POINT('Ctrl Pts',(0.113125021193992,2.80327748429537,23.3949909638554));
#63397=CARTESIAN_POINT('Ctrl Pts',(-2.29770089414027,1.60988587342226,23.554140562249));
#63398=CARTESIAN_POINT('Ctrl Pts',(-2.59616105949236,-1.06353640161169,
23.7132901606426));
#63399=CARTESIAN_POINT('Ctrl Pts',(-0.507869442880617,-2.75920832003777,
23.8724397590362));
#63400=CARTESIAN_POINT('Ctrl Pts',(2.04732629486344,-1.91823277178195,24.0315893574297));
#63401=CARTESIAN_POINT('Ctrl Pts',(2.7203353844948,0.686248730594912,24.1907389558233));
#63402=CARTESIAN_POINT('Ctrl Pts',(0.892434408187573,2.6598350985466,24.3498885542168));
#63403=CARTESIAN_POINT('Ctrl Pts',(-1.75591621096422,2.18813166524563,24.5090381526105));
#63404=CARTESIAN_POINT('Ctrl Pts',(-2.78998480004911,-0.295206266655231,
24.668187751004));
#63405=CARTESIAN_POINT('Ctrl Pts',(-1.25911190801061,-2.50714960213454,
24.8273373493976));
#63406=CARTESIAN_POINT('Ctrl Pts',(1.42931150622999,-2.41417284852102,24.9864869477912));
#63407=CARTESIAN_POINT('Ctrl Pts',(2.80371329149552,-0.101753149675579,
25.1456365461847));
#63408=CARTESIAN_POINT('Ctrl Pts',(1.60055245978652,2.30421217509344,25.3047861445783));
#63409=CARTESIAN_POINT('Ctrl Pts',(-1.07405846611233,2.59182567618851,25.4639357429719));
#63410=CARTESIAN_POINT('Ctrl Pts',(-2.76124569248608,0.496673081719335,
25.6230853413655));
#63411=CARTESIAN_POINT('Ctrl Pts',(-1.90991241648788,-2.05509038383302,
25.782234939759));
#63412=CARTESIAN_POINT('Ctrl Pts',(0.697277587574235,-2.71752937247129,
25.9413845381526));
#63413=CARTESIAN_POINT('Ctrl Pts',(2.66343320026788,-0.881637971101683,
26.1005341365462));
#63414=CARTESIAN_POINT('Ctrl Pts',(2.18099113692833,1.76477748881203,26.2596837349398));
#63415=CARTESIAN_POINT('Ctrl Pts',(-0.306520859756921,2.78876440147091,
26.4188333333333));
#63416=CARTESIAN_POINT('Ctrl Pts',(-2.51223631475264,1.24893179285964,26.5779829317269));
#63417=CARTESIAN_POINT('Ctrl Pts',(-2.40835526801112,-1.4390923623662,26.7371325301205));
#63418=CARTESIAN_POINT('Ctrl Pts',(-0.0903796039458558,-2.80410296736195,
26.896282128514));
#63419=CARTESIAN_POINT('Ctrl Pts',(2.3106855433324,-1.59119271121138,27.0554317269076));
#63420=CARTESIAN_POINT('Ctrl Pts',(2.58744764787687,1.08456285842457,27.2145813253012));
#63421=CARTESIAN_POINT('Ctrl Pts',(0.48546854847008,2.76323763234795,27.3737309236948));
#63422=CARTESIAN_POINT('Ctrl Pts',(-2.0628206590526,1.90156063615214,27.5328805220883));
#63423=CARTESIAN_POINT('Ctrl Pts',(-2.71467864715462,-0.708294971788098,
27.6920301204819));
#63424=CARTESIAN_POINT('Ctrl Pts',(-0.870827027847972,-2.66698747877582,
27.8511797188755));
#63425=CARTESIAN_POINT('Ctrl Pts',(1.77360972961834,-2.17381472333333,28.0103293172691));
#63426=CARTESIAN_POINT('Ctrl Pts',(2.7874981175229,0.317830409469884,28.1694789156627));
#63427=CARTESIAN_POINT('Ctrl Pts',(1.23873112821468,2.51728169189892,28.3286285140562));
#63428=CARTESIAN_POINT('Ctrl Pts',(-1.44884954017187,2.40249806125235,28.4877781124498));
#63429=CARTESIAN_POINT('Ctrl Pts',(-2.80444650548309,0.0790045711412627,
28.6469277108434));
#63430=CARTESIAN_POINT('Ctrl Pts',(-1.58180678169894,-2.31712089234655,
28.8060773092369));
#63431=CARTESIAN_POINT('Ctrl Pts',(1.09504940571272,-2.58302704659199,28.9652269076305));
#63432=CARTESIAN_POINT('Ctrl Pts',(2.76518410684866,-0.474256027488414,
29.1243765060241));
#63433=CARTESIAN_POINT('Ctrl Pts',(1.89317756819207,2.07051699333089,29.2835261044177));
#63434=CARTESIAN_POINT('Ctrl Pts',(-0.719300701960229,2.71178325544964,
29.4426757028112));
#63435=CARTESIAN_POINT('Ctrl Pts',(-2.67049787558951,0.860001756306001,
29.6018253012049));
#63436=CARTESIAN_POINT('Ctrl Pts',(-2.16660254253892,-1.78241278806047,
29.7609748995983));
#63437=CARTESIAN_POINT('Ctrl Pts',(0.32913472971066,-2.78618596904008,29.920124497992));
#63438=CARTESIAN_POINT('Ctrl Pts',(2.52228565055847,-1.22851008191401,30.0792740963855));
#63439=CARTESIAN_POINT('Ctrl Pts',(2.39660132461721,1.4585828791058,30.2384236947791));
#63440=CARTESIAN_POINT('Ctrl Pts',(0.067628238422609,2.80474390020647,30.3975732931727));
#63441=CARTESIAN_POINT('Ctrl Pts',(-2.32351811625089,1.572394825682,30.5567228915663));
#63442=CARTESIAN_POINT('Ctrl Pts',(-2.57856394506895,-1.10551793543479,
30.7158724899598));
#63443=CARTESIAN_POINT('Ctrl Pts',(-0.463035703261235,-2.76708508396162,
30.8750220883534));
#63444=CARTESIAN_POINT('Ctrl Pts',(2.07817926003504,-1.88476335053973,31.034171686747));
#63445=CARTESIAN_POINT('Ctrl Pts',(2.70884324499614,0.730294597006095,31.1933212851405));
#63446=CARTESIAN_POINT('Ctrl Pts',(0.849162334591095,2.67396433295012,31.3524708835341));
#63447=CARTESIAN_POINT('Ctrl Pts',(-1.79118651929591,2.15935471321182,31.5116204819277));
#63448=CARTESIAN_POINT('Ctrl Pts',(-2.78482797761209,-0.340433634481819,
31.6707700803213));
#63449=CARTESIAN_POINT('Ctrl Pts',(-1.21826882213122,-2.52724810839787,
31.8299196787149));
#63450=CARTESIAN_POINT('Ctrl Pts',(1.46829221901895,-2.39066515512857,31.9890692771084));
#63451=CARTESIAN_POINT('Ctrl Pts',(2.80499514663885,-0.0562507929721938,
32.148218875502));
#63452=CARTESIAN_POINT('Ctrl Pts',(1.56295699802168,2.32987710978769,32.3073684738957));
#63453=CARTESIAN_POINT('Ctrl Pts',(-1.11596827534518,2.57405841674206,32.4665180722891));
#63454=CARTESIAN_POINT('Ctrl Pts',(-2.76894053240879,0.451807760403934,
32.6256676706828));
#63455=CARTESIAN_POINT('Ctrl Pts',(-1.87631812163978,-2.0858073330928,32.7848172690763));
#63456=CARTESIAN_POINT('Ctrl Pts',(0.741276476036008,-2.70585866416802,
32.9439668674699));
#63457=CARTESIAN_POINT('Ctrl Pts',(2.67738679382172,-0.838308941051334,
33.1031164658635));
#63458=CARTESIAN_POINT('Ctrl Pts',(2.15207135460536,1.79993077896479,33.262266064257));
#63459=CARTESIAN_POINT('Ctrl Pts',(-0.351726937875201,2.78342416558279,
33.4214156626506));
#63460=CARTESIAN_POINT('Ctrl Pts',(-2.5321689837664,1.20800751737253,33.5805652610442));
#63461=CARTESIAN_POINT('Ctrl Pts',(-2.38468965045838,-1.47797740015734,
33.7397148594378));
#63462=CARTESIAN_POINT('Ctrl Pts',(-0.0448724219901618,-2.805200240646,
33.8988644578313));
#63463=CARTESIAN_POINT('Ctrl Pts',(2.33619776832739,-1.55349345400542,34.0580140562249));
#63464=CARTESIAN_POINT('Ctrl Pts',(2.56951053574539,1.1264002534988,34.2171636546184));
#63465=CARTESIAN_POINT('Ctrl Pts',(0.440572383654118,2.77075042165889,34.3763132530121));
#63466=CARTESIAN_POINT('Ctrl Pts',(-2.09340108698849,1.86784202045169,34.5354628514056));
#63467=CARTESIAN_POINT('Ctrl Pts',(-2.70282956208393,-0.752246158366563,
34.6946124497992));
#63468=CARTESIAN_POINT('Ctrl Pts',(-0.827441754243024,-2.68076520187573,
34.8537620481927));
#63469=CARTESIAN_POINT('Ctrl Pts',(1.8086454231506,-2.14475258658905,35.0129116465864));
#63470=CARTESIAN_POINT('Ctrl Pts',(2.78197455612906,0.363014454134983,35.1720612449799));
#63471=CARTESIAN_POINT('Ctrl Pts',(1.19772633632314,2.53704819558261,35.3312108433735));
#63472=CARTESIAN_POINT('Ctrl Pts',(-1.48763826287672,2.37867490914512,35.4903604417671));
#63473=CARTESIAN_POINT('Ctrl Pts',(-2.80535917940216,0.033493312273267,
35.6495100401606));
#63474=CARTESIAN_POINT('Ctrl Pts',(-1.544004348296,-2.3424799870727,35.8086596385542));
#63475=CARTESIAN_POINT('Ctrl Pts',(1.13681369625387,-2.5649203784333,35.9678092369478));
#63476=CARTESIAN_POINT('Ctrl Pts',(2.77251472574384,-0.429329754965117,
36.1269588353414));
#63477=CARTESIAN_POINT('Ctrl Pts',(1.859335179167,2.10096039122589,36.2861084337349));
#63478=CARTESIAN_POINT('Ctrl Pts',(-0.763203449633773,2.69975599917453,
36.4452580321285));
#63479=CARTESIAN_POINT('Ctrl Pts',(-2.68409952799179,0.816560932765415,
36.6044076305221));
#63480=CARTESIAN_POINT('Ctrl Pts',(-2.13739847908868,-1.81733026991608,
36.7635572289156));
#63481=CARTESIAN_POINT('Ctrl Pts',(0.374295901203924,-2.78047924664893,
36.9227068273092));
#63482=CARTESIAN_POINT('Ctrl Pts',(2.54188584736079,-1.18742530783014,37.0818564257028));
#63483=CARTESIAN_POINT('Ctrl Pts',(2.37262067949971,1.49727438051885,37.2410060240964));
#63484=CARTESIAN_POINT('Ctrl Pts',(0.0221143200437823,2.8054724710268,37.40015562249));
#63485=CARTESIAN_POINT('Ctrl Pts',(-2.34872493899865,1.53448886261914,37.5593052208835));
#63486=CARTESIAN_POINT('Ctrl Pts',(-2.56028558526488,-1.14720657325335,
37.7184548192771));
#63487=CARTESIAN_POINT('Ctrl Pts',(-0.41808470505867,-2.7742369623609,37.8776044176707));
#63488=CARTESIAN_POINT('Ctrl Pts',(2.10849398479986,-1.85079097113315,38.0367540160642));
#63489=CARTESIAN_POINT('Ctrl Pts',(2.69662111602106,0.774135259850986,38.1959036144578));
#63490=CARTESIAN_POINT('Ctrl Pts',(0.805698917428903,2.68741434710406,38.3550532128514));
#63491=CARTESIAN_POINT('Ctrl Pts',(-1.82604672754298,2.12996216288546,38.514202811245));
#63492=CARTESIAN_POINT('Ctrl Pts',(-2.77882082650591,-0.38548144078392,
38.6733524096386));
#63493=CARTESIAN_POINT('Ctrl Pts',(-1.17732869269255,-2.54685292441361,
38.8325020080321));
#63494=CARTESIAN_POINT('Ctrl Pts',(1.50731350036759,-2.36620050995552,38.9916516064257));
#63495=CARTESIAN_POINT('Ctrl Pts',(2.80472045702593,-0.0113602674063951,
39.1508012048193));
#63496=CARTESIAN_POINT('Ctrl Pts',(1.52653968516444,2.35613848946071,39.3099508032129));
#63497=CARTESIAN_POINT('Ctrl Pts',(-1.16086793848797,2.55318010173628,39.4691004016064));
#63498=CARTESIAN_POINT('Ctrl Pts',(-2.23204672396583,1.1261196710573,39.5752001338688));
#63499=CARTESIAN_POINT('Ctrl Pts',(-2.34668236863851,0.343918483395665,
39.62825));
#63500=CARTESIAN_POINT('',(1.37702479013102,-1.93106208855765,0.));
#63501=CARTESIAN_POINT('Ctrl Pts',(1.37702479013085,-1.93106208855777,0.));
#63502=CARTESIAN_POINT('Ctrl Pts',(2.02069053684824,-1.47206923947237,0.0530498661311914));
#63503=CARTESIAN_POINT('Ctrl Pts',(2.80157597434148,0.132344484221863,0.159149598393574));
#63504=CARTESIAN_POINT('Ctrl Pts',(1.39973361494253,2.43361003431117,0.318299196787148));
#63505=CARTESIAN_POINT('Ctrl Pts',(-1.29016829261282,2.49039187166835,0.477448795180722));
#63506=CARTESIAN_POINT('Ctrl Pts',(-2.33890237726732,0.935144475115511,
0.588485765616658));
#63507=CARTESIAN_POINT('Ctrl Pts',(-2.37527771381695,0.0747453293793789,
0.646472869921401));
#63508=CARTESIAN_POINT('Ctrl Pts',(-2.37479956011642,0.00144393851757997,
0.651410108094952));
#63509=CARTESIAN_POINT('Ctrl Pts',(1.29201581877684,2.64862154577367,-1.02348685082632E-16));
#63510=CARTESIAN_POINT('Ctrl Pts',(1.34958683951914,2.6139027695176,-1.05335179962833E-16));
#63511=CARTESIAN_POINT('Ctrl Pts',(1.40579757808849,2.57711951310873,-7.026873643365E-17));
#63512=CARTESIAN_POINT('Ctrl Pts',(1.46052207638911,2.53826450414093,-3.81639164714898E-17));
#63513=CARTESIAN_POINT('Ctrl Pts',(1.54016250524111,2.48171890439427,5.08870273341264E-18));
#63514=CARTESIAN_POINT('Ctrl Pts',(1.61665719687035,2.42078661355511,-2.95171646394387E-16));
#63515=CARTESIAN_POINT('Ctrl Pts',(1.68983041078343,2.35584690071589,-3.71230823859037E-16));
#63516=CARTESIAN_POINT('Ctrl Pts',(1.72880905664705,2.32125415927566,-4.11746793905046E-16));
#63517=CARTESIAN_POINT('Ctrl Pts',(1.76684450913562,2.2855237047089,2.98781131615067E-18));
#63518=CARTESIAN_POINT('Ctrl Pts',(1.8039051241343,2.24870979089898,-9.71445146547012E-17));
#63519=CARTESIAN_POINT('Ctrl Pts',(1.83175376478358,2.22104653014029,-1.72387442043738E-16));
#63520=CARTESIAN_POINT('Ctrl Pts',(1.85905188698991,2.19277144505213,-3.58527894598338E-16));
#63521=CARTESIAN_POINT('Ctrl Pts',(1.88578464604575,2.16390703240831,-4.02455846426619E-16));
#63522=CARTESIAN_POINT('Ctrl Pts',(1.89741557092782,2.15134866480683,-4.21568078982574E-16));
#63523=CARTESIAN_POINT('Ctrl Pts',(1.90893301001484,2.13868568977461,-1.74418497724213E-16));
#63524=CARTESIAN_POINT('Ctrl Pts',(1.92033535624658,2.12592108303427,-1.73472347597681E-16));
#63525=CARTESIAN_POINT('Ctrl Pts',(1.98513247700578,2.05338252407569,-1.68095576645527E-16));
#63526=CARTESIAN_POINT('Ctrl Pts',(2.04622485478601,1.97755495337877,1.47867480362913E-16));
#63527=CARTESIAN_POINT('Ctrl Pts',(2.10343517400832,1.89881202362381,1.45716771982052E-16));
#63528=CARTESIAN_POINT('Ctrl Pts',(2.1498698585821,1.83490042244258,1.43971152194695E-16));
#63529=CARTESIAN_POINT('Ctrl Pts',(2.19374640661719,1.76906743351724,1.25074431252417E-16));
#63530=CARTESIAN_POINT('Ctrl Pts',(2.23494640511299,1.70150389183245,9.71445146547012E-17));
#63531=CARTESIAN_POINT('Ctrl Pts',(2.2529714044549,1.67194484234535,8.49251761432007E-17));
#63532=CARTESIAN_POINT('Ctrl Pts',(2.27048380976275,1.64205448628232,-3.94957526722027E-18));
#63533=CARTESIAN_POINT('Ctrl Pts',(2.28747233024776,1.61184859939393,-1.38777878078145E-17));
#63534=CARTESIAN_POINT('Ctrl Pts',(2.29692191410317,1.59504707383844,-1.94001920112555E-17));
#63535=CARTESIAN_POINT('Ctrl Pts',(2.30620939497628,1.57814792321238,-3.53600877506368E-16));
#63536=CARTESIAN_POINT('Ctrl Pts',(2.31533271265734,1.56115385938179,-3.60822483003176E-16));
#63537=CARTESIAN_POINT('Ctrl Pts',(2.32256102651894,1.54768963162543,-3.66544089214901E-16));
#63538=CARTESIAN_POINT('Ctrl Pts',(2.32968598712138,1.53416623918464,-2.42653694158405E-16));
#63539=CARTESIAN_POINT('Ctrl Pts',(2.33670051558313,1.52059718163605,-2.35922392732846E-16));
#63540=CARTESIAN_POINT('Ctrl Pts',(2.38036738874924,1.43612702541826,-1.94018665747421E-16));
#63541=CARTESIAN_POINT('Ctrl Pts',(2.41982387271352,1.34976845265731,1.4715862347523E-16));
#63542=CARTESIAN_POINT('Ctrl Pts',(2.4549039648554,1.26186702602105,1.38777878078145E-16));
#63543=CARTESIAN_POINT('Ctrl Pts',(2.49089795323757,1.17167561727776,1.30178799967504E-16));
#63544=CARTESIAN_POINT('Ctrl Pts',(2.52228513147818,1.07985893523056,-4.56104370496148E-16));
#63545=CARTESIAN_POINT('Ctrl Pts',(2.54882950886302,0.986780146350002,-4.16333634234434E-16));
#63546=CARTESIAN_POINT('Ctrl Pts',(2.57361253388436,0.899877601214398,-3.79201885480213E-16));
#63547=CARTESIAN_POINT('Ctrl Pts',(2.59417381411934,0.811874117600765,2.29384838853516E-16));
#63548=CARTESIAN_POINT('Ctrl Pts',(2.61027212391662,0.72306925843443,2.77555756156289E-16));
#63549=CARTESIAN_POINT('Ctrl Pts',(2.61929903017754,0.673273152551058,3.04566936862236E-16));
#63550=CARTESIAN_POINT('Ctrl Pts',(2.62692179109589,0.623225210006774,3.81625854467562E-16));
#63551=CARTESIAN_POINT('Ctrl Pts',(2.63309089404061,0.572980117688449,4.44089209850063E-16));
#63552=CARTESIAN_POINT('Ctrl Pts',(2.63571616911387,0.551598210205481,4.70670625551379E-16));
#63553=CARTESIAN_POINT('Ctrl Pts',(2.63807868307449,0.530173533712499,-2.82105728213271E-16));
#63554=CARTESIAN_POINT('Ctrl Pts',(2.64017105031311,0.508748320977571,-2.77555756156289E-16));
#63555=CARTESIAN_POINT('Ctrl Pts',(2.64883715014049,0.420010058899969,-2.58710827154487E-16));
#63556=CARTESIAN_POINT('Ctrl Pts',(2.65288772475143,0.331168392804234,-2.63733613808333E-16));
#63557=CARTESIAN_POINT('Ctrl Pts',(2.65213842907589,0.24251346567146,-1.66533453693773E-16));
#63558=CARTESIAN_POINT('Ctrl Pts',(2.65181580925284,0.204341836183571,-1.24682553602233E-16));
#63559=CARTESIAN_POINT('Ctrl Pts',(2.65060272221495,0.166204869721315,2.80550455053001E-16));
#63560=CARTESIAN_POINT('Ctrl Pts',(2.64848147823716,0.128126164156209,2.22044604925031E-16));
#63561=CARTESIAN_POINT('Ctrl Pts',(2.64345202732824,0.0378418864774469,
8.23152144247318E-17));
#63562=CARTESIAN_POINT('Ctrl Pts',(2.63332045212558,-0.052116414540607,
5.07700615603077E-16));
#63563=CARTESIAN_POINT('Ctrl Pts',(2.61828345471384,-0.141416240256498,
4.9960036108132E-16));
#63564=CARTESIAN_POINT('Ctrl Pts',(2.60278436204712,-0.233460299053213,
4.91251181253792E-16));
#63565=CARTESIAN_POINT('Ctrl Pts',(2.58207326188015,-0.324805869332984,
2.73776835990291E-16));
#63566=CARTESIAN_POINT('Ctrl Pts',(2.55631815458934,-0.415057098853101,
3.88578058618805E-16));
#63567=CARTESIAN_POINT('Ctrl Pts',(2.55164298986117,-0.431439844230992,
4.0941721182917E-16));
#63568=CARTESIAN_POINT('Ctrl Pts',(2.54680150944407,-0.447786422521825,
8.02355772890154E-17));
#63569=CARTESIAN_POINT('Ctrl Pts',(2.54179457675504,-0.464094314185775,
8.32667268468867E-17));
#63570=CARTESIAN_POINT('Ctrl Pts',(2.53779818455242,-0.477110812536128,
8.56861047795307E-17));
#63571=CARTESIAN_POINT('Ctrl Pts',(2.53369907715842,-0.490093861130131,
-2.80579978572094E-17));
#63572=CARTESIAN_POINT('Ctrl Pts',(2.52949874656044,-0.503040373434415,
-2.77555756156289E-17));
#63573=CARTESIAN_POINT('Ctrl Pts',(2.50210999497329,-0.587459635478357,
-2.57835956831298E-17));
#63574=CARTESIAN_POINT('Ctrl Pts',(2.47041261765305,-0.670355637708211,
4.53801252951917E-16));
#63575=CARTESIAN_POINT('Ctrl Pts',(2.43461854159303,-0.751424609131643,
4.16333634234434E-16));
#63576=CARTESIAN_POINT('Ctrl Pts',(2.39888342881732,-0.832360036311529,
3.78927735614187E-16));
#63577=CARTESIAN_POINT('Ctrl Pts',(2.35906444173415,-0.911475228111023,
2.85466068417674E-17));
#63578=CARTESIAN_POINT('Ctrl Pts',(2.31533040039922,-0.988437898460195,
0.));
#63579=CARTESIAN_POINT('Ctrl Pts',(2.27229963182651,-1.06416295737186,-2.80875582280819E-17));
#63580=CARTESIAN_POINT('Ctrl Pts',(2.22547803483335,-1.13780478243029,1.26518886312492E-16));
#63581=CARTESIAN_POINT('Ctrl Pts',(2.17499568445539,-1.20900757805061,1.11022302462516E-16));
#63582=CARTESIAN_POINT('Ctrl Pts',(2.15763280136466,-1.23349704430628,1.05692412477636E-16));
#63583=CARTESIAN_POINT('Ctrl Pts',(2.139836646293,-1.25769759925574,2.96543489227423E-16));
#63584=CARTESIAN_POINT('Ctrl Pts',(2.12161186800647,-1.28159346943437,2.77555756156289E-16));
#63585=CARTESIAN_POINT('Ctrl Pts',(2.11095501761041,-1.29556646321094,2.66452771663535E-16));
#63586=CARTESIAN_POINT('Ctrl Pts',(2.10015160389292,-1.30943526383152,1.50560739160337E-16));
#63587=CARTESIAN_POINT('Ctrl Pts',(2.08920251355156,-1.32319660086055,1.66533453693773E-16));
#63588=CARTESIAN_POINT('Ctrl Pts',(2.08026388843326,-1.33443108966228,1.7957326822492E-16));
#63589=CARTESIAN_POINT('Ctrl Pts',(2.07123261909841,-1.34558830018916,4.59673378436067E-16));
#63590=CARTESIAN_POINT('Ctrl Pts',(2.06211416739129,-1.35666111036041,4.44089209850063E-16));
#63591=CARTESIAN_POINT('Ctrl Pts',(2.00790902752559,-1.42248404207256,3.51448258839193E-16));
#63592=CARTESIAN_POINT('Ctrl Pts',(1.95057481796449,-1.48539172201629,-2.78080721237473E-16));
#63593=CARTESIAN_POINT('Ctrl Pts',(1.89026923526248,-1.54508768501287,-1.66533453693773E-16));
#63594=CARTESIAN_POINT('Ctrl Pts',(1.83091398083794,-1.60384292645194,-5.67440088568915E-17));
#63595=CARTESIAN_POINT('Ctrl Pts',(1.76867962675818,-1.65948739321344,3.75307511728794E-17));
#63596=CARTESIAN_POINT('Ctrl Pts',(1.7036906355759,-1.71169599621308,-5.55111512312578E-17));
#63597=CARTESIAN_POINT('Ctrl Pts',(1.64072966331149,-1.76227539967243,-1.45649627458181E-16));
#63598=CARTESIAN_POINT('Ctrl Pts',(1.57518272461921,-1.80963031643797,-6.78657436235449E-19));
#63599=CARTESIAN_POINT('Ctrl Pts',(1.50714729981333,-1.85341941089056,-1.66533453693773E-16));
#63600=CARTESIAN_POINT('Ctrl Pts',(1.46473327304936,-1.8807180105448,-2.6992914479841E-16));
#63601=CARTESIAN_POINT('Ctrl Pts',(1.42135183960329,-1.90662986293965,1.96676586340341E-17));
#63602=CARTESIAN_POINT('Ctrl Pts',(1.37702479013085,-1.93106208855777,0.));
#63603=CARTESIAN_POINT('Ctrl Pts',(0.260722923799077,2.92490787419796,39.0579999999999));
#63604=CARTESIAN_POINT('Ctrl Pts',(0.737297058639913,2.88302734391227,39.0322389374024));
#63605=CARTESIAN_POINT('Ctrl Pts',(1.20411394433562,2.73137775272334,39.0064778748049));
#63606=CARTESIAN_POINT('Ctrl Pts',(1.6022299374267,2.4739167068321,38.9807168122074));
#63607=CARTESIAN_POINT('Ctrl Pts',(2.42207190078732,1.94372607642437,38.9276669460763));
#63608=CARTESIAN_POINT('Ctrl Pts',(2.95057164862713,0.964817205660412,38.8746170799451));
#63609=CARTESIAN_POINT('Ctrl Pts',(2.94659684551607,-0.0114746559244529,
38.8215672138139));
#63610=CARTESIAN_POINT('Ctrl Pts',(2.942622042405,-0.987766517509207,38.7685173476827));
#63611=CARTESIAN_POINT('Ctrl Pts',(2.40617268834321,-1.96144136991487,38.7154674815515));
#63612=CARTESIAN_POINT('Ctrl Pts',(1.58292764435524,-2.48562670401527,38.6624176154203));
#63613=CARTESIAN_POINT('Ctrl Pts',(0.759682600367258,-3.00981203811569,
38.6093677492891));
#63614=CARTESIAN_POINT('Ctrl Pts',(-0.350358133546912,-3.08450785391083,
38.5563178831579));
#63615=CARTESIAN_POINT('Ctrl Pts',(-1.23646945708876,-2.67501588233558,
38.5032680170267));
#63616=CARTESIAN_POINT('Ctrl Pts',(-2.1225807806306,-2.26552391076032,38.4502181508955));
#63617=CARTESIAN_POINT('Ctrl Pts',(-2.78476269380013,-1.37184415181466,
38.3971682847643));
#63618=CARTESIAN_POINT('Ctrl Pts',(-2.91887804171701,-0.404963860410038,
38.3441184186332));
#63619=CARTESIAN_POINT('Ctrl Pts',(-2.93736881665659,-0.271657970073306,
38.3368043181186));
#63620=CARTESIAN_POINT('Ctrl Pts',(-2.94582171308893,-0.13696063005989,
38.3294902176041));
#63621=CARTESIAN_POINT('Ctrl Pts',(-2.94471098031246,-0.00212455505907094,
38.3221761170895));
#63622=CARTESIAN_POINT('Origin',(0.,0.,-1.84858989190508));
#63623=CARTESIAN_POINT('',(-1.37702479013119,-1.93106208855753,0.));
#63624=CARTESIAN_POINT('Ctrl Pts',(-1.3799850048903,-1.93364773575773,4.26633554873046E-16));
#63625=CARTESIAN_POINT('Ctrl Pts',(-0.787715267879867,-2.35133676185328,
0.0488167807402858));
#63626=CARTESIAN_POINT('Ctrl Pts',(0.877861752617119,-2.62654930074856,
0.150487376283488));
#63627=CARTESIAN_POINT('Ctrl Pts',(2.6974957852487,-0.758175742122775,0.305011786629609));
#63628=CARTESIAN_POINT('Ctrl Pts',(2.10214177353418,1.85307404405523,0.463573231038359));
#63629=CARTESIAN_POINT('Ctrl Pts',(-0.413064550041895,2.77131496429985,
0.622134675447112));
#63630=CARTESIAN_POINT('Ctrl Pts',(-2.14343282857647,1.46669785134097,0.750473562402662));
#63631=CARTESIAN_POINT('Ctrl Pts',(-2.36935871427084,0.339352278516582,
0.825958634555295));
#63632=CARTESIAN_POINT('Ctrl Pts',(-2.36820388529326,0.000916507492466252,
0.848589891905012));
#63633=CARTESIAN_POINT('Origin',(0.,0.,0.));
#63634=CARTESIAN_POINT('Ctrl Pts',(-1.03908919352469,2.13201587949063,-0.329233991005398));
#63635=CARTESIAN_POINT('Ctrl Pts',(-1.7471110134088,1.78694442439573,-0.276380176202481));
#63636=CARTESIAN_POINT('Ctrl Pts',(-2.78026471975083,0.342102824634871,
-0.170672546596647));
#63637=CARTESIAN_POINT('Ctrl Pts',(-1.79624709676258,-2.15298261314799,
-0.0121111021878947));
#63638=CARTESIAN_POINT('Ctrl Pts',(0.830322826211876,-2.67536157371565,
0.146450342220856));
#63639=CARTESIAN_POINT('Ctrl Pts',(2.6974957852487,-0.758175742122775,0.305011786629609));
#63640=CARTESIAN_POINT('Ctrl Pts',(2.10214177353418,1.85307404405523,0.463573231038359));
#63641=CARTESIAN_POINT('Ctrl Pts',(-0.413064550041895,2.77131496429985,
0.622134675447112));
#63642=CARTESIAN_POINT('Ctrl Pts',(-2.5509176989363,1.15947323231739,0.780696119855863));
#63643=CARTESIAN_POINT('Ctrl Pts',(-2.35954923822691,-1.51136660104342,
0.939257564264615));
#63644=CARTESIAN_POINT('Ctrl Pts',(-0.0135649315166644,-2.80200471609095,
1.09781900867337));
#63645=CARTESIAN_POINT('Ctrl Pts',(2.34478101694196,-1.53412545281777,1.25638045308212));
#63646=CARTESIAN_POINT('Ctrl Pts',(2.56205685808127,1.13464159452892,1.41494189749087));
#63647=CARTESIAN_POINT('Ctrl Pts',(0.439842266833678,2.76731764321101,1.57350334189962));
#63648=CARTESIAN_POINT('Ctrl Pts',(-2.08400064757574,1.87309085041683,1.73206478630837));
#63649=CARTESIAN_POINT('Ctrl Pts',(-2.70488792678447,-0.73151121296214,
1.89062623071712));
#63650=CARTESIAN_POINT('Ctrl Pts',(-0.855867697802383,-2.66814781527329,
2.04918767512588));
#63651=CARTESIAN_POINT('Ctrl Pts',(1.77466802262196,-2.16842771739956,2.20774911953463));
#63652=CARTESIAN_POINT('Ctrl Pts',(2.78470651107863,0.311343289720562,2.36631056394338));
#63653=CARTESIAN_POINT('Ctrl Pts',(1.25195381897505,2.50681790160282,2.52487200835213));
#63654=CARTESIAN_POINT('Ctrl Pts',(-1.42399178516171,2.41324930660116,2.68343345276089));
#63655=CARTESIAN_POINT('Ctrl Pts',(-2.7996519092107,0.116077212167865,2.84199489716963));
#63656=CARTESIAN_POINT('Ctrl Pts',(-1.61887392550448,-2.28708807616797,
3.00055634157839));
#63657=CARTESIAN_POINT('Ctrl Pts',(1.04014173421655,-2.60185124395797,3.15911778598714));
#63658=CARTESIAN_POINT('Ctrl Pts',(2.74937577244265,-0.540793460784857,
3.31767923039589));
#63659=CARTESIAN_POINT('Ctrl Pts',(1.94808022437453,2.01407749008101,3.47624067480464));
#63660=CARTESIAN_POINT('Ctrl Pts',(-0.632060208719933,2.72983966543523,
3.6348021192134));
#63661=CARTESIAN_POINT('Ctrl Pts',(-2.6350493239968,0.952911204334078,3.79336356362214));
#63662=CARTESIAN_POINT('Ctrl Pts',(-2.23190343620269,-1.69414632007928,
3.95192500803089));
#63663=CARTESIAN_POINT('Ctrl Pts',(0.20925401019493,-2.79423289347191,4.11048645243965));
#63664=CARTESIAN_POINT('Ctrl Pts',(2.45933594484265,-1.34282962940415,4.2690478968484));
#63665=CARTESIAN_POINT('Ctrl Pts',(2.46373152879142,1.33474778785059,4.42760934125715));
#63666=CARTESIAN_POINT('Ctrl Pts',(0.218427035218096,2.79353080054729,4.58617078566591));
#63667=CARTESIAN_POINT('Ctrl Pts',(-2.22632910816719,1.7014650761505,4.74473223007464));
#63668=CARTESIAN_POINT('Ctrl Pts',(-2.63816376282886,-0.94425455451785,
4.90329367448341));
#63669=CARTESIAN_POINT('Ctrl Pts',(-0.641019536282537,-2.72774974243608,
5.06185511889216));
#63670=CARTESIAN_POINT('Ctrl Pts',(1.94145701387202,-2.02046266150336,5.2204165633009));
#63671=CARTESIAN_POINT('Ctrl Pts',(2.75113651059875,0.531763672408809,5.37897800770967));
#63672=CARTESIAN_POINT('Ctrl Pts',(1.04867864620236,2.59842217513736,5.5375394521184));
#63673=CARTESIAN_POINT('Ctrl Pts',(-1.61135613114964,2.29239091820107,5.69610089652718));
#63674=CARTESIAN_POINT('Ctrl Pts',(-2.80001792372147,-0.106884657847206,
5.8546623409359));
#63675=CARTESIAN_POINT('Ctrl Pts',(-1.43190741113937,-2.40856095400742,
6.01322378534467));
#63676=CARTESIAN_POINT('Ctrl Pts',(1.24371659317073,-2.5109149207244,6.17178522975341));
#63677=CARTESIAN_POINT('Ctrl Pts',(2.78366924554423,-0.320484375057478,
6.33034667416217));
#63678=CARTESIAN_POINT('Ctrl Pts',(1.7817780141982,2.16258914529891,6.48890811857092));
#63679=CARTESIAN_POINT('Ctrl Pts',(-0.847103045334166,2.67094386572056,
6.64746956297967));
#63680=CARTESIAN_POINT('Ctrl Pts',(-2.70247133997559,0.740387303953358,
6.80603100738843));
#63681=CARTESIAN_POINT('Ctrl Pts',(-2.09013976063242,-1.86623698502313,
6.96459245179718));
#63682=CARTESIAN_POINT('Ctrl Pts',(0.430755120614024,-2.76874966894979,
7.12315389620592));
#63683=CARTESIAN_POINT('Ctrl Pts',(2.55831581876159,-1.14304193917764,7.28171534061469));
#63684=CARTESIAN_POINT('Ctrl Pts',(2.34980895897243,1.52640838558285,7.44027678502343));
#63685=CARTESIAN_POINT('Ctrl Pts',(-0.00437219018642784,2.80205381589964,
7.59883822943218));
#63686=CARTESIAN_POINT('Ctrl Pts',(-2.35456097390834,1.5190679126993,7.75739967384093));
#63687=CARTESIAN_POINT('Ctrl Pts',(-2.55473627454364,-1.15102010007455,
7.91596111824968));
#63688=CARTESIAN_POINT('Ctrl Pts',(-0.422112596148098,-2.77008044277018,
8.07452256265844));
#63689=CARTESIAN_POINT('Ctrl Pts',(2.09595354186346,-1.85970520609983,8.23308400706718));
#63690=CARTESIAN_POINT('Ctrl Pts',(2.70014765665469,0.748817291137776,8.39164545147595));
#63691=CARTESIAN_POINT('Ctrl Pts',(0.838763715722044,2.67357441123917,8.55020689588469));
#63692=CARTESIAN_POINT('Ctrl Pts',(-1.78851812206262,2.15701822669591,8.70876834029344));
#63693=CARTESIAN_POINT('Ctrl Pts',(-2.78265555637215,-0.32916980091735,
8.8673297847022));
#63694=CARTESIAN_POINT('Ctrl Pts',(-1.23587473403734,-2.51478395593197,
9.02589122911094));
#63695=CARTESIAN_POINT('Ctrl Pts',(1.43941682598108,-2.40408067758287,9.1844526735197));
#63696=CARTESIAN_POINT('Ctrl Pts',(2.8003378439175,-0.0981461317030541,
9.34301411792845));
#63697=CARTESIAN_POINT('Ctrl Pts',(1.60419442889238,2.29740830884616,9.5015755623372));
#63698=CARTESIAN_POINT('Ctrl Pts',(-1.05678242634981,2.59513691480873,9.66013700674596));
#63699=CARTESIAN_POINT('Ctrl Pts',(-2.7527825872023,0.523175621412691,9.8186984511547));
#63700=CARTESIAN_POINT('Ctrl Pts',(-1.93514230974122,-2.02651152088859,
9.97725989556346));
#63701=CARTESIAN_POINT('Ctrl Pts',(0.649528893544149,-2.72573603265175,
10.1358213399722));
#63702=CARTESIAN_POINT('Ctrl Pts',(2.64109764832668,-0.936017048588331,
10.294382784381));
#63703=CARTESIAN_POINT('Ctrl Pts',(2.22100851147896,1.70840448816513,10.4529442287897));
#63704=CARTESIAN_POINT('Ctrl Pts',(-0.22714373294823,2.79283555330906,10.6115056731985));
#63705=CARTESIAN_POINT('Ctrl Pts',(-2.46788487447809,1.32705273051488,10.7700671176072));
#63706=CARTESIAN_POINT('Ctrl Pts',(-2.45513340586504,-1.3504979313758,10.928628562016));
#63707=CARTESIAN_POINT('Ctrl Pts',(-0.200533038930914,-2.79487230540894,
11.0871900064247));
#63708=CARTESIAN_POINT('Ctrl Pts',(2.23717948448735,-1.68717297792302,11.2457514508335));
#63709=CARTESIAN_POINT('Ctrl Pts',(2.63206274630088,0.961129753352717,11.4043128952422));
#63710=CARTESIAN_POINT('Ctrl Pts',(0.623538130558561,2.73179884013891,11.562874339651));
#63711=CARTESIAN_POINT('Ctrl Pts',(-1.95435606311157,2.00798831715321,11.7214357840597));
#63712=CARTESIAN_POINT('Ctrl Pts',(-2.74767473166069,-0.549370796673882,
11.8799972284685));
#63713=CARTESIAN_POINT('Ctrl Pts',(-1.03201708332093,-2.60508453662804,
12.0385586728772));
#63714=CARTESIAN_POINT('Ctrl Pts',(1.6260033530305,-2.28202493395194,12.197120117286));
#63715=CARTESIAN_POINT('Ctrl Pts',(2.7992760290567,0.124813526483961,12.3556815616948));
#63716=CARTESIAN_POINT('Ctrl Pts',(1.41645384406812,2.41768137083226,12.5142430061035));
#63717=CARTESIAN_POINT('Ctrl Pts',(-1.25977076144102,2.50289878578082,12.6728044505123));
#63718=CARTESIAN_POINT('Ctrl Pts',(-2.78566451856249,0.302651438567153,
12.831365894921));
#63719=CARTESIAN_POINT('Ctrl Pts',(-1.76789245405787,-2.17395514538134,
12.9899273393298));
#63720=CARTESIAN_POINT('Ctrl Pts',(0.864190157080086,-2.66546432646371,
13.1484887837385));
#63721=CARTESIAN_POINT('Ctrl Pts',(2.70715729817405,-0.723065741262676,
13.3070502281472));
#63722=CARTESIAN_POINT('Ctrl Pts',(2.07814568976501,1.87958378247841,13.465611672556));
#63723=CARTESIAN_POINT('Ctrl Pts',(-0.448477109148286,2.76593437843611,
13.6241731169647));
#63724=CARTESIAN_POINT('Ctrl Pts',(-2.5655832965958,1.12663527881625,13.7827345613735));
#63725=CARTESIAN_POINT('Ctrl Pts',(-2.33998579499565,-1.54142504925259,
13.9412960057822));
#63726=CARTESIAN_POINT('Ctrl Pts',(0.022316198533973,-2.80196836001547,
14.099857450191));
#63727=CARTESIAN_POINT('Ctrl Pts',(2.36424066594685,-1.50395836934669,14.2584188945997));
#63728=CARTESIAN_POINT('Ctrl Pts',(2.5473128609508,1.16735679707592,14.4169803390085));
#63729=CARTESIAN_POINT('Ctrl Pts',(0.404364597205185,2.77272681232246,14.5755417834172));
#63730=CARTESIAN_POINT('Ctrl Pts',(-2.10781994697999,1.84624477639289,14.734103227826));
#63731=CARTESIAN_POINT('Ctrl Pts',(-2.69529693160535,-0.766093436679547,
14.8926646722347));
#63732=CARTESIAN_POINT('Ctrl Pts',(-0.821625189105414,-2.678890955577,15.0512261166435));
#63733=CARTESIAN_POINT('Ctrl Pts',(1.80229479678065,-2.14552048900545,15.2097875610522));
#63734=CARTESIAN_POINT('Ctrl Pts',(2.78049052387073,0.346982924521951,15.368349005461));
#63735=CARTESIAN_POINT('Ctrl Pts',(1.21974494421116,2.52264681917943,15.5269104498698));
#63736=CARTESIAN_POINT('Ctrl Pts',(-1.45478282458735,2.394813486794,15.6854718942785));
#63737=CARTESIAN_POINT('Ctrl Pts',(-2.80090894123675,0.0802110101217299,
15.8440333386872));
#63738=CARTESIAN_POINT('Ctrl Pts',(-1.58944914047375,-2.30763431528742,
16.002594783096));
#63739=CARTESIAN_POINT('Ctrl Pts',(1.07337977774581,-2.5883161622899,16.1611562275048));
#63740=CARTESIAN_POINT('Ctrl Pts',(2.75607650988087,-0.505536324043674,
16.3197176719135));
#63741=CARTESIAN_POINT('Ctrl Pts',(1.92212503357044,2.03886244228653,16.4782791163223));
#63742=CARTESIAN_POINT('Ctrl Pts',(-0.666970940652513,2.72152061678207,
16.636840560731));
#63743=CARTESIAN_POINT('Ctrl Pts',(-2.64703766011397,0.919084506007508,
16.7954020051398));
#63744=CARTESIAN_POINT('Ctrl Pts',(-2.21002250208375,-1.72259259360078,
16.9539634495485));
#63745=CARTESIAN_POINT('Ctrl Pts',(0.245024140396729,-2.79132367773206,
17.1125248939573));
#63746=CARTESIAN_POINT('Ctrl Pts',(2.47633259500592,-1.31122140851802,17.271086338366));
#63747=CARTESIAN_POINT('Ctrl Pts',(2.44643459674846,1.3661926903175,17.4296477827748));
#63748=CARTESIAN_POINT('Ctrl Pts',(0.182630818693805,2.79609919124984,17.5882092271835));
#63749=CARTESIAN_POINT('Ctrl Pts',(-2.24793811302219,1.67281168792754,17.7467706715923));
#63750=CARTESIAN_POINT('Ctrl Pts',(-2.62585378763459,-0.977965535798613,
17.905332116001));
#63751=CARTESIAN_POINT('Ctrl Pts',(-0.606031153241877,-2.7357359054823,
18.0638935604098));
#63752=CARTESIAN_POINT('Ctrl Pts',(1.96717496328582,-1.9954316242523,18.2224550048186));
#63753=CARTESIAN_POINT('Ctrl Pts',(2.7441002692833,0.566955390982473,18.3810164492273));
#63754=CARTESIAN_POINT('Ctrl Pts',(1.01531319693132,2.61164006237112,18.5395778936361));
#63755=CARTESIAN_POINT('Ctrl Pts',(-1.64058389174553,2.27156536278176,18.6981393380448));
#63756=CARTESIAN_POINT('Ctrl Pts',(-2.79841933475915,-0.142737276458901,
18.8567007824536));
#63757=CARTESIAN_POINT('Ctrl Pts',(-1.40094218755544,-2.42670263740165,
19.0152622268623));
#63758=CARTESIAN_POINT('Ctrl Pts',(1.27577326591705,-2.49478000577529,19.1738236712711));
#63759=CARTESIAN_POINT('Ctrl Pts',(2.7875455501625,-0.284806090198347,19.3323851156798));
#63760=CARTESIAN_POINT('Ctrl Pts',(1.75393439181258,2.18523199053596,19.4909465600886));
#63761=CARTESIAN_POINT('Ctrl Pts',(-0.88124182797927,2.65987547525528,19.6495080044973));
#63762=CARTESIAN_POINT('Ctrl Pts',(-2.71173223457244,0.705714525304297,
19.8080694489061));
#63763=CARTESIAN_POINT('Ctrl Pts',(-2.06606639316088,-1.89285349731455,
19.9666308933148));
#63764=CARTESIAN_POINT('Ctrl Pts',(0.466180705424317,-2.76300565564655,
20.1251923377236));
#63765=CARTESIAN_POINT('Ctrl Pts',(2.57274555864665,-1.11018241460974,20.2837537821323));
#63766=CARTESIAN_POINT('Ctrl Pts',(2.33006666709568,1.55637849835264,20.4423152265411));
#63767=CARTESIAN_POINT('Ctrl Pts',(-0.0402592916836527,2.80176799408478,
20.6008766709498));
#63768=CARTESIAN_POINT('Ctrl Pts',(-2.37382339935842,1.48878714795069,20.7594381153585));
#63769=CARTESIAN_POINT('Ctrl Pts',(-2.53978498085384,-1.18364562022337,
20.9179995597673));
#63770=CARTESIAN_POINT('Ctrl Pts',(-0.386600015079116,-2.7752594710379,
21.0765610041761));
#63771=CARTESIAN_POINT('Ctrl Pts',(2.11959990940443,-1.83270863131529,21.2351224485848));
#63772=CARTESIAN_POINT('Ctrl Pts',(2.69033567115523,0.783338164367446,21.3936838929936));
#63773=CARTESIAN_POINT('Ctrl Pts',(0.804452967251542,2.68409763733083,21.5522453374023));
#63774=CARTESIAN_POINT('Ctrl Pts',(-1.81599755853736,2.13393476250589,21.7108067818111));
#63775=CARTESIAN_POINT('Ctrl Pts',(-2.77821146213903,-0.364781818192803,
21.8693682262198));
#63776=CARTESIAN_POINT('Ctrl Pts',(-1.20356513206848,-2.53040622748872,
22.0279296706286));
#63777=CARTESIAN_POINT('Ctrl Pts',(1.47008916186248,-2.38544808357241,22.1864911150373));
#63778=CARTESIAN_POINT('Ctrl Pts',(2.80136517195679,-0.0622725990490076,
22.3450525594461));
#63779=CARTESIAN_POINT('Ctrl Pts',(1.5746386679948,2.31776568455491,22.5036140038548));
#63780=CARTESIAN_POINT('Ctrl Pts',(-1.08993310932985,2.58138926170217,22.6621754482636));
#63781=CARTESIAN_POINT('Ctrl Pts',(-2.7592574045594,0.487876294391167,22.8207368926723));
#63782=CARTESIAN_POINT('Ctrl Pts',(-1.90902893014377,-2.05112974897222,
22.9792983370811));
#63783=CARTESIAN_POINT('Ctrl Pts',(0.684385634967381,-2.71719359006588,
23.1378597814898));
#63784=CARTESIAN_POINT('Ctrl Pts',(2.65286911563599,-0.902114271336809,
23.2964212258986));
#63785=CARTESIAN_POINT('Ctrl Pts',(2.19894585862139,1.73671005470014,23.4549826703074));
#63786=CARTESIAN_POINT('Ctrl Pts',(-0.262894499289412,2.789697328652,23.6135441147161));
#63787=CARTESIAN_POINT('Ctrl Pts',(-2.48467875996383,1.29533631271162,23.7721055591249));
#63788=CARTESIAN_POINT('Ctrl Pts',(-2.43763545819304,-1.38183142105133,
23.9306670035336));
#63789=CARTESIAN_POINT('Ctrl Pts',(-0.164721108680563,-2.79721140774162,
24.0892284479423));
#63790=CARTESIAN_POINT('Ctrl Pts',(2.25860455255274,-1.6583817951343,24.2477898923511));
#63791=CARTESIAN_POINT('Ctrl Pts',(2.61953714146364,0.99476121141571,24.4063513367598));
#63792=CARTESIAN_POINT('Ctrl Pts',(0.588499322301271,2.73956077700343,24.5649127811686));
#63793=CARTESIAN_POINT('Ctrl Pts',(-1.9799131886852,1.98279309775759,24.7234742255773));
#63794=CARTESIAN_POINT('Ctrl Pts',(-2.74041327005717,-0.584516734182513,
24.8820356699861));
#63795=CARTESIAN_POINT('Ctrl Pts',(-0.998567672067767,-2.61808848352113,
25.0405971143948));
#63796=CARTESIAN_POINT('Ctrl Pts',(1.65509714933991,-2.26101263364264,25.1991585588037));
#63797=CARTESIAN_POINT('Ctrl Pts',(2.79744787596231,0.16065517271071,25.3577200032123));
#63798=CARTESIAN_POINT('Ctrl Pts',(1.3853730777416,2.43562438374916,25.5162814476211));
#63799=CARTESIAN_POINT('Ctrl Pts',(-1.29172345032858,2.48655891366281,25.6748428920299));
#63800=CARTESIAN_POINT('Ctrl Pts',(-2.78931226320224,0.266949061797221,
25.8334043364386));
#63801=CARTESIAN_POINT('Ctrl Pts',(-1.7399043998891,-2.19641921829403,25.9919657808474));
#63802=CARTESIAN_POINT('Ctrl Pts',(0.898257358734679,-2.65417754129669,
26.1505272252561));
#63803=CARTESIAN_POINT('Ctrl Pts',(2.71619596155049,-0.688334367659731,
26.3090886696649));
#63804=CARTESIAN_POINT('Ctrl Pts',(2.05390236619762,1.90604558533434,26.4676501140736));
#63805=CARTESIAN_POINT('Ctrl Pts',(-0.483865183409376,2.7599636206894,26.6262115584824));
#63806=CARTESIAN_POINT('Ctrl Pts',(-2.57980231118642,1.09368402129775,26.7847730028911));
#63807=CARTESIAN_POINT('Ctrl Pts',(-2.32005198206061,-1.57126811963504,
26.9433344472999));
#63808=CARTESIAN_POINT('Ctrl Pts',(0.0582007337807619,-2.8014527263247,
27.1018958917086));
#63809=CARTESIAN_POINT('Ctrl Pts',(2.38330878115067,-1.47355487069022,27.2604573361174));
#63810=CARTESIAN_POINT('Ctrl Pts',(2.53215294297463,1.19988590150465,27.4190187805261));
#63811=CARTESIAN_POINT('Ctrl Pts',(0.368819578303693,2.77767831505101,27.5775802249349));
#63812=CARTESIAN_POINT('Ctrl Pts',(-2.13129294603499,1.81909732599064,27.7361416693437));
#63813=CARTESIAN_POINT('Ctrl Pts',(-2.6852640787679,-0.80055076698708,27.8947031137524));
#63814=CARTESIAN_POINT('Ctrl Pts',(-0.787247754401329,-2.68919424297219,
28.0532645581612));
#63815=CARTESIAN_POINT('Ctrl Pts',(1.82962584537607,-2.12226152233333,28.2118260025699));
#63816=CARTESIAN_POINT('Ctrl Pts',(2.77581846464243,0.382565751988956,28.3703874469787));
#63817=CARTESIAN_POINT('Ctrl Pts',(1.18733596115095,2.53806186264293,28.5289488913874));
#63818=CARTESIAN_POINT('Ctrl Pts',(-1.48533521008643,2.37598485199765,28.6875103357962));
#63819=CARTESIAN_POINT('Ctrl Pts',(-2.80170651736734,0.0443316341475483,
28.8460717802049));
#63820=CARTESIAN_POINT('Ctrl Pts',(-1.55976361883997,-2.32780200115644,
29.0046332246137));
#63821=CARTESIAN_POINT('Ctrl Pts',(1.10644174224207,-2.57435649712099,29.1631946690224));
#63822=CARTESIAN_POINT('Ctrl Pts',(2.7623251407879,-0.470196256701246,29.3217561134311));
#63823=CARTESIAN_POINT('Ctrl Pts',(1.89585453653854,2.06331293785769,29.4803175578399));
#63824=CARTESIAN_POINT('Ctrl Pts',(-0.701772262303996,2.71275512995654,
29.6388790022487));
#63825=CARTESIAN_POINT('Ctrl Pts',(-2.65859177574196,0.885107040533527,
29.7974404466574));
#63826=CARTESIAN_POINT('Ctrl Pts',(-2.18777903535026,-1.7507562924995,29.9560018910662));
#63827=CARTESIAN_POINT('Ctrl Pts',(0.28075407675448,-2.78795657276624,30.1145633354749));
#63828=CARTESIAN_POINT('Ctrl Pts',(2.49292302707169,-1.27939809455089,30.2731247798837));
#63829=CARTESIAN_POINT('Ctrl Pts',(2.42873635105556,1.39741348222569,30.4316862242924));
#63830=CARTESIAN_POINT('Ctrl Pts',(0.146804643376738,2.79820890927176,30.5902476687012));
#63831=CARTESIAN_POINT('Ctrl Pts',(-2.26917836564331,1.64388389131991,30.7488091131099));
#63832=CARTESIAN_POINT('Ctrl Pts',(-2.61311306683666,-1.01151609140548,
30.9073705575187));
#63833=CARTESIAN_POINT('Ctrl Pts',(-0.570943356725327,-2.74327329784255,
31.0659320019274));
#63834=CARTESIAN_POINT('Ctrl Pts',(1.99257021690915,-1.97007325598095,31.2244934463362));
#63835=CARTESIAN_POINT('Ctrl Pts',(2.73661388518784,0.602054106075114,31.3830548907449));
#63836=CARTESIAN_POINT('Ctrl Pts',(0.981781195472087,2.62442953562526,31.5416163351537));
#63837=CARTESIAN_POINT('Ctrl Pts',(-1.6695425306181,2.25036717930698,31.7001777795624));
#63838=CARTESIAN_POINT('Ctrl Pts',(-2.79636169250615,-0.178566480417973,
31.8587392239712));
#63839=CARTESIAN_POINT('Ctrl Pts',(-1.3697471531232,-2.44444624398976,32.0173006683799));
#63840=CARTESIAN_POINT('Ctrl Pts',(1.30762066055104,-2.47823584659426,32.1758621127887));
#63841=CARTESIAN_POINT('Ctrl Pts',(2.79096458522799,-0.249081085688892,
32.3344235571974));
#63842=CARTESIAN_POINT('Ctrl Pts',(1.72580305366397,2.20751636986205,32.4929850016062));
#63843=CARTESIAN_POINT('Ctrl Pts',(-0.915236051531332,2.64837075826291,
32.6515464460149));
#63844=CARTESIAN_POINT('Ctrl Pts',(-2.72054829604864,0.670925981097476,
32.8101078904237));
#63845=CARTESIAN_POINT('Ctrl Pts',(-2.04165410772776,-1.91915950552399,
32.9686693348324));
#63846=CARTESIAN_POINT('Ctrl Pts',(0.5015298178546,-2.75680839831995,33.1272307792412));
#63847=CARTESIAN_POINT('Ctrl Pts',(2.58675326481436,-1.07714077548725,33.2857922236499));
#63848=CARTESIAN_POINT('Ctrl Pts',(2.30994215059737,1.58609330246939,33.4443536680588));
#63849=CARTESIAN_POINT('Ctrl Pts',(-0.076139789038159,2.80102256966442,
33.6029151124674));
#63850=CARTESIAN_POINT('Ctrl Pts',(-2.39269642232381,1.45826216224833,33.7614765568762));
#63851=CARTESIAN_POINT('Ctrl Pts',(-2.52441706030621,-1.21607697489841,
33.920038001285));
#63852=CARTESIAN_POINT('Ctrl Pts',(-0.351024016063958,-2.77998324516326,
34.0785994456937));
#63853=CARTESIAN_POINT('Ctrl Pts',(2.14289857733639,-1.80541141862616,34.2371608901025));
#63854=CARTESIAN_POINT('Ctrl Pts',(2.68008236242858,0.817730538643591,34.3957223345112));
#63855=CARTESIAN_POINT('Ctrl Pts',(0.770010256154827,2.69418056348283,34.55428377892));
#63856=CARTESIAN_POINT('Ctrl Pts',(-1.84317909840598,2.11050124722063,34.7128452233287));
#63857=CARTESIAN_POINT('Ctrl Pts',(-2.7733116294966,-0.400333996597624,
34.8714066677375));
#63858=CARTESIAN_POINT('Ctrl Pts',(-1.17105809706712,-2.54561341065258,
35.0299681121462));
#63859=CARTESIAN_POINT('Ctrl Pts',(1.50052034409269,-2.36642418021518,35.188529556555));
#63860=CARTESIAN_POINT('Ctrl Pts',(2.80193296331482,-0.0263888510821259,
35.3470910009637));
#63861=CARTESIAN_POINT('Ctrl Pts',(1.54482460333755,2.33774285330196,35.5056524453724));
#63862=CARTESIAN_POINT('Ctrl Pts',(-1.12290500001934,2.56721815733726,35.6642138897812));
#63863=CARTESIAN_POINT('Ctrl Pts',(-2.76527959168139,0.452496935327245,
35.8227753341899));
#63864=CARTESIAN_POINT('Ctrl Pts',(-1.88260239509527,-2.0754115079434,35.9813367785987));
#63865=CARTESIAN_POINT('Ctrl Pts',(0.719130113544572,-2.70820542107464,
36.1398982230075));
#63866=CARTESIAN_POINT('Ctrl Pts',(2.66420539827102,-0.86806350611665,36.2984596674162));
#63867=CARTESIAN_POINT('Ctrl Pts',(2.17652250448365,1.76473072150059,36.457021111825));
#63868=CARTESIAN_POINT('Ctrl Pts',(-0.298602167564159,2.78610149950517,
36.6155825562337));
#63869=CARTESIAN_POINT('Ctrl Pts',(-2.50106500632603,1.26340737324662,36.7741440006425));
#63870=CARTESIAN_POINT('Ctrl Pts',(-2.41973773932351,-1.41293816913244,
36.9327054450512));
#63871=CARTESIAN_POINT('Ctrl Pts',(-0.128881968591299,-2.79909178025225,
37.09126688946));
#63872=CARTESIAN_POINT('Ctrl Pts',(2.27965875812724,-1.62931833193606,37.2498283338687));
#63873=CARTESIAN_POINT('Ctrl Pts',(2.60658251510917,1.02822903240515,37.4083897782775));
#63874=CARTESIAN_POINT('Ctrl Pts',(0.553362663956598,2.74687418626157,37.5669512226862));
#63875=CARTESIAN_POINT('Ctrl Pts',(-2.00514302452926,1.95727095960215,37.725512667095));
#63876=CARTESIAN_POINT('Ctrl Pts',(-2.732707048879,-0.619563618269777,37.8840741115037));
#63877=CARTESIAN_POINT('Ctrl Pts',(-0.964945338256294,-2.63066900551404,
38.0426355559125));
#63878=CARTESIAN_POINT('Ctrl Pts',(1.68390204706478,-2.23961789871709,38.2011970003212));
#63879=CARTESIAN_POINT('Ctrl Pts',(2.79519402126786,0.196448450834139,38.35975844473));
#63880=CARTESIAN_POINT('Ctrl Pts',(1.35400172213932,2.45320986049924,38.5183198891387));
#63881=CARTESIAN_POINT('Ctrl Pts',(-1.3233434007851,2.46973099698168,38.6768813335475));
#63882=CARTESIAN_POINT('Ctrl Pts',(-2.79273305520996,0.231355853883896,
38.8354427779563));
#63883=CARTESIAN_POINT('Ctrl Pts',(-1.71119063643581,-2.21881512820523,
38.994004222365));
#63884=CARTESIAN_POINT('Ctrl Pts',(0.931334562612731,-2.64189543289012,
39.1525656667738));
#63885=CARTESIAN_POINT('Ctrl Pts',(2.72641926444476,-0.654580598253606,
39.3111271111825));
#63886=CARTESIAN_POINT('Ctrl Pts',(2.02601511878175,1.93446865908499,39.4696885555913));
#63887=CARTESIAN_POINT('Ctrl Pts',(0.334552217316969,2.47661908313362,39.5753961851971));
#63888=CARTESIAN_POINT('Ctrl Pts',(-0.439445221993938,2.33068358199192,
39.62825));
#63889=CARTESIAN_POINT('Ctrl Pts',(-1.12236674703412,2.30288577939285,-0.219489327336937));
#63890=CARTESIAN_POINT('Ctrl Pts',(-1.88713280539037,1.9301586555206,-0.16663551253402));
#63891=CARTESIAN_POINT('Ctrl Pts',(-3.00308836704896,0.369520573237848,
-0.060927882928185));
#63892=CARTESIAN_POINT('Ctrl Pts',(-1.94020688832694,-2.32553288687669,
0.0976335614805664));
#63893=CARTESIAN_POINT('Ctrl Pts',(0.896868849422307,-2.88977778360442,
0.256195005889318));
#63894=CARTESIAN_POINT('Ctrl Pts',(2.91368593619747,-0.818939554630395,
0.41475645029807));
#63895=CARTESIAN_POINT('Ctrl Pts',(2.27061742039935,2.00158821764338,0.573317894706821));
#63896=CARTESIAN_POINT('Ctrl Pts',(-0.4461695090612,2.99342133559979,0.731879339115573));
#63897=CARTESIAN_POINT('Ctrl Pts',(-2.75536038441027,1.25239893566279,0.890440783524324));
#63898=CARTESIAN_POINT('Ctrl Pts',(-2.54865474444223,-1.63249471379359,
1.04900222793308));
#63899=CARTESIAN_POINT('Ctrl Pts',(-0.0146520896905362,-3.02657071016718,
1.20756367234183));
#63900=CARTESIAN_POINT('Ctrl Pts',(2.53270292761432,-1.65707756826962,1.36612511675058));
#63901=CARTESIAN_POINT('Ctrl Pts',(2.76739228878582,1.22557717223607,1.52468656115933));
#63902=CARTESIAN_POINT('Ctrl Pts',(0.475093319524896,2.98910365017368,1.68324800556808));
#63903=CARTESIAN_POINT('Ctrl Pts',(-2.25102237826412,2.02320926613654,1.84180944997683));
#63904=CARTESIAN_POINT('Ctrl Pts',(-2.92167051913873,-0.790138003193314,
2.00037089438559));
#63905=CARTESIAN_POINT('Ctrl Pts',(-0.924461008602584,-2.88198588022671,
2.15893233879434));
#63906=CARTESIAN_POINT('Ctrl Pts',(1.91689836447934,-2.34221583529375,2.31749378320309));
#63907=CARTESIAN_POINT('Ctrl Pts',(3.00788614467443,0.33629582279584,2.47605522761184));
#63908=CARTESIAN_POINT('Ctrl Pts',(1.35229135669612,2.70772621942572,2.63461667202059));
#63909=CARTESIAN_POINT('Ctrl Pts',(-1.53811726430708,2.60665859188122,2.79317811642934));
#63910=CARTESIAN_POINT('Ctrl Pts',(-3.02402933814537,0.12538019241986,2.9517395608381));
#63911=CARTESIAN_POINT('Ctrl Pts',(-1.74861818691741,-2.47038619997742,
3.11030100524684));
#63912=CARTESIAN_POINT('Ctrl Pts',(1.12350364334661,-2.81037598614788,3.26886244965561));
#63913=CARTESIAN_POINT('Ctrl Pts',(2.9697238324877,-0.584135222636071,3.42742389406434));
#63914=CARTESIAN_POINT('Ctrl Pts',(2.10420864543479,2.17549524612882,3.58598533847311));
#63915=CARTESIAN_POINT('Ctrl Pts',(-0.682716522134537,2.94862200888265,
3.74454678288185));
#63916=CARTESIAN_POINT('Ctrl Pts',(-2.84623471832721,1.02928204362586,3.90310822729061));
#63917=CARTESIAN_POINT('Ctrl Pts',(-2.41077880031416,-1.82992326945222,
4.06166967169936));
#63918=CARTESIAN_POINT('Ctrl Pts',(0.226024622515564,-3.01817601669349,
4.22023111610811));
#63919=CARTESIAN_POINT('Ctrl Pts',(2.65643883266062,-1.45045038709602,4.37879256051686));
#63920=CARTESIAN_POINT('Ctrl Pts',(2.66118669962771,1.44172082829505,4.53735400492561));
#63921=CARTESIAN_POINT('Ctrl Pts',(0.235932817422852,3.01741765470029,4.69591544933437));
#63922=CARTESIAN_POINT('Ctrl Pts',(-2.40475771909903,1.83782858546841,4.85447689374311));
#63923=CARTESIAN_POINT('Ctrl Pts',(-2.84959876311035,-1.01993160869226,
5.01303833815187));
#63924=CARTESIAN_POINT('Ctrl Pts',(-0.692393892849685,-2.94636458950742,
5.17159978256062));
#63925=CARTESIAN_POINT('Ctrl Pts',(2.09705461931962,-2.18239215557902,5.33016122696938));
#63926=CARTESIAN_POINT('Ctrl Pts',(2.97162568457982,0.574381744042531,5.48872267137811));
#63927=CARTESIAN_POINT('Ctrl Pts',(1.13272474409016,2.80667209543142,5.64728411578688));
#63928=CARTESIAN_POINT('Ctrl Pts',(-1.74049788074223,2.47611403700979,5.80584556019562));
#63929=CARTESIAN_POINT('Ctrl Pts',(-3.02442468680107,-0.115450903044226,
5.96440700460438));
#63930=CARTESIAN_POINT('Ctrl Pts',(-1.5466672862248,-2.60159449239653,6.12296844901313));
#63931=CARTESIAN_POINT('Ctrl Pts',(1.34339396041099,-2.71215159315935,6.28152989342187));
#63932=CARTESIAN_POINT('Ctrl Pts',(3.00676574774326,-0.346169518218407,
6.44009133783064));
#63933=CARTESIAN_POINT('Ctrl Pts',(1.92457818462032,2.33590933223643,6.59865278223937));
#63934=CARTESIAN_POINT('Ctrl Pts',(-0.914993915170435,2.88500601946456,
6.75721422664814));
#63935=CARTESIAN_POINT('Ctrl Pts',(-2.9190602555613,0.799725466362086,6.91577567105688));
#63936=CARTESIAN_POINT('Ctrl Pts',(-2.25765350906011,-2.01580609934939,
7.07433711546564));
#63937=CARTESIAN_POINT('Ctrl Pts',(0.46527788615717,-2.99065044527086,7.23289855987439));
#63938=CARTESIAN_POINT('Ctrl Pts',(2.76335142476968,-1.23465076048616,7.39146000428313));
#63939=CARTESIAN_POINT('Ctrl Pts',(2.53813383284947,1.64874201853731,7.55002144869191));
#63940=CARTESIAN_POINT('Ctrl Pts',(-0.00472259831748953,3.02662374506822,
7.70858289310063));
#63941=CARTESIAN_POINT('Ctrl Pts',(-2.54326669687965,1.64081324521975,7.86714433750941));
#63942=CARTESIAN_POINT('Ctrl Pts',(-2.7594849988412,-1.24326832916955,8.02570578191813));
#63943=CARTESIAN_POINT('Ctrl Pts',(-0.455942708646288,-2.99208787363906,
8.18426722632691));
#63944=CARTESIAN_POINT('Ctrl Pts',(2.26393323438981,-2.00875083257506,8.34282867073565));
#63945=CARTESIAN_POINT('Ctrl Pts',(2.91655034119946,0.808831072842144,8.50139011514441));
#63946=CARTESIAN_POINT('Ctrl Pts',(0.905986231991998,2.88784738942115,8.65995155955315));
#63947=CARTESIAN_POINT('Ctrl Pts',(-1.93185847680866,2.3298919337017,8.81851300396191));
#63948=CARTESIAN_POINT('Ctrl Pts',(-3.00567081669626,-0.355551035445139,
8.97707444837065));
#63949=CARTESIAN_POINT('Ctrl Pts',(-1.33492361736317,-2.7163307112632,9.13563589277941));
#63950=CARTESIAN_POINT('Ctrl Pts',(1.55477854131312,-2.59675514529536,9.29419733718816));
#63951=CARTESIAN_POINT('Ctrl Pts',(3.02477024692428,-0.106012029823702,
9.45275878159692));
#63952=CARTESIAN_POINT('Ctrl Pts',(1.73276220557981,2.48153354522155,9.61132022600566));
#63953=CARTESIAN_POINT('Ctrl Pts',(-1.14147799974873,2.8031235387038,9.76988167041442));
#63954=CARTESIAN_POINT('Ctrl Pts',(-2.97340368559691,0.565105405764596,
9.92844311482316));
#63955=CARTESIAN_POINT('Ctrl Pts',(-2.09023382474483,-2.18892579934503,
10.0870045592319));
#63956=CARTESIAN_POINT('Ctrl Pts',(0.701585230502688,-2.94418949143668,
10.2455660036407));
#63957=CARTESIAN_POINT('Ctrl Pts',(2.85276778415585,-1.01103390983099,10.4041274480494));
#63958=CARTESIAN_POINT('Ctrl Pts',(2.39901070446873,1.84532415499016,10.5626888924582));
#63959=CARTESIAN_POINT('Ctrl Pts',(-0.245348112796364,3.01666668703935,
10.7212503368669));
#63960=CARTESIAN_POINT('Ctrl Pts',(-2.66567291420564,1.43340905243968,10.8798117812757));
#63961=CARTESIAN_POINT('Ctrl Pts',(-2.65189948220728,-1.45873326328511,
11.0383732256844));
#63962=CARTESIAN_POINT('Ctrl Pts',(-0.216604711106824,-3.01886667414644,
11.1969346700932));
#63963=CARTESIAN_POINT('Ctrl Pts',(2.4164776962198,-1.8223910504658,11.3554961145019));
#63964=CARTESIAN_POINT('Ctrl Pts',(2.84300878208006,1.03815926627918,11.5140575589107));
#63965=CARTESIAN_POINT('Ctrl Pts',(0.67351144406832,2.95073820117182,11.6726190033194));
#63966=CARTESIAN_POINT('Ctrl Pts',(-2.11098745975819,2.16891805790105,11.8311804477282));
#63967=CARTESIAN_POINT('Ctrl Pts',(-2.96788646220135,-0.593399987047231,
11.9897418921369));
#63968=CARTESIAN_POINT('Ctrl Pts',(-1.11472784425878,-2.81386841028145,
12.1483033365457));
#63969=CARTESIAN_POINT('Ctrl Pts',(1.75631900069801,-2.46491727344607,12.3068647809544));
#63970=CARTESIAN_POINT('Ctrl Pts',(3.02362333316682,0.134816676545898,12.4654262253632));
#63971=CARTESIAN_POINT('Ctrl Pts',(1.52997519673727,2.6114458628343,12.6239876697719));
#63972=CARTESIAN_POINT('Ctrl Pts',(-1.36073478613619,2.70349300700863,12.7825491141807));
#63973=CARTESIAN_POINT('Ctrl Pts',(-3.0089209314377,0.326907365321966,12.9411105585894));
#63974=CARTESIAN_POINT('Ctrl Pts',(-1.90957976960207,-2.34818625766188,
13.0996720029982));
#63975=CARTESIAN_POINT('Ctrl Pts',(0.9334504693777,-2.87908732385182,13.2582334474069));
#63976=CARTESIAN_POINT('Ctrl Pts',(2.92412176875259,-0.781015671195471,
13.4167948918157));
#63977=CARTESIAN_POINT('Ctrl Pts',(2.24469817626766,2.03022257267676,13.5753563362244));
#63978=CARTESIAN_POINT('Ctrl Pts',(-0.484420199200288,2.98760952397606,
13.7339177806332));
#63979=CARTESIAN_POINT('Ctrl Pts',(-2.77120135286706,1.21692919227597,13.892479225042));
#63980=CARTESIAN_POINT('Ctrl Pts',(-2.52752339375828,-1.66496218910528,
14.0510406694507));
#63981=CARTESIAN_POINT('Ctrl Pts',(0.0241047248984299,-3.02653144034276,
14.2096021138595));
#63982=CARTESIAN_POINT('Ctrl Pts',(2.55372216550858,-1.62449275114906,14.3681635582682));
#63983=CARTESIAN_POINT('Ctrl Pts',(2.75146663755133,1.26091432682304,14.526725002677));
#63984=CARTESIAN_POINT('Ctrl Pts',(0.436772300596569,2.99494633584264,14.6852864470857));
#63985=CARTESIAN_POINT('Ctrl Pts',(-2.27675066969048,1.99421161996656,14.8438478914945));
#63986=CARTESIAN_POINT('Ctrl Pts',(-2.91131085595766,-0.827491810913372,
15.0024093359032));
#63987=CARTESIAN_POINT('Ctrl Pts',(-0.887474142281572,-2.89359002692629,
15.160970780312));
#63988=CARTESIAN_POINT('Ctrl Pts',(1.94673927980861,-2.31747271258928,15.3195322247207));
#63989=CARTESIAN_POINT('Ctrl Pts',(3.00333226818571,0.374791787556893,15.4780936691295));
#63990=CARTESIAN_POINT('Ctrl Pts',(1.31750110941066,2.72482374179457,15.6366551135382));
#63991=CARTESIAN_POINT('Ctrl Pts',(-1.5713760441821,2.58674523772951,15.795216557947));
#63992=CARTESIAN_POINT('Ctrl Pts',(-3.02538711470083,0.0866395022367191,
15.9537780023557));
#63993=CARTESIAN_POINT('Ctrl Pts',(-1.71683515956719,-2.49257911248963,
16.1123394467645));
#63994=CARTESIAN_POINT('Ctrl Pts',(1.15940554188062,-2.79575613861477,16.2709008911732));
#63995=CARTESIAN_POINT('Ctrl Pts',(2.97696159891635,-0.546052411150268,
16.429462335582));
#63996=CARTESIAN_POINT('Ctrl Pts',(2.07617328210605,2.20226658236796,16.5880237799907));
#63997=CARTESIAN_POINT('Ctrl Pts',(-0.720425166281659,2.93963623207596,
16.7465852243995));
#63998=CARTESIAN_POINT('Ctrl Pts',(-2.85918385675924,0.992744312697378,
16.9051466688082));
#63999=CARTESIAN_POINT('Ctrl Pts',(-2.38714422399272,-1.86064936272363,
17.063708113217));
#64000=CARTESIAN_POINT('Ctrl Pts',(0.264661541199501,-3.01503364255784,
17.2222695576257));
#64001=CARTESIAN_POINT('Ctrl Pts',(2.67479767526346,-1.41630893294889,17.3808310020345));
#64002=CARTESIAN_POINT('Ctrl Pts',(2.64250350912616,1.47568587490753,17.5393924464433));
#64003=CARTESIAN_POINT('Ctrl Pts',(0.197267721734377,3.02019188845799,17.697953890852));
#64004=CARTESIAN_POINT('Ctrl Pts',(-2.42809857245107,1.80687877833759,17.8565153352607));
#64005=CARTESIAN_POINT('Ctrl Pts',(-2.83630220791474,-1.05634434846013,
18.0150767796695));
#64006=CARTESIAN_POINT('Ctrl Pts',(-0.654601374265098,-2.95499080167026,
18.1736382240782));
#64007=CARTESIAN_POINT('Ctrl Pts',(2.12483372760391,-2.15535501186755,18.332199668487));
#64008=CARTESIAN_POINT('Ctrl Pts',(2.96402552539639,0.612393894437513,18.4907611128958));
#64009=CARTESIAN_POINT('Ctrl Pts',(1.09668522891184,2.82094932705857,18.6493225573045));
#64010=CARTESIAN_POINT('Ctrl Pts',(-1.77206809318166,2.45361942246004,18.8078840017132));
#64011=CARTESIAN_POINT('Ctrl Pts',(-3.02269797931083,-0.154176921151835,
18.966445446122));
#64012=CARTESIAN_POINT('Ctrl Pts',(-1.51322036224401,-2.62119013664323,
19.1250068905308));
#64013=CARTESIAN_POINT('Ctrl Pts',(1.37801980748479,-2.69472354933216,19.2835683349395));
#64014=CARTESIAN_POINT('Ctrl Pts',(3.01095271786289,-0.307631805800035,
19.4421297793482));
#64015=CARTESIAN_POINT('Ctrl Pts',(1.89450304181512,2.3603668828593,19.600691223757));
#64016=CARTESIAN_POINT('Ctrl Pts',(-0.951868742340097,2.87305055550742,
19.7592526681658));
#64017=CARTESIAN_POINT('Ctrl Pts',(-2.92906336232834,0.76227384620716,19.9178141125745));
#64018=CARTESIAN_POINT('Ctrl Pts',(-2.23165078734232,-2.04455578561703,
20.0763755569833));
#64019=CARTESIAN_POINT('Ctrl Pts',(0.503542645942066,-2.98444607940289,
20.234937001392));
#64020=CARTESIAN_POINT('Ctrl Pts',(2.77893763268742,-1.19915771722462,20.3934984458008));
#64021=CARTESIAN_POINT('Ctrl Pts',(2.51680929973837,1.68111407878709,20.5520598902095));
#64022=CARTESIAN_POINT('Ctrl Pts',(-0.0434858629331975,3.02631501613275,
20.7106213346183));
#64023=CARTESIAN_POINT('Ctrl Pts',(-2.56407290478473,1.60810563586303,20.869182779027));
#64024=CARTESIAN_POINT('Ctrl Pts',(-2.74333543731449,-1.27850861378411,
21.0277442234358));
#64025=CARTESIAN_POINT('Ctrl Pts',(-0.417583980308469,-2.99768197388171,
21.1863056678445));
#64026=CARTESIAN_POINT('Ctrl Pts',(2.28947473437029,-1.97959062379721,21.3448671122533));
#64027=CARTESIAN_POINT('Ctrl Pts',(2.90595197648197,0.846118613154382,21.503428556662));
#64028=CARTESIAN_POINT('Ctrl Pts',(0.868925656837218,2.89921399693704,21.6619900010708));
#64029=CARTESIAN_POINT('Ctrl Pts',(-1.96154024611074,2.30495845082584,21.8205514454795));
#64030=CARTESIAN_POINT('Ctrl Pts',(-3.00087055159965,-0.39401716928028,
21.9791128898883));
#64031=CARTESIAN_POINT('Ctrl Pts',(-1.30002457011512,-2.73320502601664,
22.137674334297));
#64032=CARTESIAN_POINT('Ctrl Pts',(1.5879091041769,-2.57662924651915,22.2962357787058));
#64033=CARTESIAN_POINT('Ctrl Pts',(3.0258799099222,-0.0672634215228445,
22.4547972231145));
#64034=CARTESIAN_POINT('Ctrl Pts',(1.70083770533339,2.50352245791043,22.6133586675233));
#64035=CARTESIAN_POINT('Ctrl Pts',(-1.17728553624331,2.78827408324539,22.771920111932));
#64036=CARTESIAN_POINT('Ctrl Pts',(-2.98039742563387,0.526977022668581,
22.9304815563408));
#64037=CARTESIAN_POINT('Ctrl Pts',(-2.06202759461993,-2.21551704939764,
23.0890430007495));
#64038=CARTESIAN_POINT('Ctrl Pts',(0.739235557084079,-2.93496241684426,
23.2476044451583));
#64039=CARTESIAN_POINT('Ctrl Pts',(2.86548267288157,-0.974414002650417,
23.406165889567));
#64040=CARTESIAN_POINT('Ctrl Pts',(2.37517984560405,1.87589826434749,23.5647273339758));
#64041=CARTESIAN_POINT('Ctrl Pts',(-0.283964115707739,3.0132769501219,23.7232887783845));
#64042=CARTESIAN_POINT('Ctrl Pts',(-2.68381274160463,1.39915072995952,23.8818502227933));
#64043=CARTESIAN_POINT('Ctrl Pts',(-2.63299916572745,-1.49257796795484,
24.0404116672021));
#64044=CARTESIAN_POINT('Ctrl Pts',(-0.177922642319488,-3.02139324327301,
24.1989731116108));
#64045=CARTESIAN_POINT('Ctrl Pts',(2.43961987121247,-1.79129240525688,24.3575345560196));
#64046=CARTESIAN_POINT('Ctrl Pts',(2.8294793156556,1.07448610946012,24.5160960004283));
#64047=CARTESIAN_POINT('Ctrl Pts',(0.635664458950241,2.95912221659957,24.6746574448371));
#64048=CARTESIAN_POINT('Ctrl Pts',(-2.13859285501431,2.14170357370654,24.8332188892458));
#64049=CARTESIAN_POINT('Ctrl Pts',(-2.96004303250402,-0.631362687264734,
24.9917803336546));
#64050=CARTESIAN_POINT('Ctrl Pts',(-1.07859763798547,-2.82791455537078,
25.1503417780633));
#64051=CARTESIAN_POINT('Ctrl Pts',(1.78774451231545,-2.44222094738204,25.3089032224721));
#64052=CARTESIAN_POINT('Ctrl Pts',(3.02164866318236,0.173530842889411,25.4674646668808));
#64053=CARTESIAN_POINT('Ctrl Pts',(1.49640346986859,2.63082691420604,25.6260261112896));
#64054=CARTESIAN_POINT('Ctrl Pts',(-1.39524831558989,2.68584357976953,25.7845875556983));
#64055=CARTESIAN_POINT('Ctrl Pts',(-3.0128610236943,0.288343630152394,25.9431490001071));
#64056=CARTESIAN_POINT('Ctrl Pts',(-1.87934861956321,-2.37245070829545,
26.1017104445158));
#64057=CARTESIAN_POINT('Ctrl Pts',(0.970247978715583,-2.8668959620021,26.2602718889246));
#64058=CARTESIAN_POINT('Ctrl Pts',(2.93388483363149,-0.743500760008172,
26.4188333333333));
#64059=CARTESIAN_POINT('Ctrl Pts',(2.2185118773636,2.0588051503584,26.5773947777421));
#64060=CARTESIAN_POINT('Ctrl Pts',(-0.522644442162044,2.98116024128573,
26.7359562221508));
#64061=CARTESIAN_POINT('Ctrl Pts',(-2.7865599469623,1.18133706414857,26.8945176665596));
#64062=CARTESIAN_POINT('Ctrl Pts',(-2.50599199017975,-1.69719702518614,
27.0530791109683));
#64063=CARTESIAN_POINT('Ctrl Pts',(0.0628652175921859,-3.02597448131387,
27.2116405553771));
#64064=CARTESIAN_POINT('Ctrl Pts',(2.57431849021943,-1.59165257140494,27.3702019997858));
#64065=CARTESIAN_POINT('Ctrl Pts',(2.73509173159499,1.29605046850281,27.5287634441946));
#64066=CARTESIAN_POINT('Ctrl Pts',(0.398378534703953,3.00029467556651,27.6873248886033));
#64067=CARTESIAN_POINT('Ctrl Pts',(-2.30210490660938,1.9648884436809,27.8458863330121));
#64068=CARTESIAN_POINT('Ctrl Pts',(-2.90047392254249,-0.864710715671257,
28.0044477774208));
#64069=CARTESIAN_POINT('Ctrl Pts',(-0.85034153634106,-2.90471906881178,
28.1630092218296));
#64070=CARTESIAN_POINT('Ctrl Pts',(1.97626076872048,-2.29234966162712,28.3215706662384));
#64071=CARTESIAN_POINT('Ctrl Pts',(2.99828576789421,0.413226392173409,28.4801321106471));
#64072=CARTESIAN_POINT('Ctrl Pts',(1.2824947161976,2.74147422020906,28.6386935550559));
#64073=CARTESIAN_POINT('Ctrl Pts',(-1.60437704326902,2.56640758652578,28.7972549994646));
#64074=CARTESIAN_POINT('Ctrl Pts',(-3.02624861237858,0.0478845823042429,
28.9558164438734));
#64075=CARTESIAN_POINT('Ctrl Pts',(-1.68477049894157,-2.51436313269221,
29.1143778882821));
#64076=CARTESIAN_POINT('Ctrl Pts',(1.19511724956988,-2.78067767943826,29.2729393326909));
#64077=CARTESIAN_POINT('Ctrl Pts',(2.98371102484459,-0.507880022610132,
29.4315007770996));
#64078=CARTESIAN_POINT('Ctrl Pts',(2.0477973424077,2.22867665702622,29.5900622215084));
#64079=CARTESIAN_POINT('Ctrl Pts',(-0.758015631487026,2.93016823741693,
29.7486236659171));
#64080=CARTESIAN_POINT('Ctrl Pts',(-2.87166397420542,0.956043731424721,
29.9071851103259));
#64081=CARTESIAN_POINT('Ctrl Pts',(-2.36311805996753,-1.8910702344971,30.0657465547346));
#64082=CARTESIAN_POINT('Ctrl Pts',(0.303255044713435,-3.01139668177433,
30.2243079991434));
#64083=CARTESIAN_POINT('Ctrl Pts',(2.69271774351707,-1.38193514713752,30.3828694435521));
#64084=CARTESIAN_POINT('Ctrl Pts',(2.62338684178872,1.50940884967445,30.5414308879609));
#64085=CARTESIAN_POINT('Ctrl Pts',(0.158570266212879,3.02247068932337,30.6999923323696));
#64086=CARTESIAN_POINT('Ctrl Pts',(-2.45104112001013,1.77563257042811,30.8585537767784));
#64087=CARTESIAN_POINT('Ctrl Pts',(-2.82254038511267,-1.09258380527705,
31.0171152211871));
#64088=CARTESIAN_POINT('Ctrl Pts',(-0.616701474735501,-2.96313227652845,
31.1756766655959));
#64089=CARTESIAN_POINT('Ctrl Pts',(2.15226427772119,-2.12796430326989,31.3342381100046));
#64090=CARTESIAN_POINT('Ctrl Pts',(2.95593914684811,0.65030558760985,31.4927995544134));
#64091=CARTESIAN_POINT('Ctrl Pts',(1.06046581326025,2.83476380957074,31.6513609988221));
#64092=CARTESIAN_POINT('Ctrl Pts',(-1.80334761520199,2.43072231566893,31.8099224432309));
#64093=CARTESIAN_POINT('Ctrl Pts',(-3.02047542781434,-0.19287764804512,
31.9684838876396));
#64094=CARTESIAN_POINT('Ctrl Pts',(-1.47952520927975,-2.64035580031392,
32.1270453320484));
#64095=CARTESIAN_POINT('Ctrl Pts',(1.41241960390228,-2.67685346249252,32.2856067764571));
#64096=CARTESIAN_POINT('Ctrl Pts',(3.01464577067142,-0.269043629396191,
32.4441682208659));
#64097=CARTESIAN_POINT('Ctrl Pts',(1.8641171243363,2.38443723840698,32.6027296652746));
#64098=CARTESIAN_POINT('Ctrl Pts',(-0.988587424762973,2.86062379573864,
32.7612911096834));
#64099=CARTESIAN_POINT('Ctrl Pts',(-2.93858598493123,0.724697182491683,
32.9198525540921));
#64100=CARTESIAN_POINT('Ctrl Pts',(-2.20528198516443,-2.07297008252769,
33.0784139985009));
#64101=CARTESIAN_POINT('Ctrl Pts',(0.541724804486454,-2.97775214437831,
33.2369754429096));
#64102=CARTESIAN_POINT('Ctrl Pts',(2.79406798309702,-1.16346796388132,33.3955368873184));
#64103=CARTESIAN_POINT('Ctrl Pts',(2.49507190870534,1.71321036873323,33.5540983317272));
#64104=CARTESIAN_POINT('Ctrl Pts',(-0.0822419941187573,3.0255098498515,
33.7126597761359));
#64105=CARTESIAN_POINT('Ctrl Pts',(-2.58445850163663,1.57513423252295,33.8712212205446));
#64106=CARTESIAN_POINT('Ctrl Pts',(-2.72673585847062,-1.31353917157969,
34.0297826649534));
#64107=CARTESIAN_POINT('Ctrl Pts',(-0.379156751408429,-3.00278433374826,
34.1883441093622));
#64108=CARTESIAN_POINT('Ctrl Pts',(2.31464066844022,-1.95010568256221,34.3469055537709));
#64109=CARTESIAN_POINT('Ctrl Pts',(2.89487691879338,0.883267355995366,34.5054669981796));
#64110=CARTESIAN_POINT('Ctrl Pts',(0.831722542943288,2.9101050167805,34.6640284425885));
#64111=CARTESIAN_POINT('Ctrl Pts',(-1.99090024395484,2.27964686209391,34.8225898869971));
#64112=CARTESIAN_POINT('Ctrl Pts',(-2.99557802304852,-0.432418668472894,
34.9811513314059));
#64113=CARTESIAN_POINT('Ctrl Pts',(-1.26491226661167,-2.74963098521777,
35.1397127758147));
#64114=CARTESIAN_POINT('Ctrl Pts',(1.62077918618811,-2.55608067700269,35.2982742202234));
#64115=CARTESIAN_POINT('Ctrl Pts',(3.02649320678206,-0.0285037792053614,
35.4568356646322));
#64116=CARTESIAN_POINT('Ctrl Pts',(1.6686341996346,2.52510069204211,35.6153971090409));
#64117=CARTESIAN_POINT('Ctrl Pts',(-1.21289995118223,2.77296723912937,35.7739585534497));
#64118=CARTESIAN_POINT('Ctrl Pts',(-2.98690225949438,0.488762193381373,
35.9325199978584));
#64119=CARTESIAN_POINT('Ctrl Pts',(-2.03348311127567,-2.24174486410168,
36.0910814422672));
#64120=CARTESIAN_POINT('Ctrl Pts',(0.776764623540637,-2.92525389321091,
36.2496428866759));
#64121=CARTESIAN_POINT('Ctrl Pts',(2.87772749916196,-0.937634247041048,
36.4082043310847));
#64122=CARTESIAN_POINT('Ctrl Pts',(2.35095937714186,1.90616464074957,36.5667657754934));
#64123=CARTESIAN_POINT('Ctrl Pts',(-0.322533566468511,3.00939293411291,
36.7253272199022));
#64124=CARTESIAN_POINT('Ctrl Pts',(-2.70151225974056,1.36466285332016,36.883888664311));
#64125=CARTESIAN_POINT('Ctrl Pts',(-2.61366703848361,-1.52617775887959,
37.0424501087197));
#64126=CARTESIAN_POINT('Ctrl Pts',(-0.139211182967247,-3.02342431778626,
37.2010115531285));
#64127=CARTESIAN_POINT('Ctrl Pts',(2.4623614610291,-1.75989965779052,37.3595729975371));
#64128=CARTESIAN_POINT('Ctrl Pts',(2.8154864438876,1.1106362009136,37.518134441946));
#64129=CARTESIAN_POINT('Ctrl Pts',(0.597711781573062,2.96702175728379,37.6766958863547));
#64130=CARTESIAN_POINT('Ctrl Pts',(-2.16584472998421,2.11413596992682,37.8352573307635));
#64131=CARTESIAN_POINT('Ctrl Pts',(-2.9517191980829,-0.669218395448239,
37.9938187751722));
#64132=CARTESIAN_POINT('Ctrl Pts',(-1.04228065031701,-2.84150334027313,
38.152380219581));
#64133=CARTESIAN_POINT('Ctrl Pts',(1.81885797164076,-2.41911153657142,38.3109416639897));
#64134=CARTESIAN_POINT('Ctrl Pts',(3.01921417384548,0.212192764679598,38.4695031083984));
#64135=CARTESIAN_POINT('Ctrl Pts',(1.46251786451651,2.64982177476087,38.6280645528072));
#64136=CARTESIAN_POINT('Ctrl Pts',(-1.429402439371,2.66766699375318,38.786625997216));
#64137=CARTESIAN_POINT('Ctrl Pts',(-3.01655597425476,0.249897813151183,
38.9451874416247));
#64138=CARTESIAN_POINT('Ctrl Pts',(-1.84833359844375,-2.39664153302016,
39.1037488860335));
#64139=CARTESIAN_POINT('Ctrl Pts',(1.00597614714323,-2.85362950697119,39.2623103304422));
#64140=CARTESIAN_POINT('Ctrl Pts',(2.94492748067747,-0.707041802870931,
39.420871774851));
#64141=CARTESIAN_POINT('Ctrl Pts',(2.18838961321059,2.08950618451892,39.5794332192597));
#64142=CARTESIAN_POINT('Ctrl Pts',(0.361364824312418,2.67510712391322,39.6851408488656));
#64143=CARTESIAN_POINT('Ctrl Pts',(-0.474664453622152,2.51747565713064,
39.7379946636685));
#64144=CARTESIAN_POINT('Ctrl Pts',(-1.20564430054356,2.47375567929507,-0.109744663668475));
#64145=CARTESIAN_POINT('Ctrl Pts',(-2.02715459737193,2.07337288664547,-0.0568908488655582));
#64146=CARTESIAN_POINT('Ctrl Pts',(-3.22591201434709,0.396938321840822,
0.0488167807402761));
#64147=CARTESIAN_POINT('Ctrl Pts',(-2.08416667989131,-2.49808316060539,
0.207378225149028));
#64148=CARTESIAN_POINT('Ctrl Pts',(0.963414872632741,-3.1041939934932,0.365939669557779));
#64149=CARTESIAN_POINT('Ctrl Pts',(3.12987608714624,-0.879703367138011,
0.524501113966532));
#64150=CARTESIAN_POINT('Ctrl Pts',(2.43909306726452,2.15010239123153,0.683062558375283));
#64151=CARTESIAN_POINT('Ctrl Pts',(-0.479274468080505,3.21552770689972,
0.841624002784034));
#64152=CARTESIAN_POINT('Ctrl Pts',(-2.95980306988425,1.34532463900819,1.00018544719279));
#64153=CARTESIAN_POINT('Ctrl Pts',(-2.73776025065754,-1.75362282654376,
1.15874689160154));
#64154=CARTESIAN_POINT('Ctrl Pts',(-0.0157392478644119,-3.2511367042434,
1.31730833601029));
#64155=CARTESIAN_POINT('Ctrl Pts',(2.72062483828669,-1.78002968372146,1.47586978041904));
#64156=CARTESIAN_POINT('Ctrl Pts',(2.97272771949037,1.31651274994322,1.63443122482779));
#64157=CARTESIAN_POINT('Ctrl Pts',(0.510344372216115,3.21088965713636,1.79299266923654));
#64158=CARTESIAN_POINT('Ctrl Pts',(-2.41804410895251,2.17332768185625,1.9515541136453));
#64159=CARTESIAN_POINT('Ctrl Pts',(-3.13845311149299,-0.848764793424488,
2.11011555805404));
#64160=CARTESIAN_POINT('Ctrl Pts',(-0.993054319402781,-3.09582394518012,
2.2686770024628));
#64161=CARTESIAN_POINT('Ctrl Pts',(2.05912870633672,-2.51600395318794,2.42723844687155));
#64162=CARTESIAN_POINT('Ctrl Pts',(3.23106577827023,0.361248355871118,2.58579989128031));
#64163=CARTESIAN_POINT('Ctrl Pts',(1.45262889441719,2.90863453724861,2.74436133568905));
#64164=CARTESIAN_POINT('Ctrl Pts',(-1.65224274345245,2.80006787716128,2.90292278009781));
#64165=CARTESIAN_POINT('Ctrl Pts',(-3.24840676708004,0.134683172671852,
3.06148422450655));
#64166=CARTESIAN_POINT('Ctrl Pts',(-1.87836244833034,-2.65368432378687,
3.22004566891531));
#64167=CARTESIAN_POINT('Ctrl Pts',(1.20686555247667,-3.01890072833779,3.37860711332406));
#64168=CARTESIAN_POINT('Ctrl Pts',(3.19007189253275,-0.627476984487285,
3.53716855773281));
#64169=CARTESIAN_POINT('Ctrl Pts',(2.26033706649506,2.33691300217663,3.69573000214156));
#64170=CARTESIAN_POINT('Ctrl Pts',(-0.73337283554914,3.16740435233008,3.85429144655032));
#64171=CARTESIAN_POINT('Ctrl Pts',(-3.05742011265761,1.10565288291763,4.01285289095907));
#64172=CARTESIAN_POINT('Ctrl Pts',(-2.58965416442564,-1.96570021882515,
4.17141433536782));
#64173=CARTESIAN_POINT('Ctrl Pts',(0.242795234836198,-3.24211913991506,
4.32997577977658));
#64174=CARTESIAN_POINT('Ctrl Pts',(2.8535417204786,-1.55807114478789,4.48853722418531));
#64175=CARTESIAN_POINT('Ctrl Pts',(2.85864187046401,1.54869386873951,4.64709866859408));
#64176=CARTESIAN_POINT('Ctrl Pts',(0.253438599627609,3.24130450885329,4.80566011300282));
#64177=CARTESIAN_POINT('Ctrl Pts',(-2.58318633003087,1.97419209478631,4.96422155741158));
#64178=CARTESIAN_POINT('Ctrl Pts',(-3.06103376339185,-1.09560866286668,
5.12278300182033));
#64179=CARTESIAN_POINT('Ctrl Pts',(-0.743768249416836,-3.16497943657876,
5.28134444622908));
#64180=CARTESIAN_POINT('Ctrl Pts',(2.25265222476723,-2.34432164965467,5.43990589063783));
#64181=CARTESIAN_POINT('Ctrl Pts',(3.19211485856089,0.616999815676252,5.59846733504658));
#64182=CARTESIAN_POINT('Ctrl Pts',(1.21677084197797,3.01492201572549,5.75702877945533));
#64183=CARTESIAN_POINT('Ctrl Pts',(-1.86963963033482,2.65983715581851,5.91559022386409));
#64184=CARTESIAN_POINT('Ctrl Pts',(-3.24883144988067,-0.124017148241245,
6.07415166827284));
#64185=CARTESIAN_POINT('Ctrl Pts',(-1.66142716131023,-2.79462803078564,
6.23271311268159));
#64186=CARTESIAN_POINT('Ctrl Pts',(1.44307132765125,-2.9133882655943,6.39127455709034));
#64187=CARTESIAN_POINT('Ctrl Pts',(3.22986224994229,-0.371854661379337,
6.54983600149909));
#64188=CARTESIAN_POINT('Ctrl Pts',(2.06737835504244,2.50922951917395,6.70839744590785));
#64189=CARTESIAN_POINT('Ctrl Pts',(-0.982884785006702,3.09906817320855,
6.86695889031659));
#64190=CARTESIAN_POINT('Ctrl Pts',(-3.13564917114702,0.859063628770815,
7.02552033472535));
#64191=CARTESIAN_POINT('Ctrl Pts',(-2.42516725748781,-2.16537521367566,
7.1840817791341));
#64192=CARTESIAN_POINT('Ctrl Pts',(0.499800651700313,-3.21255122159192,
7.34264322354285));
#64193=CARTESIAN_POINT('Ctrl Pts',(2.96838703077778,-1.32625958179467,7.5012046679516));
#64194=CARTESIAN_POINT('Ctrl Pts',(2.72645870672651,1.77107565149178,7.65976611236035));
#64195=CARTESIAN_POINT('Ctrl Pts',(-0.00507300644854954,3.2511936742368,
7.8183275567691));
#64196=CARTESIAN_POINT('Ctrl Pts',(-2.73197241985096,1.76255857774021,7.97688900117786));
#64197=CARTESIAN_POINT('Ctrl Pts',(-2.96423372313876,-1.33551655826455,
8.1354504455866));
#64198=CARTESIAN_POINT('Ctrl Pts',(-0.489772821144476,-3.21409530450794,
8.29401188999536));
#64199=CARTESIAN_POINT('Ctrl Pts',(2.43191292691616,-2.15779645905029,8.45257333440411));
#64200=CARTESIAN_POINT('Ctrl Pts',(3.13295302574422,0.868844854546515,8.61113477881286));
#64201=CARTESIAN_POINT('Ctrl Pts',(0.973208748261957,3.10212036760313,8.76969622322162));
#64202=CARTESIAN_POINT('Ctrl Pts',(-2.0751988315547,2.50276564070748,8.92825766763037));
#64203=CARTESIAN_POINT('Ctrl Pts',(-3.22868607702037,-0.381932269972927,
9.08681911203912));
#64204=CARTESIAN_POINT('Ctrl Pts',(-1.43397250068901,-2.91787746659443,
9.24538055644787));
#64205=CARTESIAN_POINT('Ctrl Pts',(1.67014025664517,-2.78942961300785,9.40394200085662));
#64206=CARTESIAN_POINT('Ctrl Pts',(3.24920264993105,-0.11387792794435,9.56250344526537));
#64207=CARTESIAN_POINT('Ctrl Pts',(1.86132998226725,2.66565878159693,9.72106488967412));
#64208=CARTESIAN_POINT('Ctrl Pts',(-1.22617357314765,3.01111016259887,9.87962633408288));
#64209=CARTESIAN_POINT('Ctrl Pts',(-3.19402478399152,0.607035190116496,
10.0381877784916));
#64210=CARTESIAN_POINT('Ctrl Pts',(-2.24532533974844,-2.35134007780147,
10.1967492229004));
#64211=CARTESIAN_POINT('Ctrl Pts',(0.753641567461229,-3.16264295022161,
10.3553106673091));
#64212=CARTESIAN_POINT('Ctrl Pts',(3.06443791998503,-1.08605077107364,10.5138721117179));
#64213=CARTESIAN_POINT('Ctrl Pts',(2.57701289745849,1.98224382181518,10.6724335561266));
#64214=CARTESIAN_POINT('Ctrl Pts',(-0.263552492644499,3.24049782076964,
10.8309950005354));
#64215=CARTESIAN_POINT('Ctrl Pts',(-2.86346095393319,1.53976537436449,10.9895564449442));
#64216=CARTESIAN_POINT('Ctrl Pts',(-2.84866555854953,-1.56696859519441,
11.1481178893529));
#64217=CARTESIAN_POINT('Ctrl Pts',(-0.232676383282734,-3.24286104288395,
11.3066793337616));
#64218=CARTESIAN_POINT('Ctrl Pts',(2.59577590795226,-1.95760912300858,11.4652407781704));
#64219=CARTESIAN_POINT('Ctrl Pts',(3.05395481785924,1.11518877920565,11.6238022225792));
#64220=CARTESIAN_POINT('Ctrl Pts',(0.723484757578079,3.16967756220472,11.7823636669879));
#64221=CARTESIAN_POINT('Ctrl Pts',(-2.26761885640482,2.3298477986489,11.9409251113967));
#64222=CARTESIAN_POINT('Ctrl Pts',(-3.188098192742,-0.637429177420582,12.0994865558054));
#64223=CARTESIAN_POINT('Ctrl Pts',(-1.19743860519664,-3.02265228393486,
12.2580480002142));
#64224=CARTESIAN_POINT('Ctrl Pts',(1.88663464836552,-2.64780961294021,12.4166094446229));
#64225=CARTESIAN_POINT('Ctrl Pts',(3.24797063727694,0.144819826607834,12.5751708890317));
#64226=CARTESIAN_POINT('Ctrl Pts',(1.64349654940643,2.80521035483633,12.7337323334404));
#64227=CARTESIAN_POINT('Ctrl Pts',(-1.46169881083137,2.90408722823644,12.8922937778492));
#64228=CARTESIAN_POINT('Ctrl Pts',(-3.23217734431291,0.351163292076785,
13.0508552222579));
#64229=CARTESIAN_POINT('Ctrl Pts',(-2.05126708514628,-2.52241736994243,
13.2094166666667));
#64230=CARTESIAN_POINT('Ctrl Pts',(1.00271078167531,-3.09271032123992,13.3679781110754));
#64231=CARTESIAN_POINT('Ctrl Pts',(3.14108623933113,-0.838965601128271,
13.5265395554842));
#64232=CARTESIAN_POINT('Ctrl Pts',(2.41125066277032,2.18086136287512,13.6851009998929));
#64233=CARTESIAN_POINT('Ctrl Pts',(-0.520363289252294,3.209284669516,13.8436624443017));
#64234=CARTESIAN_POINT('Ctrl Pts',(-2.97681940913832,1.3072231057357,14.0022238887104));
#64235=CARTESIAN_POINT('Ctrl Pts',(-2.71506099252092,-1.78849932895798,
14.1607853331192));
#64236=CARTESIAN_POINT('Ctrl Pts',(0.0258932512628897,-3.25109452067006,
14.3193467775279));
#64237=CARTESIAN_POINT('Ctrl Pts',(2.74320366507031,-1.74502713295143,14.4779082219367));
#64238=CARTESIAN_POINT('Ctrl Pts',(2.95562041415185,1.35447185657016,14.6364696663454));
#64239=CARTESIAN_POINT('Ctrl Pts',(0.469180003987954,3.21716585936283,14.7950311107542));
#64240=CARTESIAN_POINT('Ctrl Pts',(-2.44568139240097,2.14217846354022,14.9535925551629));
#64241=CARTESIAN_POINT('Ctrl Pts',(-3.12732478030997,-0.888890185147194,
15.1121539995717));
#64242=CARTESIAN_POINT('Ctrl Pts',(-0.953323095457733,-3.10828909827557,
15.2707154439804));
#64243=CARTESIAN_POINT('Ctrl Pts',(2.09118376283658,-2.48942493617312,15.4292768883892));
#64244=CARTESIAN_POINT('Ctrl Pts',(3.2261740125007,0.402600650591831,15.5878383327979));
#64245=CARTESIAN_POINT('Ctrl Pts',(1.41525727461016,2.92700066440971,15.7463997772067));
#64246=CARTESIAN_POINT('Ctrl Pts',(-1.68796926377685,2.77867698866502,15.9049612216154));
#64247=CARTESIAN_POINT('Ctrl Pts',(-3.2498652881649,0.0930679943517114,
16.0635226660242));
#64248=CARTESIAN_POINT('Ctrl Pts',(-1.84422117866062,-2.67752390969185,
16.2220841104329));
#64249=CARTESIAN_POINT('Ctrl Pts',(1.24543130601543,-3.00319611493964,16.3806455548417));
#64250=CARTESIAN_POINT('Ctrl Pts',(3.19784668795183,-0.586568498256862,
16.5392069992504));
#64251=CARTESIAN_POINT('Ctrl Pts',(2.23022153064166,2.36567072244939,16.6977684436592));
#64252=CARTESIAN_POINT('Ctrl Pts',(-0.773879391910806,3.15775184736984,
16.856329888068));
#64253=CARTESIAN_POINT('Ctrl Pts',(-3.07133005340451,1.06640411938725,17.0148913324767));
#64254=CARTESIAN_POINT('Ctrl Pts',(-2.56426594590169,-1.99870613184649,
17.1734527768855));
#64255=CARTESIAN_POINT('Ctrl Pts',(0.28429894200228,-3.23874360738362,17.3320142212942));
#64256=CARTESIAN_POINT('Ctrl Pts',(2.873262755521,-1.52139645737976,17.4905756657029));
#64257=CARTESIAN_POINT('Ctrl Pts',(2.83857242150387,1.58517905949756,17.6491371101117));
#64258=CARTESIAN_POINT('Ctrl Pts',(0.211904624774947,3.24428458566613,17.8076985545204));
#64259=CARTESIAN_POINT('Ctrl Pts',(-2.60825903187995,1.94094586874764,17.9662599989292));
#64260=CARTESIAN_POINT('Ctrl Pts',(-3.04675062819489,-1.13472316112164,
18.124821443338));
#64261=CARTESIAN_POINT('Ctrl Pts',(-0.703171595288318,-3.17424569785823,
18.2833828877467));
#64262=CARTESIAN_POINT('Ctrl Pts',(2.28249249192199,-2.3152783994828,18.4419443321555));
#64263=CARTESIAN_POINT('Ctrl Pts',(3.18395078150948,0.657832397892554,18.6005057765642));
#64264=CARTESIAN_POINT('Ctrl Pts',(1.17805726089236,3.03025859174602,18.759067220973));
#64265=CARTESIAN_POINT('Ctrl Pts',(-1.9035522946178,2.63567348213832,18.9176286653817));
#64266=CARTESIAN_POINT('Ctrl Pts',(-3.24697662386251,-0.165616565844775,
19.0761901097904));
#64267=CARTESIAN_POINT('Ctrl Pts',(-1.62549853693258,-2.8156776358848,19.2347515541992));
#64268=CARTESIAN_POINT('Ctrl Pts',(1.48026634905252,-2.89466709288903,19.393312998608));
#64269=CARTESIAN_POINT('Ctrl Pts',(3.23435988556329,-0.330457521401717,
19.5518744430167));
#64270=CARTESIAN_POINT('Ctrl Pts',(2.03507169181765,2.53550177518263,19.7104358874255));
#64271=CARTESIAN_POINT('Ctrl Pts',(-1.02249565670092,3.08622563575957,19.8689973318342));
#64272=CARTESIAN_POINT('Ctrl Pts',(-3.14639449008423,0.818833167110018,
20.027558776243));
#64273=CARTESIAN_POINT('Ctrl Pts',(-2.39723518152376,-2.1962580739195,20.1861202206517));
#64274=CARTESIAN_POINT('Ctrl Pts',(0.540904586459818,-3.20588650315923,
20.3446816650605));
#64275=CARTESIAN_POINT('Ctrl Pts',(2.98512970672818,-1.2881330198395,20.5032431094692));
#64276=CARTESIAN_POINT('Ctrl Pts',(2.70355193238106,1.80584965922154,20.661804553878));
#64277=CARTESIAN_POINT('Ctrl Pts',(-0.0467124341827413,3.25086203818072,
20.8203659982867));
#64278=CARTESIAN_POINT('Ctrl Pts',(-2.75432241021104,1.72742412377537,20.9789274426955));
#64279=CARTESIAN_POINT('Ctrl Pts',(-2.94688589377513,-1.37337160734485,
21.1374888871042));
#64280=CARTESIAN_POINT('Ctrl Pts',(-0.448567945537823,-3.22010447672553,
21.296050331513));
#64281=CARTESIAN_POINT('Ctrl Pts',(2.45934955933615,-2.12647261627913,21.4546117759217));
#64282=CARTESIAN_POINT('Ctrl Pts',(3.1215682818087,0.908899061941314,21.6131732203305));
#64283=CARTESIAN_POINT('Ctrl Pts',(0.933398346422899,3.11433035654325,21.7717346647392));
#64284=CARTESIAN_POINT('Ctrl Pts',(-2.10708293368412,2.47598213914579,21.930296109148));
#64285=CARTESIAN_POINT('Ctrl Pts',(-3.22352964106027,-0.423252520367754,
22.0888575535567));
#64286=CARTESIAN_POINT('Ctrl Pts',(-1.39648400816177,-2.93600382454456,
22.2474189979655));
#64287=CARTESIAN_POINT('Ctrl Pts',(1.70572904649132,-2.76781040946589,22.4059804423742));
#64288=CARTESIAN_POINT('Ctrl Pts',(3.25039464788761,-0.0722542439966821,
22.564541886783));
#64289=CARTESIAN_POINT('Ctrl Pts',(1.82703674267198,2.68927923126595,22.7231033311917));
#64290=CARTESIAN_POINT('Ctrl Pts',(-1.26463796315678,2.99515890478861,22.8816647756005));
#64291=CARTESIAN_POINT('Ctrl Pts',(-3.20153744670834,0.56607775094599,23.0402262200092));
#64292=CARTESIAN_POINT('Ctrl Pts',(-2.21502625909608,-2.37990434982304,
23.198787664418));
#64293=CARTESIAN_POINT('Ctrl Pts',(0.79408547920078,-3.15273124362265,23.3573491088267));
#64294=CARTESIAN_POINT('Ctrl Pts',(3.07809623012716,-1.04671373396402,23.5159105532355));
#64295=CARTESIAN_POINT('Ctrl Pts',(2.55141383258672,2.01508647399485,23.6744719976443));
#64296=CARTESIAN_POINT('Ctrl Pts',(-0.305033732126069,3.23685657159181,
23.833033442053));
#64297=CARTESIAN_POINT('Ctrl Pts',(-2.88294672324543,1.50296514720743,23.9915948864617));
#64298=CARTESIAN_POINT('Ctrl Pts',(-2.82836287326186,-1.60332451485834,
24.1501563308705));
#64299=CARTESIAN_POINT('Ctrl Pts',(-0.191124175958415,-3.24557507880439,
24.3087177752792));
#64300=CARTESIAN_POINT('Ctrl Pts',(2.6206351898722,-1.92420301537947,24.4672792196881));
#64301=CARTESIAN_POINT('Ctrl Pts',(3.03942148984757,1.15421100750453,24.6258406640967));
#64302=CARTESIAN_POINT('Ctrl Pts',(0.682829595599215,3.17868365619569,24.7844021085055));
#64303=CARTESIAN_POINT('Ctrl Pts',(-2.29727252134343,2.30061404965549,24.9429635529143));
#64304=CARTESIAN_POINT('Ctrl Pts',(-3.17967279495086,-0.678208640346959,
25.101524997323));
#64305=CARTESIAN_POINT('Ctrl Pts',(-1.15862760390318,-3.03774062722042,
25.2600864417318));
#64306=CARTESIAN_POINT('Ctrl Pts',(1.92039187529098,-2.62342926112145,25.4186478861405));
#64307=CARTESIAN_POINT('Ctrl Pts',(3.24584945040241,0.186406513068115,25.5772093305493));
#64308=CARTESIAN_POINT('Ctrl Pts',(1.60743386199557,2.82602944466292,25.735770774958));
#64309=CARTESIAN_POINT('Ctrl Pts',(-1.49877318085119,2.88512824587626,25.8943322193668));
#64310=CARTESIAN_POINT('Ctrl Pts',(-3.23640978418636,0.309738198507568,
26.0528936637755));
#64311=CARTESIAN_POINT('Ctrl Pts',(-2.01879283923732,-2.54848219829688,
26.2114551081843));
#64312=CARTESIAN_POINT('Ctrl Pts',(1.04223859869649,-3.07961438270751,26.370016552593));
#64313=CARTESIAN_POINT('Ctrl Pts',(3.15157370571249,-0.798667152356616,
26.5285779970018));
#64314=CARTESIAN_POINT('Ctrl Pts',(2.38312138852957,2.21156471538246,26.6871394414106));
#64315=CARTESIAN_POINT('Ctrl Pts',(-0.561423700914708,3.20235686188205,
26.8457008858193));
#64316=CARTESIAN_POINT('Ctrl Pts',(-2.99331758273818,1.26899010699941,27.0042623302281));
#64317=CARTESIAN_POINT('Ctrl Pts',(-2.69193199829888,-1.82312593073724,
27.1628237746367));
#64318=CARTESIAN_POINT('Ctrl Pts',(0.0675297014036026,-3.25049623630303,
27.3213852190456));
#64319=CARTESIAN_POINT('Ctrl Pts',(2.7653281992882,-1.70975027211967,27.4799466634543));
#64320=CARTESIAN_POINT('Ctrl Pts',(2.93803052021534,1.39221503550097,27.6385081078631));
#64321=CARTESIAN_POINT('Ctrl Pts',(0.427937491104215,3.22291103608202,27.7970695522718));
#64322=CARTESIAN_POINT('Ctrl Pts',(-2.47291686718377,2.11067956137115,27.9556309966806));
#64323=CARTESIAN_POINT('Ctrl Pts',(-3.11568376631709,-0.928870664355431,
28.1141924410893));
#64324=CARTESIAN_POINT('Ctrl Pts',(-0.91343531828079,-3.12024389465136,
28.2727538854981));
#64325=CARTESIAN_POINT('Ctrl Pts',(2.12289569206488,-2.4624378009209,28.4313153299068));
#64326=CARTESIAN_POINT('Ctrl Pts',(3.22075307114599,0.443887032357858,28.5898767743156));
#64327=CARTESIAN_POINT('Ctrl Pts',(1.37765347124425,2.9448865777752,28.7484382187243));
#64328=CARTESIAN_POINT('Ctrl Pts',(-1.72341887645161,2.75683032105391,28.9069996631331));
#64329=CARTESIAN_POINT('Ctrl Pts',(-3.25079070738982,0.0514375304609387,
29.0655611075418));
#64330=CARTESIAN_POINT('Ctrl Pts',(-1.80977737904317,-2.70092426422798,
29.2241225519506));
#64331=CARTESIAN_POINT('Ctrl Pts',(1.28379275689769,-2.98699886175553,29.3826839963593));
#64332=CARTESIAN_POINT('Ctrl Pts',(3.20509690890129,-0.545563788519015,
29.541245440768));
#64333=CARTESIAN_POINT('Ctrl Pts',(2.19974014827687,2.39404037619475,29.6998068851769));
#64334=CARTESIAN_POINT('Ctrl Pts',(-0.814259000670061,3.14758134487732,
29.8583683295855));
#64335=CARTESIAN_POINT('Ctrl Pts',(-3.08473617266887,1.02698042231591,30.0169297739943));
#64336=CARTESIAN_POINT('Ctrl Pts',(-2.53845708458481,-2.03138417649469,
30.1754912184031));
#64337=CARTESIAN_POINT('Ctrl Pts',(0.325756012672393,-3.23483679078243,
30.3340526628118));
#64338=CARTESIAN_POINT('Ctrl Pts',(2.89251245996244,-1.48447219972415,30.4926141072206));
#64339=CARTESIAN_POINT('Ctrl Pts',(2.81803733252187,1.62140421712322,30.6511755516294));
#64340=CARTESIAN_POINT('Ctrl Pts',(0.170335889049024,3.24673246937499,30.8097369960381));
#64341=CARTESIAN_POINT('Ctrl Pts',(-2.63290387437695,1.9073812495363,30.9682984404469));
#64342=CARTESIAN_POINT('Ctrl Pts',(-3.03196770338867,-1.17365151914861,
31.1268598848556));
#64343=CARTESIAN_POINT('Ctrl Pts',(-0.66245959274568,-3.18299125521435,
31.2854213292644));
#64344=CARTESIAN_POINT('Ctrl Pts',(2.31195833853325,-2.28585535055883,31.4439827736731));
#64345=CARTESIAN_POINT('Ctrl Pts',(3.17526440850837,0.698557069144588,31.6025442180818));
#64346=CARTESIAN_POINT('Ctrl Pts',(1.13915043104843,3.04509808351621,31.7611056624906));
#64347=CARTESIAN_POINT('Ctrl Pts',(-1.93715269978589,2.61107745203088,31.9196671068993));
#64348=CARTESIAN_POINT('Ctrl Pts',(-3.24458916312253,-0.207188815672271,
32.0782285513081));
#64349=CARTESIAN_POINT('Ctrl Pts',(-1.58930326543629,-2.83626535663808,
32.2367899957168));
#64350=CARTESIAN_POINT('Ctrl Pts',(1.51721854725351,-2.87547107839077,32.3953514401256));
#64351=CARTESIAN_POINT('Ctrl Pts',(3.23832695611484,-0.289006173103491,
32.5539128845344));
#64352=CARTESIAN_POINT('Ctrl Pts',(2.00243119500863,2.5613581069519,32.7124743289431));
#64353=CARTESIAN_POINT('Ctrl Pts',(-1.06193879799461,3.07287683321437,32.8710357733519));
#64354=CARTESIAN_POINT('Ctrl Pts',(-3.15662367381384,0.778468383885889,
33.0295972177606));
#64355=CARTESIAN_POINT('Ctrl Pts',(-2.36890986260109,-2.22678065953139,
33.1881586621693));
#64356=CARTESIAN_POINT('Ctrl Pts',(0.581919791118306,-3.19869589043669,
33.3467201065781));
#64357=CARTESIAN_POINT('Ctrl Pts',(3.00138270137967,-1.24979515227539,33.5052815509869));
#64358=CARTESIAN_POINT('Ctrl Pts',(2.68020166681331,1.84032743499706,33.6638429953956));
#64359=CARTESIAN_POINT('Ctrl Pts',(-0.0883441991993578,3.24999713003858,
33.8224044398044));
#64360=CARTESIAN_POINT('Ctrl Pts',(-2.77622058094945,1.69200630279757,33.9809658842131));
#64361=CARTESIAN_POINT('Ctrl Pts',(-2.92905465663503,-1.41100136826097,
34.1395273286219));
#64362=CARTESIAN_POINT('Ctrl Pts',(-0.4072894867529,-3.22558542233326,34.2980887730306));
#64363=CARTESIAN_POINT('Ctrl Pts',(2.48638275954405,-2.09479994649826,34.4566502174393));
#64364=CARTESIAN_POINT('Ctrl Pts',(3.10967147515819,0.948804173347135,34.6152116618481));
#64365=CARTESIAN_POINT('Ctrl Pts',(0.893434829731745,3.12602947007818,34.7737731062569));
#64366=CARTESIAN_POINT('Ctrl Pts',(-2.13862138950371,2.44879247696718,34.9323345506656));
#64367=CARTESIAN_POINT('Ctrl Pts',(-3.21784441660045,-0.464503340348162,
35.0908959950743));
#64368=CARTESIAN_POINT('Ctrl Pts',(-1.35876643615622,-2.95364855978295,
35.2494574394831));
#64369=CARTESIAN_POINT('Ctrl Pts',(1.74103802828354,-2.7457371737902,35.4080188838919));
#64370=CARTESIAN_POINT('Ctrl Pts',(3.25105345024931,-0.0306187073285951,
35.5665803283006));
#64371=CARTESIAN_POINT('Ctrl Pts',(1.79244379593166,2.71245853078226,35.7251417727094));
#64372=CARTESIAN_POINT('Ctrl Pts',(-1.30289490234511,2.97871632092147,35.8837032171181));
#64373=CARTESIAN_POINT('Ctrl Pts',(-3.20852492730738,0.525027451435503,
36.0422646615269));
#64374=CARTESIAN_POINT('Ctrl Pts',(-2.18436382745606,-2.40807822025996,
36.2008261059356));
#64375=CARTESIAN_POINT('Ctrl Pts',(0.834399133536698,-3.14230236534719,
36.3593875503444));
#64376=CARTESIAN_POINT('Ctrl Pts',(3.0912496000529,-1.00720498796545,36.5179489947531));
#64377=CARTESIAN_POINT('Ctrl Pts',(2.52539624980007,2.04759855999854,36.6765104391619));
#64378=CARTESIAN_POINT('Ctrl Pts',(-0.346464965372859,3.23268436872066,
36.8350718835706));
#64379=CARTESIAN_POINT('Ctrl Pts',(-2.90195951315509,1.4659183333937,36.9936333279794));
#64380=CARTESIAN_POINT('Ctrl Pts',(-2.8075963376437,-1.63941734862674,37.1521947723881));
#64381=CARTESIAN_POINT('Ctrl Pts',(-0.149540397343195,-3.24775685532027,
37.3107562167969));
#64382=CARTESIAN_POINT('Ctrl Pts',(2.64506416393096,-1.89048098364498,37.4693176612057));
#64383=CARTESIAN_POINT('Ctrl Pts',(3.02439037266604,1.19304336942204,37.6278791056144));
#64384=CARTESIAN_POINT('Ctrl Pts',(0.642060899189524,3.187169328306,37.7864405500232));
#64385=CARTESIAN_POINT('Ctrl Pts',(-2.32654643543915,2.27100098025149,37.9450019944319));
#64386=CARTESIAN_POINT('Ctrl Pts',(-3.1707313472868,-0.7188731726267,38.1035634388407));
#64387=CARTESIAN_POINT('Ctrl Pts',(-1.11961596237772,-3.05233767503222,
38.2621248832494));
#64388=CARTESIAN_POINT('Ctrl Pts',(1.95381389621675,-2.59860517442575,38.4206863276582));
#64389=CARTESIAN_POINT('Ctrl Pts',(3.24323432642311,0.227937078525055,38.5792477720669));
#64390=CARTESIAN_POINT('Ctrl Pts',(1.57103400689371,2.8464336890225,38.7378092164756));
#64391=CARTESIAN_POINT('Ctrl Pts',(-1.5354614779569,2.86560299052469,38.8963706608845));
#64392=CARTESIAN_POINT('Ctrl Pts',(-3.24037889329957,0.268439772418473,
39.0549321052931));
#64393=CARTESIAN_POINT('Ctrl Pts',(-1.98547656045168,-2.5744679378351,39.213493549702));
#64394=CARTESIAN_POINT('Ctrl Pts',(1.08061773167372,-3.06536358105226,39.3720549941106));
#64395=CARTESIAN_POINT('Ctrl Pts',(3.16343569691019,-0.759503007488255,
39.5306164385195));
#64396=CARTESIAN_POINT('Ctrl Pts',(2.35076410763942,2.24454370995285,39.6891778829282));
#64397=CARTESIAN_POINT('Ctrl Pts',(0.388177431307865,2.87359516469282,39.794885512534));
#64398=CARTESIAN_POINT('Ctrl Pts',(-0.509883685250365,2.70426773226936,
39.8477393273369));
#64399=CARTESIAN_POINT('Ctrl Pts',(-1.28892185405299,2.64462557919729,-1.41553435639707E-14));
#64400=CARTESIAN_POINT('Ctrl Pts',(-2.1671763893535,2.21658711777033,0.0528538148029031));
#64401=CARTESIAN_POINT('Ctrl Pts',(-3.44873566164522,0.424356070443797,
0.158561444408738));
#64402=CARTESIAN_POINT('Ctrl Pts',(-2.22812647145566,-2.67063343433409,
0.317122888817489));
#64403=CARTESIAN_POINT('Ctrl Pts',(1.02996089584317,-3.31861020338198,0.475684333226241));
#64404=CARTESIAN_POINT('Ctrl Pts',(3.34606623809502,-0.940467179645626,
0.634245777634992));
#64405=CARTESIAN_POINT('Ctrl Pts',(2.60756871412969,2.29861656481967,0.792807222043744));
#64406=CARTESIAN_POINT('Ctrl Pts',(-0.51237942709981,3.43763407819966,0.951368666452495));
#64407=CARTESIAN_POINT('Ctrl Pts',(-3.16424575535823,1.43825034235358,1.10993011086125));
#64408=CARTESIAN_POINT('Ctrl Pts',(-2.92686575687285,-1.87475093929392,
1.26849155527));
#64409=CARTESIAN_POINT('Ctrl Pts',(-0.0168264060382829,-3.47570269831962,
1.42705299967875));
#64410=CARTESIAN_POINT('Ctrl Pts',(2.90854674895906,-1.9029817991733,1.5856144440875));
#64411=CARTESIAN_POINT('Ctrl Pts',(3.17806315019492,1.40744832765037,1.74417588849625));
#64412=CARTESIAN_POINT('Ctrl Pts',(0.545595424907332,3.43267566409904,1.90273733290501));
#64413=CARTESIAN_POINT('Ctrl Pts',(-2.5850658396409,2.32344609757596,2.06129877731376));
#64414=CARTESIAN_POINT('Ctrl Pts',(-3.35523570384725,-0.907391583655662,
2.21986022172251));
#64415=CARTESIAN_POINT('Ctrl Pts',(-1.06164763020298,-3.30966201013354,
2.37842166613126));
#64416=CARTESIAN_POINT('Ctrl Pts',(2.2013590481941,-2.68979207108213,2.53698311054001));
#64417=CARTESIAN_POINT('Ctrl Pts',(3.45424541186603,0.386200888946397,2.69554455494876));
#64418=CARTESIAN_POINT('Ctrl Pts',(1.55296643213827,3.1095428550715,2.85410599935752));
#64419=CARTESIAN_POINT('Ctrl Pts',(-1.76636822259782,2.99347716244134,3.01266744376627));
#64420=CARTESIAN_POINT('Ctrl Pts',(-3.47278419601471,0.143986152923845,
3.17122888817502));
#64421=CARTESIAN_POINT('Ctrl Pts',(-2.00810670974327,-2.83698244759632,
3.32979033258377));
#64422=CARTESIAN_POINT('Ctrl Pts',(1.29022746160673,-3.2274254705277,3.48835177699252));
#64423=CARTESIAN_POINT('Ctrl Pts',(3.41041995257781,-0.670818746338501,
3.64691322140127));
#64424=CARTESIAN_POINT('Ctrl Pts',(2.41646548755533,2.49833075822444,3.80547466581002));
#64425=CARTESIAN_POINT('Ctrl Pts',(-0.784029148963742,3.3861866957775,3.96403611021878));
#64426=CARTESIAN_POINT('Ctrl Pts',(-3.26860550698802,1.18202372220942,4.12259755462753));
#64427=CARTESIAN_POINT('Ctrl Pts',(-2.76852952853711,-2.10147716819809,
4.28115899903628));
#64428=CARTESIAN_POINT('Ctrl Pts',(0.25956584715683,-3.46606226313663,4.43972044344503));
#64429=CARTESIAN_POINT('Ctrl Pts',(3.05064460829658,-1.66569190247976,4.59828188785378));
#64430=CARTESIAN_POINT('Ctrl Pts',(3.05609704130031,1.65566690918397,4.75684333226253));
#64431=CARTESIAN_POINT('Ctrl Pts',(0.270944381832366,3.46519136300629,4.91540477667129));
#64432=CARTESIAN_POINT('Ctrl Pts',(-2.7616149409627,2.11055560410422,5.07396622108003));
#64433=CARTESIAN_POINT('Ctrl Pts',(-3.27246876367335,-1.17128571704109,
5.23252766548879));
#64434=CARTESIAN_POINT('Ctrl Pts',(-0.795142605983985,-3.3835942836501,
5.39108910989755));
#64435=CARTESIAN_POINT('Ctrl Pts',(2.40824983021483,-2.50625114373032,5.54965055430628));
#64436=CARTESIAN_POINT('Ctrl Pts',(3.41260403254196,0.659617887309973,5.70821199871505));
#64437=CARTESIAN_POINT('Ctrl Pts',(1.30081693986578,3.22317193601956,5.86677344312379));
#64438=CARTESIAN_POINT('Ctrl Pts',(-1.99878137992741,2.84356027462723,6.02533488753255));
#64439=CARTESIAN_POINT('Ctrl Pts',(-3.47323821296028,-0.132583393438264,
6.1838963319413));
#64440=CARTESIAN_POINT('Ctrl Pts',(-1.77618703639565,-2.98766156917474,
6.34245777635005));
#64441=CARTESIAN_POINT('Ctrl Pts',(1.54274869489151,-3.11462493802925,6.5010192207588));
#64442=CARTESIAN_POINT('Ctrl Pts',(3.45295875214133,-0.397539804540268,
6.65958066516755));
#64443=CARTESIAN_POINT('Ctrl Pts',(2.21017852546455,2.68254970611146,6.81814210957631));
#64444=CARTESIAN_POINT('Ctrl Pts',(-1.05077565484297,3.31313032695253,6.97670355398506));
#64445=CARTESIAN_POINT('Ctrl Pts',(-3.35223808673274,0.918401791179546,
7.13526499839381));
#64446=CARTESIAN_POINT('Ctrl Pts',(-2.5926810059155,-2.31494432800193,7.29382644280256));
#64447=CARTESIAN_POINT('Ctrl Pts',(0.53432341724346,-3.43445199791299,7.45238788721131));
#64448=CARTESIAN_POINT('Ctrl Pts',(3.17342263678587,-1.41786840310318,7.61094933162007));
#64449=CARTESIAN_POINT('Ctrl Pts',(2.91478358060356,1.89340928444624,7.76951077602881));
#64450=CARTESIAN_POINT('Ctrl Pts',(-0.00542341457961224,3.47576360340539,
7.92807222043756));
#64451=CARTESIAN_POINT('Ctrl Pts',(-2.92067814282227,1.88430391026066,8.08663366484632));
#64452=CARTESIAN_POINT('Ctrl Pts',(-3.16898244743632,-1.42776478735954,
8.24519510925507));
#64453=CARTESIAN_POINT('Ctrl Pts',(-0.523602933642665,-3.43610273537683,
8.40375655366383));
#64454=CARTESIAN_POINT('Ctrl Pts',(2.59989261944251,-2.30684208552552,8.56231799807257));
#64455=CARTESIAN_POINT('Ctrl Pts',(3.34935571028899,0.928858636250884,8.72087944248133));
#64456=CARTESIAN_POINT('Ctrl Pts',(1.04043126453191,3.31639334578512,8.87944088689007));
#64457=CARTESIAN_POINT('Ctrl Pts',(-2.21853918630074,2.67563934771326,9.03800233129883));
#64458=CARTESIAN_POINT('Ctrl Pts',(-3.45170133734449,-0.408313504500715,
9.19656377570758));
#64459=CARTESIAN_POINT('Ctrl Pts',(-1.53302138401484,-3.11942422192565,
9.35512522011632));
#64460=CARTESIAN_POINT('Ctrl Pts',(1.78550197197721,-2.98210408072033,9.51368666452509));
#64461=CARTESIAN_POINT('Ctrl Pts',(3.47363505293783,-0.121743826064997,
9.67224810893383));
#64462=CARTESIAN_POINT('Ctrl Pts',(1.98989775895469,2.84978401797231,9.83080955334259));
#64463=CARTESIAN_POINT('Ctrl Pts',(-1.31086914654657,3.21909678649394,9.98937099775133));
#64464=CARTESIAN_POINT('Ctrl Pts',(-3.41464588238613,0.6489649744684,10.1479324421601));
#64465=CARTESIAN_POINT('Ctrl Pts',(-2.40041685475204,-2.51375435625792,
10.3064938865688));
#64466=CARTESIAN_POINT('Ctrl Pts',(0.805697904419769,-3.38109640900654,
10.4650553309776));
#64467=CARTESIAN_POINT('Ctrl Pts',(3.2761080558142,-1.1610676323163,10.6236167753863));
#64468=CARTESIAN_POINT('Ctrl Pts',(2.75501509044826,2.1191634886402,10.7821782197951));
#64469=CARTESIAN_POINT('Ctrl Pts',(-0.281756872492634,3.46432895449993,
10.9407396642038));
#64470=CARTESIAN_POINT('Ctrl Pts',(-3.06124899366075,1.64612169628929,11.0993011086126));
#64471=CARTESIAN_POINT('Ctrl Pts',(-3.04543163489178,-1.67520392710372,
11.2578625530213));
#64472=CARTESIAN_POINT('Ctrl Pts',(-0.248748055458642,-3.46685541162145,
11.4164239974301));
#64473=CARTESIAN_POINT('Ctrl Pts',(2.77507411968471,-2.09282719555137,11.5749854418389));
#64474=CARTESIAN_POINT('Ctrl Pts',(3.26490085363842,1.19221829213213,11.7335468862476));
#64475=CARTESIAN_POINT('Ctrl Pts',(0.773458071087839,3.38861692323762,11.8921083306564));
#64476=CARTESIAN_POINT('Ctrl Pts',(-2.42425025305144,2.49077753939675,12.0506697750651));
#64477=CARTESIAN_POINT('Ctrl Pts',(-3.40830992328265,-0.681458367793936,
12.2092312194739));
#64478=CARTESIAN_POINT('Ctrl Pts',(-1.2801493661345,-3.23143615758826,12.3677926638826));
#64479=CARTESIAN_POINT('Ctrl Pts',(2.01695029603303,-2.83070195243435,12.5263541082914));
#64480=CARTESIAN_POINT('Ctrl Pts',(3.47231794138706,0.154822976669773,12.6849155527001));
#64481=CARTESIAN_POINT('Ctrl Pts',(1.75701790207559,2.99897484683836,12.8434769971089));
#64482=CARTESIAN_POINT('Ctrl Pts',(-1.56266283552656,3.10468144946425,13.0020384415176));
#64483=CARTESIAN_POINT('Ctrl Pts',(-3.45543375718812,0.375419218831596,
13.1605998859264));
#64484=CARTESIAN_POINT('Ctrl Pts',(-2.19295440069049,-2.69664848222298,
13.3191613303351));
#64485=CARTESIAN_POINT('Ctrl Pts',(1.07197109397293,-3.30633331862803,13.4777227747439));
#64486=CARTESIAN_POINT('Ctrl Pts',(3.35805070990966,-0.896915531061065,
13.6362842191526));
#64487=CARTESIAN_POINT('Ctrl Pts',(2.57780314927297,2.33150015307347,13.7948456635614));
#64488=CARTESIAN_POINT('Ctrl Pts',(-0.556306379304298,3.43095981505594,
13.9534071079701));
#64489=CARTESIAN_POINT('Ctrl Pts',(-3.18243746540957,1.39751701919542,14.1119685523789));
#64490=CARTESIAN_POINT('Ctrl Pts',(-2.90259859128356,-1.91203646881067,
14.2705299967876));
#64491=CARTESIAN_POINT('Ctrl Pts',(0.0276817776273479,-3.47565760099736,
14.4290914411964));
#64492=CARTESIAN_POINT('Ctrl Pts',(2.93268516463204,-1.86556151475381,14.5876528856051));
#64493=CARTESIAN_POINT('Ctrl Pts',(3.15977419075238,1.44802938631728,14.7462143300139));
#64494=CARTESIAN_POINT('Ctrl Pts',(0.501587707379338,3.43938538288301,14.9047757744226));
#64495=CARTESIAN_POINT('Ctrl Pts',(-2.61461211511146,2.29014530711388,15.0633372188314));
#64496=CARTESIAN_POINT('Ctrl Pts',(-3.34333870466228,-0.950288559381016,
15.2218986632402));
#64497=CARTESIAN_POINT('Ctrl Pts',(-1.01917204863389,-3.32298816962486,
15.3804601076489));
#64498=CARTESIAN_POINT('Ctrl Pts',(2.23562824586454,-2.66137715975695,15.5390215520576));
#64499=CARTESIAN_POINT('Ctrl Pts',(3.44901575681568,0.430409513626772,15.6975829964664));
#64500=CARTESIAN_POINT('Ctrl Pts',(1.51301343980967,3.12917758702485,15.8561444408751));
#64501=CARTESIAN_POINT('Ctrl Pts',(-1.8045624833716,2.97060873960054,16.0147058852839));
#64502=CARTESIAN_POINT('Ctrl Pts',(-3.47434346162898,0.099496486466701,
16.1732673296926));
#64503=CARTESIAN_POINT('Ctrl Pts',(-1.97160719775406,-2.86246870689406,
16.3318287741014));
#64504=CARTESIAN_POINT('Ctrl Pts',(1.33145707015024,-3.21063609126451,16.4903902185102));
#64505=CARTESIAN_POINT('Ctrl Pts',(3.41873177698731,-0.627084585363457,
16.6489516629189));
#64506=CARTESIAN_POINT('Ctrl Pts',(2.38426977917728,2.52907486253082,16.8075131073277));
#64507=CARTESIAN_POINT('Ctrl Pts',(-0.827333617539956,3.37586746266372,
16.9660745517364));
#64508=CARTESIAN_POINT('Ctrl Pts',(-3.28347625004977,1.14006392607712,17.1246359961451));
#64509=CARTESIAN_POINT('Ctrl Pts',(-2.74138766781067,-2.13676290096935,
17.2831974405539));
#64510=CARTESIAN_POINT('Ctrl Pts',(0.303936342805055,-3.4624535722094,17.4417588849627));
#64511=CARTESIAN_POINT('Ctrl Pts',(3.07172783577854,-1.62648398181063,17.6003203293714));
#64512=CARTESIAN_POINT('Ctrl Pts',(3.03464133388157,1.69467224408758,17.7588817737802));
#64513=CARTESIAN_POINT('Ctrl Pts',(0.226541527815518,3.46837728287428,17.9174432181889));
#64514=CARTESIAN_POINT('Ctrl Pts',(-2.78841949130883,2.07501295915769,18.0760046625977));
#64515=CARTESIAN_POINT('Ctrl Pts',(-3.25719904847505,-1.21310197378316,
18.2345661070064));
#64516=CARTESIAN_POINT('Ctrl Pts',(-0.751741816311538,-3.3935005940462,
18.3931275514152));
#64517=CARTESIAN_POINT('Ctrl Pts',(2.44015125624008,-2.47520178709804,18.5516889958239));
#64518=CARTESIAN_POINT('Ctrl Pts',(3.40387603762256,0.703270901347592,18.7102504402327));
#64519=CARTESIAN_POINT('Ctrl Pts',(1.25942929287289,3.23956785643348,18.8688118846414));
#64520=CARTESIAN_POINT('Ctrl Pts',(-2.03503649605394,2.8177275418166,19.0273733290502));
#64521=CARTESIAN_POINT('Ctrl Pts',(-3.4712552684142,-0.177056210537707,
19.1859347734589));
#64522=CARTESIAN_POINT('Ctrl Pts',(-1.73777671162116,-3.01016513512639,
19.3444962178677));
#64523=CARTESIAN_POINT('Ctrl Pts',(1.58251289062026,-3.0946106364459,19.5030576622764));
#64524=CARTESIAN_POINT('Ctrl Pts',(3.45776705326368,-0.353283237003404,
19.6616191066852));
#64525=CARTESIAN_POINT('Ctrl Pts',(2.17564034182019,2.71063666750596,19.8201805510939));
#64526=CARTESIAN_POINT('Ctrl Pts',(-1.09312257106175,3.29940071601172,19.9787419955027));
#64527=CARTESIAN_POINT('Ctrl Pts',(-3.36372561784012,0.875392488012878,
20.1373034399114));
#64528=CARTESIAN_POINT('Ctrl Pts',(-2.5628195757052,-2.34796036222197,20.2958648843202));
#64529=CARTESIAN_POINT('Ctrl Pts',(0.578266526977567,-3.42732692691558,
20.4544263287289));
#64530=CARTESIAN_POINT('Ctrl Pts',(3.19132178076895,-1.37710832245438,20.6129877731377));
#64531=CARTESIAN_POINT('Ctrl Pts',(2.89029456502375,1.93058523965599,20.7715492175465));
#64532=CARTESIAN_POINT('Ctrl Pts',(-0.0499390054322844,3.4754090602287,
20.9301106619552));
#64533=CARTESIAN_POINT('Ctrl Pts',(-2.94457191563734,1.84674261168771,21.088672106364));
#64534=CARTESIAN_POINT('Ctrl Pts',(-3.15043635023577,-1.46823460090559,
21.2472335507727));
#64535=CARTESIAN_POINT('Ctrl Pts',(-0.479551910767174,-3.44252697956934,
21.4057949951815));
#64536=CARTESIAN_POINT('Ctrl Pts',(2.62922438430201,-2.27335460876106,21.5643564395902));
#64537=CARTESIAN_POINT('Ctrl Pts',(3.33718458713544,0.971679510728251,21.722917883999));
#64538=CARTESIAN_POINT('Ctrl Pts',(0.997871036008576,3.32944671614946,21.8814793284077));
#64539=CARTESIAN_POINT('Ctrl Pts',(-2.2526256212575,2.64700582746574,22.0400407728164));
#64540=CARTESIAN_POINT('Ctrl Pts',(-3.44618873052089,-0.452487871455233,
22.1986022172252));
#64541=CARTESIAN_POINT('Ctrl Pts',(-1.49294344620842,-3.13880262307247,
22.3571636616339));
#64542=CARTESIAN_POINT('Ctrl Pts',(1.82354898880575,-2.95899157241263,22.5157251060427));
#64543=CARTESIAN_POINT('Ctrl Pts',(3.47490938585301,-0.0772450664705207,
22.6742865504514));
#64544=CARTESIAN_POINT('Ctrl Pts',(1.95323578001058,2.87503600462147,22.8328479948602));
#64545=CARTESIAN_POINT('Ctrl Pts',(-1.35199039007024,3.20204372633183,22.991409439269));
#64546=CARTESIAN_POINT('Ctrl Pts',(-3.42267746778281,0.605178479223403,
23.1499708836777));
#64547=CARTESIAN_POINT('Ctrl Pts',(-2.36802492357223,-2.54429165024845,
23.3085323280865));
#64548=CARTESIAN_POINT('Ctrl Pts',(0.848935401317481,-3.37050007040103,
23.4670937724952));
#64549=CARTESIAN_POINT('Ctrl Pts',(3.29070978737274,-1.11901346527762,23.625655216904));
#64550=CARTESIAN_POINT('Ctrl Pts',(2.72764781956938,2.1542746836422,23.7842166613127));
#64551=CARTESIAN_POINT('Ctrl Pts',(-0.326103348544396,3.46043619306171,
23.9427781057215));
#64552=CARTESIAN_POINT('Ctrl Pts',(-3.08208070488623,1.60677956445533,24.1013395501302));
#64553=CARTESIAN_POINT('Ctrl Pts',(-3.02372658079627,-1.71407106176184,
24.259900994539));
#64554=CARTESIAN_POINT('Ctrl Pts',(-0.204325709597339,-3.46975691433578,
24.4184624389477));
#64555=CARTESIAN_POINT('Ctrl Pts',(2.80165050853192,-2.05711362550206,24.5770238833565));
#64556=CARTESIAN_POINT('Ctrl Pts',(3.24936366403954,1.23393590554894,24.7355853277652));
#64557=CARTESIAN_POINT('Ctrl Pts',(0.729994732248181,3.39824509579182,24.894146772174));
#64558=CARTESIAN_POINT('Ctrl Pts',(-2.45595218767254,2.45952452560444,25.0527082165827));
#64559=CARTESIAN_POINT('Ctrl Pts',(-3.39930255739772,-0.725054593429181,
25.2112696609915));
#64560=CARTESIAN_POINT('Ctrl Pts',(-1.23865756982089,-3.24756669907006,
25.3698311054002));
#64561=CARTESIAN_POINT('Ctrl Pts',(2.05303923826652,-2.80463757486085,25.528392549809));
#64562=CARTESIAN_POINT('Ctrl Pts',(3.47005023762246,0.199282183246816,25.6869539942178));
#64563=CARTESIAN_POINT('Ctrl Pts',(1.71846425412255,3.0212319751198,25.8455154386265));
#64564=CARTESIAN_POINT('Ctrl Pts',(-1.6022980461125,3.08441291198299,26.0040768830352));
#64565=CARTESIAN_POINT('Ctrl Pts',(-3.45995854467842,0.331132766862739,
26.162638327444));
#64566=CARTESIAN_POINT('Ctrl Pts',(-2.15823705891142,-2.7245136882983,26.3211997718528));
#64567=CARTESIAN_POINT('Ctrl Pts',(1.11422921867739,-3.29233280341293,26.4797612162615));
#64568=CARTESIAN_POINT('Ctrl Pts',(3.3692625777935,-0.853833544705057,26.6383226606703));
#64569=CARTESIAN_POINT('Ctrl Pts',(2.54773089969555,2.36432428040652,26.796884105079));
#64570=CARTESIAN_POINT('Ctrl Pts',(-0.600202959667374,3.42355348247838,
26.9554455494878));
#64571=CARTESIAN_POINT('Ctrl Pts',(-3.20007521851407,1.35664314985023,27.1140069938965));
#64572=CARTESIAN_POINT('Ctrl Pts',(-2.87787200641801,-1.94905483628834,
27.2725684383053));
#64573=CARTESIAN_POINT('Ctrl Pts',(0.072194185215024,-3.47501799129219,
27.431129882714));
#64574=CARTESIAN_POINT('Ctrl Pts',(2.95633790835697,-1.8278479728344,27.5896913271228));
#64575=CARTESIAN_POINT('Ctrl Pts',(3.1409693088357,1.48837960249914,27.7482527715315));
#64576=CARTESIAN_POINT('Ctrl Pts',(0.457496447504475,3.44552739659752,27.9068142159403));
#64577=CARTESIAN_POINT('Ctrl Pts',(-2.64372882775816,2.25647067906141,28.065375660349));
#64578=CARTESIAN_POINT('Ctrl Pts',(-3.33089361009169,-0.993030613039605,
28.2239371047578));
#64579=CARTESIAN_POINT('Ctrl Pts',(-0.976529100220519,-3.33576872049095,
28.3824985491665));
#64580=CARTESIAN_POINT('Ctrl Pts',(2.26953061540928,-2.63252594021469,28.5410599935753));
#64581=CARTESIAN_POINT('Ctrl Pts',(3.44322037439778,0.474547672542312,28.699621437984));
#64582=CARTESIAN_POINT('Ctrl Pts',(1.4728122262909,3.14829893534133,28.8581828823928));
#64583=CARTESIAN_POINT('Ctrl Pts',(-1.84246070963419,2.94725305558204,29.0167443268015));
#64584=CARTESIAN_POINT('Ctrl Pts',(-3.47533280240106,0.0549904786176304,
29.1753057712103));
#64585=CARTESIAN_POINT('Ctrl Pts',(-1.93478425914477,-2.88748539576375,
29.333867215619));
#64586=CARTESIAN_POINT('Ctrl Pts',(1.3724682642255,-3.1933200440728,29.4924286600278));
#64587=CARTESIAN_POINT('Ctrl Pts',(3.42648279295799,-0.583247554427895,
29.6509901044365));
#64588=CARTESIAN_POINT('Ctrl Pts',(2.35168295414604,2.55940409536327,29.8095515488453));
#64589=CARTESIAN_POINT('Ctrl Pts',(-0.870502369853091,3.36499445233771,
29.968112993254));
#64590=CARTESIAN_POINT('Ctrl Pts',(-3.29780837113232,1.0979171132071,30.1266744376629));
#64591=CARTESIAN_POINT('Ctrl Pts',(-2.71379610920208,-2.17169811849229,
30.2852358820715));
#64592=CARTESIAN_POINT('Ctrl Pts',(0.348256980631351,-3.45827689979053,
30.4437973264803));
#64593=CARTESIAN_POINT('Ctrl Pts',(3.09230717640782,-1.58700925231077,30.602358770889));
#64594=CARTESIAN_POINT('Ctrl Pts',(3.01268782325502,1.73339958457198,30.7609202152978));
#64595=CARTESIAN_POINT('Ctrl Pts',(0.182101511885165,3.4709942494266,30.9194816597066));
#64596=CARTESIAN_POINT('Ctrl Pts',(-2.81476662874377,2.0391299286445,31.0780431041153));
#64597=CARTESIAN_POINT('Ctrl Pts',(-3.24139502166468,-1.25471923302017,
31.2366045485241));
#64598=CARTESIAN_POINT('Ctrl Pts',(-0.708217710755854,-3.40285023390025,
31.3951659929327));
#64599=CARTESIAN_POINT('Ctrl Pts',(2.4716523993453,-2.44374639784777,31.5537274373416));
#64600=CARTESIAN_POINT('Ctrl Pts',(3.39458967016864,0.746808550679325,31.7122888817503));
#64601=CARTESIAN_POINT('Ctrl Pts',(1.2178350488366,3.25543235746169,31.8708503261591));
#64602=CARTESIAN_POINT('Ctrl Pts',(-2.07095778436978,2.79143258839283,32.0294117705678));
#64603=CARTESIAN_POINT('Ctrl Pts',(-3.46870289843071,-0.221499983299419,
32.1879732149766));
#64604=CARTESIAN_POINT('Ctrl Pts',(-1.69908132159284,-3.03217491296225,
32.3465346593853));
#64605=CARTESIAN_POINT('Ctrl Pts',(1.62201749060475,-3.07408869428902,32.5050961037941));
#64606=CARTESIAN_POINT('Ctrl Pts',(3.46200814155826,-0.308968716810793,
32.6636575482028));
#64607=CARTESIAN_POINT('Ctrl Pts',(2.14074526568096,2.73827897549683,32.8222189926116));
#64608=CARTESIAN_POINT('Ctrl Pts',(-1.13529017122625,3.2851298706901,32.9807804370203));
#64609=CARTESIAN_POINT('Ctrl Pts',(-3.37466136269644,0.832239585280099,
33.139341881429));
#64610=CARTESIAN_POINT('Ctrl Pts',(-2.53253774003776,-2.38059123653509,
33.2979033258378));
#64611=CARTESIAN_POINT('Ctrl Pts',(0.622114777750159,-3.41963963649505,
33.4564647702466));
#64612=CARTESIAN_POINT('Ctrl Pts',(3.20869741966233,-1.33612234066947,33.6150262146553));
#64613=CARTESIAN_POINT('Ctrl Pts',(2.86533142492128,1.9674445012609,33.7735876590641));
#64614=CARTESIAN_POINT('Ctrl Pts',(-0.0944464042799534,3.47448441022565,
33.9321491034729));
#64615=CARTESIAN_POINT('Ctrl Pts',(-2.96798266026227,1.80887837307219,34.0907105478815));
#64616=CARTESIAN_POINT('Ctrl Pts',(-3.13137345479944,-1.50846356494225,
34.2492719922904));
#64617=CARTESIAN_POINT('Ctrl Pts',(-0.435422222097375,-3.44838651091826,
34.407833436699));
#64618=CARTESIAN_POINT('Ctrl Pts',(2.65812485064789,-2.23949421043432,34.5663948811079));
#64619=CARTESIAN_POINT('Ctrl Pts',(3.32446603152299,1.01434099069891,34.7249563255165));
#64620=CARTESIAN_POINT('Ctrl Pts',(0.95514711652021,3.34195392337585,34.8835177699254));
#64621=CARTESIAN_POINT('Ctrl Pts',(-2.28634253505258,2.61793809184046,35.042079214334));
#64622=CARTESIAN_POINT('Ctrl Pts',(-3.44011081015237,-0.496588012223433,
35.2006406587429));
#64623=CARTESIAN_POINT('Ctrl Pts',(-1.45262060570077,-3.15766613434814,
35.3592021031516));
#64624=CARTESIAN_POINT('Ctrl Pts',(1.86129687037896,-2.9353936705777,35.5177635475603));
#64625=CARTESIAN_POINT('Ctrl Pts',(3.47561369371654,-0.0327336354518328,
35.6763249919691));
#64626=CARTESIAN_POINT('Ctrl Pts',(1.91625339222871,2.89981636952241,35.8348864363779));
#64627=CARTESIAN_POINT('Ctrl Pts',(-1.39288985350799,3.18446540271358,35.9934478807866));
#64628=CARTESIAN_POINT('Ctrl Pts',(-3.43014759512038,0.561292709489631,
36.1520093251954));
#64629=CARTESIAN_POINT('Ctrl Pts',(-2.33524454363645,-2.57441157641824,
36.3105707696041));
#64630=CARTESIAN_POINT('Ctrl Pts',(0.892033643532763,-3.35935083748346,
36.4691322140128));
#64631=CARTESIAN_POINT('Ctrl Pts',(3.30477170094384,-1.07677572888985,36.6276936584217));
#64632=CARTESIAN_POINT('Ctrl Pts',(2.69983312245829,2.18903247924752,36.7862551028303));
#64633=CARTESIAN_POINT('Ctrl Pts',(-0.370396364277214,3.4559758033284,36.9448165472391));
#64634=CARTESIAN_POINT('Ctrl Pts',(-3.10240676656962,1.56717381346724,37.1033779916479));
#64635=CARTESIAN_POINT('Ctrl Pts',(-3.0015256368038,-1.75265693837389,37.2619394360566));
#64636=CARTESIAN_POINT('Ctrl Pts',(-0.159869611719143,-3.47208939285428,
37.4205008804654));
#64637=CARTESIAN_POINT('Ctrl Pts',(2.82776686683283,-2.02106230949944,37.5790623248741));
#64638=CARTESIAN_POINT('Ctrl Pts',(3.23329430144447,1.27545053793049,37.7376237692828));
#64639=CARTESIAN_POINT('Ctrl Pts',(0.686410016805987,3.40731689932821,37.8961852136916));
#64640=CARTESIAN_POINT('Ctrl Pts',(-2.4872481408941,2.42786599057616,38.0547466581004));
#64641=CARTESIAN_POINT('Ctrl Pts',(-3.38974349649071,-0.768527949805165,
38.2133081025091));
#64642=CARTESIAN_POINT('Ctrl Pts',(-1.19695127443843,-3.26317200979131,
38.3718695469179));
#64643=CARTESIAN_POINT('Ctrl Pts',(2.08876982079273,-2.77809881228007,38.5304309913266));
#64644=CARTESIAN_POINT('Ctrl Pts',(3.46725447900073,0.243681392370514,38.6889924357354));
#64645=CARTESIAN_POINT('Ctrl Pts',(1.6795501492709,3.04304560328413,38.8475538801441));
#64646=CARTESIAN_POINT('Ctrl Pts',(-1.6415205165428,3.0635389872962,39.0061153245529));
#64647=CARTESIAN_POINT('Ctrl Pts',(-3.46420181234437,0.28698173168576,39.1646767689616));
#64648=CARTESIAN_POINT('Ctrl Pts',(-2.12261952245961,-2.75229434265003,
39.3232382133705));
#64649=CARTESIAN_POINT('Ctrl Pts',(1.15525931620421,-3.27709765513333,39.481799657779));
#64650=CARTESIAN_POINT('Ctrl Pts',(3.3819439131429,-0.81196421210558,39.640361102188));
#64651=CARTESIAN_POINT('Ctrl Pts',(2.51313860206826,2.39958123538677,39.7989225465966));
#64652=CARTESIAN_POINT('Ctrl Pts',(0.414990038303313,3.07208320547242,39.9046301762025));
#64653=CARTESIAN_POINT('Ctrl Pts',(-0.545102916878579,2.89105980740808,
39.9574839910054));
#64654=CARTESIAN_POINT('Ctrl Pts',(-2.9422704459833,-0.00265502083472174,
38.1778238829104));
#64655=CARTESIAN_POINT('Ctrl Pts',(-2.94427742279841,-0.221182694545831,
38.18965195611));
#64656=CARTESIAN_POINT('Ctrl Pts',(-2.9219878224732,-0.439304875887155,
38.2014800293096));
#64657=CARTESIAN_POINT('Ctrl Pts',(-2.87386223354923,-0.651569636405941,
38.2133081025091));
#64658=CARTESIAN_POINT('Ctrl Pts',(-2.65881275580662,-1.60007596980054,
38.266161917312));
#64659=CARTESIAN_POINT('Ctrl Pts',(-1.92788201512251,-2.43162398979594,
38.319015732115));
#64660=CARTESIAN_POINT('Ctrl Pts',(-1.01479646224192,-2.76655246687509,
38.3718695469179));
#64661=CARTESIAN_POINT('Ctrl Pts',(-0.101710909361328,-3.10148094395424,
38.4247233617208));
#64662=CARTESIAN_POINT('Ctrl Pts',(0.993529455715749,-2.93978987811714,
38.4775771765237));
#64663=CARTESIAN_POINT('Ctrl Pts',(1.77089708128894,-2.35531431109013,38.5304309913266));
#64664=CARTESIAN_POINT('Ctrl Pts',(2.54826470686207,-1.77083874406317,38.5832848061296));
#64665=CARTESIAN_POINT('Ctrl Pts',(3.00775959293139,-0.763578675846303,
38.6361386209325));
#64666=CARTESIAN_POINT('Ctrl Pts',(2.93955631434443,0.206612060081017,38.6889924357354));
#64667=CARTESIAN_POINT('Ctrl Pts',(2.87135303575745,1.17680279600839,38.7418462505383));
#64668=CARTESIAN_POINT('Ctrl Pts',(2.27545159251423,2.10992419964619,38.7947000653412));
#64669=CARTESIAN_POINT('Ctrl Pts',(1.42398909325699,2.57990046546716,38.8475538801441));
#64670=CARTESIAN_POINT('Ctrl Pts',(0.572526593999702,3.04987673128816,38.900407694947));
#64671=CARTESIAN_POINT('Ctrl Pts',(-0.534496961271609,3.05670785929219,
38.95326150975));
#64672=CARTESIAN_POINT('Ctrl Pts',(-1.39178895487418,2.59736388069241,39.0061153245529));
#64673=CARTESIAN_POINT('Ctrl Pts',(-1.67231312023668,2.44705676576241,39.0234102163686));
#64674=CARTESIAN_POINT('Ctrl Pts',(-1.92609759023508,2.24683453296096,39.0407051081843));
#64675=CARTESIAN_POINT('Ctrl Pts',(-2.14341454569378,2.01149633185929,39.058));
#64676=CARTESIAN_POINT('Ctrl Pts',(-1.3799850048903,-1.93364773575773,1.50920942409982E-16));
#64677=CARTESIAN_POINT('Ctrl Pts',(-1.43331552021448,-1.9046528475011,1.23773392155628E-16));
#64678=CARTESIAN_POINT('Ctrl Pts',(-1.48535269583483,-1.87353821396734,
3.98761059851725E-16));
#64679=CARTESIAN_POINT('Ctrl Pts',(-1.53595409369946,-1.84033239929008,
4.04190569902596E-16));
#64680=CARTESIAN_POINT('Ctrl Pts',(-1.604148816696,-1.79558143529797,4.20181454187173E-16));
#64681=CARTESIAN_POINT('Ctrl Pts',(-1.66973713239356,-1.74703457128715,
1.05440529867363E-16));
#64682=CARTESIAN_POINT('Ctrl Pts',(-1.73263418143615,-1.69505071632867,
1.6306400674182E-16));
#64683=CARTESIAN_POINT('Ctrl Pts',(-1.76925523715114,-1.66478373754839,
1.96614588036684E-16));
#64684=CARTESIAN_POINT('Ctrl Pts',(-1.80496365153929,-1.63335064415344,
2.27902642928896E-16));
#64685=CARTESIAN_POINT('Ctrl Pts',(-1.83973953560591,-1.60081498486991,
2.22044604925031E-16));
#64686=CARTESIAN_POINT('Ctrl Pts',(-1.85332304959686,-1.5881065061369,2.19756446239185E-16));
#64687=CARTESIAN_POINT('Ctrl Pts',(-1.86676425940608,-1.57522975614015,
8.38314136196732E-16));
#64688=CARTESIAN_POINT('Ctrl Pts',(-1.88006186427144,-1.56218832508201,
8.74300631892311E-16));
#64689=CARTESIAN_POINT('Ctrl Pts',(-1.89032248524922,-1.55212537145611,
9.02068323622498E-16));
#64690=CARTESIAN_POINT('Ctrl Pts',(-1.90049621943027,-1.541965647287,6.20660402139477E-16));
#64691=CARTESIAN_POINT('Ctrl Pts',(-1.91057614643099,-1.53171754005162,
5.96744875736022E-16));
#64692=CARTESIAN_POINT('Ctrl Pts',(-1.97048681206202,-1.47080728485966,
4.54601474732619E-16));
#64693=CARTESIAN_POINT('Ctrl Pts',(-2.02715048831372,-1.40671555173584,
3.98298047110711E-16));
#64694=CARTESIAN_POINT('Ctrl Pts',(-2.08047392334861,-1.33983470059731,
4.44089209850063E-16));
#64695=CARTESIAN_POINT('Ctrl Pts',(-2.12704705061845,-1.28142041445932,
4.8408358846985E-16));
#64696=CARTESIAN_POINT('Ctrl Pts',(-2.17107203351392,-1.22087734268402,
2.12674681454476E-16));
#64697=CARTESIAN_POINT('Ctrl Pts',(-2.21247079422441,-1.15843840004056,
1.11022302462516E-16));
#64698=CARTESIAN_POINT('Ctrl Pts',(-2.23235211616136,-1.1284527507411,6.2204810399683E-17));
#64699=CARTESIAN_POINT('Ctrl Pts',(-2.25162750605615,-1.09802950060355,
6.56803286684185E-16));
#64700=CARTESIAN_POINT('Ctrl Pts',(-2.27028681415291,-1.06719266209682,
6.80011602582908E-16));
#64701=CARTESIAN_POINT('Ctrl Pts',(-2.28194103140091,-1.04793261165253,
6.94507035856293E-16));
#64702=CARTESIAN_POINT('Ctrl Pts',(-2.29335807228086,-1.02850535079581,
4.25198681390034E-16));
#64703=CARTESIAN_POINT('Ctrl Pts',(-2.30451762944014,-1.00894825067258,
4.02455846426619E-16));
#64704=CARTESIAN_POINT('Ctrl Pts',(-2.34844909879478,-0.931958444314987,
3.1292486029765E-16));
#64705=CARTESIAN_POINT('Ctrl Pts',(-2.38843712460482,-0.852891211717048,
-9.72483045965204E-17));
#64706=CARTESIAN_POINT('Ctrl Pts',(-2.42438430062746,-0.772143474284519,
-1.11022302462516E-16));
#64707=CARTESIAN_POINT('Ctrl Pts',(-2.46273528155508,-0.685996096914061,
-1.25717374173389E-16));
#64708=CARTESIAN_POINT('Ctrl Pts',(-2.49648798427418,-0.597935475902931,
5.41089475014295E-17));
#64709=CARTESIAN_POINT('Ctrl Pts',(-2.52548424257669,-0.50839454562273,
9.71445146547012E-17));
#64710=CARTESIAN_POINT('Ctrl Pts',(-2.54723143630358,-0.441238847912579,
1.29421190019655E-16));
#64711=CARTESIAN_POINT('Ctrl Pts',(-2.56630236075426,-0.373249325614532,
2.04320780950305E-16));
#64712=CARTESIAN_POINT('Ctrl Pts',(-2.58261145214044,-0.304595415567763,
1.66533453693773E-16));
#64713=CARTESIAN_POINT('Ctrl Pts',(-2.59484327068007,-0.253104983032686,
1.38192958251375E-16));
#64714=CARTESIAN_POINT('Ctrl Pts',(-2.60552123925938,-0.201240582374946,
1.5471389960288E-16));
#64715=CARTESIAN_POINT('Ctrl Pts',(-2.61460229316052,-0.149071024239955,
1.11022302462516E-16));
#64716=CARTESIAN_POINT('Ctrl Pts',(-2.61710931909131,-0.134668462988168,
9.89602699957222E-17));
#64717=CARTESIAN_POINT('Ctrl Pts',(-2.61949459731049,-0.12024263420335,
1.16564317379691E-16));
#64718=CARTESIAN_POINT('Ctrl Pts',(-2.62175713377957,-0.105794966493652,
1.11022302462516E-16));
#64719=CARTESIAN_POINT('Ctrl Pts',(-2.62409044163309,-0.090895380567459,
1.05306935171277E-16));
#64720=CARTESIAN_POINT('Ctrl Pts',(-2.6262918233183,-0.0759811813352656,
7.70470624417152E-17));
#64721=CARTESIAN_POINT('Ctrl Pts',(-2.62835986373368,-0.0610601137217946,
8.32667268468867E-17));
#64722=CARTESIAN_POINT('Ctrl Pts',(-2.64106933028015,0.0306396462349494,
1.21490649406612E-16));
#64723=CARTESIAN_POINT('Ctrl Pts',(-2.64875729230249,0.122667828184756,
-4.14607165871163E-17));
#64724=CARTESIAN_POINT('Ctrl Pts',(-2.65128955031192,0.214630073542032,
2.77555756156289E-17));
#64725=CARTESIAN_POINT('Ctrl Pts',(-2.6522874300278,0.250869374168836,5.50314431378172E-17));
#64726=CARTESIAN_POINT('Ctrl Pts',(-2.65248421901964,0.287098764165966,
-2.21971999331922E-16));
#64727=CARTESIAN_POINT('Ctrl Pts',(-2.65186976537464,0.323295201004453,
-1.94289029309402E-16));
#64728=CARTESIAN_POINT('Ctrl Pts',(-2.65036470656989,0.411955698680346,
-1.5423721520059E-16));
#64729=CARTESIAN_POINT('Ctrl Pts',(-2.64399624125764,0.500417941371144,
2.04597414681203E-16));
#64730=CARTESIAN_POINT('Ctrl Pts',(-2.63300888454151,0.588420542790668,
3.05311331771918E-16));
#64731=CARTESIAN_POINT('Ctrl Pts',(-2.62180125647045,0.678187394953273,
4.08044332391981E-16));
#64732=CARTESIAN_POINT('Ctrl Pts',(-2.60578758503461,0.767476722877809,
2.99792977684327E-16));
#64733=CARTESIAN_POINT('Ctrl Pts',(-2.58517343697646,0.856014478842741,
3.60822483003176E-16));
#64734=CARTESIAN_POINT('Ctrl Pts',(-2.58085119192177,0.874578519267442,
3.73618766255344E-16));
#64735=CARTESIAN_POINT('Ctrl Pts',(-2.57632651353202,0.893109507092954,
2.82887540844693E-16));
#64736=CARTESIAN_POINT('Ctrl Pts',(-2.57160101103184,0.911604886184466,
2.77555756156289E-16));
#64737=CARTESIAN_POINT('Ctrl Pts',(-2.56852674851983,0.923637395020121,
2.74087065622529E-16));
#64738=CARTESIAN_POINT('Ctrl Pts',(-2.56536774805562,0.935653628378105,
4.46031676548968E-16));
#64739=CARTESIAN_POINT('Ctrl Pts',(-2.5621271994808,0.94764335418908,4.44089209850063E-16));
#64740=CARTESIAN_POINT('Ctrl Pts',(-2.53799030793295,1.03694758923018,4.29620947158036E-16));
#64741=CARTESIAN_POINT('Ctrl Pts',(-2.5092973140664,1.1249247517235,-6.39262323456962E-17));
#64742=CARTESIAN_POINT('Ctrl Pts',(-2.47633894099238,1.21129265927984,-2.77555756156289E-17));
#64743=CARTESIAN_POINT('Ctrl Pts',(-2.44273663726984,1.29934799669203,9.12177238205123E-18));
#64744=CARTESIAN_POINT('Ctrl Pts',(-2.40470049237272,1.38573136318406,4.0019736649877E-16));
#64745=CARTESIAN_POINT('Ctrl Pts',(-2.36248309795556,1.47014709570666,4.71844785465692E-16));
#64746=CARTESIAN_POINT('Ctrl Pts',(-2.31988758449421,1.55531889564026,5.44133912760492E-16));
#64747=CARTESIAN_POINT('Ctrl Pts',(-2.27303530164497,1.63848852974037,3.07321867395325E-16));
#64748=CARTESIAN_POINT('Ctrl Pts',(-2.22213328141617,1.71934315364419,2.77555756156289E-16));
#64749=CARTESIAN_POINT('Ctrl Pts',(-2.19269440901531,1.76610493137767,2.60340707584599E-16));
#64750=CARTESIAN_POINT('Ctrl Pts',(-2.16190002568321,1.81209214358458,2.90467042585057E-16));
#64751=CARTESIAN_POINT('Ctrl Pts',(-2.12978288301151,1.85724110714762,2.77555756156289E-16));
#64752=CARTESIAN_POINT('Ctrl Pts',(-2.12127057434455,1.8692073619845,2.74133756369675E-16));
#64753=CARTESIAN_POINT('Ctrl Pts',(-2.11266398018409,1.88111653721518,-2.91895564785909E-16));
#64754=CARTESIAN_POINT('Ctrl Pts',(-2.1039679732652,1.89296153585496,-2.77555756156289E-16));
#64755=CARTESIAN_POINT('Ctrl Pts',(-2.04579977039086,1.97219356618236,-1.81635766058884E-16));
#64756=CARTESIAN_POINT('Ctrl Pts',(-1.98380145034343,2.0483310193058,-8.17499915602886E-17));
#64757=CARTESIAN_POINT('Ctrl Pts',(-1.91824824132448,2.1210661916555,0.));
#64758=CARTESIAN_POINT('Ctrl Pts',(-1.85247574695605,2.19404467410286,8.20234575848791E-17));
#64759=CARTESIAN_POINT('Ctrl Pts',(-1.78312414776718,2.26359897673652,7.51967810516288E-17));
#64760=CARTESIAN_POINT('Ctrl Pts',(-1.71042093086391,2.32940356785321,5.55111512312578E-17));
#64761=CARTESIAN_POINT('Ctrl Pts',(-1.63906649560604,2.39398735982976,3.61907269315061E-17));
#64762=CARTESIAN_POINT('Ctrl Pts',(-1.56448311831147,2.45496005537572,4.87793435120361E-16));
#64763=CARTESIAN_POINT('Ctrl Pts',(-1.48684438145143,2.51198742522398,4.9960036108132E-16));
#64764=CARTESIAN_POINT('Ctrl Pts',(-1.42291629818212,2.55894401668503,5.09322236739183E-16));
#64765=CARTESIAN_POINT('Ctrl Pts',(-1.35691584895575,2.60322544461548,2.73980132176117E-17));
#64766=CARTESIAN_POINT('Ctrl Pts',(-1.28892185405323,2.64462557919718,0.));
#64767=CARTESIAN_POINT('Origin',(0.,0.,0.));
#64768=CARTESIAN_POINT('Origin',(-1.44337567297407,-2.5,-6.));
#64769=CARTESIAN_POINT('',(-1.44337567297407,-2.5,-6.));
#64770=CARTESIAN_POINT('',(1.44337567297406,-2.5,-6.));
#64771=CARTESIAN_POINT('',(-0.721687836487033,-2.5,-6.));
#64772=CARTESIAN_POINT('',(-1.44337567297407,-2.5,-3.));
#64773=CARTESIAN_POINT('',(-1.44337567297407,-2.5,-6.));
#64774=CARTESIAN_POINT('',(1.44337567297406,-2.5,-3.));
#64775=CARTESIAN_POINT('',(-1.44337567297407,-2.5,-3.));
#64776=CARTESIAN_POINT('',(1.44337567297406,-2.5,-6.));
#64777=CARTESIAN_POINT('Origin',(-2.88675134594813,3.53525079574969E-16,
-6.));
#64778=CARTESIAN_POINT('',(-2.88675134594813,3.53525079574969E-16,-6.));
#64779=CARTESIAN_POINT('',(-2.52590742770461,-0.625,-6.));
#64780=CARTESIAN_POINT('',(-2.88675134594813,5.55111512312578E-16,-3.));
#64781=CARTESIAN_POINT('',(-2.88675134594813,3.53525079574969E-16,-6.));
#64782=CARTESIAN_POINT('',(-2.88675134594813,3.53525079574969E-16,-3.));
#64783=CARTESIAN_POINT('Origin',(-1.44337567297406,2.5,-6.));
#64784=CARTESIAN_POINT('',(-1.44337567297406,2.5,-6.));
#64785=CARTESIAN_POINT('',(-1.80421959121758,1.875,-6.));
#64786=CARTESIAN_POINT('',(-1.44337567297406,2.5,-3.));
#64787=CARTESIAN_POINT('',(-1.44337567297406,2.5,-6.));
#64788=CARTESIAN_POINT('',(-1.44337567297406,2.5,-3.));
#64789=CARTESIAN_POINT('Origin',(1.44337567297406,2.5,-6.));
#64790=CARTESIAN_POINT('',(1.44337567297406,2.5,-6.));
#64791=CARTESIAN_POINT('',(0.721687836487033,2.5,-6.));
#64792=CARTESIAN_POINT('',(1.44337567297406,2.5,-3.));
#64793=CARTESIAN_POINT('',(1.44337567297406,2.5,-6.));
#64794=CARTESIAN_POINT('',(1.44337567297406,2.5,-3.));
#64795=CARTESIAN_POINT('Origin',(2.88675134594813,0.,-6.));
#64796=CARTESIAN_POINT('',(2.88675134594813,0.,-6.));
#64797=CARTESIAN_POINT('',(2.52590742770461,0.625,-6.));
#64798=CARTESIAN_POINT('',(2.88675134594813,0.,-3.));
#64799=CARTESIAN_POINT('',(2.88675134594813,0.,-6.));
#64800=CARTESIAN_POINT('',(2.88675134594813,0.,-3.));
#64801=CARTESIAN_POINT('Origin',(1.44337567297406,-2.5,-6.));
#64802=CARTESIAN_POINT('',(1.80421959121758,-1.875,-6.));
#64803=CARTESIAN_POINT('',(1.44337567297406,-2.5,-3.));
#64804=CARTESIAN_POINT('Origin',(0.,0.,-3.));
#64805=CARTESIAN_POINT('Origin',(0.,0.,0.));
#64806=CARTESIAN_POINT('',(-5.,-6.12323399573677E-16,0.));
#64807=CARTESIAN_POINT('Origin',(0.,0.,0.));
#64808=CARTESIAN_POINT('Origin',(0.,0.,-6.));
#64809=CARTESIAN_POINT('',(-5.,-6.12323399573677E-16,-6.));
#64810=CARTESIAN_POINT('',(-5.,-6.12323399573677E-16,-6.));
#64811=CARTESIAN_POINT('Origin',(0.,0.,-6.));
#64812=CARTESIAN_POINT('Origin',(0.,0.,-6.));
#64813=CARTESIAN_POINT('Origin',(0.,0.,40.));
#64814=CARTESIAN_POINT('',(0.,0.,0.));
#64815=CARTESIAN_POINT('Origin',(0.,0.,0.));
#64816=CARTESIAN_POINT('',(-3.5,-4.28626379701574E-16,2.));
#64817=CARTESIAN_POINT('Origin',(0.,0.,2.));
#64818=CARTESIAN_POINT('',(-3.5,-4.28626379701574E-16,0.));
#64819=CARTESIAN_POINT('',(-3.5,-4.28626379701574E-16,0.));
#64820=CARTESIAN_POINT('Origin',(0.,0.,0.));
#64821=CARTESIAN_POINT('Origin',(0.,0.,0.));
#64822=CARTESIAN_POINT('',(-7.,-8.57252759403147E-16,2.));
#64823=CARTESIAN_POINT('Origin',(0.,0.,2.));
#64824=CARTESIAN_POINT('',(-7.,-8.57252759403147E-16,0.));
#64825=CARTESIAN_POINT('',(-7.,-8.57252759403147E-16,0.));
#64826=CARTESIAN_POINT('Origin',(0.,0.,0.));
#64827=CARTESIAN_POINT('Origin',(0.,0.,2.));
#64828=CARTESIAN_POINT('Origin',(0.,0.,0.));
#64829=CARTESIAN_POINT('',(0.,0.,0.));
#64830=CARTESIAN_POINT('Origin',(0.,0.,0.));
#64831=CARTESIAN_POINT('',(-3.93802926031087,0.00240391602587063,0.404163522034967));
#64832=CARTESIAN_POINT('',(-3.93675118057464,0.0040445736593347,0.220836477965066));
#64833=CARTESIAN_POINT('',(-3.933,-4.81653586104654E-16,0.));
#64834=CARTESIAN_POINT('',(1.74869447533108,3.5228619944509,0.));
#64835=CARTESIAN_POINT('Ctrl Pts',(-3.93802926031087,0.00240391602587063,
0.404163522034967));
#64836=CARTESIAN_POINT('Ctrl Pts',(-3.93883377792363,0.125055838975485,
0.397936338459335));
#64837=CARTESIAN_POINT('Ctrl Pts',(-3.93360440738597,0.247633516884382,
0.391709154883702));
#64838=CARTESIAN_POINT('Ctrl Pts',(-3.92211779044761,0.369616139861192,
0.385481971308069));
#64839=CARTESIAN_POINT('Ctrl Pts',(-3.79982975336477,1.66825921310945,0.319186554641402));
#64840=CARTESIAN_POINT('Ctrl Pts',(-2.96834465298263,2.89945868843819,0.252891137974736));
#64841=CARTESIAN_POINT('Ctrl Pts',(-1.80941221321754,3.49902123369862,0.186595721308069));
#64842=CARTESIAN_POINT('Ctrl Pts',(-0.722098059799251,4.06153274770308,
0.124397147538713));
#64843=CARTESIAN_POINT('Ctrl Pts',(0.653443523808812,4.06806145998554,0.0621985737693561));
#64844=CARTESIAN_POINT('Ctrl Pts',(1.75279216821279,3.52834843496255,-3.8597597340484E-16));
#64845=CARTESIAN_POINT('',(-1.74869447533093,3.52286199445097,0.));
#64846=CARTESIAN_POINT('Origin',(0.,0.,0.));
#64847=CARTESIAN_POINT('Ctrl Pts',(-1.74869447533093,3.52286199445097,-8.32667268468867E-15));
#64848=CARTESIAN_POINT('Ctrl Pts',(-2.91721720025602,2.94282529798265,0.0659890197515385));
#64849=CARTESIAN_POINT('Ctrl Pts',(-3.7645849420613,1.74090009686325,0.131978039503085));
#64850=CARTESIAN_POINT('Ctrl Pts',(-3.91293878839921,0.452893260042974,
0.197967059254632));
#64851=CARTESIAN_POINT('Ctrl Pts',(-3.9300768225852,0.304100992460439,0.205590198824777));
#64852=CARTESIAN_POINT('Ctrl Pts',(-3.93788639153707,0.15415995008081,0.213213338394921));
#64853=CARTESIAN_POINT('Ctrl Pts',(-3.93675118057464,0.0040445736593347,
0.220836477965066));
#64854=CARTESIAN_POINT('Origin',(0.,0.,0.));
#64855=CARTESIAN_POINT('',(-3.92802248803715,0.00242352018653469,1.65416352203497));
#64856=CARTESIAN_POINT('',(-3.92713181934273,0.00148022330437236,1.47083647796506));
#64857=CARTESIAN_POINT('',(-3.933,-4.81653586104654E-16,0.));
#64858=CARTESIAN_POINT('Ctrl Pts',(-3.92802248803715,0.00242352018653469,
1.65416352203497));
#64859=CARTESIAN_POINT('Ctrl Pts',(-3.93080769929044,0.500504119499087,
1.62904217179267));
#64860=CARTESIAN_POINT('Ctrl Pts',(-3.84303217595021,0.997638580245937,
1.60392082155037));
#64861=CARTESIAN_POINT('Ctrl Pts',(-3.66020947060703,1.45693784959832,1.57879947130807));
#64862=CARTESIAN_POINT('Ctrl Pts',(-3.17773908943919,2.66903179131414,1.5125040546414));
#64863=CARTESIAN_POINT('Ctrl Pts',(-2.03332616040844,3.61762793685371,1.44620863797474));
#64864=CARTESIAN_POINT('Ctrl Pts',(-0.752770987957444,3.86691928292382,
1.37991322130807));
#64865=CARTESIAN_POINT('Ctrl Pts',(0.52778418449355,4.11621062899393,1.31361780464141));
#64866=CARTESIAN_POINT('Ctrl Pts',(1.9444816003648,3.66619717559459,1.24732238797474));
#64867=CARTESIAN_POINT('Ctrl Pts',(2.84640187373471,2.72358226420012,1.18102697130807));
#64868=CARTESIAN_POINT('Ctrl Pts',(3.74832214710463,1.78096735280565,1.1147315546414));
#64869=CARTESIAN_POINT('Ctrl Pts',(4.13546527797321,0.345750983416053,1.04843613797474));
#64870=CARTESIAN_POINT('Ctrl Pts',(3.82997742875317,-0.922539768331961,
0.98214072130807));
#64871=CARTESIAN_POINT('Ctrl Pts',(3.52448957953313,-2.19083052007998,0.915845304641404));
#64872=CARTESIAN_POINT('Ctrl Pts',(2.52637075022448,-3.29219565418641,0.849549887974737));
#64873=CARTESIAN_POINT('Ctrl Pts',(1.29417138623458,-3.72081813581125,0.78325447130807));
#64874=CARTESIAN_POINT('Ctrl Pts',(0.0619720222446886,-4.14944061743609,
0.716959054641403));
#64875=CARTESIAN_POINT('Ctrl Pts',(-1.40430787642644,-3.90532044657934,
0.650663637974736));
#64876=CARTESIAN_POINT('Ctrl Pts',(-2.43090233887023,-3.10021702556709,
0.58436822130807));
#64877=CARTESIAN_POINT('Ctrl Pts',(-3.36106793040868,-2.37073763789067,
0.524299988217036));
#64878=CARTESIAN_POINT('Ctrl Pts',(-3.93026877743734,-1.18071268995158,
0.464231755126001));
#64879=CARTESIAN_POINT('Ctrl Pts',(-3.93802926031087,0.00240391602587063,
0.404163522034967));
#64880=CARTESIAN_POINT('Ctrl Pts',(-3.93675118057464,0.0040445736593347,
0.220836477965066));
#64881=CARTESIAN_POINT('Ctrl Pts',(-3.92805954028601,-1.14530025900202,
0.279202358146468));
#64882=CARTESIAN_POINT('Ctrl Pts',(-3.39501944186553,-2.30486465960329,
0.33756823832787));
#64883=CARTESIAN_POINT('Ctrl Pts',(-2.50983784011762,-3.03729680249085,
0.395934118509273));
#64884=CARTESIAN_POINT('Ctrl Pts',(-1.50904309462757,-3.86539155568325,
0.46192313826082));
#64885=CARTESIAN_POINT('Ctrl Pts',(-0.0581136527769394,-4.14749258954689,
0.527912158012366));
#64886=CARTESIAN_POINT('Ctrl Pts',(1.18097747525515,-3.75784467875485,0.593901177763913));
#64887=CARTESIAN_POINT('Ctrl Pts',(2.42006860328725,-3.3681967679628,0.65989019751546));
#64888=CARTESIAN_POINT('Ctrl Pts',(3.4473214175008,-2.30679991251506,0.725879217267006));
#64889=CARTESIAN_POINT('Ctrl Pts',(3.7952461569347,-1.05580326723859,0.791868237018553));
#64890=CARTESIAN_POINT('Ctrl Pts',(4.14317089636859,0.195193378037875,0.857857256770099));
#64891=CARTESIAN_POINT('Ctrl Pts',(3.81176756102284,1.63578981314307,0.923846276521646));
#64892=CARTESIAN_POINT('Ctrl Pts',(2.95175447945861,2.60896495945216,0.989835296273193));
#64893=CARTESIAN_POINT('Ctrl Pts',(2.09174139789438,3.58214010576126,1.05582431602474));
#64894=CARTESIAN_POINT('Ctrl Pts',(0.703118570111659,4.08789396327424,1.12181333577629));
#64895=CARTESIAN_POINT('Ctrl Pts',(-0.581358437963121,3.89619610319946,
1.18780235552783));
#64896=CARTESIAN_POINT('Ctrl Pts',(-1.8658354460379,3.70449824312467,1.25379137527938));
#64897=CARTESIAN_POINT('Ctrl Pts',(-3.04616663440473,2.81534866546211,1.31978039503093));
#64898=CARTESIAN_POINT('Ctrl Pts',(-3.58469551400156,1.63362301388125,1.38576941478248));
#64899=CARTESIAN_POINT('Ctrl Pts',(-3.81610305421957,1.12583181343609,1.41412510251));
#64900=CARTESIAN_POINT('Ctrl Pts',(-3.92900515343478,0.564017970515558,
1.44248079023753));
#64901=CARTESIAN_POINT('Ctrl Pts',(-3.92713181934273,0.00148022330437236,
1.47083647796506));
#64902=CARTESIAN_POINT('Origin',(0.,0.,0.));
#64903=CARTESIAN_POINT('',(-3.92922266509235,-0.00303564498597975,2.90416352203497));
#64904=CARTESIAN_POINT('',(-3.93210165425081,-0.00353477514852048,2.72083647796507));
#64905=CARTESIAN_POINT('',(-3.933,-4.81653586104654E-16,0.));
#64906=CARTESIAN_POINT('Ctrl Pts',(-3.92922266509235,-0.00303564498597975,
2.90416352203497));
#64907=CARTESIAN_POINT('Ctrl Pts',(-3.92297871157792,0.868988737466586,
2.860148005126));
#64908=CARTESIAN_POINT('Ctrl Pts',(-3.63674668852252,1.74473416863609,2.81613248821704));
#64909=CARTESIAN_POINT('Ctrl Pts',(-3.1031365207039,2.42700192932171,2.77211697130807));
#64910=CARTESIAN_POINT('Ctrl Pts',(-2.29942203778026,3.45462192902401,2.70582155464141));
#64911=CARTESIAN_POINT('Ctrl Pts',(-0.934508767172172,4.04332104416919,
2.63952613797474));
#64912=CARTESIAN_POINT('Ctrl Pts',(0.364487440276112,3.9226192477873,2.57323072130807));
#64913=CARTESIAN_POINT('Ctrl Pts',(1.66348364772439,3.80191745140542,2.5069353046414));
#64914=CARTESIAN_POINT('Ctrl Pts',(2.89656279201286,2.97181474349649,2.44063988797474));
#64915=CARTESIAN_POINT('Ctrl Pts',(3.49718050582551,1.81370463302472,2.37434447130807));
#64916=CARTESIAN_POINT('Ctrl Pts',(4.09779821963816,0.655594522552941,2.30804905464141));
#64917=CARTESIAN_POINT('Ctrl Pts',(4.06595450297497,-0.830522990481683,
2.24175363797474));
#64918=CARTESIAN_POINT('Ctrl Pts',(3.41628053171535,-1.96184182221916,2.17545822130807));
#64919=CARTESIAN_POINT('Ctrl Pts',(2.76660656045572,-3.09316065395665,2.1091628046414));
#64920=CARTESIAN_POINT('Ctrl Pts',(1.49910233459966,-3.86968080439699,2.04286738797474));
#64921=CARTESIAN_POINT('Ctrl Pts',(0.19612795048357,-3.93463064846122,1.97657197130807));
#64922=CARTESIAN_POINT('Ctrl Pts',(-1.10684643363252,-3.99958049252545,
1.91027655464141));
#64923=CARTESIAN_POINT('Ctrl Pts',(-2.44529097600864,-3.35296003021357,
1.84398113797474));
#64924=CARTESIAN_POINT('Ctrl Pts',(-3.20424933054423,-2.29185393011158,
1.77768572130807));
#64925=CARTESIAN_POINT('Ctrl Pts',(-3.67561527519315,-1.6328332127583,1.7365116548837));
#64926=CARTESIAN_POINT('Ctrl Pts',(-3.92345750757062,-0.813934019634444,
1.69533758845933));
#64927=CARTESIAN_POINT('Ctrl Pts',(-3.92802248803715,0.00242352018653469,
1.65416352203497));
#64928=CARTESIAN_POINT('Ctrl Pts',(-3.92713181934273,0.00148022330437236,
1.47083647796506));
#64929=CARTESIAN_POINT('Ctrl Pts',(-3.92464555258188,-0.745113194575937,
1.50846980998908));
#64930=CARTESIAN_POINT('Ctrl Pts',(-3.71999058729667,-1.49298171797386,
1.5461031420131));
#64931=CARTESIAN_POINT('Ctrl Pts',(-3.32188673684523,-2.11752639505612,
1.58373647403711));
#64932=CARTESIAN_POINT('Ctrl Pts',(-2.62382250926525,-3.21264842691343,
1.64972549378866));
#64933=CARTESIAN_POINT('Ctrl Pts',(-1.33096748327849,-3.92859076512888,
1.71571451354021));
#64934=CARTESIAN_POINT('Ctrl Pts',(-0.0323314417446383,-3.93924298867845,
1.78170353329176));
#64935=CARTESIAN_POINT('Ctrl Pts',(1.26630459978921,-3.94989521222801,1.8476925530433));
#64936=CARTESIAN_POINT('Ctrl Pts',(2.57072165687014,-3.2552573211117,1.91368157279485));
#64937=CARTESIAN_POINT('Ctrl Pts',(3.28667213041528,-2.17175971616106,1.9796705925464));
#64938=CARTESIAN_POINT('Ctrl Pts',(4.00262260396041,-1.08826211121042,2.04565961229794));
#64939=CARTESIAN_POINT('Ctrl Pts',(4.13010649396975,0.384095207574565,2.11164863204949));
#64940=CARTESIAN_POINT('Ctrl Pts',(3.61104023017667,1.57453066739559,2.17763765180103));
#64941=CARTESIAN_POINT('Ctrl Pts',(3.0919739663836,2.76496612721661,2.24362667155258));
#64942=CARTESIAN_POINT('Ctrl Pts',(1.92635754878811,3.67347972807368,2.30961569130413));
#64943=CARTESIAN_POINT('Ctrl Pts',(0.645217602507054,3.8861845142162,2.37560471105568));
#64944=CARTESIAN_POINT('Ctrl Pts',(-0.635922343774005,4.09888930035871,
2.44159373080722));
#64945=CARTESIAN_POINT('Ctrl Pts',(-2.03258581874064,3.61578527178667,2.50758275055877));
#64946=CARTESIAN_POINT('Ctrl Pts',(-2.90849151609697,2.65695776267421,2.57357177031032));
#64947=CARTESIAN_POINT('Ctrl Pts',(-3.56006454516537,1.94370044929889,2.62266000619523));
#64948=CARTESIAN_POINT('Ctrl Pts',(-3.92346857353215,0.967194528045436,
2.67174824208015));
#64949=CARTESIAN_POINT('Ctrl Pts',(-3.93210165425081,-0.00353477514852048,
2.72083647796507));
#64950=CARTESIAN_POINT('Origin',(0.,0.,0.));
#64951=CARTESIAN_POINT('',(-3.93905614328696,-0.0012270906503109,4.15416352203497));
#64952=CARTESIAN_POINT('',(-3.93880751349539,0.00135256466245784,3.97083647796506));
#64953=CARTESIAN_POINT('',(-3.933,-4.81653586104654E-16,0.));
#64954=CARTESIAN_POINT('Ctrl Pts',(-3.93905614328696,-0.0012270906503109,
4.15416352203497));
#64955=CARTESIAN_POINT('Ctrl Pts',(-3.93400271395434,1.23712682041522,4.09125383845934));
#64956=CARTESIAN_POINT('Ctrl Pts',(-3.30186786252818,2.47992387689092,4.0283441548837));
#64957=CARTESIAN_POINT('Ctrl Pts',(-2.29585618320052,3.20138074646178,3.96543447130807));
#64958=CARTESIAN_POINT('Ctrl Pts',(-1.2357020119849,3.96166566694986,3.89913905464141));
#64959=CARTESIAN_POINT('Ctrl Pts',(0.239655229969981,4.14298438694454,3.83284363797474));
#64960=CARTESIAN_POINT('Ctrl Pts',(1.45235556362318,3.66202916089297,3.76654822130808));
#64961=CARTESIAN_POINT('Ctrl Pts',(2.66505589727639,3.1810739348414,3.70025280464141));
#64962=CARTESIAN_POINT('Ctrl Pts',(3.61509932262791,2.03784476274358,3.63395738797474));
#64963=CARTESIAN_POINT('Ctrl Pts',(3.86598381354877,0.757603762828532,3.56766197130808));
#64964=CARTESIAN_POINT('Ctrl Pts',(4.11686830446962,-0.522637237086509,
3.50136655464141));
#64965=CARTESIAN_POINT('Ctrl Pts',(3.66859386095981,-1.93989006481879,3.43507113797474));
#64966=CARTESIAN_POINT('Ctrl Pts',(2.727122341044,-2.84299104576975,3.36877572130807));
#64967=CARTESIAN_POINT('Ctrl Pts',(1.78565082112817,-3.74609202672072,3.30248030464141));
#64968=CARTESIAN_POINT('Ctrl Pts',(0.350982224806341,-4.13504116089037,
3.23618488797474));
#64969=CARTESIAN_POINT('Ctrl Pts',(-0.917718077119649,-3.83113398528177,
3.16988947130807));
#64970=CARTESIAN_POINT('Ctrl Pts',(-2.18641837904563,-3.52722680967316,
3.10359405464141));
#64971=CARTESIAN_POINT('Ctrl Pts',(-3.28915038657576,-2.5304633242863,3.03729863797474));
#64972=CARTESIAN_POINT('Ctrl Pts',(-3.71925854272124,-1.29881113946316,
2.97100322130807));
#64973=CARTESIAN_POINT('Ctrl Pts',(-3.86380498477882,-0.884889806828835,
2.94872332155037));
#64974=CARTESIAN_POINT('Ctrl Pts',(-3.93238324727252,-0.44443943146198,
2.92644342179267));
#64975=CARTESIAN_POINT('Ctrl Pts',(-3.92922266509235,-0.00303564498597975,
2.90416352203497));
#64976=CARTESIAN_POINT('Ctrl Pts',(-3.93210165425081,-0.00353477514852048,
2.72083647796507));
#64977=CARTESIAN_POINT('Ctrl Pts',(-3.93507397192935,-0.337751025753829,
2.7377372618317));
#64978=CARTESIAN_POINT('Ctrl Pts',(-3.89599232991999,-0.671282525635842,
2.75463804569833));
#64979=CARTESIAN_POINT('Ctrl Pts',(-3.8121385671165,-0.993149807387589,
2.77153882956496));
#64980=CARTESIAN_POINT('Ctrl Pts',(-3.48473200103367,-2.24987887868406,
2.8375278493165));
#64981=CARTESIAN_POINT('Ctrl Pts',(-2.47477094912201,-3.32878603162411,
2.90351686906805));
#64982=CARTESIAN_POINT('Ctrl Pts',(-1.24236721552543,-3.73835094435147,
2.9695058888196));
#64983=CARTESIAN_POINT('Ctrl Pts',(-0.00996348192884827,-4.14791585707883,
3.03549490857114));
#64984=CARTESIAN_POINT('Ctrl Pts',(1.44488293335264,-3.88813852959348,3.10148392832269));
#64985=CARTESIAN_POINT('Ctrl Pts',(2.45938288232363,-3.07736603319569,3.16747294807423));
#64986=CARTESIAN_POINT('Ctrl Pts',(3.47388283129462,-2.26659353679789,3.23346196782578));
#64987=CARTESIAN_POINT('Ctrl Pts',(4.04803631395511,-0.904825871487629,
3.29945098757733));
#64988=CARTESIAN_POINT('Ctrl Pts',(3.92027415756993,0.387551512556629,3.36544000732888));
#64989=CARTESIAN_POINT('Ctrl Pts',(3.79251200118475,1.67992889660089,3.43142902708043));
#64990=CARTESIAN_POINT('Ctrl Pts',(2.9628342057539,2.90291599937915,3.49741804683197));
#64991=CARTESIAN_POINT('Ctrl Pts',(1.80921997711047,3.4993525625956,3.56340706658351));
#64992=CARTESIAN_POINT('Ctrl Pts',(0.655605748467037,4.09578912581204,3.62939608633506));
#64993=CARTESIAN_POINT('Ctrl Pts',(-0.821944913388967,4.06567514946666,
3.69538510608661));
#64994=CARTESIAN_POINT('Ctrl Pts',(-1.95029923212904,3.42272967879372,3.76137412583816));
#64995=CARTESIAN_POINT('Ctrl Pts',(-3.07865355086909,2.77978420812079,3.82736314558971));
#64996=CARTESIAN_POINT('Ctrl Pts',(-3.85781152649321,1.52400724312031,3.89335216534125));
#64997=CARTESIAN_POINT('Ctrl Pts',(-3.93280948119039,0.227497431243224,
3.9593411850928));
#64998=CARTESIAN_POINT('Ctrl Pts',(-3.93716436455993,0.152213391285224,
3.96317294938355));
#64999=CARTESIAN_POINT('Ctrl Pts',(-3.93914500265902,0.0767920107140475,
3.96700471367431));
#65000=CARTESIAN_POINT('Ctrl Pts',(-3.93880751349539,0.00135256466245784,
3.97083647796506));
#65001=CARTESIAN_POINT('Origin',(0.,0.,0.));
#65002=CARTESIAN_POINT('',(-3.93296230846032,0.00363373906124689,5.40416352203497));
#65003=CARTESIAN_POINT('',(-3.92828912629456,0.00246571223358432,5.22083647796506));
#65004=CARTESIAN_POINT('',(-3.933,-4.81653586104654E-16,0.));
#65005=CARTESIAN_POINT('Ctrl Pts',(-3.93296230846032,0.00363373906124689,
5.40416352203497));
#65006=CARTESIAN_POINT('Ctrl Pts',(-3.9357953201641,0.310142843416023,5.38865508845934));
#65007=CARTESIAN_POINT('Ctrl Pts',(-3.90300011193378,0.616052391820026,
5.37314665488371));
#65008=CARTESIAN_POINT('Ctrl Pts',(-3.83227848816066,0.912927092582172,
5.35763822130808));
#65009=CARTESIAN_POINT('Ctrl Pts',(-3.5299578512944,2.18200638991017,5.29134280464141));
#65010=CARTESIAN_POINT('Ctrl Pts',(-2.53457385463363,3.285983824268,5.22504738797474));
#65011=CARTESIAN_POINT('Ctrl Pts',(-1.30346046335894,3.71763165307261,5.15875197130808));
#65012=CARTESIAN_POINT('Ctrl Pts',(-0.0723470720842406,4.14927948187723,
5.09245655464141));
#65013=CARTESIAN_POINT('Ctrl Pts',(1.39449571380438,3.90859770512862,5.02616113797475));
#65014=CARTESIAN_POINT('Ctrl Pts',(2.42311992072895,3.10616872311079,4.95986572130808));
#65015=CARTESIAN_POINT('Ctrl Pts',(3.45174412765351,2.30373974109297,4.89357030464141));
#65016=CARTESIAN_POINT('Ctrl Pts',(4.04214975561404,0.939563553805948,4.82727488797474));
#65017=CARTESIAN_POINT('Ctrl Pts',(3.92307209884529,-0.359582528175298,
4.76097947130807));
#65018=CARTESIAN_POINT('Ctrl Pts',(3.80399444207653,-1.65872861015655,4.69468405464141));
#65019=CARTESIAN_POINT('Ctrl Pts',(2.97543350057849,-2.89284458683203,4.62838863797474));
#65020=CARTESIAN_POINT('Ctrl Pts',(1.81807558455521,-3.49490993557188,4.56209322130808));
#65021=CARTESIAN_POINT('Ctrl Pts',(0.660717668531931,-4.09697528431174,
4.49579780464141));
#65022=CARTESIAN_POINT('Ctrl Pts',(-0.825437222016575,-4.06699000511596,
4.42950238797474));
#65023=CARTESIAN_POINT('Ctrl Pts',(-1.9575680744248,-3.4187309805296,4.36320697130807));
#65024=CARTESIAN_POINT('Ctrl Pts',(-3.08969892683302,-2.77047195594323,
4.29691155464141));
#65025=CARTESIAN_POINT('Ctrl Pts',(-3.86780574110097,-1.50393918596629,
4.23061613797475));
#65026=CARTESIAN_POINT('Ctrl Pts',(-3.93438359799676,-0.201047240487073,
4.16432072130808));
#65027=CARTESIAN_POINT('Ctrl Pts',(-3.93778375542175,-0.134508034676906,
4.16093498821704));
#65028=CARTESIAN_POINT('Ctrl Pts',(-3.93932811354563,-0.0678739974030474,
4.15754925512601));
#65029=CARTESIAN_POINT('Ctrl Pts',(-3.93905614328696,-0.0012270906503109,
4.15416352203497));
#65030=CARTESIAN_POINT('Ctrl Pts',(-3.93880751349539,0.00135256466245784,
3.97083647796506));
#65031=CARTESIAN_POINT('Ctrl Pts',(-3.93333290739557,-1.22239413900672,
4.03299373342586));
#65032=CARTESIAN_POINT('Ctrl Pts',(-3.31786739155683,-2.45089458463356,
4.09515098888665));
#65033=CARTESIAN_POINT('Ctrl Pts',(-2.33195280377124,-3.17501835816601,
4.15730824434744));
#65034=CARTESIAN_POINT('Ctrl Pts',(-1.28526023788469,-3.94378167694446,
4.22329726409898));
#65035=CARTESIAN_POINT('Ctrl Pts',(0.178962827658628,-4.14406565574766,
4.28928628385053));
#65036=CARTESIAN_POINT('Ctrl Pts',(1.39365528985826,-3.68462622601686,4.35527530360208));
#65037=CARTESIAN_POINT('Ctrl Pts',(2.60834775205789,-3.22518679628606,4.42126432335363));
#65038=CARTESIAN_POINT('Ctrl Pts',(3.57350961091383,-2.10602395802126,4.48725334310517));
#65039=CARTESIAN_POINT('Ctrl Pts',(3.84943877691641,-0.836998557262767,
4.55324236285672));
#65040=CARTESIAN_POINT('Ctrl Pts',(4.12536794291899,0.432026843495729,4.61923138260827));
#65041=CARTESIAN_POINT('Ctrl Pts',(3.71206441606821,1.85091480674793,4.68522040235981));
#65042=CARTESIAN_POINT('Ctrl Pts',(2.79781829806152,2.77325769599943,4.75120942211136));
#65043=CARTESIAN_POINT('Ctrl Pts',(1.88357218005484,3.69560058525093,4.81719844186291));
#65044=CARTESIAN_POINT('Ctrl Pts',(0.468383470892278,4.12139840050174,4.88318746161446));
#65045=CARTESIAN_POINT('Ctrl Pts',(-0.80302547217005,3.85666897385885,4.949176481366));
#65046=CARTESIAN_POINT('Ctrl Pts',(-2.07443441523238,3.59193954721596,5.01516550111755));
#65047=CARTESIAN_POINT('Ctrl Pts',(-3.20206359219447,2.63668287867936,5.08115452086909));
#65048=CARTESIAN_POINT('Ctrl Pts',(-3.67219512395154,1.42608851501744,5.14714354062064));
#65049=CARTESIAN_POINT('Ctrl Pts',(-3.84720087310926,0.97544660051541,5.17170785306878));
#65050=CARTESIAN_POINT('Ctrl Pts',(-3.93109787542163,0.489422814161963,
5.19627216551692));
#65051=CARTESIAN_POINT('Ctrl Pts',(-3.92828912629456,0.00246571223358432,
5.22083647796506));
#65052=CARTESIAN_POINT('Origin',(0.,0.,0.));
#65053=CARTESIAN_POINT('',(-3.92652974478545,-0.000411687324547438,6.65416352203497));
#65054=CARTESIAN_POINT('',(-3.93002130470952,-0.00320230624235995,6.47083647796506));
#65055=CARTESIAN_POINT('',(-3.933,-4.81653586104654E-16,0.));
#65056=CARTESIAN_POINT('Ctrl Pts',(-3.92652974478545,-0.000411687324547438,
6.65416352203497));
#65057=CARTESIAN_POINT('Ctrl Pts',(-3.92589461438976,0.682335166633042,
6.61976092179267));
#65058=CARTESIAN_POINT('Ctrl Pts',(-3.75684139145261,1.36537647043677,6.58535832155038));
#65059=CARTESIAN_POINT('Ctrl Pts',(-3.42117596084786,1.95329192188792,6.55095572130808));
#65060=CARTESIAN_POINT('Ctrl Pts',(-2.77433300636735,3.0862324422038,6.48466030464142));
#65061=CARTESIAN_POINT('Ctrl Pts',(-1.50877413310263,3.8659222616113,6.41836488797474));
#65062=CARTESIAN_POINT('Ctrl Pts',(-0.20596645283144,3.93412914220049,6.35206947130808));
#65063=CARTESIAN_POINT('Ctrl Pts',(1.09684122743973,4.00233602278968,6.28577405464141));
#65064=CARTESIAN_POINT('Ctrl Pts',(2.43689771471741,3.35905996456059,6.21947863797475));
#65065=CARTESIAN_POINT('Ctrl Pts',(3.19850761012674,2.29985724668934,6.15318322130808));
#65066=CARTESIAN_POINT('Ctrl Pts',(3.96011750553607,1.24065452881808,6.08688780464141));
#65067=CARTESIAN_POINT('Ctrl Pts',(4.14328080907704,-0.234474848695338,
6.02059238797475));
#65068=CARTESIAN_POINT('Ctrl Pts',(3.66384225990336,-1.44777559785307,5.95429697130808));
#65069=CARTESIAN_POINT('Ctrl Pts',(3.18440371072968,-2.66107634701081,5.88800155464141));
#65070=CARTESIAN_POINT('Ctrl Pts',(2.04236330884135,-3.61254846781286,5.82170613797475));
#65071=CARTESIAN_POINT('Ctrl Pts',(0.762437010209958,-3.86503351766844,
5.75541072130808));
#65072=CARTESIAN_POINT('Ctrl Pts',(-0.517489288421428,-4.11751856752401,
5.68911530464141));
#65073=CARTESIAN_POINT('Ctrl Pts',(-1.93530148379588,-3.67101654643311,
5.62281988797474));
#65074=CARTESIAN_POINT('Ctrl Pts',(-2.83957894294725,-2.73067495573858,
5.55652447130808));
#65075=CARTESIAN_POINT('Ctrl Pts',(-3.53231950235033,-2.0103067181193,5.50573748821704));
#65076=CARTESIAN_POINT('Ctrl Pts',(-3.92368476815972,-1.00012158053316,
5.45495050512601));
#65077=CARTESIAN_POINT('Ctrl Pts',(-3.93296230846032,0.00363373906124689,
5.40416352203497));
#65078=CARTESIAN_POINT('Ctrl Pts',(-3.92828912629456,0.00246571223358432,
5.22083647796506));
#65079=CARTESIAN_POINT('Ctrl Pts',(-3.92355251456471,-0.818727857066773,
5.26226118526847));
#65080=CARTESIAN_POINT('Ctrl Pts',(-3.6722360563846,-1.64257565411253,5.30368589257188));
#65081=CARTESIAN_POINT('Ctrl Pts',(-3.19545580456006,-2.30386798269549,
5.34511059987528));
#65082=CARTESIAN_POINT('Ctrl Pts',(-2.43595106685949,-3.35729805795928,
5.41109961962683));
#65083=CARTESIAN_POINT('Ctrl Pts',(-1.10430770490628,-3.99822614969962,
5.47708863937837));
#65084=CARTESIAN_POINT('Ctrl Pts',(0.192812962944398,-3.93466245600138,
5.54307765912992));
#65085=CARTESIAN_POINT('Ctrl Pts',(1.48993363079507,-3.87109876230314,5.60906667888147));
#65086=CARTESIAN_POINT('Ctrl Pts',(2.75253160454323,-3.10304328316634,5.67505569863302));
#65087=CARTESIAN_POINT('Ctrl Pts',(3.40540080922965,-1.98040167883568,5.74104471838456));
#65088=CARTESIAN_POINT('Ctrl Pts',(4.05827001391607,-0.85776007450501,5.80703373813611));
#65089=CARTESIAN_POINT('Ctrl Pts',(4.10141044954074,0.619467655019518,5.87302275788765));
#65090=CARTESIAN_POINT('Ctrl Pts',(3.51516848040003,1.77829582336785,5.9390117776392));
#65091=CARTESIAN_POINT('Ctrl Pts',(2.92892651125932,2.93712399171616,6.00500079739075));
#65092=CARTESIAN_POINT('Ctrl Pts',(1.71330213735326,3.77755259888829,6.0709898171423));
#65093=CARTESIAN_POINT('Ctrl Pts',(0.422101510131257,3.91670471139359,6.13697883689384));
#65094=CARTESIAN_POINT('Ctrl Pts',(-0.869099117090753,4.0558568238989,6.20296785664539));
#65095=CARTESIAN_POINT('Ctrl Pts',(-2.23587599762871,3.49373244173736,6.26895687639693));
#65096=CARTESIAN_POINT('Ctrl Pts',(-3.05556191587462,2.48642049125139,6.33494589614848));
#65097=CARTESIAN_POINT('Ctrl Pts',(-3.61821914155989,1.79497107770904,6.38024275675401));
#65098=CARTESIAN_POINT('Ctrl Pts',(-3.92309448347202,0.893755285438259,
6.42553961735953));
#65099=CARTESIAN_POINT('Ctrl Pts',(-3.93002130470952,-0.00320230624235995,
6.47083647796506));
#65100=CARTESIAN_POINT('Origin',(0.,0.,0.));
#65101=CARTESIAN_POINT('',(-3.93447829914432,-0.00349241703522352,7.90416352203497));
#65102=CARTESIAN_POINT('',(-3.93938385220859,1.46978575541911E-5,7.72083647796507));
#65103=CARTESIAN_POINT('',(-3.933,-4.81653586104654E-16,0.));
#65104=CARTESIAN_POINT('Ctrl Pts',(-3.93447829914432,-0.00349241703522352,
7.90416352203497));
#65105=CARTESIAN_POINT('Ctrl Pts',(-3.9247550811977,1.04882587479658,7.85086675512601));
#65106=CARTESIAN_POINT('Ctrl Pts',(-3.48928102444049,2.10824344340663,7.79756998821704));
#65107=CARTESIAN_POINT('Ctrl Pts',(-2.73422329881441,2.83616241414651,7.74427322130808));
#65108=CARTESIAN_POINT('Ctrl Pts',(-1.79501310969974,3.74161492587582,7.67797780464141));
#65109=CARTESIAN_POINT('Ctrl Pts',(-0.361321637001168,4.13415057686167,
7.61168238797475));
#65110=CARTESIAN_POINT('Ctrl Pts',(0.90813467596085,3.83341697412564,7.54538697130808));
#65111=CARTESIAN_POINT('Ctrl Pts',(2.17759098892287,3.5326833713896,7.47909155464142));
#65112=CARTESIAN_POINT('Ctrl Pts',(3.28281214214833,2.53868051493168,7.41279613797475));
#65113=CARTESIAN_POINT('Ctrl Pts',(3.71599896057147,1.30810779839759,7.34650072130808));
#65114=CARTESIAN_POINT('Ctrl Pts',(4.14918577899461,0.0775350818634785,
7.28020530464142));
#65115=CARTESIAN_POINT('Ctrl Pts',(3.91033826261541,-1.3896074947468,7.21390988797475));
#65116=CARTESIAN_POINT('Ctrl Pts',(3.10919605171297,-2.41923421751785,7.14761447130808));
#65117=CARTESIAN_POINT('Ctrl Pts',(2.30805384081054,-3.44886094028888,7.08131905464142));
#65118=CARTESIAN_POINT('Ctrl Pts',(0.944616935384907,-4.04097180922069,
7.01502363797475));
#65119=CARTESIAN_POINT('Ctrl Pts',(-0.354677020107964,-3.92351863747392,
6.94872822130808));
#65120=CARTESIAN_POINT('Ctrl Pts',(-1.65397097560085,-3.80606546572714,
6.88243280464142));
#65121=CARTESIAN_POINT('Ctrl Pts',(-2.88912198116097,-2.97904825330177,
6.81613738797475));
#65122=CARTESIAN_POINT('Ctrl Pts',(-3.49263396609285,-1.82244403647695,
6.74984197130808));
#65123=CARTESIAN_POINT('Ctrl Pts',(-3.78296620794476,-1.26603504445995,
6.71794915488371));
#65124=CARTESIAN_POINT('Ctrl Pts',(-3.92711854031175,-0.633349893280725,
6.68605633845934));
#65125=CARTESIAN_POINT('Ctrl Pts',(-3.92652974478545,-0.000411687324547438,
6.65416352203497));
#65126=CARTESIAN_POINT('Ctrl Pts',(-3.93002130470952,-0.00320230624235995,
6.47083647796506));
#65127=CARTESIAN_POINT('Ctrl Pts',(-3.93318556124973,-0.412943488880185,
6.49152863711108));
#65128=CARTESIAN_POINT('Ctrl Pts',(-3.87417469570846,-0.821796081297978,
6.5122207962571));
#65129=CARTESIAN_POINT('Ctrl Pts',(-3.74915976782805,-1.2093578942389,6.53291295540312));
#65130=CARTESIAN_POINT('Ctrl Pts',(-3.35047674558173,-2.44532481043286,
6.59890197515467));
#65131=CARTESIAN_POINT('Ctrl Pts',(-2.28051574513518,-3.46475912401038,
6.66489099490622));
#65132=CARTESIAN_POINT('Ctrl Pts',(-1.02672255697162,-3.80323365993697,
6.73088001465776));
#65133=CARTESIAN_POINT('Ctrl Pts',(0.227070631191932,-4.14170819586356,
6.79686903440931));
#65134=CARTESIAN_POINT('Ctrl Pts',(1.6646960070725,-3.79922295413924,6.86285805416086));
#65135=CARTESIAN_POINT('Ctrl Pts',(2.63120966385873,-2.93180510707663,6.92884707391241));
#65136=CARTESIAN_POINT('Ctrl Pts',(3.59772332064497,-2.06438726001401,6.99483609366395));
#65137=CARTESIAN_POINT('Ctrl Pts',(4.09312525833685,-0.67203680761309,7.0608251134155));
#65138=CARTESIAN_POINT('Ctrl Pts',(3.89172352271858,0.610928394972594,7.12681413316704));
#65139=CARTESIAN_POINT('Ctrl Pts',(3.69032178710031,1.89389359755828,7.19280315291859));
#65140=CARTESIAN_POINT('Ctrl Pts',(2.79211637817189,3.06747355032872,7.25879217267014));
#65141=CARTESIAN_POINT('Ctrl Pts',(1.6063058044677,3.59701642248127,7.32478119242169));
#65142=CARTESIAN_POINT('Ctrl Pts',(0.420495230763517,4.12655929463381,7.39077021217323));
#65143=CARTESIAN_POINT('Ctrl Pts',(-1.05292050771645,4.01206508616847,7.45675923192478));
#65144=CARTESIAN_POINT('Ctrl Pts',(-2.14269236632785,3.30569431501852,7.52274825167632));
#65145=CARTESIAN_POINT('Ctrl Pts',(-3.23313122693673,2.59889120501564,7.58877766043924));
#65146=CARTESIAN_POINT('Ctrl Pts',(-3.93945619971352,1.29948678660994,7.65480706920215));
#65147=CARTESIAN_POINT('Ctrl Pts',(-3.93938382520912,1.46977953919901E-5,
7.72083647796507));
#65148=CARTESIAN_POINT('Origin',(0.,0.,0.));
#65149=CARTESIAN_POINT('',(-3.93821611579729,0.00204091754689266,9.15416352203497));
#65150=CARTESIAN_POINT('',(-3.92998043343738,0.00319075123336177,8.97083647796505));
#65151=CARTESIAN_POINT('',(-3.933,-4.81653586104654E-16,0.));
#65152=CARTESIAN_POINT('Ctrl Pts',(-3.93821611579729,0.00204091754689266,
9.15416352203497));
#65153=CARTESIAN_POINT('Ctrl Pts',(-3.93894783685051,0.118157629700958,
9.148268005126));
#65154=CARTESIAN_POINT('Ctrl Pts',(-3.93425943595939,0.234214412386688,
9.14237248821704));
#65155=CARTESIAN_POINT('Ctrl Pts',(-3.92395904216079,0.349770957401461,
9.13647697130808));
#65156=CARTESIAN_POINT('Ctrl Pts',(-3.80813053903654,1.64921075523655,9.07018155464141));
#65157=CARTESIAN_POINT('Ctrl Pts',(-2.98265834852961,2.88539485919645,9.00388613797475));
#65158=CARTESIAN_POINT('Ctrl Pts',(-1.82680963916627,3.49035253655646,8.93759072130809));
#65159=CARTESIAN_POINT('Ctrl Pts',(-0.670960929802935,4.09531021391648,
8.87129530464142));
#65160=CARTESIAN_POINT('Ctrl Pts',(0.815264298416776,4.06904146467662,8.80499988797475));
#65161=CARTESIAN_POINT('Ctrl Pts',(1.94901271550604,3.42361559203026,8.73870447130808));
#65162=CARTESIAN_POINT('Ctrl Pts',(3.08276113259532,2.7781897193839,8.67240905464142));
#65163=CARTESIAN_POINT('Ctrl Pts',(3.86403273855411,1.51360672333098,8.60611363797475));
#65164=CARTESIAN_POINT('Ctrl Pts',(3.93386853603566,0.210885344169694,8.53981822130808));
#65165=CARTESIAN_POINT('Ctrl Pts',(4.00370433351722,-1.09183603499157,8.47352280464141));
#65166=CARTESIAN_POINT('Ctrl Pts',(3.36210432252157,-2.43269579726122,8.40722738797475));
#65167=CARTESIAN_POINT('Ctrl Pts',(2.30385471425629,-3.19562947520453,8.34093197130808));
#65168=CARTESIAN_POINT('Ctrl Pts',(1.245605105991,-3.95856315314785,8.27463655464141));
#65169=CARTESIAN_POINT('Ctrl Pts',(-0.229294099543933,-4.14357074676481,
8.20834113797475));
#65170=CARTESIAN_POINT('Ctrl Pts',(-1.44319336796336,-3.66564962726439,
8.14204572130808));
#65171=CARTESIAN_POINT('Ctrl Pts',(-2.65709263638277,-3.18772850776397,
8.07575030464142));
#65172=CARTESIAN_POINT('Ctrl Pts',(-3.60999196768669,-2.04687867514619,
8.00945488797475));
#65173=CARTESIAN_POINT('Ctrl Pts',(-3.86407718057327,-0.767269072600908,
7.94315947130809));
#65174=CARTESIAN_POINT('Ctrl Pts',(-3.91389607993295,-0.516373944605648,
7.93016082155038));
#65175=CARTESIAN_POINT('Ctrl Pts',(-3.9368497132457,-0.260144324880089,
7.91716217179267));
#65176=CARTESIAN_POINT('Ctrl Pts',(-3.93447829914432,-0.00349241703522352,
7.90416352203497));
#65177=CARTESIAN_POINT('Ctrl Pts',(-3.93938382520912,1.46977953919901E-5,
7.72083647796507));
#65178=CARTESIAN_POINT('Ctrl Pts',(-3.93931153924511,-1.29786766323116,
7.78678510870525));
#65179=CARTESIAN_POINT('Ctrl Pts',(-3.23496159726654,-2.5958172902133,7.85273373944543));
#65180=CARTESIAN_POINT('Ctrl Pts',(-2.14671745478129,-3.30308184131171,
7.91868237018561));
#65181=CARTESIAN_POINT('Ctrl Pts',(-1.05780683742692,-4.01077954341983,
7.98467138993715));
#65182=CARTESIAN_POINT('Ctrl Pts',(0.415468342137214,-4.12706843993453,
8.0506604096887));
#65183=CARTESIAN_POINT('Ctrl Pts',(1.60192307417263,-3.59897040075338,8.11664942944025));
#65184=CARTESIAN_POINT('Ctrl Pts',(2.78837780620806,-3.07087236157223,8.18263844919179));
#65185=CARTESIAN_POINT('Ctrl Pts',(3.68801209071479,-1.89838738669521,8.24862746894334));
#65186=CARTESIAN_POINT('Ctrl Pts',(3.89097646142656,-0.61566846410235,8.31461648869489));
#65187=CARTESIAN_POINT('Ctrl Pts',(4.09394083213833,0.667050458490491,8.38060550844643));
#65188=CARTESIAN_POINT('Ctrl Pts',(3.60023528905517,2.06000332879919,8.44659452819797));
#65189=CARTESIAN_POINT('Ctrl Pts',(2.63477895410256,2.92859784608333,8.51258354794952));
#65190=CARTESIAN_POINT('Ctrl Pts',(1.66932261914996,3.79719236336747,8.57857256770107));
#65191=CARTESIAN_POINT('Ctrl Pts',(0.232115492327916,4.14142852762707,8.64456158745263));
#65192=CARTESIAN_POINT('Ctrl Pts',(-1.02208906270644,3.80448149278736,8.71055060720417));
#65193=CARTESIAN_POINT('Ctrl Pts',(-2.2762936177408,3.46753445794766,8.77653962695572));
#65194=CARTESIAN_POINT('Ctrl Pts',(-3.34749560098745,2.44940422400868,8.84252864670726));
#65195=CARTESIAN_POINT('Ctrl Pts',(-3.74768386318513,1.21392386198126,8.9085176664588));
#65196=CARTESIAN_POINT('Ctrl Pts',(-3.8736606644409,0.82500225001839,8.92929060362755));
#65197=CARTESIAN_POINT('Ctrl Pts',(-3.93314325094733,0.414542291462066,
8.9500635407963));
#65198=CARTESIAN_POINT('Ctrl Pts',(-3.92998043343738,0.00319075123336177,
8.97083647796505));
#65199=CARTESIAN_POINT('Origin',(0.,0.,0.));
#65200=CARTESIAN_POINT('',(-3.92814797210457,0.00249985979813405,10.404163522035));
#65201=CARTESIAN_POINT('',(-3.92831996318525,-0.00248455515896013,10.2208364779651));
#65202=CARTESIAN_POINT('',(-3.933,-4.81653586104654E-16,0.));
#65203=CARTESIAN_POINT('Ctrl Pts',(-3.92814797210457,0.00249985979813405,
10.404163522035));
#65204=CARTESIAN_POINT('Ctrl Pts',(-3.93099418832143,0.493964345027469,
10.3793738384593));
#65205=CARTESIAN_POINT('Ctrl Pts',(-3.84559145503871,0.984475393727741,
10.3545841548837));
#65206=CARTESIAN_POINT('Ctrl Pts',(-3.66745126380575,1.43860888180441,10.3297944713081));
#65207=CARTESIAN_POINT('Ctrl Pts',(-3.19104832115264,2.65310477169666,10.2634990546414));
#65208=CARTESIAN_POINT('Ctrl Pts',(-2.05139084139042,3.60742982376513,10.1972036379748));
#65209=CARTESIAN_POINT('Ctrl Pts',(-0.772099935454148,3.86311480244487,
10.1309082213081));
#65210=CARTESIAN_POINT('Ctrl Pts',(0.507190970482145,4.1187997811246,10.0646128046414));
#65211=CARTESIAN_POINT('Ctrl Pts',(1.92611530259251,3.67584468641558,9.99831738797475));
#65212=CARTESIAN_POINT('Ctrl Pts',(2.83274145133105,2.737767367237,9.93202197130808));
#65213=CARTESIAN_POINT('Ctrl Pts',(3.73936760006958,1.79969004805842,9.86572655464141));
#65214=CARTESIAN_POINT('Ctrl Pts',(4.13369556543631,0.366490504410305,9.79943113797476));
#65215=CARTESIAN_POINT('Ctrl Pts',(3.83454946698936,-0.903340839555381,
9.73313572130809));
#65216=CARTESIAN_POINT('Ctrl Pts',(3.5354033685424,-2.17317218352107,9.66684030464142));
#65217=CARTESIAN_POINT('Ctrl Pts',(2.54278320628176,-3.27963532780432,9.60054488797475));
#65218=CARTESIAN_POINT('Ctrl Pts',(1.31275308835322,-3.71436045857372,9.53424947130808));
#65219=CARTESIAN_POINT('Ctrl Pts',(0.0827229704247114,-4.14908558934312,
9.46795405464141));
#65220=CARTESIAN_POINT('Ctrl Pts',(-1.38471710317168,-3.9120727065987,9.40165863797475));
#65221=CARTESIAN_POINT('Ctrl Pts',(-2.41534473209911,-3.11221851937135,
9.33536322130809));
#65222=CARTESIAN_POINT('Ctrl Pts',(-3.35432073684664,-2.3834937423295,9.27496332155038));
#65223=CARTESIAN_POINT('Ctrl Pts',(-3.9307195927702,-1.18758127887811,9.21456342179267));
#65224=CARTESIAN_POINT('Ctrl Pts',(-3.93821611579729,0.00204091754689266,
9.15416352203497));
#65225=CARTESIAN_POINT('Ctrl Pts',(-3.92998043343738,0.00319075123336177,
8.97083647796505));
#65226=CARTESIAN_POINT('Ctrl Pts',(-3.92309598486073,-0.892190824441041,
9.01605256054785));
#65227=CARTESIAN_POINT('Ctrl Pts',(-3.61940103242935,-1.7917966653998,9.06126864313065));
#65228=CARTESIAN_POINT('Ctrl Pts',(-3.05858836669887,-2.48269665568713,
9.10648472571345));
#65229=CARTESIAN_POINT('Ctrl Pts',(-2.24013006686625,-3.49100632121223,
9.17247374546499));
#65230=CARTESIAN_POINT('Ctrl Pts',(-0.874038926052342,-4.05479516214657,
9.23846276521654));
#65231=CARTESIAN_POINT('Ctrl Pts',(0.417330244931444,-3.91721596899267,
9.30445178496809));
#65232=CARTESIAN_POINT('Ctrl Pts',(1.70869941591521,-3.77963677583877,9.37044080471963));
#65233=CARTESIAN_POINT('Ctrl Pts',(2.92534661706887,-2.94068954859666,9.43642982447118));
#65234=CARTESIAN_POINT('Ctrl Pts',(3.51299972402516,-1.78257634340435,9.50241884422273));
#65235=CARTESIAN_POINT('Ctrl Pts',(4.10065283098146,-0.624463138212041,
9.56840786397428));
#65236=CARTESIAN_POINT('Ctrl Pts',(4.0593118437404,0.852816044930448,9.63439688372583));
#65237=CARTESIAN_POINT('Ctrl Pts',(3.40781061717775,1.97625207868741,9.70038590347737));
#65238=CARTESIAN_POINT('Ctrl Pts',(2.75630939061511,3.09968811244436,9.76637492322892));
#65239=CARTESIAN_POINT('Ctrl Pts',(1.49464792473085,3.86928099681577,9.83236394298046));
#65240=CARTESIAN_POINT('Ctrl Pts',(0.197605646350524,3.93442467072329,9.89835296273201));
#65241=CARTESIAN_POINT('Ctrl Pts',(-1.09943663202981,3.99956834463081,9.96434198248356));
#65242=CARTESIAN_POINT('Ctrl Pts',(-2.4318597229062,3.36026280807446,10.0303310022351));
#65243=CARTESIAN_POINT('Ctrl Pts',(-3.19264708406683,2.30775866971944,10.0963200219866));
#65244=CARTESIAN_POINT('Ctrl Pts',(-3.67116379448099,1.6457592153455,10.1378255073128));
#65245=CARTESIAN_POINT('Ctrl Pts',(-3.92353549711722,0.820294119899656,
10.1793309926389));
#65246=CARTESIAN_POINT('Ctrl Pts',(-3.92831996318525,-0.00248455515896013,
10.2208364779651));
#65247=CARTESIAN_POINT('Origin',(0.,0.,0.));
#65248=CARTESIAN_POINT('',(-3.92906811331088,-0.00297329045681721,11.654163522035));
#65249=CARTESIAN_POINT('',(-3.93883030069056,-0.00132569677973748,11.4708364779651));
#65250=CARTESIAN_POINT('',(-3.933,-4.81653586104654E-16,0.));
#65251=CARTESIAN_POINT('Ctrl Pts',(-3.92906811331088,-0.00297329045681721,
11.654163522035));
#65252=CARTESIAN_POINT('Ctrl Pts',(-3.92301413618412,0.862565781599686,
11.6104796717927));
#65253=CARTESIAN_POINT('Ctrl Pts',(-3.64143222706962,1.73168447743578,11.5667958215504));
#65254=CARTESIAN_POINT('Ctrl Pts',(-3.11523612143517,2.41145147056757,11.5231119713081));
#65255=CARTESIAN_POINT('Ctrl Pts',(-2.31667120836259,3.44307839438409,11.4568165546414));
#65256=CARTESIAN_POINT('Ctrl Pts',(-0.954719260784739,4.0385969656079,11.3905211379748));
#65257=CARTESIAN_POINT('Ctrl Pts',(0.344864347868389,3.92439331219059,11.3242257213081));
#65258=CARTESIAN_POINT('Ctrl Pts',(1.64444795652151,3.81018965877329,11.2579303046414));
#65259=CARTESIAN_POINT('Ctrl Pts',(2.88166322624992,2.98626378071489,11.1916348879748));
#65260=CARTESIAN_POINT('Ctrl Pts',(3.48806565025659,1.8311723858493,11.1253394713081));
#65261=CARTESIAN_POINT('Ctrl Pts',(4.09446807426328,0.676080990983685,11.0590440546414));
#65262=CARTESIAN_POINT('Ctrl Pts',(4.07005765254821,-0.810175920689126,
10.9927486379747));
#65263=CARTESIAN_POINT('Ctrl Pts',(3.42604987078477,-1.94473046206733,10.9264532213081));
#65264=CARTESIAN_POINT('Ctrl Pts',(2.78204208902133,-3.07928500344552,10.8601578046414));
#65265=CARTESIAN_POINT('Ctrl Pts',(1.51843694720952,-3.86213717452911,10.7938623879748));
#65266=CARTESIAN_POINT('Ctrl Pts',(0.215803905812841,-3.9336017797221,10.7275669713081));
#65267=CARTESIAN_POINT('Ctrl Pts',(-1.08682913558383,-4.00506638491508,
10.6612715546414));
#65268=CARTESIAN_POINT('Ctrl Pts',(-2.42849007656536,-3.36514342421749,
10.5949761379748));
#65269=CARTESIAN_POINT('Ctrl Pts',(-3.19274634428412,-2.30784858001068,
10.5286807213081));
#65270=CARTESIAN_POINT('Ctrl Pts',(-3.67122612849879,-1.64590542000571,
10.487174988217));
#65271=CARTESIAN_POINT('Ctrl Pts',(-3.92338251028428,-0.820366381532528,
10.445669255126));
#65272=CARTESIAN_POINT('Ctrl Pts',(-3.92814797210457,0.00249985979813405,
10.404163522035));
#65273=CARTESIAN_POINT('Ctrl Pts',(-3.92831996318525,-0.00248455515896013,
10.2208364779651));
#65274=CARTESIAN_POINT('Ctrl Pts',(-3.93114225616083,-0.487830765593514,
10.2453200123905));
#65275=CARTESIAN_POINT('Ctrl Pts',(-3.84781252523088,-0.972242192165111,
10.2698035468159));
#65276=CARTESIAN_POINT('Ctrl Pts',(-3.67392952307573,-1.42161434311076,
10.2942870812413));
#65277=CARTESIAN_POINT('Ctrl Pts',(-3.20527296947916,-2.63278047743221,
10.3602761009928));
#65278=CARTESIAN_POINT('Ctrl Pts',(-2.07880823084118,-3.58941000592143,
10.4262651207444));
#65279=CARTESIAN_POINT('Ctrl Pts',(-0.807722698804678,-3.85568794418083,
10.4922541404959));
#65280=CARTESIAN_POINT('Ctrl Pts',(0.463362833231834,-4.12196588244023,
10.5582431602475));
#65281=CARTESIAN_POINT('Ctrl Pts',(1.87906915866685,-3.69789223046981,10.624232179999));
#65282=CARTESIAN_POINT('Ctrl Pts',(2.79443810742862,-2.77666367153396,10.6902211997506));
#65283=CARTESIAN_POINT('Ctrl Pts',(3.70980705619038,-1.85543511259812,10.7562102195021));
#65284=CARTESIAN_POINT('Ctrl Pts',(4.12483862827887,-0.437051646696854,
10.8221992392537));
#65285=CARTESIAN_POINT('Ctrl Pts',(3.85045547167055,0.832308922064393,10.8881882590052));
#65286=CARTESIAN_POINT('Ctrl Pts',(3.57607231506224,2.10166949082563,10.9541772787568));
#65287=CARTESIAN_POINT('Ctrl Pts',(2.61227442975715,3.22200716244686,11.0201662985083));
#65288=CARTESIAN_POINT('Ctrl Pts',(1.39814251297149,3.68292587415053,11.0861553182599));
#65289=CARTESIAN_POINT('Ctrl Pts',(0.184010596185846,4.1438445858542,11.1521443380114));
#65290=CARTESIAN_POINT('Ctrl Pts',(-1.28045535208038,3.94534433764033,11.2181333577629));
#65291=CARTESIAN_POINT('Ctrl Pts',(-2.32808357370425,3.17785656613293,11.2841223775145));
#65292=CARTESIAN_POINT('Ctrl Pts',(-3.31616190220804,2.45399478123114,11.346360410998));
#65293=CARTESIAN_POINT('Ctrl Pts',(-3.9334439337259,1.22399246925214,11.4085984444815));
#65294=CARTESIAN_POINT('Ctrl Pts',(-3.93883030069056,-0.00132569677973748,
11.4708364779651));
#65295=CARTESIAN_POINT('Origin',(0.,0.,0.));
#65296=CARTESIAN_POINT('',(-3.93896652246607,-0.00134093135676028,12.904163522035));
#65297=CARTESIAN_POINT('',(-3.93205478066481,0.0035322142048073,12.7208364779651));
#65298=CARTESIAN_POINT('',(-3.933,-4.81653586104654E-16,0.));
#65299=CARTESIAN_POINT('Ctrl Pts',(-3.93896652246607,-0.00134093135676028,
12.904163522035));
#65300=CARTESIAN_POINT('Ctrl Pts',(-3.93353066281598,1.23055890227001,12.841585505126));
#65301=CARTESIAN_POINT('Ctrl Pts',(-3.30894493164482,2.46720899017099,12.779007488217));
#65302=CARTESIAN_POINT('Ctrl Pts',(-2.31183883771011,3.18985822187321,12.7164294713081));
#65303=CARTESIAN_POINT('Ctrl Pts',(-1.25550041052026,3.95543588454092,12.6501340546414));
#65304=CARTESIAN_POINT('Ctrl Pts',(0.218931533905592,4.14413118771503,12.5838386379748));
#65305=CARTESIAN_POINT('Ctrl Pts',(1.43402214654648,3.66924716671025,12.5175432213081));
#65306=CARTESIAN_POINT('Ctrl Pts',(2.6491127591874,3.19436314570546,12.4512478046414));
#65307=CARTESIAN_POINT('Ctrl Pts',(3.60486204004333,2.05589980052175,12.3849523879747));
#65308=CARTESIAN_POINT('Ctrl Pts',(3.86214638478224,0.776929591218173,12.3186569713081));
#65309=CARTESIAN_POINT('Ctrl Pts',(4.11943072952114,-0.502040618085386,
12.2523615546414));
#65310=CARTESIAN_POINT('Ctrl Pts',(3.67825013814305,-1.92151769150881,12.1860661379748));
#65311=CARTESIAN_POINT('Ctrl Pts',(2.74130715547621,-2.82931605985119,12.1197707213081));
#65312=CARTESIAN_POINT('Ctrl Pts',(1.80436417280937,-3.73711442819359,12.0534753046414));
#65313=CARTESIAN_POINT('Ctrl Pts',(0.371658798853772,-4.13323409145493,
11.9871798879748));
#65314=CARTESIAN_POINT('Ctrl Pts',(-0.898545590880796,-3.83567596497744,
11.9208844713081));
#65315=CARTESIAN_POINT('Ctrl Pts',(-2.16874998061535,-3.53811783849996,
11.8545890546414));
#65316=CARTESIAN_POINT('Ctrl Pts',(-3.27645338612888,-2.54688192228365,
11.7882936379748));
#65317=CARTESIAN_POINT('Ctrl Pts',(-3.71271614960198,-1.3173963259709,11.7219982213081));
#65318=CARTESIAN_POINT('Ctrl Pts',(-3.86151353184563,-0.898052174796522,
11.6993866548837));
#65319=CARTESIAN_POINT('Ctrl Pts',(-3.93220176350824,-0.450992274867368,
11.6767750884593));
#65320=CARTESIAN_POINT('Ctrl Pts',(-3.92906811331088,-0.00297329045681721,
11.654163522035));
#65321=CARTESIAN_POINT('Ctrl Pts',(-3.93883030069056,-0.00132569677973748,
11.4708364779651));
#65322=CARTESIAN_POINT('Ctrl Pts',(-3.93915492837218,-0.0751736536879503,
11.4745874642331));
#65323=CARTESIAN_POINT('Ctrl Pts',(-3.93725698015438,-0.149004596470233,
11.4783384505011));
#65324=CARTESIAN_POINT('Ctrl Pts',(-3.93308367658131,-0.222706699664195,
11.4820894367691));
#65325=CARTESIAN_POINT('Ctrl Pts',(-3.85966506285299,-1.51930689915301,
11.5480784565207));
#65326=CARTESIAN_POINT('Ctrl Pts',(-3.08203734041481,-2.77603200332971,
11.6140674762722));
#65327=CARTESIAN_POINT('Ctrl Pts',(-1.95446702898915,-3.42035146054613,
11.6800564960238));
#65328=CARTESIAN_POINT('Ctrl Pts',(-0.826896717563501,-4.06467091776254,
11.7460455157753));
#65329=CARTESIAN_POINT('Ctrl Pts',(0.650616182849622,-4.0965847280187,11.8120345355269));
#65330=CARTESIAN_POINT('Ctrl Pts',(1.80495606953855,-3.50155380768333,11.8780235552784));
#65331=CARTESIAN_POINT('Ctrl Pts',(2.9592959562275,-2.90652288734796,11.94401257503));
#65332=CARTESIAN_POINT('Ctrl Pts',(3.79046282919224,-1.68454723642106,12.0100015947815));
#65333=CARTESIAN_POINT('Ctrl Pts',(3.91979915488898,-0.392326479347616,
12.075990614533));
#65334=CARTESIAN_POINT('Ctrl Pts',(4.04913548058573,0.899894277725841,12.1419796342846));
#65335=CARTESIAN_POINT('Ctrl Pts',(3.47664125901443,2.26236014094584,12.2079686540361));
#65336=CARTESIAN_POINT('Ctrl Pts',(2.46312963968748,3.07436787960692,12.2739576737877));
#65337=CARTESIAN_POINT('Ctrl Pts',(1.44961802036054,3.88637561826799,12.3399466935392));
#65338=CARTESIAN_POINT('Ctrl Pts',(-0.00491099672205467,4.14792523237016,
12.4059357132908));
#65339=CARTESIAN_POINT('Ctrl Pts',(-1.23781265514471,3.73986167014628,12.4719247330423));
#65340=CARTESIAN_POINT('Ctrl Pts',(-2.47071431356738,3.33179810792238,12.5379137527939));
#65341=CARTESIAN_POINT('Ctrl Pts',(-3.48198861333012,2.25412136937241,12.6039027725454));
#65342=CARTESIAN_POINT('Ctrl Pts',(-3.81092586479075,0.997792330164229,
12.669891792297));
#65343=CARTESIAN_POINT('Ctrl Pts',(-3.89557431561527,0.674489613847985,
12.6868733541863));
#65344=CARTESIAN_POINT('Ctrl Pts',(-3.93503604178621,0.339355922885629,
12.7038549160757));
#65345=CARTESIAN_POINT('Ctrl Pts',(-3.93205478066481,0.0035322142048073,
12.7208364779651));
#65346=CARTESIAN_POINT('Origin',(0.,0.,0.));
#65347=CARTESIAN_POINT('',(-3.93316249357423,0.00362678856332621,14.154163522035));
#65348=CARTESIAN_POINT('',(-3.92715970428353,-0.00147643720250167,13.9708364779651));
#65349=CARTESIAN_POINT('',(-3.933,-4.81653586104654E-16,0.));
#65350=CARTESIAN_POINT('Ctrl Pts',(-3.93316249357423,0.00362678856332621,
14.154163522035));
#65351=CARTESIAN_POINT('Ctrl Pts',(-3.93594260249156,0.303541798933824,
14.138986755126));
#65352=CARTESIAN_POINT('Ctrl Pts',(-3.90455172321724,0.602880753633413,
14.123809988217));
#65353=CARTESIAN_POINT('Ctrl Pts',(-3.83679646632876,0.89374893743381,14.1086332213081));
#65354=CARTESIAN_POINT('Ctrl Pts',(-3.54082677701855,2.16432438711924,14.0423378046414));
#65355=CARTESIAN_POINT('Ctrl Pts',(-2.55097665652956,3.27326632209662,13.9760423879748));
#65356=CARTESIAN_POINT('Ctrl Pts',(-1.32203750399143,3.71106603622693,13.9097469713081));
#65357=CARTESIAN_POINT('Ctrl Pts',(-0.0930983514533078,4.14886575035724,
13.8434515546414));
#65358=CARTESIAN_POINT('Ctrl Pts',(1.37492983313397,3.91552324364048,13.7771561379748));
#65359=CARTESIAN_POINT('Ctrl Pts',(2.40755443900989,3.11824885318679,13.7108607213081));
#65360=CARTESIAN_POINT('Ctrl Pts',(3.44017904488582,2.32097446273309,13.6445653046414));
#65361=CARTESIAN_POINT('Ctrl Pts',(4.03740007205041,0.959768188542436,13.5782698879748));
#65362=CARTESIAN_POINT('Ctrl Pts',(3.92482144688428,-0.339957199179704,
13.5119744713081));
#65363=CARTESIAN_POINT('Ctrl Pts',(3.81224282171815,-1.63968258690184,13.4456790546414));
#65364=CARTESIAN_POINT('Ctrl Pts',(2.98986454422134,-2.87792708815543,13.3793836379748));
#65365=CARTESIAN_POINT('Ctrl Pts',(1.83553226970559,-3.48577331076856,13.3130882213081));
#65366=CARTESIAN_POINT('Ctrl Pts',(0.681199995189843,-4.09361953338168,
13.2467928046414));
#65367=CARTESIAN_POINT('Ctrl Pts',(-0.805086276344844,-4.0710674773543,
13.1804973879748));
#65368=CARTESIAN_POINT('Ctrl Pts',(-1.94044516826687,-3.42847879330567,
13.1142019713081));
#65369=CARTESIAN_POINT('Ctrl Pts',(-3.07580406018889,-2.78589010925704,
13.0479065546414));
#65370=CARTESIAN_POINT('Ctrl Pts',(-3.86023557249827,-1.52326479718716,
12.9816111379748));
#65371=CARTESIAN_POINT('Ctrl Pts',(-3.93332887367604,-0.220722130071536,
12.9153157213081));
#65372=CARTESIAN_POINT('Ctrl Pts',(-3.93742745294064,-0.147684323861175,
12.9115983215504));
#65373=CARTESIAN_POINT('Ctrl Pts',(-3.93928943559665,-0.0745210091099791,
12.9078809217927));
#65374=CARTESIAN_POINT('Ctrl Pts',(-3.93896652246607,-0.00134093135676028,
12.904163522035));
#65375=CARTESIAN_POINT('Ctrl Pts',(-3.93205478066481,0.0035322142048073,
12.7208364779651));
#65376=CARTESIAN_POINT('Ctrl Pts',(-3.92345109451774,-0.965628712188094,
12.7698439358273));
#65377=CARTESIAN_POINT('Ctrl Pts',(-3.56135912009011,-1.94053648152827,
12.8188513936894));
#65378=CARTESIAN_POINT('Ctrl Pts',(-2.91172602776107,-2.65341233514967,
12.8678588515516));
#65379=CARTESIAN_POINT('Ctrl Pts',(-2.03698873611219,-3.61330662138906,
12.9338478713032));
#65380=CARTESIAN_POINT('Ctrl Pts',(-0.640913949655874,-4.09811385400143,
12.9998368910547));
#65381=CARTESIAN_POINT('Ctrl Pts',(0.640483768856276,-3.8869687447801,13.0658259108062));
#65382=CARTESIAN_POINT('Ctrl Pts',(1.92188148736843,-3.67582363555876,13.1318149305578));
#65383=CARTESIAN_POINT('Ctrl Pts',(3.08860213793641,-2.76872618450373,13.1978039503093));
#65384=CARTESIAN_POINT('Ctrl Pts',(3.60911880551019,-1.57892587817744,13.2637929700609));
#65385=CARTESIAN_POINT('Ctrl Pts',(4.12963547308396,-0.389125571851176,
13.3297819898124));
#65386=CARTESIAN_POINT('Ctrl Pts',(4.00394815766355,1.08337758974633,13.395771009564));
#65387=CARTESIAN_POINT('Ctrl Pts',(3.28931665917947,2.16775030774074,13.4617600293155));
#65388=CARTESIAN_POINT('Ctrl Pts',(2.5746851606954,3.25212302573516,13.5277490490671));
#65389=CARTESIAN_POINT('Ctrl Pts',(1.27110947914766,3.94836530012648,13.5937380688186));
#65390=CARTESIAN_POINT('Ctrl Pts',(-0.0275359561305553,3.93928765796377,
13.6597270885702));
#65391=CARTESIAN_POINT('Ctrl Pts',(-1.32618139140878,3.93021001580106,13.7257161083217));
#65392=CARTESIAN_POINT('Ctrl Pts',(-2.61989658041747,3.21581245708433,13.7917051280733));
#65393=CARTESIAN_POINT('Ctrl Pts',(-3.31929927211619,2.12155551970592,13.8576941478248));
#65394=CARTESIAN_POINT('Ctrl Pts',(-3.71902259246606,1.49616470906661,13.8954082578716));
#65395=CARTESIAN_POINT('Ctrl Pts',(-3.92462191057852,0.746698057506936,
13.9331223679183));
#65396=CARTESIAN_POINT('Ctrl Pts',(-3.92715970428353,-0.00147643720250167,
13.9708364779651));
#65397=CARTESIAN_POINT('Origin',(0.,0.,0.));
#65398=CARTESIAN_POINT('',(-3.92651200951893,-0.000303167493754808,15.404163522035));
#65399=CARTESIAN_POINT('',(-3.937381585586,-0.00245136677763253,15.2208364779651));
#65400=CARTESIAN_POINT('',(-3.933,-4.81653586104654E-16,0.));
#65401=CARTESIAN_POINT('Ctrl Pts',(-3.92651200951893,-0.000303167493754808,
15.404163522035));
#65402=CARTESIAN_POINT('Ctrl Pts',(-3.92604892251585,0.675869111194285,
15.3700925884593));
#65403=CARTESIAN_POINT('Ctrl Pts',(-3.76041551457725,1.3522540035424,15.3360216548837));
#65404=CARTESIAN_POINT('Ctrl Pts',(-3.43090235579558,1.93615684080429,15.3019507213081));
#65405=CARTESIAN_POINT('Ctrl Pts',(-2.78973377407503,3.07231830826751,15.2356553046414));
#65406=CARTESIAN_POINT('Ctrl Pts',(-1.5280902657161,3.85832793543452,15.1693598879748));
#65407=CARTESIAN_POINT('Ctrl Pts',(-0.225640009256706,3.93304981832414,
15.1030644713081));
#65408=CARTESIAN_POINT('Ctrl Pts',(1.07681024720271,4.00777170121378,15.0367690546414));
#65409=CARTESIAN_POINT('Ctrl Pts',(2.42006725176258,3.37120583982601,14.9704736379748));
#65410=CARTESIAN_POINT('Ctrl Pts',(3.18696511248698,2.31582548111636,14.9041782213081));
#65411=CARTESIAN_POINT('Ctrl Pts',(3.95386297321136,1.26044512240672,14.8378828046414));
#65412=CARTESIAN_POINT('Ctrl Pts',(4.14440169010027,-0.213749733624791,
14.7715873879748));
#65413=CARTESIAN_POINT('Ctrl Pts',(3.67103733317019,-1.42943316936038,14.7052919713081));
#65414=CARTESIAN_POINT('Ctrl Pts',(3.1976729762401,-2.64511660509598,14.6389965546414));
#65415=CARTESIAN_POINT('Ctrl Pts',(2.06040554549099,-3.60228862053565,14.5727011379748));
#65416=CARTESIAN_POINT('Ctrl Pts',(0.781758032342482,-3.86117192909937,
14.5064057213081));
#65417=CARTESIAN_POINT('Ctrl Pts',(-0.49688948080601,-4.12005523766308,
14.4401103046414));
#65418=CARTESIAN_POINT('Ctrl Pts',(-1.9169170763539,-3.68064983935086,14.3738148879748));
#65419=CARTESIAN_POINT('Ctrl Pts',(-2.82588624506214,-2.74484265799801,
14.3075194713081));
#65420=CARTESIAN_POINT('Ctrl Pts',(-3.52676843137341,-2.02326638697389,
14.2564008215504));
#65421=CARTESIAN_POINT('Ctrl Pts',(-3.92379848245872,-1.00655215561986,
14.2052821717927));
#65422=CARTESIAN_POINT('Ctrl Pts',(-3.93316249357423,0.00362678856332621,
14.154163522035));
#65423=CARTESIAN_POINT('Ctrl Pts',(-3.92715970428353,-0.00147643720250167,
13.9708364779651));
#65424=CARTESIAN_POINT('Ctrl Pts',(-3.92906233138436,-0.562395580067438,
13.9991113876699));
#65425=CARTESIAN_POINT('Ctrl Pts',(-3.81682903223787,-1.12258843310771,
14.0273862973747));
#65426=CARTESIAN_POINT('Ctrl Pts',(-3.58669355618862,-1.6292252192563,14.0556612070795));
#65427=CARTESIAN_POINT('Ctrl Pts',(-3.0495949541736,-2.81163270479997,14.121650226831));
#65428=CARTESIAN_POINT('Ctrl Pts',(-1.87030755575485,-3.70233135984722,
14.1876392465825));
#65429=CARTESIAN_POINT('Ctrl Pts',(-0.586083352258435,-3.89554255338986,
14.2536282663341));
#65430=CARTESIAN_POINT('Ctrl Pts',(0.698140851238002,-4.08875374693251,
14.3196172860856));
#65431=CARTESIAN_POINT('Ctrl Pts',(2.08730185981211,-3.58447747897051,14.3856063058372));
#65432=CARTESIAN_POINT('Ctrl Pts',(2.94853484413587,-2.61244861269697,14.4515953255887));
#65433=CARTESIAN_POINT('Ctrl Pts',(3.8097678284596,-1.64041974642346,14.5175843453403));
#65434=CARTESIAN_POINT('Ctrl Pts',(4.14307278853302,-0.200638281838427,
14.5835733650918));
#65435=CARTESIAN_POINT('Ctrl Pts',(3.79660484433925,1.05096961754631,14.6495623848434));
#65436=CARTESIAN_POINT('Ctrl Pts',(3.45013690014547,2.30257751693109,14.7155514045949));
#65437=CARTESIAN_POINT('Ctrl Pts',(2.42389605168447,3.36601185111556,14.7815404243465));
#65438=CARTESIAN_POINT('Ctrl Pts',(1.18541035034992,3.7568002052743,14.847529444098));
#65439=CARTESIAN_POINT('Ctrl Pts',(-0.0530753509846368,4.14758855943303,
14.9135184638496));
#65440=CARTESIAN_POINT('Ctrl Pts',(-1.50380590519273,3.86573093356604,14.9795074836011));
#65441=CARTESIAN_POINT('Ctrl Pts',(-2.50586703457503,3.03963416978028,15.0454965033527));
#65442=CARTESIAN_POINT('Ctrl Pts',(-3.39339536200238,2.30795797003797,15.1039431615568));
#65443=CARTESIAN_POINT('Ctrl Pts',(-3.9289562489058,1.14934281299856,15.1623898197609));
#65444=CARTESIAN_POINT('Ctrl Pts',(-3.937381585586,-0.00245136677763253,
15.2208364779651));
#65445=CARTESIAN_POINT('Origin',(0.,0.,0.));
#65446=CARTESIAN_POINT('',(-3.93427892592546,-0.0035228168194773,16.654163522035));
#65447=CARTESIAN_POINT('',(-3.93429847074092,0.00343138669546231,16.4708364779651));
#65448=CARTESIAN_POINT('',(-3.933,-4.81653586104654E-16,0.));
#65449=CARTESIAN_POINT('Ctrl Pts',(-3.93427892592546,-0.0035228168194773,
16.654163522035));
#65450=CARTESIAN_POINT('Ctrl Pts',(-3.92458523529087,1.04238322102138,16.6011984217927));
#65451=CARTESIAN_POINT('Ctrl Pts',(-3.49510551886889,2.09531909947515,16.5482333215504));
#65452=CARTESIAN_POINT('Ctrl Pts',(-2.74837386927502,2.82245201232602,16.4952682213081));
#65453=CARTESIAN_POINT('Ctrl Pts',(-1.81370395226269,3.73259056033171,16.4289728046414));
#65454=CARTESIAN_POINT('Ctrl Pts',(-0.381993636524734,4.13229175872001,
16.3626773879748));
#65455=CARTESIAN_POINT('Ctrl Pts',(0.888950886713486,3.83791096929153,16.2963819713081));
#65456=CARTESIAN_POINT('Ctrl Pts',(2.15989540995167,3.54353017986306,16.2300865546414));
#65457=CARTESIAN_POINT('Ctrl Pts',(3.27007414069013,2.55506740261785,16.1637911379748));
#65458=CARTESIAN_POINT('Ctrl Pts',(3.70941012102833,1.32667661515893,16.0974957213081));
#65459=CARTESIAN_POINT('Ctrl Pts',(4.14874610136655,0.0982858276999579,
16.0312003046414));
#65460=CARTESIAN_POINT('Ctrl Pts',(3.91723933130444,-1.37003296997274,15.9649048879748));
#65461=CARTESIAN_POINT('Ctrl Pts',(3.1212567099161,-2.40365364351869,15.8986094713081));
#65462=CARTESIAN_POINT('Ctrl Pts',(2.32527408852779,-3.4372743170646,15.8323140546414));
#65463=CARTESIAN_POINT('Ctrl Pts',(0.964815615813289,-4.03619686648378,
15.7660186379748));
#65464=CARTESIAN_POINT('Ctrl Pts',(-0.335049519007167,-3.92524344557252,
15.6997232213081));
#65465=CARTESIAN_POINT('Ctrl Pts',(-1.63491465382764,-3.81429002466125,
15.6334278046414));
#65466=CARTESIAN_POINT('Ctrl Pts',(-2.87418645075407,-2.99346063341953,
15.5671323879748));
#65467=CARTESIAN_POINT('Ctrl Pts',(-3.48347552167619,-1.83988928391893,
15.5008369713081));
#65468=CARTESIAN_POINT('Ctrl Pts',(-3.77963514100862,-1.27916816147398,
15.468612488217));
#65469=CARTESIAN_POINT('Ctrl Pts',(-3.92694999984484,-0.639830761090415,
15.436388005126));
#65470=CARTESIAN_POINT('Ctrl Pts',(-3.92651200951893,-0.000303167493754808,
15.404163522035));
#65471=CARTESIAN_POINT('Ctrl Pts',(-3.937381585586,-0.00245136677763253,
15.2208364779651));
#65472=CARTESIAN_POINT('Ctrl Pts',(-3.93846884938094,-0.151086864494689,
15.2283788395125));
#65473=CARTESIAN_POINT('Ctrl Pts',(-3.9307776674093,-0.299608771734014,
15.2359212010599));
#65474=CARTESIAN_POINT('Ctrl Pts',(-3.91393159770783,-0.447084924292802,
15.2434635626073));
#65475=CARTESIAN_POINT('Ctrl Pts',(-3.76654332690187,-1.73737135287563,
15.3094525823588));
#65476=CARTESIAN_POINT('Ctrl Pts',(-2.91837508073346,-2.94760830833676,
15.3754416021104));
#65477=CARTESIAN_POINT('Ctrl Pts',(-1.75582976645362,-3.52644400385163,
15.4414306218619));
#65478=CARTESIAN_POINT('Ctrl Pts',(-0.593284452173774,-4.10527969936651,
15.5074196416135));
#65479=CARTESIAN_POINT('Ctrl Pts',(0.883637930217515,-4.05271413493511,
15.573408661365));
#65480=CARTESIAN_POINT('Ctrl Pts',(2.00209080232236,-3.39269478443345,15.6393976811166));
#65481=CARTESIAN_POINT('Ctrl Pts',(3.1205436744272,-2.73267543393178,15.7053867008681));
#65482=CARTESIAN_POINT('Ctrl Pts',(3.88052703624564,-1.46520229735984,15.7713757206197));
#65483=CARTESIAN_POINT('Ctrl Pts',(3.93581266973757,-0.167702444224742,
15.8373647403712));
#65484=CARTESIAN_POINT('Ctrl Pts',(3.99109830322949,1.12979740891036,15.9033537601228));
#65485=CARTESIAN_POINT('Ctrl Pts',(3.34168620839496,2.45732397860861,15.9693427798743));
#65486=CARTESIAN_POINT('Ctrl Pts',(2.28343127320179,3.21009144754939,16.0353317996259));
#65487=CARTESIAN_POINT('Ctrl Pts',(1.22517633800864,3.96285891649017,16.1013208193774));
#65488=CARTESIAN_POINT('Ctrl Pts',(-0.241921437543155,4.14086728467346,
16.167309839129));
#65489=CARTESIAN_POINT('Ctrl Pts',(-1.44949130477761,3.66302067130938,16.2332988588805));
#65490=CARTESIAN_POINT('Ctrl Pts',(-2.65706117201209,3.18517405794529,16.299287878632));
#65491=CARTESIAN_POINT('Ctrl Pts',(-3.60510313092923,2.05147246303385,16.3652768983836));
#65492=CARTESIAN_POINT('Ctrl Pts',(-3.86171446555683,0.778400197568591,
16.4312659181351));
#65493=CARTESIAN_POINT('Ctrl Pts',(-3.91300711095021,0.523932699601581,
16.4444561047451));
#65494=CARTESIAN_POINT('Ctrl Pts',(-3.93667444784825,0.26389680817035,16.4576462913551));
#65495=CARTESIAN_POINT('Ctrl Pts',(-3.93429847074092,0.00343138669546231,
16.4708364779651));
#65496=CARTESIAN_POINT('Origin',(0.,0.,0.));
#65497=CARTESIAN_POINT('',(-3.93834707504816,0.00194035199596952,17.904163522035));
#65498=CARTESIAN_POINT('',(-3.9266456040214,-0.000298839343342066,17.7208364779651));
#65499=CARTESIAN_POINT('',(-3.933,-4.81653586104654E-16,0.));
#65500=CARTESIAN_POINT('Ctrl Pts',(-3.93834707504816,0.00194035199596952,
17.904163522035));
#65501=CARTESIAN_POINT('Ctrl Pts',(-3.93900955662444,0.111515013993062,
17.8985996717927));
#65502=CARTESIAN_POINT('Ctrl Pts',(-3.93483467582154,0.221038430779974,
17.8930358215504));
#65503=CARTESIAN_POINT('Ctrl Pts',(-3.92565930759555,0.330141315023366,
17.8874719713081));
#65504=CARTESIAN_POINT('Ctrl Pts',(-3.81633126440203,1.63014416475303,17.8211765546414));
#65505=CARTESIAN_POINT('Ctrl Pts',(-2.99705204268746,2.87044131989379,17.7548811379748));
#65506=CARTESIAN_POINT('Ctrl Pts',(-1.84424342167773,3.48117228657177,17.6885857213081));
#65507=CARTESIAN_POINT('Ctrl Pts',(-0.691434800668018,4.09190325324974,
17.6222903046414));
#65508=CARTESIAN_POINT('Ctrl Pts',(0.794903219636835,4.07306803146494,17.5559948879748));
#65509=CARTESIAN_POINT('Ctrl Pts',(1.93186548638391,3.43332055446555,17.4896994713081));
#65510=CARTESIAN_POINT('Ctrl Pts',(3.06882775313098,2.79357307746616,17.4234040546414));
#65511=CARTESIAN_POINT('Ctrl Pts',(3.85641426632028,1.53291334525214,17.3571086379748));
#65512=CARTESIAN_POINT('Ctrl Pts',(3.93276461410269,0.230557535679648,17.2908132213081));
#65513=CARTESIAN_POINT('Ctrl Pts',(4.0091149618851,-1.07179827389284,17.2245178046414));
#65514=CARTESIAN_POINT('Ctrl Pts',(3.37422914426067,-2.41585016082385,17.1582223879748));
#65515=CARTESIAN_POINT('Ctrl Pts',(2.31980850399665,-3.18406702064856,17.0919269713081));
#65516=CARTESIAN_POINT('Ctrl Pts',(1.26538786373261,-3.95228388047328,17.0256315546414));
#65517=CARTESIAN_POINT('Ctrl Pts',(-0.208567599171001,-4.14466571319169,
16.9593361379748));
#65518=CARTESIAN_POINT('Ctrl Pts',(-1.42484195742051,-3.67282176038683,
16.8930407213081));
#65519=CARTESIAN_POINT('Ctrl Pts',(-2.64111631566999,-3.20097780758199,
16.8267453046414));
#65520=CARTESIAN_POINT('Ctrl Pts',(-3.59970956926536,-2.06490806925393,
16.7604498879748));
#65521=CARTESIAN_POINT('Ctrl Pts',(-3.86019143691972,-0.78658525127837,
16.6941544713081));
#65522=CARTESIAN_POINT('Ctrl Pts',(-3.9125676929753,-0.52954715554103,16.6808241548837));
#65523=CARTESIAN_POINT('Ctrl Pts',(-3.93671864496475,-0.266757633157094,
16.6674938384594));
#65524=CARTESIAN_POINT('Ctrl Pts',(-3.93427892592546,-0.0035228168194773,
16.654163522035));
#65525=CARTESIAN_POINT('Ctrl Pts',(-3.93429847074092,0.00343138669546231,
16.4708364779651));
#65526=CARTESIAN_POINT('Ctrl Pts',(-3.92478770167089,-1.03918239385564,
16.5236353111066));
#65527=CARTESIAN_POINT('Ctrl Pts',(-3.4979820902233,-2.08867858084047,16.5764341442482));
#65528=CARTESIAN_POINT('Ctrl Pts',(-2.75534870673093,-2.8154571538885,16.6292329773898));
#65529=CARTESIAN_POINT('Ctrl Pts',(-1.82719090293942,-3.72379930386122,
16.6952219971413));
#65530=CARTESIAN_POINT('Ctrl Pts',(-0.405694585018322,-4.12804066778764,
16.7612110168929));
#65531=CARTESIAN_POINT('Ctrl Pts',(0.861544310291354,-3.84401962566144,
16.8272000366444));
#65532=CARTESIAN_POINT('Ctrl Pts',(2.12878320560107,-3.55999858353522,16.893189056396));
#65533=CARTESIAN_POINT('Ctrl Pts',(3.24176467829938,-2.58771513535637,16.9591780761475));
#65534=CARTESIAN_POINT('Ctrl Pts',(3.69344395429821,-1.37011577522619,17.0251670958991));
#65535=CARTESIAN_POINT('Ctrl Pts',(4.14512323029704,-0.152516415096028,
17.0911561156506));
#65536=CARTESIAN_POINT('Ctrl Pts',(3.93550030959638,1.31039885698542,17.1571451354021));
#65537=CARTESIAN_POINT('Ctrl Pts',(3.16007382274637,2.35216472974554,17.2231341551537));
#65538=CARTESIAN_POINT('Ctrl Pts',(2.38464733589636,3.39393060250563,17.2891231749052));
#65539=CARTESIAN_POINT('Ctrl Pts',(1.04341728289697,4.0145470759444,17.3551121946568));
#65540=CARTESIAN_POINT('Ctrl Pts',(-0.252587576200152,3.93127778176702,
17.4211012144083));
#65541=CARTESIAN_POINT('Ctrl Pts',(-1.5485924352973,3.84800848758964,17.4870902341599));
#65542=CARTESIAN_POINT('Ctrl Pts',(-2.79937210049219,3.06085342579612,17.5530792539114));
#65543=CARTESIAN_POINT('Ctrl Pts',(-3.43510460409732,1.92841951866681,17.619068273663));
#65544=CARTESIAN_POINT('Ctrl Pts',(-3.76191329414888,1.34627334923204,17.6529910084304));
#65545=CARTESIAN_POINT('Ctrl Pts',(-3.92618702824121,0.672882336433972,
17.6869137431977));
#65546=CARTESIAN_POINT('Ctrl Pts',(-3.9266456040214,-0.000298839343342066,
17.7208364779651));
#65547=CARTESIAN_POINT('Origin',(0.,0.,0.));
#65548=CARTESIAN_POINT('',(-3.9282768393018,0.00257866899793263,19.154163522035));
#65549=CARTESIAN_POINT('',(-3.93538156611592,-0.00321517502500232,18.9708364779651));
#65550=CARTESIAN_POINT('',(-3.933,-4.81653586104654E-16,0.));
#65551=CARTESIAN_POINT('Ctrl Pts',(-3.9282768393018,0.00257866899793263,
19.154163522035));
#65552=CARTESIAN_POINT('Ctrl Pts',(-3.93117933039081,0.487427862220609,
19.129705505126));
#65553=CARTESIAN_POINT('Ctrl Pts',(-3.84811414897009,0.971317557029167,
19.1052474882171));
#65554=CARTESIAN_POINT('Ctrl Pts',(-3.67460044557047,1.42024851790461,19.0807894713081));
#65555=CARTESIAN_POINT('Ctrl Pts',(-3.20427763456445,2.63711189716341,19.0144940546414));
#65556=CARTESIAN_POINT('Ctrl Pts',(-2.06940736477127,3.5971248902646,18.9481986379748));
#65557=CARTESIAN_POINT('Ctrl Pts',(-0.791411240478813,3.8592049097762,18.8819032213081));
#65558=CARTESIAN_POINT('Ctrl Pts',(0.48658488381363,4.1212849292878,18.8156078046414));
#65559=CARTESIAN_POINT('Ctrl Pts',(1.90770686260538,3.68543197520983,18.7493123879748));
#65560=CARTESIAN_POINT('Ctrl Pts',(2.81901336701189,2.75190078378659,18.6830169713081));
#65561=CARTESIAN_POINT('Ctrl Pts',(3.7303198714184,1.81836959236335,18.6167215546414));
#65562=CARTESIAN_POINT('Ctrl Pts',(4.1318109014397,0.387160163594836,18.5504261379748));
#65563=CARTESIAN_POINT('Ctrl Pts',(3.83901947212335,-0.884151446221029,
18.4841307213081));
#65564=CARTESIAN_POINT('Ctrl Pts',(3.546228042807,-2.15546305603691,18.4178353046414));
#65565=CARTESIAN_POINT('Ctrl Pts',(2.55915415415299,-3.26687684690014,18.3515398879748));
#65566=CARTESIAN_POINT('Ctrl Pts',(1.33131365222046,-3.70774840659508,18.2852444713081));
#65567=CARTESIAN_POINT('Ctrl Pts',(0.103473150287937,-4.14861996629002,
18.2189490546414));
#65568=CARTESIAN_POINT('Ctrl Pts',(-1.36513396492305,-3.91894929481668,
18.1526536379748));
#65569=CARTESIAN_POINT('Ctrl Pts',(-2.39974909019232,-3.12425968692074,
18.0863582213081));
#65570=CARTESIAN_POINT('Ctrl Pts',(-3.34753402561069,-2.39626449305453,
18.0256266548837));
#65571=CARTESIAN_POINT('Ctrl Pts',(-3.93111583371302,-1.1941092492171,17.9648950884594));
#65572=CARTESIAN_POINT('Ctrl Pts',(-3.93834707504816,0.00194035199596952,
17.904163522035));
#65573=CARTESIAN_POINT('Ctrl Pts',(-3.9266456040214,-0.000298839343342066,
17.7208364779651));
#65574=CARTESIAN_POINT('Ctrl Pts',(-3.92707908386185,-0.636639617187392,
17.7529027629493));
#65575=CARTESIAN_POINT('Ctrl Pts',(-3.7811366333853,-1.2727928965762,17.7849690479334));
#65576=CARTESIAN_POINT('Ctrl Pts',(-3.48773693817145,-1.83151208873438,
17.8170353329176));
#65577=CARTESIAN_POINT('Ctrl Pts',(-2.88395142662511,-2.98129703654113,
17.8830243526692));
#65578=CARTESIAN_POINT('Ctrl Pts',(-1.65569506151712,-3.80315417968951,
17.9490133724207));
#65579=CARTESIAN_POINT('Ctrl Pts',(-0.362528793721696,-3.92266725007212,
18.0150023921723));
#65580=CARTESIAN_POINT('Ctrl Pts',(0.930637474073712,-4.04218032045474,
18.0809914119238));
#65581=CARTESIAN_POINT('Ctrl Pts',(2.28871364455655,-3.45934931807162,18.1469804316753));
#65582=CARTESIAN_POINT('Ctrl Pts',(3.0929963143472,-2.4396965550044,18.2129694514269));
#65583=CARTESIAN_POINT('Ctrl Pts',(3.89727898413784,-1.4200437919372,18.2789584711784));
#65584=CARTESIAN_POINT('Ctrl Pts',(4.1477681532363,0.0364307318140862,18.34494749093));
#65585=CARTESIAN_POINT('Ctrl Pts',(3.73034761461436,1.26619593871039,18.4109365106815));
#65586=CARTESIAN_POINT('Ctrl Pts',(3.3129270759924,2.49596114560672,18.4769255304331));
#65587=CARTESIAN_POINT('Ctrl Pts',(2.22759682964998,3.49901703564806,18.5429145501846));
#65588=CARTESIAN_POINT('Ctrl Pts',(0.96880448596242,3.8183980082025,18.6089035699362));
#65589=CARTESIAN_POINT('Ctrl Pts',(-0.289987857725137,4.13777898075694,
18.6748925896877));
#65590=CARTESIAN_POINT('Ctrl Pts',(-1.72224229875783,3.77348503582448,18.7408816094393));
#65591=CARTESIAN_POINT('Ctrl Pts',(-2.67546178547362,2.89147881118572,18.8068706291908));
#65592=CARTESIAN_POINT('Ctrl Pts',(-3.46496405315379,2.16095879542366,18.8615259121156));
#65593=CARTESIAN_POINT('Ctrl Pts',(-3.92585074558825,1.07529075325076,18.9161811950403));
#65594=CARTESIAN_POINT('Ctrl Pts',(-3.93538156611592,-0.00321517502500232,
18.9708364779651));
#65595=CARTESIAN_POINT('Origin',(0.,0.,0.));
#65596=CARTESIAN_POINT('',(-3.92891717919508,-0.00290821770756955,20.404163522035));
#65597=CARTESIAN_POINT('',(-3.93645074190752,0.00287690968989754,20.2208364779651));
#65598=CARTESIAN_POINT('',(-3.933,-4.81653586104654E-16,0.));
#65599=CARTESIAN_POINT('Ctrl Pts',(-3.92891717919508,-0.00290821770756955,
20.404163522035));
#65600=CARTESIAN_POINT('Ctrl Pts',(-3.92305522360385,0.856142276174852,
20.3608113384593));
#65601=CARTESIAN_POINT('Ctrl Pts',(-3.64607827536016,1.71863158079485,20.3174591548837));
#65602=CARTESIAN_POINT('Ctrl Pts',(-3.12725777950586,2.39584078513516,20.2741069713081));
#65603=CARTESIAN_POINT('Ctrl Pts',(-2.33386242750779,3.43144874462641,20.2078115546414));
#65604=CARTESIAN_POINT('Ctrl Pts',(-0.974905937332626,4.03377152685725,
20.1415161379748));
#65605=CARTESIAN_POINT('Ctrl Pts',(0.325232594901768,3.92606903230323,20.0752207213081));
#65606=CARTESIAN_POINT('Ctrl Pts',(1.62537112713614,3.8183665377492,20.0089253046414));
#65607=CARTESIAN_POINT('Ctrl Pts',(2.86669170142975,3.00063876641033,19.9426298879748));
#65608=CARTESIAN_POINT('Ctrl Pts',(3.47886360905618,1.84859467617474,19.8763344713081));
#65609=CARTESIAN_POINT('Ctrl Pts',(4.09103551668261,0.696550585939142,19.8100390546414));
#65610=CARTESIAN_POINT('Ctrl Pts',(4.07405875764185,-0.789809823193177,
19.7437436379748));
#65611=CARTESIAN_POINT('Ctrl Pts',(3.43573338553496,-1.92757111171479,19.6774482213081));
#65612=CARTESIAN_POINT('Ctrl Pts',(2.79740801342808,-3.06533240023639,19.6111528046414));
#65613=CARTESIAN_POINT('Ctrl Pts',(1.5377340282551,-3.8544945681473,19.5448573879748));
#65614=CARTESIAN_POINT('Ctrl Pts',(0.23547470165254,-3.93247326145755,19.4785619713081));
#65615=CARTESIAN_POINT('Ctrl Pts',(-1.06678462495002,-4.01045195476781,
19.4122665546415));
#65616=CARTESIAN_POINT('Ctrl Pts',(-2.41162929298214,-3.37724717347741,
19.3459711379748));
#65617=CARTESIAN_POINT('Ctrl Pts',(-3.18116395088876,-2.32378790012402,
19.2796757213081));
#65618=CARTESIAN_POINT('Ctrl Pts',(-3.66679826362155,-1.65897577639373,
19.2378383215504));
#65619=CARTESIAN_POINT('Ctrl Pts',(-3.92331189547844,-0.82679476690109,
19.1960009217927));
#65620=CARTESIAN_POINT('Ctrl Pts',(-3.9282768393018,0.00257866899793263,
19.154163522035));
#65621=CARTESIAN_POINT('Ctrl Pts',(-3.93538156611592,-0.00321517502500232,
18.9708364779651));
#65622=CARTESIAN_POINT('Ctrl Pts',(-3.93735794983994,-0.226862400015945,
18.9821702147919));
#65623=CARTESIAN_POINT('Ctrl Pts',(-3.91992542781245,-0.450201644536789,
18.9935039516187));
#65624=CARTESIAN_POINT('Ctrl Pts',(-3.88198951431208,-0.670002158083677,
19.0048376884455));
#65625=CARTESIAN_POINT('Ctrl Pts',(-3.66111322403586,-1.94975839836931,
19.070826708197));
#65626=CARTESIAN_POINT('Ctrl Pts',(-2.74517611108449,-3.10955237459557,
19.1368157279486));
#65627=CARTESIAN_POINT('Ctrl Pts',(-1.55145477700773,-3.62101278042009,
19.2028047477001));
#65628=CARTESIAN_POINT('Ctrl Pts',(-0.357733442930951,-4.13247318624461,
19.2687937674516));
#65629=CARTESIAN_POINT('Ctrl Pts',(1.11377211227119,-3.99560002166745,19.3347827872032));
#65630=CARTESIAN_POINT('Ctrl Pts',(2.19268307268018,-3.27274906215669,19.4007718069548));
#65631=CARTESIAN_POINT('Ctrl Pts',(3.27159403308916,-2.54989810264594,19.4667608267063));
#65632=CARTESIAN_POINT('Ctrl Pts',(3.9579103987049,-1.24106934820161,19.5327498464579));
#65633=CARTESIAN_POINT('Ctrl Pts',(3.93896467676769,0.0574696114667197,
19.5987388662094));
#65634=CARTESIAN_POINT('Ctrl Pts',(3.92001895483048,1.35600857113501,19.6647278859609));
#65635=CARTESIAN_POINT('Ctrl Pts',(3.19581114534032,2.64425773602735,19.7307169057125));
#65636=CARTESIAN_POINT('Ctrl Pts',(2.09627107566941,3.33532503039472,19.796705925464));
#65637=CARTESIAN_POINT('Ctrl Pts',(0.996731005998481,4.0263923247621,19.8626949452156));
#65638=CARTESIAN_POINT('Ctrl Pts',(-0.47814132385321,4.12027774860455,19.9286839649671));
#65639=CARTESIAN_POINT('Ctrl Pts',(-1.65643328493112,3.57420959844803,19.9946729847187));
#65640=CARTESIAN_POINT('Ctrl Pts',(-2.83472524600906,3.02814144829149,20.0606620044702));
#65641=CARTESIAN_POINT('Ctrl Pts',(-3.71643683831319,1.84211972413594,20.1266510242218));
#65642=CARTESIAN_POINT('Ctrl Pts',(-3.89988369773019,0.556464397103722,
20.1926400439733));
#65643=CARTESIAN_POINT('Ctrl Pts',(-3.92601202070485,0.373348601469244,
20.2020388553039));
#65644=CARTESIAN_POINT('Ctrl Pts',(-3.93797514673285,0.188211610232611,
20.2114376666345));
#65645=CARTESIAN_POINT('Ctrl Pts',(-3.93645074190752,0.00287690968989754,
20.2208364779651));
#65646=CARTESIAN_POINT('Origin',(0.,0.,0.));
#65647=CARTESIAN_POINT('',(-3.93886994768263,-0.00145307456529742,21.654163522035));
#65648=CARTESIAN_POINT('',(-3.92682300552281,0.000912804021836195,21.4708364779651));
#65649=CARTESIAN_POINT('',(-3.933,-4.81653586104654E-16,0.));
#65650=CARTESIAN_POINT('Ctrl Pts',(-3.93886994768263,-0.00145307456529742,
21.654163522035));
#65651=CARTESIAN_POINT('Ctrl Pts',(-3.93307041227624,1.22399755147868,21.5919171717927));
#65652=CARTESIAN_POINT('Ctrl Pts',(-3.31597754125522,2.45448525381708,21.5296708215504));
#65653=CARTESIAN_POINT('Ctrl Pts',(-2.3277636632771,3.17825590774622,21.4674244713081));
#65654=CARTESIAN_POINT('Ctrl Pts',(-1.27526740379634,3.94910716065609,21.4011290546414));
#65655=CARTESIAN_POINT('Ctrl Pts',(0.198202360151425,4.14517431985207,21.3348336379748));
#65656=CARTESIAN_POINT('Ctrl Pts',(1.41565285799402,3.67637338594032,21.2685382213081));
#65657=CARTESIAN_POINT('Ctrl Pts',(2.63310335583664,3.20757245202857,21.2022428046414));
#65658=CARTESIAN_POINT('Ctrl Pts',(3.59453458757408,2.07390342500907,21.1359473879748));
#65659=CARTESIAN_POINT('Ctrl Pts',(3.85821234921109,0.796235992399213,21.0696519713081));
#65660=CARTESIAN_POINT('Ctrl Pts',(4.1218901108481,-0.481431440210624,21.0033565546414));
#65661=CARTESIAN_POINT('Ctrl Pts',(3.6878144023847,-1.90309727841081,20.9370611379748));
#65662=CARTESIAN_POINT('Ctrl Pts',(2.75542339601885,-2.81557031449561,20.8707657213081));
#65663=CARTESIAN_POINT('Ctrl Pts',(1.823032389653,-3.72804335058041,20.8044703046414));
#65664=CARTESIAN_POINT('Ctrl Pts',(0.392326085384676,-4.13132358454981,
20.7381748879748));
#65665=CARTESIAN_POINT('Ctrl Pts',(-0.879350623459857,-3.84012197309118,
20.6718794713081));
#65666=CARTESIAN_POINT('Ctrl Pts',(-2.15102733230437,-3.54892036163256,
20.6055840546414));
#65667=CARTESIAN_POINT('Ctrl Pts',(-3.26367444572511,-2.56323690474595,
20.5392886379748));
#65668=CARTESIAN_POINT('Ctrl Pts',(-3.70608089552499,-1.33594860792683,
20.4729932213081));
#65669=CARTESIAN_POINT('Ctrl Pts',(-3.85918701973527,-0.91121394481419,
20.4500499882171));
#65670=CARTESIAN_POINT('Ctrl Pts',(-3.93201949613523,-0.457542658063658,
20.427106755126));
#65671=CARTESIAN_POINT('Ctrl Pts',(-3.92891717919508,-0.00290821770756955,
20.404163522035));
#65672=CARTESIAN_POINT('Ctrl Pts',(-3.93645074190752,0.00287690968989754,
20.2208364779651));
#65673=CARTESIAN_POINT('Ctrl Pts',(-3.92727230606611,-1.11302263999166,
20.277426686386));
#65674=CARTESIAN_POINT('Ctrl Pts',(-3.42913855164522,-2.23608962586235,
20.334016894807));
#65675=CARTESIAN_POINT('Ctrl Pts',(-2.58996741576936,-2.96830157940845,
20.390607103228));
#65676=CARTESIAN_POINT('Ctrl Pts',(-1.61142214786158,-3.82212329897966,
20.4565961229795));
#65677=CARTESIAN_POINT('Ctrl Pts',(-0.169149485516115,-4.14447780821319,
20.522585142731));
#65678=CARTESIAN_POINT('Ctrl Pts',(1.0797894842757,-3.78850896141388,20.5885741624826));
#65679=CARTESIAN_POINT('Ctrl Pts',(2.32872845406747,-3.43254011461459,20.6545631822341));
#65680=CARTESIAN_POINT('Ctrl Pts',(3.3843337313056,-2.39824791178247,20.7205522019857));
#65681=CARTESIAN_POINT('Ctrl Pts',(3.7656996114002,-1.15682838734449,20.7865412217372));
#65682=CARTESIAN_POINT('Ctrl Pts',(4.14706549149481,0.0845911370935058,
20.8525302414888));
#65683=CARTESIAN_POINT('Ctrl Pts',(3.85419197444593,1.53313798313737,20.9185192612403));
#65684=CARTESIAN_POINT('Ctrl Pts',(3.0205044495625,2.52889271248087,20.9845082809919));
#65685=CARTESIAN_POINT('Ctrl Pts',(2.18681692467907,3.52464744182437,21.0504973007434));
#65686=CARTESIAN_POINT('Ctrl Pts',(0.812315391961076,4.06761005446749,21.116486320495));
#65687=CARTESIAN_POINT('Ctrl Pts',(-0.476813786790554,3.91042121692691,
21.1824753402465));
#65688=CARTESIAN_POINT('Ctrl Pts',(-1.76594296554219,3.75323237938633,21.2484643599981));
#65689=CARTESIAN_POINT('Ctrl Pts',(-2.96969979032745,2.89589209166208,21.3144533797496));
#65690=CARTESIAN_POINT('Ctrl Pts',(-3.53968464960523,1.72898179933011,21.3804423995011));
#65691=CARTESIAN_POINT('Ctrl Pts',(-3.79994641379366,1.19615688935483,21.4105737589891));
#65692=CARTESIAN_POINT('Ctrl Pts',(-3.92807036204732,0.598788410850091,
21.4407051184771));
#65693=CARTESIAN_POINT('Ctrl Pts',(-3.92682300552281,0.000912804021836195,
21.4708364779651));
#65694=CARTESIAN_POINT('Origin',(0.,0.,0.));
#65695=CARTESIAN_POINT('',(-3.93336305982959,0.00361627372896939,22.904163522035));
#65696=CARTESIAN_POINT('',(-3.93314739898817,-0.00354003882696159,22.7208364779651));
#65697=CARTESIAN_POINT('',(-3.933,-4.81653586104654E-16,0.));
#65698=CARTESIAN_POINT('Ctrl Pts',(-3.93336305982959,0.00361627372896939,
22.904163522035));
#65699=CARTESIAN_POINT('Ctrl Pts',(-3.93608756649877,0.296938794665777,
22.8893184217927));
#65700=CARTESIAN_POINT('Ctrl Pts',(-3.90606924847603,0.589708845978146,
22.8744733215504));
#65701=CARTESIAN_POINT('Ctrl Pts',(-3.84121847047142,0.874548425935453,
22.8596282213081));
#65702=CARTESIAN_POINT('Ctrl Pts',(-3.55160713213065,2.14658824568881,22.7933328046414));
#65703=CARTESIAN_POINT('Ctrl Pts',(-2.56731564801377,3.26046694217167,22.7270373879748));
#65704=CARTESIAN_POINT('Ctrl Pts',(-1.34058147503169,3.70440759042506,22.6607419713081));
#65705=CARTESIAN_POINT('Ctrl Pts',(-0.113847302049577,4.14834823867847,
22.5944465546415));
#65706=CARTESIAN_POINT('Ctrl Pts',(1.35532955979775,3.92235083870236,22.5281511379748));
#65707=CARTESIAN_POINT('Ctrl Pts',(2.39192873445742,3.13025098298425,22.4618557213081));
#65708=CARTESIAN_POINT('Ctrl Pts',(3.42852790911707,2.33815112726615,22.3955603046414));
#65709=CARTESIAN_POINT('Ctrl Pts',(4.03254939658908,0.979948815806054,22.3292648879748));
#65710=CARTESIAN_POINT('Ctrl Pts',(3.926472619055,-0.320323366316481,22.2629694713081));
#65711=CARTESIAN_POINT('Ctrl Pts',(3.82039584152092,-1.62059554843902,22.1966740546414));
#65712=CARTESIAN_POINT('Ctrl Pts',(3.00422079898074,-2.86293760122399,22.1303786379748));
#65713=CARTESIAN_POINT('Ctrl Pts',(1.85294304060728,-3.47654949273874,22.0640832213081));
#65714=CARTESIAN_POINT('Ctrl Pts',(0.701665282233811,-4.09016138425349,
21.9977878046415));
#65715=CARTESIAN_POINT('Ctrl Pts',(-0.784715191972952,-4.075043114498,21.9314923879748));
#65716=CARTESIAN_POINT('Ctrl Pts',(-1.92327372351062,-3.4381408452317,21.8651969713081));
#65717=CARTESIAN_POINT('Ctrl Pts',(-3.06183225504826,-2.80123857596541,
21.7989015546414));
#65718=CARTESIAN_POINT('Ctrl Pts',(-3.85256884391683,-1.54255230718833,
21.7326061379748));
#65719=CARTESIAN_POINT('Ctrl Pts',(-3.93217576084423,-0.240391499487906,
21.6663107213081));
#65720=CARTESIAN_POINT('Ctrl Pts',(-3.93703784197572,-0.160860577582587,
21.6622616548837));
#65721=CARTESIAN_POINT('Ctrl Pts',(-3.93924720199552,-0.0811674829656328,
21.6582125884594));
#65722=CARTESIAN_POINT('Ctrl Pts',(-3.93886994768263,-0.00145307456529742,
21.654163522035));
#65723=CARTESIAN_POINT('Ctrl Pts',(-3.92682300552281,0.000912804021836195,
21.4708364779651));
#65724=CARTESIAN_POINT('Ctrl Pts',(-3.92533859568391,-0.710585805859282,
21.5066941382286));
#65725=CARTESIAN_POINT('Ctrl Pts',(-3.74063776254721,-1.42280261393549,
21.5425517984922));
#65726=CARTESIAN_POINT('Ctrl Pts',(-3.37738304094838,-2.02781391547153,
21.5784094587558));
#65727=CARTESIAN_POINT('Ctrl Pts',(-2.70888367924349,-3.14121904100145,
21.6443984785073));
#65728=CARTESIAN_POINT('Ctrl Pts',(-1.43567206206342,-3.89154899512166,
21.7103874982589));
#65729=CARTESIAN_POINT('Ctrl Pts',(-0.137789558142141,-3.93697339573595,
21.7763765180104));
#65730=CARTESIAN_POINT('Ctrl Pts',(1.16009294577916,-3.98239779635025,21.842365537762));
#65731=CARTESIAN_POINT('Ctrl Pts',(2.4826463364417,-3.32291664345865,21.9083545575135));
#65732=CARTESIAN_POINT('Ctrl Pts',(3.22735044469825,-2.25897202022772,21.9743435772651));
#65733=CARTESIAN_POINT('Ctrl Pts',(3.97205455295482,-1.19502739699677,22.0403325970166));
#65734=CARTESIAN_POINT('Ctrl Pts',(4.13890937880536,0.273380696573503,22.1063216167682));
#65735=CARTESIAN_POINT('Ctrl Pts',(3.65190029886735,1.47728456574835,22.1723106365197));
#65736=CARTESIAN_POINT('Ctrl Pts',(3.16489121892935,2.68118843492317,22.2382996562713));
#65737=CARTESIAN_POINT('Ctrl Pts',(2.0240182332028,3.62058807970259,22.3042886760228));
#65738=CARTESIAN_POINT('Ctrl Pts',(0.749032747709332,3.86751799270859,22.3702776957744));
#65739=CARTESIAN_POINT('Ctrl Pts',(-0.525952737784169,4.1144479057146,22.4362667155259));
#65740=CARTESIAN_POINT('Ctrl Pts',(-1.93505072304459,3.6689080869472,22.5022557352774));
#65741=CARTESIAN_POINT('Ctrl Pts',(-2.8363136221232,2.73387463465757,22.568244755029));
#65742=CARTESIAN_POINT('Ctrl Pts',(-3.53100120856598,2.01315692523182,22.6191086626744));
#65743=CARTESIAN_POINT('Ctrl Pts',(-3.92397248148655,1.00161997425012,22.6699725703197));
#65744=CARTESIAN_POINT('Ctrl Pts',(-3.93314739898817,-0.00354003882696159,
22.7208364779651));
#65745=CARTESIAN_POINT('Origin',(0.,0.,0.));
#65746=CARTESIAN_POINT('',(-3.92649966780813,-0.000194383930052777,24.154163522035));
#65747=CARTESIAN_POINT('',(-3.93821094167311,0.00191457267368049,23.9708364779651));
#65748=CARTESIAN_POINT('',(-3.933,-4.81653586104654E-16,0.));
#65749=CARTESIAN_POINT('Ctrl Pts',(-3.92649966780813,-0.000194383930052777,
24.154163522035));
#65750=CARTESIAN_POINT('Ctrl Pts',(-3.92620568854956,0.669400878559864,
24.120424255126));
#65751=CARTESIAN_POINT('Ctrl Pts',(-3.76395243069231,1.33912979693549,24.0866849882171));
#65752=CARTESIAN_POINT('Ctrl Pts',(-3.44054292979195,1.9189733284899,24.0529457213081));
#65753=CARTESIAN_POINT('Ctrl Pts',(-2.80506475908943,3.05832732303874,23.9866503046415));
#65754=CARTESIAN_POINT('Ctrl Pts',(-1.54736817451896,3.85063709663954,23.9203548879748));
#65755=CARTESIAN_POINT('Ctrl Pts',(-0.245307921498792,3.93187211272784,
23.8540594713081));
#65756=CARTESIAN_POINT('Ctrl Pts',(1.05675233152134,4.01310712881613,23.7877640546414));
#65757=CARTESIAN_POINT('Ctrl Pts',(2.40317625299117,3.38326738739196,23.7214686379748));
#65758=CARTESIAN_POINT('Ctrl Pts',(3.1753428957673,2.33173578724029,23.6551732213081));
#65759=CARTESIAN_POINT('Ctrl Pts',(3.94750953854344,1.28020418708861,23.5888778046414));
#65760=CARTESIAN_POINT('Ctrl Pts',(4.14541890262589,-0.193019271790565,
23.5225823879748));
#65761=CARTESIAN_POINT('Ctrl Pts',(3.67814057872457,-1.41105498487359,23.4562869713081));
#65762=CARTESIAN_POINT('Ctrl Pts',(3.21086225482324,-2.62909069795662,23.3899915546414));
#65763=CARTESIAN_POINT('Ctrl Pts',(2.07839624293814,-3.59193866524351,23.3236961379748));
#65764=CARTESIAN_POINT('Ctrl Pts',(0.801059499496516,-3.85721375677617,
23.2574007213081));
#65765=CARTESIAN_POINT('Ctrl Pts',(-0.476277243945107,-4.12248884830884,
23.1911053046414));
#65766=CARTESIAN_POINT('Ctrl Pts',(-1.89848471894325,-3.69019106408728,
23.1248098879748));
#65767=CARTESIAN_POINT('Ctrl Pts',(-2.81212286016002,-2.75894170046458,
23.0585144713081));
#65768=CARTESIAN_POINT('Ctrl Pts',(-3.52117597161916,-2.03622093276366,
23.0070641548837));
#65769=CARTESIAN_POINT('Ctrl Pts',(-3.92392043378181,-1.01298423891683,
22.9556138384594));
#65770=CARTESIAN_POINT('Ctrl Pts',(-3.93336305982959,0.00361627372896939,
22.904163522035));
#65771=CARTESIAN_POINT('Ctrl Pts',(-3.93314739898817,-0.00354003882696159,
22.7208364779651));
#65772=CARTESIAN_POINT('Ctrl Pts',(-3.9358756922358,-0.302438778350537,
22.7359615900713));
#65773=CARTESIAN_POINT('Ctrl Pts',(-3.90466658238743,-0.60077363364454,
22.7510867021775));
#65774=CARTESIAN_POINT('Ctrl Pts',(-3.83736180721441,-0.890729948748711,
22.7662118142836));
#65775=CARTESIAN_POINT('Ctrl Pts',(-3.54371928033023,-2.15577399405356,
22.8322008340352));
#65776=CARTESIAN_POINT('Ctrl Pts',(-2.56300641366511,-3.26133499885145,
22.8981898537867));
#65777=CARTESIAN_POINT('Ctrl Pts',(-1.34200992031493,-3.7037487569815,22.9641788735383));
#65778=CARTESIAN_POINT('Ctrl Pts',(-0.121013426964719,-4.14616251511156,
23.0301678932898));
#65779=CARTESIAN_POINT('Ctrl Pts',(1.34026669307056,-3.92542902657374,23.0961569130414));
#65780=CARTESIAN_POINT('Ctrl Pts',(2.37611006032544,-3.14210860128767,23.1621459327929));
#65781=CARTESIAN_POINT('Ctrl Pts',(3.41195342758027,-2.35878817600163,23.2281349525445));
#65782=CARTESIAN_POINT('Ctrl Pts',(4.02236004205474,-1.01288081396738,23.294123972296));
#65783=CARTESIAN_POINT('Ctrl Pts',(3.92924487580339,0.282453867097757,23.3601129920475));
#65784=CARTESIAN_POINT('Ctrl Pts',(3.83612970955204,1.57778854816291,23.4261020117991));
#65785=CARTESIAN_POINT('Ctrl Pts',(3.03949276257486,2.82255054825896,23.4920910315506));
#65786=CARTESIAN_POINT('Ctrl Pts',(1.9022606519978,3.44965938795798,23.5580800513022));
#65787=CARTESIAN_POINT('Ctrl Pts',(0.765028541420735,4.076768227657,23.6240690710537));
#65788=CARTESIAN_POINT('Ctrl Pts',(-0.712798732756265,4.08622390695897,
23.6900580908053));
#65789=CARTESIAN_POINT('Ctrl Pts',(-1.85796234749118,3.47371866972136,23.7560471105568));
#65790=CARTESIAN_POINT('Ctrl Pts',(-3.00312596222609,2.86121343248376,23.8220361303084));
#65791=CARTESIAN_POINT('Ctrl Pts',(-3.81562591751894,1.62674727870669,23.8880251500599));
#65792=CARTESIAN_POINT('Ctrl Pts',(-3.92530883132,0.332710173915526,23.9540141698115));
#65793=CARTESIAN_POINT('Ctrl Pts',(-3.93462916866347,0.222748996429926,
23.9596216058627));
#65794=CARTESIAN_POINT('Ctrl Pts',(-3.93887460484717,0.112357669032555,
23.9652290419139));
#65795=CARTESIAN_POINT('Ctrl Pts',(-3.93821094167311,0.00191457267368049,
23.9708364779651));
#65796=CARTESIAN_POINT('Origin',(0.,0.,0.));
#65797=CARTESIAN_POINT('',(-3.93407891385469,-0.00354965325188361,25.404163522035));
#65798=CARTESIAN_POINT('',(-3.92767634141232,0.00202018669269811,25.2208364779651));
#65799=CARTESIAN_POINT('',(-3.933,-4.81653586104654E-16,0.));
#65800=CARTESIAN_POINT('Ctrl Pts',(-3.93407891385469,-0.00354965325188361,
25.404163522035));
#65801=CARTESIAN_POINT('Ctrl Pts',(-3.9244242454102,1.0359427451275,25.3515300884594));
#65802=CARTESIAN_POINT('Ctrl Pts',(-3.50088813201609,2.08238911627919,25.2988966548837));
#65803=CARTESIAN_POINT('Ctrl Pts',(-2.76245569162327,2.80867100939486,25.2462632213081));
#65804=CARTESIAN_POINT('Ctrl Pts',(-1.83234942664463,3.72347282737578,25.1799678046414));
#65805=CARTESIAN_POINT('Ctrl Pts',(-0.40265608081936,4.13032957499881,25.1136723879748));
#65806=CARTESIAN_POINT('Ctrl Pts',(0.869744861155389,3.84230896254983,25.0473769713081));
#65807=CARTESIAN_POINT('Ctrl Pts',(2.14214580313014,3.55428835010084,24.9810815546414));
#65808=CARTESIAN_POINT('Ctrl Pts',(3.25725434125437,2.57139037757985,24.9147861379748));
#65809=CARTESIAN_POINT('Ctrl Pts',(3.70272849391131,1.34521224629211,24.8484907213081));
#65810=CARTESIAN_POINT('Ctrl Pts',(4.14820264656826,0.119034115004331,24.7821953046414));
#65811=CARTESIAN_POINT('Ctrl Pts',(3.92404241375788,-1.3504241750502,24.7158998879748));
#65812=CARTESIAN_POINT('Ctrl Pts',(3.13323929267643,-2.38801294427511,24.6496044713081));
#65813=CARTESIAN_POINT('Ctrl Pts',(2.342436171595,-3.42560171349998,24.5833090546414));
#65814=CARTESIAN_POINT('Ctrl Pts',(0.984990162242543,-4.03132096189525,
24.5170136379748));
#65815=CARTESIAN_POINT('Ctrl Pts',(-0.31541363694263,-3.92687006721989,
24.4507182213081));
#65816=CARTESIAN_POINT('Ctrl Pts',(-1.6158174361278,-3.82241917254453,24.3844228046415));
#65817=CARTESIAN_POINT('Ctrl Pts',(-2.85917902514569,-3.00779813479854,
24.3181273879748));
#65818=CARTESIAN_POINT('Ctrl Pts',(-3.47422994123735,-1.85728850817714,
24.2518319713081));
#65819=CARTESIAN_POINT('Ctrl Pts',(-3.77626725753592,-1.29229977162088,
24.2192758215504));
#65820=CARTESIAN_POINT('Ctrl Pts',(-3.92678333825044,-0.64630930105307,
24.1867196717927));
#65821=CARTESIAN_POINT('Ctrl Pts',(-3.92649966780813,-0.000194383930052777,
24.154163522035));
#65822=CARTESIAN_POINT('Ctrl Pts',(-3.93821094167311,0.00191457267368049,
23.9708364779651));
#65823=CARTESIAN_POINT('Ctrl Pts',(-3.93106453231111,-1.18735071827648,
24.0312180616654));
#65824=CARTESIAN_POINT('Ctrl Pts',(-3.3546954866468,-2.38261875282536,24.0915996453658));
#65825=CARTESIAN_POINT('Ctrl Pts',(-2.41612259034546,-3.11144614439781,
24.1519812290661));
#65826=CARTESIAN_POINT('Ctrl Pts',(-1.39038756326069,-3.90795730211473,
24.2179702488177));
#65827=CARTESIAN_POINT('Ctrl Pts',(0.0679483632180516,-4.14737156174339,
24.2839592685692));
#65828=CARTESIAN_POINT('Ctrl Pts',(1.29450610594822,-3.72061815062074,24.3499482883208));
#65829=CARTESIAN_POINT('Ctrl Pts',(2.52106384867842,-3.29386473949807,24.4159373080723));
#65830=CARTESIAN_POINT('Ctrl Pts',(3.51584340766002,-2.20094365762405,24.4819263278238));
#65831=CARTESIAN_POINT('Ctrl Pts',(3.82564965869348,-0.939760698265326,
24.5479153475754));
#65832=CARTESIAN_POINT('Ctrl Pts',(4.13545590972695,0.321422261093383,24.6139043673269));
#65833=CARTESIAN_POINT('Ctrl Pts',(3.76028885281226,1.75086709793682,24.6798933870785));
#65834=CARTESIAN_POINT('Ctrl Pts',(2.871064626524,2.69735674158764,24.74588240683));
#65835=CARTESIAN_POINT('Ctrl Pts',(1.98184040023576,3.64384638523844,24.8118714265816));
#65836=CARTESIAN_POINT('Ctrl Pts',(0.578559004573957,4.10738083569666,24.8778604463331));
#65837=CARTESIAN_POINT('Ctrl Pts',(-0.699481858119317,3.87678611883963,
24.9438494660847));
#65838=CARTESIAN_POINT('Ctrl Pts',(-1.97752272081263,3.64619140198259,25.0098384858362));
#65839=CARTESIAN_POINT('Ctrl Pts',(-3.13032305053739,2.72146751781024,25.0758275055878));
#65840=CARTESIAN_POINT('Ctrl Pts',(-3.63269766039478,1.52389408727378,25.1418165253393));
#65841=CARTESIAN_POINT('Ctrl Pts',(-3.83322404099964,1.04587417778395,25.1681565095479));
#65842=CARTESIAN_POINT('Ctrl Pts',(-3.93012045155741,0.524382140035048,
25.1944964937565));
#65843=CARTESIAN_POINT('Ctrl Pts',(-3.92767634141232,0.00202018669269811,
25.2208364779651));
#65844=CARTESIAN_POINT('Origin',(0.,0.,0.));
#65845=CARTESIAN_POINT('',(-3.93847239432236,0.00183746061217384,26.654163522035));
#65846=CARTESIAN_POINT('',(-3.93096036061645,-0.0034105068734492,26.4708364779651));
#65847=CARTESIAN_POINT('',(-3.933,-4.81653586104654E-16,0.));
#65848=CARTESIAN_POINT('Ctrl Pts',(-3.93847239432236,0.00183746061217384,
26.654163522035));
#65849=CARTESIAN_POINT('Ctrl Pts',(-3.93906782029507,0.104871598938666,
26.6489313384594));
#65850=CARTESIAN_POINT('Ctrl Pts',(-3.93537654477555,0.207862391149194,
26.6436991548837));
#65851=CARTESIAN_POINT('Ctrl Pts',(-3.92726137617655,0.310503414455952,
26.6384669713081));
#65852=CARTESIAN_POINT('Ctrl Pts',(-3.82443652765684,1.61103679767247,26.5721715546415));
#65853=CARTESIAN_POINT('Ctrl Pts',(-3.01137076827103,2.8554159790709,26.5058761379748));
#65854=CARTESIAN_POINT('Ctrl Pts',(-1.86163107209072,3.47190495817833,26.4395807213081));
#65855=CARTESIAN_POINT('Ctrl Pts',(-0.711891375910411,4.08839393728577,
26.3732853046414));
#65856=CARTESIAN_POINT('Ctrl Pts',(0.774522257064396,4.07699271410221,26.3069898879748));
#65857=CARTESIAN_POINT('Ctrl Pts',(1.91466993337585,3.44293963546029,26.2406944713081));
#65858=CARTESIAN_POINT('Ctrl Pts',(3.05481760968731,2.80888655681837,26.1743990546414));
#65859=CARTESIAN_POINT('Ctrl Pts',(3.84869932933542,1.55218162271808,26.1081036379748));
#65860=CARTESIAN_POINT('Ctrl Pts',(3.93156231758308,0.250223959999214,26.0418082213081));
#65861=CARTESIAN_POINT('Ctrl Pts',(4.01442530583075,-1.05173370271969,25.9755128046415));
#65862=CARTESIAN_POINT('Ctrl Pts',(3.38626956267792,-2.39894409405719,25.9092173879748));
#65863=CARTESIAN_POINT('Ctrl Pts',(2.33570426580363,-3.17242491950617,25.8429219713081));
#65864=CARTESIAN_POINT('Ctrl Pts',(1.28513896892936,-3.94590574495512,25.7766265546414));
#65865=CARTESIAN_POINT('Ctrl Pts',(-0.187835881666348,-4.1456570045156,
25.7103311379748));
#65866=CARTESIAN_POINT('Ctrl Pts',(-1.40645490573152,-3.67990202116044,
25.6440357213081));
#65867=CARTESIAN_POINT('Ctrl Pts',(-2.62507392979665,-3.21414703780529,
25.5777403046415));
#65868=CARTESIAN_POINT('Ctrl Pts',(-3.58933712733127,-2.08288581153454,
25.5114448879748));
#65869=CARTESIAN_POINT('Ctrl Pts',(-3.8562091340326,-0.805881754229776,
25.4451494713081));
#65870=CARTESIAN_POINT('Ctrl Pts',(-3.91120540717406,-0.542720155505481,
25.4314874882171));
#65871=CARTESIAN_POINT('Ctrl Pts',(-3.93658496197046,-0.273369169197457,
25.417825505126));
#65872=CARTESIAN_POINT('Ctrl Pts',(-3.93407891385469,-0.00354965325188361,
25.404163522035));
#65873=CARTESIAN_POINT('Ctrl Pts',(-3.92767634141232,0.00202018669269811,
25.2208364779651));
#65874=CARTESIAN_POINT('Ctrl Pts',(-3.92399727276726,-0.784280499380038,
25.260485513508));
#65875=CARTESIAN_POINT('Ctrl Pts',(-3.69522588961778,-1.57255229767332,
25.300134549051));
#65876=CARTESIAN_POINT('Ctrl Pts',(-3.25599248064403,-2.21748922140678,
25.339783584594));
#65877=CARTESIAN_POINT('Ctrl Pts',(-2.52496380104585,-3.29087612265032,
25.4057726043455));
#65878=CARTESIAN_POINT('Ctrl Pts',(-1.21095755185952,-3.96722694823681,
25.4717616240971));
#65879=CARTESIAN_POINT('Ctrl Pts',(0.0873999482272789,-3.93841424054347,
25.5377506438486));
#65880=CARTESIAN_POINT('Ctrl Pts',(1.38575744831402,-3.90960153285012,25.6037396636002));
#65881=CARTESIAN_POINT('Ctrl Pts',(2.66846619930122,-3.17562529187698,25.6697286833517));
#65882=CARTESIAN_POINT('Ctrl Pts',(3.35115819074181,-2.07086558271892,25.7357177031032));
#65883=CARTESIAN_POINT('Ctrl Pts',(4.03385018218244,-0.966105873560801,
25.8017067228548));
#65884=CARTESIAN_POINT('Ctrl Pts',(4.11652541407643,0.509437303782197,25.8676957426063));
#65885=CARTESIAN_POINT('Ctrl Pts',(3.56151924841617,1.68354570007079,25.9336847623579));
#65886=CARTESIAN_POINT('Ctrl Pts',(3.00651308275592,2.85765409635936,25.9996737821094));
#65887=CARTESIAN_POINT('Ctrl Pts',(1.8138255195414,3.73032771159348,26.065662801861));
#65888=CARTESIAN_POINT('Ctrl Pts',(0.526813308981318,3.90399964376866,26.1316518216125));
#65889=CARTESIAN_POINT('Ctrl Pts',(-0.760198901578725,4.07767157594384,
26.1976408413641));
#65890=CARTESIAN_POINT('Ctrl Pts',(-2.14153575948438,3.55234182506012,26.2636298611156));
#65891=CARTESIAN_POINT('Ctrl Pts',(-2.9878969104734,2.56733666149362,26.3296188808671));
#65892=CARTESIAN_POINT('Ctrl Pts',(-3.59163921219624,1.86469419738052,26.3766914132331));
#65893=CARTESIAN_POINT('Ctrl Pts',(-3.92315787657576,0.928144826430376,
26.4237639455991));
#65894=CARTESIAN_POINT('Ctrl Pts',(-3.93096036061645,-0.0034105068734492,
26.4708364779651));
#65895=CARTESIAN_POINT('Origin',(0.,0.,0.));
#65896=CARTESIAN_POINT('',(-3.92840989342865,0.00265517403989252,27.904163522035));
#65897=CARTESIAN_POINT('',(-3.93924705030466,0.000656224253225424,27.7208364779651));
#65898=CARTESIAN_POINT('',(-3.933,-4.81653586104654E-16,0.));
#65899=CARTESIAN_POINT('Ctrl Pts',(-3.92840989342865,0.00265517403989252,
27.904163522035));
#65900=CARTESIAN_POINT('Ctrl Pts',(-3.93136414635793,0.480888864434302,
27.8800371717927));
#65901=CARTESIAN_POINT('Ctrl Pts',(-3.85060148071847,0.958158959844772,
27.8559108215504));
#65902=CARTESIAN_POINT('Ctrl Pts',(-3.68165771049416,1.40185262775938,27.8317844713081));
#65903=CARTESIAN_POINT('Ctrl Pts',(-3.21742679583935,2.62105305763651,27.7654890546414));
#65904=CARTESIAN_POINT('Ctrl Pts',(-2.08737212377921,3.5867299779047,27.6991936379748));
#65905=CARTESIAN_POINT('Ctrl Pts',(-0.810702749059684,3.85519848255106,
27.6328982213081));
#65906=CARTESIAN_POINT('Ctrl Pts',(0.465966625659809,4.12366698719743,27.5666028046414));
#65907=CARTESIAN_POINT('Ctrl Pts',(1.88925070303869,3.69492707622201,27.5003073879748));
#65908=CARTESIAN_POINT('Ctrl Pts',(2.80521476759667,2.76596536400124,27.4340119713081));
#65909=CARTESIAN_POINT('Ctrl Pts',(3.72117883215465,1.83700365178048,27.3677165546414));
#65910=CARTESIAN_POINT('Ctrl Pts',(4.12982288389174,0.407820138314366,27.3014211379748));
#65911=CARTESIAN_POINT('Ctrl Pts',(3.84339344762151,-0.864939936629703,
27.2351257213081));
#65912=CARTESIAN_POINT('Ctrl Pts',(3.55696401135128,-2.13770001157377,27.1688303046415));
#65913=CARTESIAN_POINT('Ctrl Pts',(2.57546108707372,-3.2540366479958,27.1025348879748));
#65914=CARTESIAN_POINT('Ctrl Pts',(1.34984091446835,-3.70104360860882,27.0362394713081));
#65915=CARTESIAN_POINT('Ctrl Pts',(0.124220741862938,-4.14805056922186,
26.9699440546414));
#65916=CARTESIAN_POINT('Ctrl Pts',(-1.3455166790703,-3.92572785402585,26.9036486379748));
#65917=CARTESIAN_POINT('Ctrl Pts',(-2.38409342071011,-3.13622270391051,
26.8373532213081));
#65918=CARTESIAN_POINT('Ctrl Pts',(-3.34070334710301,-2.40902707814848,
26.7762899882171));
#65919=CARTESIAN_POINT('Ctrl Pts',(-3.9315233577615,-1.20064282587445,26.715226755126));
#65920=CARTESIAN_POINT('Ctrl Pts',(-3.93847239432236,0.00183746061217384,
26.654163522035));
#65921=CARTESIAN_POINT('Ctrl Pts',(-3.93096036061645,-0.0034105068734492,
26.4708364779651));
#65922=CARTESIAN_POINT('Ctrl Pts',(-3.93409585351461,-0.377763740610767,
26.4897529653507));
#65923=CARTESIAN_POINT('Ctrl Pts',(-3.88495439272852,-0.751310486780916,
26.5086694527362));
#65924=CARTESIAN_POINT('Ctrl Pts',(-3.78019431150709,-1.10854699869474,
26.5275859401218));
#65925=CARTESIAN_POINT('Ctrl Pts',(-3.41474511747934,-2.35474491906723,
26.5935749598733));
#65926=CARTESIAN_POINT('Ctrl Pts',(-2.37246128535146,-3.40246018356284,
26.6595639796249));
#65927=CARTESIAN_POINT('Ctrl Pts',(-1.1281796234269,-3.77438156766775,26.7255529993764));
#65928=CARTESIAN_POINT('Ctrl Pts',(0.116102038497622,-4.14630295177265,
26.791542019128));
#65929=CARTESIAN_POINT('Ctrl Pts',(1.56238153021876,-3.84243045548688,26.8575310388795));
#65930=CARTESIAN_POINT('Ctrl Pts',(2.55177235978977,-3.00120031068882,26.9235200586311));
#65931=CARTESIAN_POINT('Ctrl Pts',(3.5411631893608,-2.15997016589073,26.9895090783826));
#65932=CARTESIAN_POINT('Ctrl Pts',(4.07366535678164,-0.78138237258023,27.0554980981342));
#65933=CARTESIAN_POINT('Ctrl Pts',(3.90668502935641,0.506515115735212,27.1214871178857));
#65934=CARTESIAN_POINT('Ctrl Pts',(3.73970470193117,1.79441260405062,27.1874761376373));
#65935=CARTESIAN_POINT('Ctrl Pts',(2.87324187965999,2.99161978737102,27.2534651573888));
#65936=CARTESIAN_POINT('Ctrl Pts',(1.70203399236642,3.55272089670649,27.3194541771404));
#65937=CARTESIAN_POINT('Ctrl Pts',(0.530826105072816,4.11382200604197,27.3854431968919));
#65938=CARTESIAN_POINT('Ctrl Pts',(-0.945126847243146,4.03881704139246,
27.4514322166435));
#65939=CARTESIAN_POINT('Ctrl Pts',(-2.05341993275692,3.36187627089729,27.517421236395));
#65940=CARTESIAN_POINT('Ctrl Pts',(-3.16171301827067,2.68493550040213,27.5834102561465));
#65941=CARTESIAN_POINT('Ctrl Pts',(-3.90234623698222,1.40605892406135,27.6493992758981));
#65942=CARTESIAN_POINT('Ctrl Pts',(-3.93790678169248,0.107868715418545,
27.7153882956496));
#65943=CARTESIAN_POINT('Ctrl Pts',(-3.93888543102711,0.0721416759634396,
27.7172043564214));
#65944=CARTESIAN_POINT('Ctrl Pts',(-3.9393300680325,0.0364000086293204,
27.7190204171933));
#65945=CARTESIAN_POINT('Ctrl Pts',(-3.93924705030466,0.000656224253225424,
27.7208364779651));
#65946=CARTESIAN_POINT('Origin',(0.,0.,0.));
#65947=CARTESIAN_POINT('',(-3.92876997665636,-0.00284051892226578,29.154163522035));
#65948=CARTESIAN_POINT('',(-3.92912953761977,0.00289384936589777,28.9708364779651));
#65949=CARTESIAN_POINT('',(-3.933,-4.81653586104654E-16,0.));
#65950=CARTESIAN_POINT('Ctrl Pts',(-3.92876997665636,-0.00284051892226578,
29.154163522035));
#65951=CARTESIAN_POINT('Ctrl Pts',(-3.92310187586187,0.849718058506195,
29.111143005126));
#65952=CARTESIAN_POINT('Ctrl Pts',(-3.65068494473056,1.70557539765092,29.0681224882171));
#65953=CARTESIAN_POINT('Ctrl Pts',(-3.13920121202234,2.38017016989005,29.0251019713081));
#65954=CARTESIAN_POINT('Ctrl Pts',(-2.35099526717338,3.41973326024983,28.9588065546414));
#65955=CARTESIAN_POINT('Ctrl Pts',(-0.995068227481178,4.02884518692243,
28.8925111379748));
#65956=CARTESIAN_POINT('Ctrl Pts',(0.30559270653279,3.92764654531323,28.8262157213081));
#65957=CARTESIAN_POINT('Ctrl Pts',(1.60625364054687,3.82644790370401,28.7599203046414));
#65958=CARTESIAN_POINT('Ctrl Pts',(2.85164846888267,3.01493869381287,28.6936248879748));
#65959=CARTESIAN_POINT('Ctrl Pts',(3.46957454719653,1.86597072555893,28.6273294713081));
#65960=CARTESIAN_POINT('Ctrl Pts',(4.08750062551035,0.717002757305092,28.5610340546415));
#65961=CARTESIAN_POINT('Ctrl Pts',(4.0779579538023,-0.76942396931155,28.4947386379748));
#65962=CARTESIAN_POINT('Ctrl Pts',(3.44533095848979,-1.9103635448963,28.4284432213081));
#65963=CARTESIAN_POINT('Ctrl Pts',(2.81270396317727,-3.05130312048108,28.3621478046414));
#65964=CARTESIAN_POINT('Ctrl Pts',(1.55699264426028,-3.84675554503403,28.2958523879748));
#65965=CARTESIAN_POINT('Ctrl Pts',(0.255139607303237,-3.9312463758943,28.2295569713081));
#65966=CARTESIAN_POINT('Ctrl Pts',(-1.04671342965381,-4.01573720675458,
28.1632615546415));
#65967=CARTESIAN_POINT('Ctrl Pts',(-2.39470818465087,-3.38926644392217,
28.0969661379748));
#65968=CARTESIAN_POINT('Ctrl Pts',(-3.16950198352466,-2.33966909276295,
28.0306707213081));
#65969=CARTESIAN_POINT('Ctrl Pts',(-3.66233139485763,-1.67204314446506,
27.9885016548837));
#65970=CARTESIAN_POINT('Ctrl Pts',(-3.92324632385603,-0.833222115898168,
27.9463325884593));
#65971=CARTESIAN_POINT('Ctrl Pts',(-3.92840989342865,0.00265517403989252,
27.904163522035));
#65972=CARTESIAN_POINT('Ctrl Pts',(-3.93924705030466,0.000656224253225424,
27.7208364779651));
#65973=CARTESIAN_POINT('Ctrl Pts',(-3.93631350682071,-1.26239864932264,
27.7850094369448));
#65974=CARTESIAN_POINT('Ctrl Pts',(-3.27451985550136,-2.5280969835108,27.8491823959246));
#65975=CARTESIAN_POINT('Ctrl Pts',(-2.23438232319365,-3.24442307889484,
27.9133553549043));
#65976=CARTESIAN_POINT('Ctrl Pts',(-1.16480944927562,-3.98102082362052,
27.9793443746558));
#65977=CARTESIAN_POINT('Ctrl Pts',(0.304824169269371,-4.13671247212701,
28.0453333944074));
#65978=CARTESIAN_POINT('Ctrl Pts',(1.50499252110454,-3.64056904789417,28.1113224141589));
#65979=CARTESIAN_POINT('Ctrl Pts',(2.70516087293964,-3.14442562366137,28.1773114339105));
#65980=CARTESIAN_POINT('Ctrl Pts',(3.63586395806496,-1.9964471266893,28.243300453662));
#65981=CARTESIAN_POINT('Ctrl Pts',(3.87309819051212,-0.719622045046852,
28.3092894734135));
#65982=CARTESIAN_POINT('Ctrl Pts',(4.11033242295931,0.557203036595705,28.3752784931651));
#65983=CARTESIAN_POINT('Ctrl Pts',(3.65409780272822,1.96287470290867,28.4412675129166));
#65984=CARTESIAN_POINT('Ctrl Pts',(2.71224269533156,2.85700630777853,28.5072565326682));
#65985=CARTESIAN_POINT('Ctrl Pts',(1.77038758793493,3.75113791264836,28.5732455524197));
#65986=CARTESIAN_POINT('Ctrl Pts',(0.342911993372745,4.13372945607512,28.6392345721713));
#65987=CARTESIAN_POINT('Ctrl Pts',(-0.919864152115334,3.83048240078438,
28.7052235919229));
#65988=CARTESIAN_POINT('Ctrl Pts',(-2.18264029760341,3.52723534549364,28.7712126116744));
#65989=CARTESIAN_POINT('Ctrl Pts',(-3.28071699401739,2.5381496914854,28.8372016314259));
#65990=CARTESIAN_POINT('Ctrl Pts',(-3.71383968715089,1.31382657120668,28.9031906511775));
#65991=CARTESIAN_POINT('Ctrl Pts',(-3.86183876734026,0.895472376128801,
28.9257392601067));
#65992=CARTESIAN_POINT('Ctrl Pts',(-3.93219744831015,0.449651723668126,
28.9482878690359));
#65993=CARTESIAN_POINT('Ctrl Pts',(-3.92912953761977,0.00289384936589777,
28.9708364779651));
#65994=CARTESIAN_POINT('Origin',(0.,0.,0.));
#65995=CARTESIAN_POINT('',(-3.93876665726707,-0.00156339645701664,30.404163522035));
#65996=CARTESIAN_POINT('',(-3.9290580015118,-0.00286337897428823,30.2208364779651));
#65997=CARTESIAN_POINT('',(-3.933,-4.81653586104654E-16,0.));
#65998=CARTESIAN_POINT('Ctrl Pts',(-3.93876665726707,-0.00156339645701664,
30.404163522035));
#65999=CARTESIAN_POINT('Ctrl Pts',(-3.93262187151115,1.2174425911067,30.3422488384594));
#66000=CARTESIAN_POINT('Ctrl Pts',(-3.32296578001872,2.44175279030972,30.2803341548837));
#66001=CARTESIAN_POINT('Ctrl Pts',(-2.34363026191953,3.16657409239259,30.2184194713081));
#66002=CARTESIAN_POINT('Ctrl Pts',(-1.29500249739966,3.94267965339049,30.1521240546414));
#66003=CARTESIAN_POINT('Ctrl Pts',(0.177468228542797,4.14611376416382,30.0858286379748));
#66004=CARTESIAN_POINT('Ctrl Pts',(1.39724815815262,3.68340764398078,30.0195332213081));
#66005=CARTESIAN_POINT('Ctrl Pts',(2.61702808776238,3.22070152379777,29.9532378046414));
#66006=CARTESIAN_POINT('Ctrl Pts',(3.58411722103958,2.09185517265848,29.8869423879748));
#66007=CARTESIAN_POINT('Ctrl Pts',(3.85418180391149,0.815522476449609,29.8206469713082));
#66008=CARTESIAN_POINT('Ctrl Pts',(4.12424638678342,-0.460810219759336,
29.7543515546415));
#66009=CARTESIAN_POINT('Ctrl Pts',(3.69728641925003,-1.88462926103782,29.6880561379748));
#66010=CARTESIAN_POINT('Ctrl Pts',(2.7694707121116,-2.8017541401688,29.6217607213081));
#66011=CARTESIAN_POINT('Ctrl Pts',(1.84165500497318,-3.71887901929977,29.5554653046414));
#66012=CARTESIAN_POINT('Ctrl Pts',(0.412983558229673,-4.12930973628314,
29.4891698879748));
#66013=CARTESIAN_POINT('Ctrl Pts',(-0.860133659870229,-3.84447192399102,
29.4228744713081));
#66014=CARTESIAN_POINT('Ctrl Pts',(-2.13325087797013,-3.5596341116989,29.3565790546415));
#66015=CARTESIAN_POINT('Ctrl Pts',(-3.25081386742647,-2.57952777013129,
29.2902836379748));
#66016=CARTESIAN_POINT('Ctrl Pts',(-3.69935293715175,-1.35446747232396,
29.2239882213081));
#66017=CARTESIAN_POINT('Ctrl Pts',(-3.85682539015349,-0.924375060777911,
29.2007133215504));
#66018=CARTESIAN_POINT('Ctrl Pts',(-3.93183652460341,-0.464090565480743,
29.1774384217927));
#66019=CARTESIAN_POINT('Ctrl Pts',(-3.92876997665636,-0.00284051892226578,
29.154163522035));
#66020=CARTESIAN_POINT('Ctrl Pts',(-3.92912953761977,0.00289384936589777,
28.9708364779651));
#66021=CARTESIAN_POINT('Ctrl Pts',(-3.92321913750707,-0.857795413495037,
29.0142768887874));
#66022=CARTESIAN_POINT('Ctrl Pts',(-3.64478664922453,-1.72196316619954,
29.0577172996098));
#66023=CARTESIAN_POINT('Ctrl Pts',(-3.12396193915647,-2.39991818272362,
29.1011577104321));
#66024=CARTESIAN_POINT('Ctrl Pts',(-2.33279280817549,-3.42977922982612,
29.1671467301837));
#66025=CARTESIAN_POINT('Ctrl Pts',(-0.982285856360496,-4.02994073748189,
29.2331357499352));
#66026=CARTESIAN_POINT('Ctrl Pts',(0.312303847731737,-3.92698507608034,
29.2991247696868));
#66027=CARTESIAN_POINT('Ctrl Pts',(1.60689355182397,-3.82402941467878,29.3651137894383));
#66028=CARTESIAN_POINT('Ctrl Pts',(2.8455660081934,-3.01795658421989,29.4311028091899));
#66029=CARTESIAN_POINT('Ctrl Pts',(3.46401497166392,-1.87599193952265,29.4970918289414));
#66030=CARTESIAN_POINT('Ctrl Pts',(4.08246393513439,-0.734027294825464,
29.5630808486929));
#66031=CARTESIAN_POINT('Ctrl Pts',(4.08068940570598,0.743829164110116,29.6290698684445));
#66032=CARTESIAN_POINT('Ctrl Pts',(3.45949981181636,1.88430531844186,29.695058888196));
#66033=CARTESIAN_POINT('Ctrl Pts',(2.83831021792669,3.0247814727737,29.7610479079476));
#66034=CARTESIAN_POINT('Ctrl Pts',(1.59770555957574,3.82787732250171,29.8270369276991));
#66035=CARTESIAN_POINT('Ctrl Pts',(0.302872341801343,3.92772374609487,29.8930259474507));
#66036=CARTESIAN_POINT('Ctrl Pts',(-0.991960875972982,4.02757016968802,
29.9590149672022));
#66037=CARTESIAN_POINT('Ctrl Pts',(-2.34102265317071,3.4241671671464,30.0250039869538));
#66038=CARTESIAN_POINT('Ctrl Pts',(-3.1297163043756,2.39240910698635,30.0909930067053));
#66039=CARTESIAN_POINT('Ctrl Pts',(-3.64700802865811,1.71569527118052,30.1342741637919));
#66040=CARTESIAN_POINT('Ctrl Pts',(-3.92323828559463,0.85470989324939,30.1775553208785));
#66041=CARTESIAN_POINT('Ctrl Pts',(-3.9290580015118,-0.00286337897428823,
30.2208364779651));
#66042=CARTESIAN_POINT('Origin',(0.,0.,0.));
#66043=CARTESIAN_POINT('',(-3.93356382969395,0.00360218745272173,31.654163522035));
#66044=CARTESIAN_POINT('',(-3.93922268899305,-0.000712863612796303,31.470836477965));
#66045=CARTESIAN_POINT('',(-3.933,-4.81653586104654E-16,0.));
#66046=CARTESIAN_POINT('Ctrl Pts',(-3.93356382969395,0.00360218745272173,
31.654163522035));
#66047=CARTESIAN_POINT('Ctrl Pts',(-3.93623015633234,0.290333862757325,
31.6396500884593));
#66048=CARTESIAN_POINT('Ctrl Pts',(-3.90755272302672,0.576536680174273,
31.6251366548837));
#66049=CARTESIAN_POINT('Ctrl Pts',(-3.84554438997229,0.855326038390887,
31.6106232213081));
#66050=CARTESIAN_POINT('Ctrl Pts',(-3.56229864696938,2.12879840927471,31.5443278046415));
#66051=CARTESIAN_POINT('Ctrl Pts',(-2.58359042039501,3.24758600458463,31.4780323879748));
#66052=CARTESIAN_POINT('Ctrl Pts',(-1.3590919126262,3.69765648218316,31.4117369713081));
#66053=CARTESIAN_POINT('Ctrl Pts',(-0.134593404857421,4.14772695978168,
31.3454415546415));
#66054=CARTESIAN_POINT('Ctrl Pts',(1.33569538410578,3.92908031966886,31.2791461379748));
#66055=CARTESIAN_POINT('Ctrl Pts',(2.37624319794866,3.14217481235523,31.2128507213081));
#66056=CARTESIAN_POINT('Ctrl Pts',(3.41679101179155,2.3552693050416,31.1465553046414));
#66057=CARTESIAN_POINT('Ctrl Pts',(4.02759785051412,1.00010493052715,31.0802598879748));
#66058=CARTESIAN_POINT('Ctrl Pts',(3.9280255740277,-0.30068152085102,31.0139644713081));
#66059=CARTESIAN_POINT('Ctrl Pts',(3.82845329754128,-1.60146797222919,30.9476690546415));
#66060=CARTESIAN_POINT('Ctrl Pts',(3.01850190584588,-2.84787650047109,30.8813736379748));
#66061=CARTESIAN_POINT('Ctrl Pts',(1.87030746179732,-3.46723871193523,30.8150782213081));
#66062=CARTESIAN_POINT('Ctrl Pts',(0.722113017748764,-4.08660092339936,
30.7487828046414));
#66063=CARTESIAN_POINT('Ctrl Pts',(-0.764324478652949,-4.07891681808573,
30.6824873879748));
#66064=CARTESIAN_POINT('Ctrl Pts',(-1.90605416978368,-3.44771689514194,
30.6161919713081));
#66065=CARTESIAN_POINT('Ctrl Pts',(-3.04778386091445,-2.81651697219814,
30.5498965546414));
#66066=CARTESIAN_POINT('Ctrl Pts',(-3.84480574677421,-1.56180123162415,
30.4836011379748));
#66067=CARTESIAN_POINT('Ctrl Pts',(-3.93092428815543,-0.260054855725923,
30.4173057213081));
#66068=CARTESIAN_POINT('Ctrl Pts',(-3.93661491298216,-0.174036791253616,
30.4129249882171));
#66069=CARTESIAN_POINT('Ctrl Pts',(-3.93920142757912,-0.0878133707686297,
30.408544255126));
#66070=CARTESIAN_POINT('Ctrl Pts',(-3.93876665726707,-0.00156339645701664,
30.404163522035));
#66071=CARTESIAN_POINT('Ctrl Pts',(-3.9290580015118,-0.00286337897428823,
30.2208364779651));
#66072=CARTESIAN_POINT('Ctrl Pts',(-3.93211136973696,-0.452797193170657,
30.24354434063));
#66073=CARTESIAN_POINT('Ctrl Pts',(-3.86072952940889,-0.901791765875257,
30.266252203295));
#66074=CARTESIAN_POINT('Ctrl Pts',(-3.71067383999213,-1.32274152209106,
30.28896006596));
#66075=CARTESIAN_POINT('Ctrl Pts',(-3.27461219919171,-2.54602097322994,
30.3549490857115));
#66076=CARTESIAN_POINT('Ctrl Pts',(-2.17416339237878,-3.53246675772921,
30.4209381054631));
#66077=CARTESIAN_POINT('Ctrl Pts',(-0.910662644202927,-3.83268039751804,
30.4869271252146));
#66078=CARTESIAN_POINT('Ctrl Pts',(0.35283810397296,-4.13289403730688,30.5529161449662));
#66079=CARTESIAN_POINT('Ctrl Pts',(1.77939079351173,-3.74687553238531,30.6189051647177));
#66080=CARTESIAN_POINT('Ctrl Pts',(2.71909593917019,-2.85048465259049,30.6848941844692));
#66081=CARTESIAN_POINT('Ctrl Pts',(3.65880108482858,-1.95409377279572,30.7508832042208));
#66082=CARTESIAN_POINT('Ctrl Pts',(4.11165868660664,-0.547330518127737,
30.8168722239723));
#66083=CARTESIAN_POINT('Ctrl Pts',(3.87135885883217,0.72892116666162,30.8828612437239));
#66084=CARTESIAN_POINT('Ctrl Pts',(3.6310590310577,2.00517285145101,30.9488502634754));
#66085=CARTESIAN_POINT('Ctrl Pts',(2.69760177373066,3.15091296636183,31.014839283227));
#66086=CARTESIAN_POINT('Ctrl Pts',(1.49624540046417,3.64417277069235,31.0808283029785));
#66087=CARTESIAN_POINT('Ctrl Pts',(0.294889027197638,4.13743257502288,31.1468173227301));
#66088=CARTESIAN_POINT('Ctrl Pts',(-1.17436646200829,3.97821206877312,31.2128063424816));
#66089=CARTESIAN_POINT('Ctrl Pts',(-2.24216732149253,3.23904788224822,31.2787953622332));
#66090=CARTESIAN_POINT('Ctrl Pts',(-3.27800464315046,2.52200982741351,31.3428090674771));
#66091=CARTESIAN_POINT('Ctrl Pts',(-3.93606189014718,1.25922849148747,31.4068227727211));
#66092=CARTESIAN_POINT('Ctrl Pts',(-3.93922268899305,-0.000712863612796303,
31.470836477965));
#66093=CARTESIAN_POINT('Origin',(0.,0.,0.));
#66094=CARTESIAN_POINT('',(-3.92649272786585,-8.54312940767876E-5,32.904163522035));
#66095=CARTESIAN_POINT('',(-3.93104799417585,0.00342476555473607,32.7208364779651));
#66096=CARTESIAN_POINT('',(-3.933,-4.81653586104654E-16,0.));
#66097=CARTESIAN_POINT('Ctrl Pts',(-3.92649272786585,-8.54312940767876E-5,
32.904163522035));
#66098=CARTESIAN_POINT('Ctrl Pts',(-3.92636480720739,0.662930438433491,
32.8707559217927));
#66099=CARTESIAN_POINT('Ctrl Pts',(-3.76745221108675,1.3260038941436,32.8373483215504));
#66100=CARTESIAN_POINT('Ctrl Pts',(-3.45009744168608,1.90174181477382,32.8039407213081));
#66101=CARTESIAN_POINT('Ctrl Pts',(-2.82032557791886,3.04425983648661,32.7376453046415));
#66102=CARTESIAN_POINT('Ctrl Pts',(-1.56660737729212,3.8428499376043,32.6713498879748));
#66103=CARTESIAN_POINT('Ctrl Pts',(-0.264969697583205,3.93059605487079,
32.6050544713081));
#66104=CARTESIAN_POINT('Ctrl Pts',(1.03666798212571,4.01834217213727,32.5387590546415));
#66105=CARTESIAN_POINT('Ctrl Pts',(2.38622514091682,3.39524430555255,32.4724636379748));
#66106=CARTESIAN_POINT('Ctrl Pts',(3.16364125068744,2.34758776708021,32.4061682213081));
#66107=CARTESIAN_POINT('Ctrl Pts',(3.94105736045805,1.2999312286079,32.3398728046414));
#66108=CARTESIAN_POINT('Ctrl Pts',(4.1463324212082,-0.172283981752003,32.2735773879748));
#66109=CARTESIAN_POINT('Ctrl Pts',(3.68515181888459,-1.39264150410918,32.2072819713081));
#66110=CARTESIAN_POINT('Ctrl Pts',(3.22397121656098,-2.61299902646635,32.1409865546415));
#66111=CARTESIAN_POINT('Ctrl Pts',(2.0963349511636,-3.5814988608208,32.0746911379748));
#66112=CARTESIAN_POINT('Ctrl Pts',(0.820340928864169,-3.85315909970353,
32.0083957213081));
#66113=CARTESIAN_POINT('Ctrl Pts',(-0.455653093435257,-4.12481933858626,
31.9421003046414));
#66114=CARTESIAN_POINT('Ctrl Pts',(-1.88000487263673,-3.69963998199727,
31.8758048879748));
#66115=CARTESIAN_POINT('Ctrl Pts',(-2.79828913252171,-2.77297173047393,
31.8095094713081));
#66116=CARTESIAN_POINT('Ctrl Pts',(-3.51554203489395,-2.04917026509265,
31.7577274882171));
#66117=CARTESIAN_POINT('Ctrl Pts',(-3.9240507341067,-1.01941794661383,31.705945505126));
#66118=CARTESIAN_POINT('Ctrl Pts',(-3.93356382969395,0.00360218745272173,
31.654163522035));
#66119=CARTESIAN_POINT('Ctrl Pts',(-3.93922268899305,-0.000712863612796303,
31.470836477965));
#66120=CARTESIAN_POINT('Ctrl Pts',(-3.93932022391611,-0.0395917322542401,
31.4728117924726));
#66121=CARTESIAN_POINT('Ctrl Pts',(-3.93879416874135,-0.0784678966759154,
31.4747871069802));
#66122=CARTESIAN_POINT('Ctrl Pts',(-3.93763638107598,-0.117325238088634,
31.4767624214878));
#66123=CARTESIAN_POINT('Ctrl Pts',(-3.89895835141275,-1.41542630510057,
31.5427514412393));
#66124=CARTESIAN_POINT('Ctrl Pts',(-3.15525606232387,-2.69252057232445,
31.6087404609909));
#66125=CARTESIAN_POINT('Ctrl Pts',(-2.04534050789141,-3.36679783887364,
31.6747294807424));
#66126=CARTESIAN_POINT('Ctrl Pts',(-0.935424953458954,-4.04107510542283,
31.740718500494));
#66127=CARTESIAN_POINT('Ctrl Pts',(0.540703866317046,-4.11253537129732,
31.8067075202455));
#66128=CARTESIAN_POINT('Ctrl Pts',(1.71056089907212,-3.5486232388958,31.8726965399971));
#66129=CARTESIAN_POINT('Ctrl Pts',(2.88041793182723,-2.98471110649425,31.9386855597486));
#66130=CARTESIAN_POINT('Ctrl Pts',(3.74400317756135,-1.78542657581666,32.0046745795002));
#66131=CARTESIAN_POINT('Ctrl Pts',(3.9078901538305,-0.4971318000896,32.0706635992517));
#66132=CARTESIAN_POINT('Ctrl Pts',(4.07177713009964,0.79116297563746,32.1366526190033));
#66133=CARTESIAN_POINT('Ctrl Pts',(3.53596583690379,2.16846799641394,32.2026416387548));
#66134=CARTESIAN_POINT('Ctrl Pts',(2.54455765667983,3.00731970580081,32.2686306585064));
#66135=CARTESIAN_POINT('Ctrl Pts',(1.55314947645591,3.84617141518765,32.3346196782579));
#66136=CARTESIAN_POINT('Ctrl Pts',(0.106144409203796,4.14656981318491,32.4006086980095));
#66137=CARTESIAN_POINT('Ctrl Pts',(-1.13724050020451,3.77166137474724,32.466597717761));
#66138=CARTESIAN_POINT('Ctrl Pts',(-2.38062540961286,3.39675293630955,32.5325867375126));
#66139=CARTESIAN_POINT('Ctrl Pts',(-3.42039016117747,2.34653766143695,32.5985757572641));
#66140=CARTESIAN_POINT('Ctrl Pts',(-3.78284557273839,1.09946571291651,32.6645647770157));
#66141=CARTESIAN_POINT('Ctrl Pts',(-3.88587272585993,0.744988255839808,
32.6833220106655));
#66142=CARTESIAN_POINT('Ctrl Pts',(-3.93417544392954,0.374605407215546,
32.7020792443153));
#66143=CARTESIAN_POINT('Ctrl Pts',(-3.93104799417585,0.00342476555473607,
32.7208364779651));
#66144=CARTESIAN_POINT('Origin',(0.,0.,0.));
#66145=CARTESIAN_POINT('',(-3.93387845178167,-0.00357291855290098,34.1541635220349));
#66146=CARTESIAN_POINT('',(-3.92762769288195,-0.00197752355235662,33.9708364779651));
#66147=CARTESIAN_POINT('',(-3.933,-4.81653586104654E-16,0.));
#66148=CARTESIAN_POINT('Ctrl Pts',(-3.93387845178167,-0.00357291855290098,
34.1541635220349));
#66149=CARTESIAN_POINT('Ctrl Pts',(-3.92427200125995,1.02950432289123,34.101861755126));
#66150=CARTESIAN_POINT('Ctrl Pts',(-3.50662895259015,2.0694535888524,34.0495599882171));
#66151=CARTESIAN_POINT('Ctrl Pts',(-2.77646841359207,2.79481975000012,33.9972582213081));
#66152=CARTESIAN_POINT('Ctrl Pts',(-1.85094906640237,3.71426195494336,33.9309628046415));
#66153=CARTESIAN_POINT('Ctrl Pts',(-0.423308453033832,4.12826407478453,
33.8646673879748));
#66154=CARTESIAN_POINT('Ctrl Pts',(0.850517079696137,3.84661084392644,33.7983719713081));
#66155=CARTESIAN_POINT('Ctrl Pts',(2.12434261242611,3.56495761306834,33.7320765546414));
#66156=CARTESIAN_POINT('Ctrl Pts',(3.24435306451751,2.58764903151097,33.6657811379748));
#66157=CARTESIAN_POINT('Ctrl Pts',(3.69595424636158,1.36371422812528,33.5994857213081));
#66158=CARTESIAN_POINT('Ctrl Pts',(4.14755542820564,0.139779424739578,33.5331903046415));
#66159=CARTESIAN_POINT('Ctrl Pts',(3.93074733980237,-1.33078160047445,33.4668948879748));
#66160=CARTESIAN_POINT('Ctrl Pts',(3.14514350025717,-2.3723125110148,33.4005994713081));
#66161=CARTESIAN_POINT('Ctrl Pts',(2.35953966071195,-3.41384342155519,33.3343040546414));
#66162=CARTESIAN_POINT('Ctrl Pts',(1.00514007002477,-4.02634421742187,33.2680086379748));
#66163=CARTESIAN_POINT('Ctrl Pts',(-0.295769865086573,-3.92839846173285,
33.2017132213081));
#66164=CARTESIAN_POINT('Ctrl Pts',(-1.59667980019788,-3.83045270604383,
33.1354178046415));
#66165=CARTESIAN_POINT('Ctrl Pts',(-2.84410007973336,-3.02206039879914,
33.0691223879748));
#66166=CARTESIAN_POINT('Ctrl Pts',(-3.46489745604721,-1.87464127402288,
33.0028269713081));
#66167=CARTESIAN_POINT('Ctrl Pts',(-3.77286248855624,-1.30542983475844,
32.9699391548837));
#66168=CARTESIAN_POINT('Ctrl Pts',(-3.92661865822607,-0.65278553701605,
32.9370513384593));
#66169=CARTESIAN_POINT('Ctrl Pts',(-3.92649272786585,-8.54312940767876E-5,
32.904163522035));
#66170=CARTESIAN_POINT('Ctrl Pts',(-3.93104799417585,0.00342476555473607,
32.7208364779651));
#66171=CARTESIAN_POINT('Ctrl Pts',(-3.92317289699638,-0.931229299076759,
32.7680682640668));
#66172=CARTESIAN_POINT('Ctrl Pts',(-3.58919907311395,-1.87094185961445,
32.8153000501685));
#66173=CARTESIAN_POINT('Ctrl Pts',(-2.9817228678744,-2.57450465531943,32.8625318362703));
#66174=CARTESIAN_POINT('Ctrl Pts',(-2.13299867989226,-3.5574744528668,32.9285208560218));
#66175=CARTESIAN_POINT('Ctrl Pts',(-0.750404232370731,-4.07948542579326,
32.9945098757734));
#66176=CARTESIAN_POINT('Ctrl Pts',(0.536187196027154,-3.9027232507419,33.0604988955249));
#66177=CARTESIAN_POINT('Ctrl Pts',(1.82277862442504,-3.72596107569055,33.1264879152765));
#66178=CARTESIAN_POINT('Ctrl Pts',(3.01336703369929,-2.85042575266138,33.192476935028));
#66179=CARTESIAN_POINT('Ctrl Pts',(3.56555199237859,-1.67498790166057,33.2584659547796));
#66180=CARTESIAN_POINT('Ctrl Pts',(4.11773695105789,-0.499550050659755,
33.3244549745311));
#66181=CARTESIAN_POINT('Ctrl Pts',(4.03151845914224,0.9757903283127,33.3904439942827));
#66182=CARTESIAN_POINT('Ctrl Pts',(3.34617536971732,2.07890737556271,33.4564330140342));
#66183=CARTESIAN_POINT('Ctrl Pts',(2.66083228029241,3.18202442281269,33.5224220337857));
#66184=CARTESIAN_POINT('Ctrl Pts',(1.37636459335825,3.91291813834024,33.5884110535373));
#66185=CARTESIAN_POINT('Ctrl Pts',(0.0779416438280532,3.938612773708,33.6544000732888));
#66186=CARTESIAN_POINT('Ctrl Pts',(-1.22048130570222,3.96430740907576,33.7203890930404));
#66187=CARTESIAN_POINT('Ctrl Pts',(-2.53285951782854,3.28480296428364,33.786378112792));
#66188=CARTESIAN_POINT('Ctrl Pts',(-3.26130836427971,2.20966360203028,33.8523671325435));
#66189=CARTESIAN_POINT('Ctrl Pts',(-3.69723370628901,1.56626839798642,33.8918569143507));
#66190=CARTESIAN_POINT('Ctrl Pts',(-3.92404344920073,0.781189220414063,
33.9313466961579));
#66191=CARTESIAN_POINT('Ctrl Pts',(-3.92762769288195,-0.00197752355235662,
33.9708364779651));
#66192=CARTESIAN_POINT('Origin',(0.,0.,0.));
#66193=CARTESIAN_POINT('',(-3.93859184179281,0.0017323510934187,35.4041635220349));
#66194=CARTESIAN_POINT('',(-3.93814916617749,-0.00196197512325486,35.2208364779651));
#66195=CARTESIAN_POINT('',(-3.933,-4.81653586104654E-16,0.));
#66196=CARTESIAN_POINT('Ctrl Pts',(-3.93859184179281,0.0017323510934187,
35.4041635220349));
#66197=CARTESIAN_POINT('Ctrl Pts',(-3.93912260889036,0.0982274365966933,
35.399263005126));
#66198=CARTESIAN_POINT('Ctrl Pts',(-3.93588505782954,0.194686303980022,
35.3943624882171));
#66199=CARTESIAN_POINT('Ctrl Pts',(-3.92876520998431,0.290857753704378,
35.3894619713081));
#66200=CARTESIAN_POINT('Ctrl Pts',(-3.8324461301253,1.5918891447566,35.3231665546415));
#66201=CARTESIAN_POINT('Ctrl Pts',(-3.02561416698513,2.84031921217913,35.2568711379748));
#66202=CARTESIAN_POINT('Ctrl Pts',(-1.87897215434241,3.46255077964548,35.1905757213081));
#66203=CARTESIAN_POINT('Ctrl Pts',(-0.732330141699747,4.08478234711179,
35.1242803046415));
#66204=CARTESIAN_POINT('Ctrl Pts',(0.754121920445437,4.08081541462198,35.0579848879748));
#66205=CARTESIAN_POINT('Ctrl Pts',(1.89742648602436,3.45247259625468,34.9916894713081));
#66206=CARTESIAN_POINT('Ctrl Pts',(3.04073105160337,2.82412977788732,34.9253940546415));
#66207=CARTESIAN_POINT('Ctrl Pts',(3.84088812061606,1.57141107364234,34.8590986379748));
#66208=CARTESIAN_POINT('Ctrl Pts',(3.93026167685899,0.26988412422172,34.7928032213081));
#66209=CARTESIAN_POINT('Ctrl Pts',(4.01963523310191,-1.03164282519879,34.7265078046414));
#66210=CARTESIAN_POINT('Ctrl Pts',(3.39822527657522,-2.38197801979493,34.6602123879748));
#66211=CARTESIAN_POINT('Ctrl Pts',(2.35154160189833,-3.16070346248766,34.5939169713081));
#66212=CARTESIAN_POINT('Ctrl Pts',(1.3048579272214,-3.93942890518042,34.5276215546415));
#66213=CARTESIAN_POINT('Ctrl Pts',(-0.16709946560576,-4.14654459596973,
34.4613261379748));
#66214=CARTESIAN_POINT('Ctrl Pts',(-1.38803267274777,-3.68689023274352,
34.3950307213081));
#66215=CARTESIAN_POINT('Ctrl Pts',(-2.60896587988981,-3.22723586951729,
34.3287353046414));
#66216=CARTESIAN_POINT('Ctrl Pts',(-3.57887490134668,-2.10081145227551,
34.2624398879748));
#66217=CARTESIAN_POINT('Ctrl Pts',(-3.85213037156966,-0.825158098631946,
34.1961444713081));
#66218=CARTESIAN_POINT('Ctrl Pts',(-3.90980919066372,-0.55589293460251,
34.1821508215504));
#66219=CARTESIAN_POINT('Ctrl Pts',(-3.93644871492879,-0.279978897620677,
34.1681571717927));
#66220=CARTESIAN_POINT('Ctrl Pts',(-3.93387845178167,-0.00357291855290098,
34.1541635220349));
#66221=CARTESIAN_POINT('Ctrl Pts',(-3.92762769288195,-0.00197752355235662,
33.9708364779651));
#66222=CARTESIAN_POINT('Ctrl Pts',(-3.93003286510151,-0.52751402815515,
33.9973357159094));
#66223=CARTESIAN_POINT('Ctrl Pts',(-3.83192067024081,-1.05218937311693,
34.0238349538538));
#66224=CARTESIAN_POINT('Ctrl Pts',(-3.62902757271598,-1.53261357085699,
34.0503341917981));
#66225=CARTESIAN_POINT('Ctrl Pts',(-3.12377845392507,-2.72897710177648,
34.1163232115497));
#66226=CARTESIAN_POINT('Ctrl Pts',(-1.9687607355672,-3.65092988390098,34.1823122313012));
#66227=CARTESIAN_POINT('Ctrl Pts',(-0.690169787889638,-3.8784547367334,
34.2483012510528));
#66228=CARTESIAN_POINT('Ctrl Pts',(0.588421159787958,-4.10597958956582,
34.3142902708043));
#66229=CARTESIAN_POINT('Ctrl Pts',(1.99058533678528,-3.63907651310612,34.3802792905558));
#66230=CARTESIAN_POINT('Ctrl Pts',(2.87753401594177,-2.69045413789849,34.4462683103074));
#66231=CARTESIAN_POINT('Ctrl Pts',(3.76448269509826,-1.74183176269087,34.512257330059));
#66232=CARTESIAN_POINT('Ctrl Pts',(4.13621587641395,-0.311490088735288,
34.5782463498105));
#66233=CARTESIAN_POINT('Ctrl Pts',(3.8233818036528,0.948945238063219,34.6442353695621));
#66234=CARTESIAN_POINT('Ctrl Pts',(3.51054773089165,2.20938056486173,34.7102243893136));
#66235=CARTESIAN_POINT('Ctrl Pts',(2.51314640405376,3.2999095445031,34.7762134090651));
#66236=CARTESIAN_POINT('Ctrl Pts',(1.28556735528643,3.72371616206282,34.8422024288167));
#66237=CARTESIAN_POINT('Ctrl Pts',(0.0579883065191089,4.14752277962253,
34.9081914485682));
#66238=CARTESIAN_POINT('Ctrl Pts',(-1.39976846417762,3.9046070351005,34.9741804683198));
#66239=CARTESIAN_POINT('Ctrl Pts',(-2.42358772202978,3.10563488431345,35.0401694880713));
#66240=CARTESIAN_POINT('Ctrl Pts',(-3.35793682135874,2.37648381223565,35.1003918180359));
#66241=CARTESIAN_POINT('Ctrl Pts',(-3.93087693228753,1.18421586887302,35.1606141480005));
#66242=CARTESIAN_POINT('Ctrl Pts',(-3.93814916617749,-0.00196197512325486,
35.2208364779651));
#66243=CARTESIAN_POINT('Origin',(0.,0.,0.));
#66244=CARTESIAN_POINT('',(-3.92854696981776,0.00272907840631081,36.6541635220349));
#66245=CARTESIAN_POINT('',(-3.93324212187193,0.00353561962986205,36.4708364779651));
#66246=CARTESIAN_POINT('',(-3.933,-4.81653586104654E-16,0.));
#66247=CARTESIAN_POINT('Ctrl Pts',(-3.92854696981776,0.00272907840631081,
36.6541635220349));
#66248=CARTESIAN_POINT('Ctrl Pts',(-3.93154855147801,0.474347357201858,
36.6303688384593));
#66249=CARTESIAN_POINT('Ctrl Pts',(-3.85305357694903,0.944999852833924,
36.6065741548837));
#66250=CARTESIAN_POINT('Ctrl Pts',(-3.6886229876758,1.38342200393479,36.5827794713081));
#66251=CARTESIAN_POINT('Ctrl Pts',(-3.23049567558203,2.60492928268355,36.5164840546415));
#66252=CARTESIAN_POINT('Ctrl Pts',(-2.10528466290456,3.57624532739106,36.4501886379748));
#66253=CARTESIAN_POINT('Ctrl Pts',(-0.829973923421927,3.85109544722928,
36.3838932213081));
#66254=CARTESIAN_POINT('Ctrl Pts',(0.445336816060738,4.12594556706751,36.3175978046415));
#66255=CARTESIAN_POINT('Ctrl Pts',(1.87074728234857,3.7043297620364,36.2513023879748));
#66256=CARTESIAN_POINT('Ctrl Pts',(2.79134596938285,2.77996084689474,36.1850069713081));
#66257=CARTESIAN_POINT('Ctrl Pts',(3.71194465641712,1.8555919317531,36.1187115546415));
#66258=CARTESIAN_POINT('Ctrl Pts',(4.12773156419788,0.428469906500936,36.0524161379748));
#66259=CARTESIAN_POINT('Ctrl Pts',(3.84767129915961,-0.845706838817057,
35.9861207213081));
#66260=CARTESIAN_POINT('Ctrl Pts',(3.56761103412134,-2.11988358413505,35.9198253046414));
#66261=CARTESIAN_POINT('Ctrl Pts',(2.59170359626402,-3.24111504951888,35.8535298879748));
#66262=CARTESIAN_POINT('Ctrl Pts',(1.36833440376772,-3.69424620751226,35.7872344713082));
#66263=CARTESIAN_POINT('Ctrl Pts',(0.144965211271464,-4.14737736550564,
35.7209390546415));
#66264=CARTESIAN_POINT('Ctrl Pts',(-1.32586573586376,-3.93240821610861,
35.6546436379748));
#66265=CARTESIAN_POINT('Ctrl Pts',(-2.36837811114245,-3.14810728406921,
35.5883482213081));
#66266=CARTESIAN_POINT('Ctrl Pts',(-3.3338286052278,-2.42178140026698,35.5269533215504));
#66267=CARTESIAN_POINT('Ctrl Pts',(-3.93194225903368,-1.207182180102,35.4655584217927));
#66268=CARTESIAN_POINT('Ctrl Pts',(-3.93859184179281,0.0017323510934187,
35.4041635220349));
#66269=CARTESIAN_POINT('Ctrl Pts',(-3.93814916617749,-0.00196197512325486,
35.2208364779651));
#66270=CARTESIAN_POINT('Ctrl Pts',(-3.93884553107946,-0.115546415687587,
35.226603167752));
#66271=CARTESIAN_POINT('Ctrl Pts',(-3.93435509495706,-0.229075014060918,
35.232369857539));
#66272=CARTESIAN_POINT('Ctrl Pts',(-3.92449851330675,-0.342135794579535,
35.238136547326));
#66273=CARTESIAN_POINT('Ctrl Pts',(-3.8117083017239,-1.63590576563339,35.3041255670775));
#66274=CARTESIAN_POINT('Ctrl Pts',(-2.99624613355058,-2.86841715068901,
35.3701145868291));
#66275=CARTESIAN_POINT('Ctrl Pts',(-1.84961489770968,-3.47817052594584,
35.4361036065806));
#66276=CARTESIAN_POINT('Ctrl Pts',(-0.702983661868818,-4.08792390120266,
35.5020926263321));
#66277=CARTESIAN_POINT('Ctrl Pts',(0.774816641639593,-4.07491926666073,
35.5680816460837));
#66278=CARTESIAN_POINT('Ctrl Pts',(1.91053947962039,-3.44508118611152,35.6340706658352));
#66279=CARTESIAN_POINT('Ctrl Pts',(3.04626231760121,-2.81524310556228,35.7000596855868));
#66280=CARTESIAN_POINT('Ctrl Pts',(3.8399076900544,-1.56857157900572,35.7660487053384));
#66281=CARTESIAN_POINT('Ctrl Pts',(3.92991185646822,-0.273017019234441,
35.8320377250899));
#66282=CARTESIAN_POINT('Ctrl Pts',(4.01991602288204,1.02253754053684,35.8980267448414));
#66283=CARTESIAN_POINT('Ctrl Pts',(3.40627898325649,2.36697513352282,35.964015764593));
#66284=CARTESIAN_POINT('Ctrl Pts',(2.36855747134988,3.147805737116,36.0300047843445));
#66285=CARTESIAN_POINT('Ctrl Pts',(1.33083595944332,3.92863634070914,36.0959938040961));
#66286=CARTESIAN_POINT('Ctrl Pts',(-0.130970024744263,4.14585995490953,
36.1619828238476));
#66287=CARTESIAN_POINT('Ctrl Pts',(-1.35090055112145,3.70051526108771,36.2279718435992));
#66288=CARTESIAN_POINT('Ctrl Pts',(-2.57083107749874,3.25517056726585,36.2939608633507));
#66289=CARTESIAN_POINT('Ctrl Pts',(-3.54888614606559,2.14725756542165,36.3599498831023));
#66290=CARTESIAN_POINT('Ctrl Pts',(-3.83948982933842,0.881511996143767,
36.4259389028538));
#66291=CARTESIAN_POINT('Ctrl Pts',(-3.90539675722059,0.594449557663731,
36.4409047612242));
#66292=CARTESIAN_POINT('Ctrl Pts',(-3.9359445283657,0.299268979327574,36.4558706195946));
#66293=CARTESIAN_POINT('Ctrl Pts',(-3.93324212187193,0.00353561962986205,
36.4708364779651));
#66294=CARTESIAN_POINT('Origin',(0.,0.,0.));
#66295=CARTESIAN_POINT('',(-3.92861605367513,-0.00280348551048665,37.9041635220349));
#66296=CARTESIAN_POINT('',(-3.92680078726362,-0.000862425370787758,37.7208364779651));
#66297=CARTESIAN_POINT('',(-3.933,-4.81653586104654E-16,0.));
#66298=CARTESIAN_POINT('Ctrl Pts',(-3.92861605367513,-0.00280348551048665,
37.9041635220349));
#66299=CARTESIAN_POINT('Ctrl Pts',(-3.92314714083183,0.843271536769385,
37.8614746717927));
#66300=CARTESIAN_POINT('Ctrl Pts',(-3.65525453228082,1.69252296329638,37.8187858215504));
#66301=CARTESIAN_POINT('Ctrl Pts',(-3.15107129829004,2.36445631166207,37.7760969713081));
#66302=CARTESIAN_POINT('Ctrl Pts',(-2.36807907938348,3.40796301304478,37.7098015546415));
#66303=CARTESIAN_POINT('Ctrl Pts',(-1.01520532603393,4.02381712229028,37.6435061379748));
#66304=CARTESIAN_POINT('Ctrl Pts',(0.285947880721249,3.92911729405849,37.5772107213081));
#66305=CARTESIAN_POINT('Ctrl Pts',(1.58710108747643,3.8344174658267,37.5109153046415));
#66306=CARTESIAN_POINT('Ctrl Pts',(2.83653374763726,3.02916370011762,37.4446198879748));
#66307=CARTESIAN_POINT('Ctrl Pts',(3.46019728219322,1.88330455174309,37.3783244713081));
#66308=CARTESIAN_POINT('Ctrl Pts',(4.08386081674918,0.737445403368564,37.3120290546415));
#66309=CARTESIAN_POINT('Ctrl Pts',(4.08175522570026,-0.749019127671417,
37.2457336379748));
#66310=CARTESIAN_POINT('Ctrl Pts',(3.45484308914238,-1.89311051940086,37.1794382213081));
#66311=CARTESIAN_POINT('Ctrl Pts',(2.82793095258448,-3.03720191113034,37.1131428046415));
#66312=CARTESIAN_POINT('Ctrl Pts',(1.57621227051757,-3.83892016354926,37.0468473879748));
#66313=CARTESIAN_POINT('Ctrl Pts',(0.274797744277373,-3.92991993716301,
36.9805519713081));
#66314=CARTESIAN_POINT('Ctrl Pts',(-1.02661678196279,-4.02091971077676,
36.9142565546415));
#66315=CARTESIAN_POINT('Ctrl Pts',(-2.37772715237623,-3.40120100558538,
36.8479611379748));
#66316=CARTESIAN_POINT('Ctrl Pts',(-3.15776053182792,-2.35549239659468,
36.7816657213081));
#66317=CARTESIAN_POINT('Ctrl Pts',(-3.65782512345545,-1.68510845881512,
36.7391649882171));
#66318=CARTESIAN_POINT('Ctrl Pts',(-3.92318571251892,-0.839649116044735,
36.696664255126));
#66319=CARTESIAN_POINT('Ctrl Pts',(-3.92854696981776,0.00272907840631081,
36.6541635220349));
#66320=CARTESIAN_POINT('Ctrl Pts',(-3.93324212187193,0.00353561962986205,
36.4708364779651));
#66321=CARTESIAN_POINT('Ctrl Pts',(-3.92402879649918,-1.00470931789247,
36.5218596393462));
#66322=CARTESIAN_POINT('Ctrl Pts',(-3.52833688498228,-2.01937942887946,
36.5728828007273));
#66323=CARTESIAN_POINT('Ctrl Pts',(-2.82974005739278,-2.74067810778768,
36.6239059621085));
#66324=CARTESIAN_POINT('Ctrl Pts',(-1.92623430419552,-3.67354450572974,
36.68989498186));
#66325=CARTESIAN_POINT('Ctrl Pts',(-0.516070499822165,-4.1156991649024,
36.7558840016115));
#66326=CARTESIAN_POINT('Ctrl Pts',(0.758318344745277,-3.86570807659067,
36.8218730213631));
#66327=CARTESIAN_POINT('Ctrl Pts',(2.03270718931276,-3.61571698827893,36.8878620411146));
#66328=CARTESIAN_POINT('Ctrl Pts',(3.17132107407428,-2.67358015248279,36.9538510608662));
#66329=CARTESIAN_POINT('Ctrl Pts',(3.6554375232991,-1.46851025784295,37.0198400806177));
#66330=CARTESIAN_POINT('Ctrl Pts',(4.13955397252392,-0.263440363203115,
37.0858291003693));
#66331=CARTESIAN_POINT('Ctrl Pts',(3.96917298621199,1.20456259028048,37.1518181201208));
#66332=CARTESIAN_POINT('Ctrl Pts',(3.22191610266395,2.26671584208094,37.2178071398724));
#66333=CARTESIAN_POINT('Ctrl Pts',(2.47465921911595,3.32886909388133,37.2837961596239));
#66334=CARTESIAN_POINT('Ctrl Pts',(1.15052643833195,3.98517264399873,37.3497851793755));
#66335=CARTESIAN_POINT('Ctrl Pts',(-0.147243479843609,3.93663134576437,
37.415774199127));
#66336=CARTESIAN_POINT('Ctrl Pts',(-1.44501339801924,3.88809004753,37.4817632188786));
#66337=CARTESIAN_POINT('Ctrl Pts',(-2.71642045358641,3.1347039009438,37.5477522386301));
#66338=CARTESIAN_POINT('Ctrl Pts',(-3.38224359437478,2.0196969376997,37.6137412583817));
#66339=CARTESIAN_POINT('Ctrl Pts',(-3.7424372333312,1.41650610375378,37.6494396649095));
#66340=CARTESIAN_POINT('Ctrl Pts',(-3.92540438127228,0.707485529535139,
37.6851380714373));
#66341=CARTESIAN_POINT('Ctrl Pts',(-3.92680078726362,-0.000862425370787757,
37.7208364779651));
#66342=CARTESIAN_POINT('Origin',(0.,0.,0.));
#66343=CARTESIAN_POINT('',(-3.93300000000003,-4.81653586104657E-16,39.067));
#66344=CARTESIAN_POINT('',(-3.936306081373,-0.00286452337122285,38.970836477965));
#66345=CARTESIAN_POINT('',(-3.933,-4.81653586104654E-16,0.));
#66346=CARTESIAN_POINT('',(-3.55519577774135,1.66475697885233,39.067));
#66347=CARTESIAN_POINT('Origin',(0.,0.,39.067));
#66348=CARTESIAN_POINT('Ctrl Pts',(-3.55517835630003,1.66474646536772,39.067));
#66349=CARTESIAN_POINT('Ctrl Pts',(-3.281770047254,2.25009079435063,39.0344714904361));
#66350=CARTESIAN_POINT('Ctrl Pts',(-2.87218003711123,2.77178961343465,39.0019429808721));
#66351=CARTESIAN_POINT('Ctrl Pts',(-2.35968662710541,3.15555731452043,38.9694144713081));
#66352=CARTESIAN_POINT('Ctrl Pts',(-1.31518859720181,3.93770319171364,38.9031190546415));
#66353=CARTESIAN_POINT('Ctrl Pts',(0.156742781769128,4.1469198966438,38.8368236379748));
#66354=CARTESIAN_POINT('Ctrl Pts',(1.37894059931111,3.68993834295183,38.7705282213081));
#66355=CARTESIAN_POINT('Ctrl Pts',(2.60113841685301,3.23295678925989,38.7042328046414));
#66356=CARTESIAN_POINT('Ctrl Pts',(3.57360267296599,2.10977697694588,38.6379373879748));
#66357=CARTESIAN_POINT('Ctrl Pts',(3.84998555909052,0.835006136376253,38.5716419713081));
#66358=CARTESIAN_POINT('Ctrl Pts',(4.12636844521508,-0.439764704193487,
38.5053465546415));
#66359=CARTESIAN_POINT('Ctrl Pts',(3.70666996135107,-1.86612657301888,38.4390511379748));
#66360=CARTESIAN_POINT('Ctrl Pts',(2.78348499916481,-2.78798189487759,38.3727557213081));
#66361=CARTESIAN_POINT('Ctrl Pts',(1.86030003697863,-3.70983721673622,38.3064603046415));
#66362=CARTESIAN_POINT('Ctrl Pts',(0.433628596470313,-4.12718599162826,
38.2401648879748));
#66363=CARTESIAN_POINT('Ctrl Pts',(-0.840914130798121,-3.84866608078101,
38.1738694713081));
#66364=CARTESIAN_POINT('Ctrl Pts',(-2.11545685806663,-3.57014616993374,
38.1075740546415));
#66365=CARTESIAN_POINT('Ctrl Pts',(-3.23787087209523,-2.59575757334711,
38.0412786379748));
#66366=CARTESIAN_POINT('Ctrl Pts',(-3.69252253687772,-1.37298362829381,
37.9749832213081));
#66367=CARTESIAN_POINT('Ctrl Pts',(-3.8544155494613,-0.937576539730567,
37.9513766548837));
#66368=CARTESIAN_POINT('Ctrl Pts',(-3.93164031536341,-0.470675683991357,
37.9277700884593));
#66369=CARTESIAN_POINT('Ctrl Pts',(-3.92861605367513,-0.00280348551048665,
37.9041635220349));
#66370=CARTESIAN_POINT('Ctrl Pts',(-3.92680078726362,-0.000862425370787757,
37.7208364779651));
#66371=CARTESIAN_POINT('Ctrl Pts',(-3.92798565790354,-0.60190588968295,
37.7511270911888));
#66372=CARTESIAN_POINT('Ctrl Pts',(-3.79844381669874,-1.20246508373146,
37.7814177044126));
#66373=CARTESIAN_POINT('Ctrl Pts',(-3.53552131443984,-1.73747658063651,
37.8117083176363));
#66374=CARTESIAN_POINT('Ctrl Pts',(-2.96273666770691,-2.90301535582683,
37.8776973373879));
#66375=CARTESIAN_POINT('Ctrl Pts',(-1.75692814823142,-3.75746512630542,
37.9436863571394));
#66376=CARTESIAN_POINT('Ctrl Pts',(-0.467423498028026,-3.91155642168368,
38.0096753768909));
#66377=CARTESIAN_POINT('Ctrl Pts',(0.822081152175291,-4.06564771706194,
38.0756643966425));
#66378=CARTESIAN_POINT('Ctrl Pts',(2.19528193310649,-3.51938053733994,38.141653416394));
#66379=CARTESIAN_POINT('Ctrl Pts',(3.02657250539957,-2.52162900267819,38.2076424361456));
#66380=CARTESIAN_POINT('Ctrl Pts',(3.85786307769267,-1.52387746801641,38.2736314558971));
#66381=CARTESIAN_POINT('Ctrl Pts',(4.14724344134762,-0.074641578414862,
38.3396204756487));
#66382=CARTESIAN_POINT('Ctrl Pts',(3.76290363779945,1.16586313888606,38.4056094954002));
#66383=CARTESIAN_POINT('Ctrl Pts',(3.37856383425128,2.40636785618698,38.4715985151518));
#66384=CARTESIAN_POINT('Ctrl Pts',(2.3205038635,3.43814140118727,38.5375875349033));
#66385=CARTESIAN_POINT('Ctrl Pts',(1.07070171926435,3.79110107416724,38.6035765546549));
#66386=CARTESIAN_POINT('Ctrl Pts',(-0.179100424971232,4.14406074714718,
38.6695655744064));
#66387=CARTESIAN_POINT('Ctrl Pts',(-1.62064474269115,3.81820654810687,38.7355545941579));
#66388=CARTESIAN_POINT('Ctrl Pts',(-2.5971139356278,2.96205423396555,38.8015436139095));
#66389=CARTESIAN_POINT('Ctrl Pts',(-3.43214814261489,2.22990981623014,38.8579745685947));
#66390=CARTESIAN_POINT('Ctrl Pts',(-3.92707614700865,1.10996207692717,38.9144055232799));
#66391=CARTESIAN_POINT('Ctrl Pts',(-3.936306081373,-0.00286452337122285,
38.970836477965));
#66392=CARTESIAN_POINT('Origin',(0.,0.,-2.31077344927314));
#66393=CARTESIAN_POINT('',(-3.22696940764995,-0.00257222088861585,39.5642265507268));
#66394=CARTESIAN_POINT('',(-3.22275,-3.94673047195213E-16,39.77725));
#66395=CARTESIAN_POINT('',(-3.22275,7.67147279210326E-13,-2.31077344927314));
#66396=CARTESIAN_POINT('',(-1.54513563095096,-2.82819261092058,39.7772500000001));
#66397=CARTESIAN_POINT('Ctrl Pts',(-3.22696940764995,-0.00257222088861592,
39.5642265507268));
#66398=CARTESIAN_POINT('Ctrl Pts',(-3.2273947683947,-0.0785187605428588,
39.5689389504846));
#66399=CARTESIAN_POINT('Ctrl Pts',(-3.19081253852192,-1.22220206883349,
39.639946766909));
#66400=CARTESIAN_POINT('Ctrl Pts',(-2.48759436411792,-2.31329607816883,
39.7109545833334));
#66401=CARTESIAN_POINT('Ctrl Pts',(-1.54513563095092,-2.82819261092061,
39.7772500000001));
#66402=CARTESIAN_POINT('Origin',(0.,0.,39.77725));
#66403=CARTESIAN_POINT('Origin',(0.,0.,-2.31077344927314));
#66404=CARTESIAN_POINT('',(-3.21915773887147,-0.00229721152486538,38.3142265507269));
#66405=CARTESIAN_POINT('',(-3.22545904493893,-0.00234722672036308,38.5607734492731));
#66406=CARTESIAN_POINT('',(-3.22275,7.67147279210326E-13,-2.31077344927314));
#66407=CARTESIAN_POINT('Ctrl Pts',(-3.21915773887147,-0.00229721152486602,
38.3142265507269));
#66408=CARTESIAN_POINT('Ctrl Pts',(-3.22163585719237,-0.385677615200072,
38.3378331171513));
#66409=CARTESIAN_POINT('Ctrl Pts',(-2.98064768969752,-1.8426918296433,38.4277351002423));
#66410=CARTESIAN_POINT('Ctrl Pts',(-0.813711880402819,-3.723849330995,38.5839325000001));
#66411=CARTESIAN_POINT('Ctrl Pts',(2.6933860485815,-2.69790671903219,38.7828187500001));
#66412=CARTESIAN_POINT('Ctrl Pts',(3.72510480439603,0.808430209081211,38.9817050000001));
#66413=CARTESIAN_POINT('Ctrl Pts',(1.33455622972935,3.56947348912338,39.1805912500001));
#66414=CARTESIAN_POINT('Ctrl Pts',(-2.19806823460843,3.06735493880013,39.3747651002423));
#66415=CARTESIAN_POINT('Ctrl Pts',(-3.22141066915511,0.989919349467212,
39.5026435338179));
#66416=CARTESIAN_POINT('Ctrl Pts',(-3.22696940764995,-0.00257222088861592,
39.5642265507268));
#66417=CARTESIAN_POINT('',(-3.17710367210759,0.540490350682096,39.7772500000001));
#66418=CARTESIAN_POINT('Origin',(0.,0.,39.77725));
#66419=CARTESIAN_POINT('Ctrl Pts',(-3.22545904493893,-0.00234722672036301,
38.5607734492731));
#66420=CARTESIAN_POINT('Ctrl Pts',(-3.2267400589162,-0.156795392107344,
38.5703315143395));
#66421=CARTESIAN_POINT('Ctrl Pts',(-3.14662046190347,-1.37623279221256,
38.6458785991574));
#66422=CARTESIAN_POINT('Ctrl Pts',(-1.59232210767045,-3.45719070782108,
38.7874147037269));
#66423=CARTESIAN_POINT('Ctrl Pts',(2.03356109694112,-3.21705406573836,38.9853817629815));
#66424=CARTESIAN_POINT('Ctrl Pts',(3.80457448616929,-0.0471873108411222,
39.1833488222361));
#66425=CARTESIAN_POINT('Ctrl Pts',(2.11292542611656,3.16852227003697,39.3813158814907));
#66426=CARTESIAN_POINT('Ctrl Pts',(-1.51168002663127,3.4916201787766,39.5792829407454));
#66427=CARTESIAN_POINT('Ctrl Pts',(-2.99782464886751,1.59432608031001,39.7112609802485));
#66428=CARTESIAN_POINT('Ctrl Pts',(-3.17710367210759,0.540490350682096,
39.7772500000001));
#66429=CARTESIAN_POINT('Origin',(0.,0.,-2.31077344927314));
#66430=CARTESIAN_POINT('',(-3.21910113068401,0.00223624140265653,37.0642265507269));
#66431=CARTESIAN_POINT('',(-3.21767028658882,-0.000706682268057368,37.3107734492731));
#66432=CARTESIAN_POINT('',(-3.22275,7.67147279210326E-13,-2.31077344927314));
#66433=CARTESIAN_POINT('Ctrl Pts',(-3.21910113068401,0.00223624140265662,
37.0642265507269));
#66434=CARTESIAN_POINT('Ctrl Pts',(-3.21470804856876,-0.688019117399231,
37.1067272838179));
#66435=CARTESIAN_POINT('Ctrl Pts',(-2.65809139214385,-2.46144279789799,
37.2155234335756));
#66436=CARTESIAN_POINT('Ctrl Pts',(0.265894155143361,-3.80259787822564,
37.3906150000001));
#66437=CARTESIAN_POINT('Ctrl Pts',(3.34291656752411,-1.83178361584359,37.58950125));
#66438=CARTESIAN_POINT('Ctrl Pts',(3.34809261142426,1.82229995960197,37.7883875000001));
#66439=CARTESIAN_POINT('Ctrl Pts',(0.276689784930593,3.80180535505515,37.98727375));
#66440=CARTESIAN_POINT('Ctrl Pts',(-2.65425757115236,2.46758184103052,38.1625534335757));
#66441=CARTESIAN_POINT('Ctrl Pts',(-3.21467644243972,0.690987374809255,
38.2715377004846));
#66442=CARTESIAN_POINT('Ctrl Pts',(-3.21915773887147,-0.00229721152486602,
38.3142265507269));
#66443=CARTESIAN_POINT('Ctrl Pts',(-3.21767028658882,-0.000706682268057576,
37.3107734492731));
#66444=CARTESIAN_POINT('Ctrl Pts',(-3.21864118459424,-0.493209307392164,
37.3410640624968));
#66445=CARTESIAN_POINT('Ctrl Pts',(-2.88124583165036,-2.05738254559314,
37.4373436954722));
#66446=CARTESIAN_POINT('Ctrl Pts',(-0.451594402129131,-3.77906146290628,
37.599612348199));
#66447=CARTESIAN_POINT('Ctrl Pts',(2.92405992033173,-2.43620673106119,37.7975794074536));
#66448=CARTESIAN_POINT('Ctrl Pts',(3.63542572274911,1.12635998382311,37.9955464667083));
#66449=CARTESIAN_POINT('Ctrl Pts',(1.03446251089667,3.6627049053714,38.1935135259629));
#66450=CARTESIAN_POINT('Ctrl Pts',(-2.33810477673144,2.90035219882563,38.3819225201512));
#66451=CARTESIAN_POINT('Ctrl Pts',(-3.21789591985027,0.909516980274446,
38.5043424945879));
#66452=CARTESIAN_POINT('Ctrl Pts',(-3.22545904493893,-0.00234722672036301,
38.5607734492731));
#66453=CARTESIAN_POINT('Origin',(0.,0.,-2.31077344927314));
#66454=CARTESIAN_POINT('',(-3.22733202596944,0.00141951042163625,35.8142265507269));
#66455=CARTESIAN_POINT('',(-3.22294839772763,0.00289713149391357,36.0607734492731));
#66456=CARTESIAN_POINT('',(-3.22275,7.67147279210326E-13,-2.31077344927314));
#66457=CARTESIAN_POINT('Ctrl Pts',(-3.22733202596944,0.00141951042163634,
35.8142265507269));
#66458=CARTESIAN_POINT('Ctrl Pts',(-3.22188327365915,-0.989180363824584,
35.8756214504846));
#66459=CARTESIAN_POINT('Ctrl Pts',(-2.20255972880747,-3.0591374276618,36.003311766909));
#66460=CARTESIAN_POINT('Ctrl Pts',(1.32400383155469,-3.57456197073556,36.1972975000001));
#66461=CARTESIAN_POINT('Ctrl Pts',(3.72301656637914,-0.818308191127896,
36.39618375));
#66462=CARTESIAN_POINT('Ctrl Pts',(2.7009133954788,2.68989738238965,36.5950700000001));
#66463=CARTESIAN_POINT('Ctrl Pts',(-0.803084758776685,3.72632936992902,
36.79395625));
#66464=CARTESIAN_POINT('Ctrl Pts',(-2.97803672572911,1.84884530856887,36.950341766909));
#66465=CARTESIAN_POINT('Ctrl Pts',(-3.22156066470263,0.388686230720639,
37.0404318671513));
#66466=CARTESIAN_POINT('Ctrl Pts',(-3.21910113068401,0.00223624140265662,
37.0642265507269));
#66467=CARTESIAN_POINT('Ctrl Pts',(-3.22294839772764,0.00289713149391371,
36.0607734492731));
#66468=CARTESIAN_POINT('Ctrl Pts',(-3.21539888225747,-0.823271536800272,
36.1117966106542));
#66469=CARTESIAN_POINT('Ctrl Pts',(-2.47182598037544,-2.73001053479381,
36.2288087917869));
#66470=CARTESIAN_POINT('Ctrl Pts',(0.732631374839026,-3.7347631354025,36.4118099926711));
#66471=CARTESIAN_POINT('Ctrl Pts',(3.53161527805439,-1.41876657738429,36.6097770519258));
#66472=CARTESIAN_POINT('Ctrl Pts',(3.11277826536447,2.18993404682541,36.8077441111804));
#66473=CARTESIAN_POINT('Ctrl Pts',(-0.14225523522422,3.80328436424815,37.0057111704351));
#66474=CARTESIAN_POINT('Ctrl Pts',(-2.78946082450622,2.23465375975559,37.1733876164659));
#66475=CARTESIAN_POINT('Ctrl Pts',(-3.21652605383795,0.579722601147174,
37.2750750427453));
#66476=CARTESIAN_POINT('Ctrl Pts',(-3.21767028658882,-0.000706682268057576,
37.3107734492731));
#66477=CARTESIAN_POINT('Origin',(0.,0.,-2.31077344927314));
#66478=CARTESIAN_POINT('',(-3.22346981451293,-0.00292769470226793,34.5642265507269));
#66479=CARTESIAN_POINT('',(-3.22696929196504,-0.00160766725765038,34.8107734492731));
#66480=CARTESIAN_POINT('',(-3.22275,7.67147279210326E-13,-2.31077344927314));
#66481=CARTESIAN_POINT('Ctrl Pts',(-3.22346981451293,-0.00292769470226783,
34.5642265507269));
#66482=CARTESIAN_POINT('Ctrl Pts',(-3.22557592068063,-0.229418253827942,
34.5782202004846));
#66483=CARTESIAN_POINT('Ctrl Pts',(-3.10033260871109,-1.52660312344819,
34.658509266909));
#66484=CARTESIAN_POINT('Ctrl Pts',(-1.34306394368559,-3.56744436540872,
34.8050937500001));
#66485=CARTESIAN_POINT('Ctrl Pts',(2.27535763353318,-3.05830470675803,35.00398));
#66486=CARTESIAN_POINT('Ctrl Pts',(3.80293119371364,0.261140562795601,35.2028662500001));
#66487=CARTESIAN_POINT('Ctrl Pts',(1.83595469168445,3.34062126768144,35.4017525000001));
#66488=CARTESIAN_POINT('Ctrl Pts',(-1.81809823225042,3.35037293181705,35.6006387500001));
#66489=CARTESIAN_POINT('Ctrl Pts',(-3.18922508991673,1.22879610595737,35.7381301002423));
#66490=CARTESIAN_POINT('Ctrl Pts',(-3.22776694324977,0.0804888053123557,
35.8093260338179));
#66491=CARTESIAN_POINT('Ctrl Pts',(-3.22733202596944,0.00141951042163634,
35.8142265507269));
#66492=CARTESIAN_POINT('Ctrl Pts',(-3.22696929196504,-0.00160766725764983,
34.8107734492731));
#66493=CARTESIAN_POINT('Ctrl Pts',(-3.22753990218318,-0.0946801960727776,
34.81654013906));
#66494=CARTESIAN_POINT('Ctrl Pts',(-3.18175512899714,-1.25222502802182,
34.8882958485986));
#66495=CARTESIAN_POINT('Ctrl Pts',(-1.78696199451318,-3.36035276851525,
35.0260405778887));
#66496=CARTESIAN_POINT('Ctrl Pts',(1.84582284769266,-3.32838428188693,35.2240076371433));
#66497=CARTESIAN_POINT('Ctrl Pts',(3.79679204988465,-0.263768978904437,
35.421974696398));
#66498=CARTESIAN_POINT('Ctrl Pts',(2.28832616929499,3.04117858234319,35.6199417556526));
#66499=CARTESIAN_POINT('Ctrl Pts',(-1.30514082959193,3.5751659222856,35.8179088149073));
#66500=CARTESIAN_POINT('Ctrl Pts',(-3.08976124773103,1.55359860142908,35.9648527127807));
#66501=CARTESIAN_POINT('Ctrl Pts',(-3.22516278382668,0.245224791032393,
36.0458075909027));
#66502=CARTESIAN_POINT('Ctrl Pts',(-3.22294839772764,0.00289713149391371,
36.0607734492731));
#66503=CARTESIAN_POINT('Origin',(0.,0.,-2.31077344927314));
#66504=CARTESIAN_POINT('',(-3.21741785881761,-7.00034835067217E-5,33.3142265507269));
#66505=CARTESIAN_POINT('',(-3.21834786352283,-0.00162040783760142,33.5607734492731));
#66506=CARTESIAN_POINT('',(-3.22275,7.67147279210326E-13,-2.31077344927314));
#66507=CARTESIAN_POINT('Ctrl Pts',(-3.21741785881761,-7.00034835066088E-5,
33.3142265507269));
#66508=CARTESIAN_POINT('Ctrl Pts',(-3.21752104774941,-0.534900734659731,
33.3471143671513));
#66509=CARTESIAN_POINT('Ctrl Pts',(-2.83756055391816,-2.14770788379053,
33.4462976002423));
#66510=CARTESIAN_POINT('Ctrl Pts',(-0.286187673586392,-3.80112834136171,
33.61177625));
#66511=CARTESIAN_POINT('Ctrl Pts',(3.0432488488294,-2.29545561834177,33.8106625000001));
#66512=CARTESIAN_POINT('Ctrl Pts',(3.57621472747308,1.31953335496755,34.00954875));
#66513=CARTESIAN_POINT('Ctrl Pts',(0.822962489122625,3.72199043445967,34.208435));
#66514=CARTESIAN_POINT('Ctrl Pts',(-2.43959062434672,2.7758812439376,34.3933276002424));
#66515=CARTESIAN_POINT('Ctrl Pts',(-3.21559816731754,0.843588877853916,
34.5119247838179));
#66516=CARTESIAN_POINT('Ctrl Pts',(-3.22346981451293,-0.00292769470226783,
34.5642265507269));
#66517=CARTESIAN_POINT('Ctrl Pts',(-3.21834786352283,-0.00162040783760153,
33.5607734492731));
#66518=CARTESIAN_POINT('Ctrl Pts',(-3.22031869209415,-0.432251674099872,
33.5872726872174));
#66519=CARTESIAN_POINT('Ctrl Pts',(-2.93972437209767,-1.93278809414023,
33.6797609449134));
#66520=CARTESIAN_POINT('Ctrl Pts',(-0.666791331988793,-3.74707795879318,
33.8382382223608));
#66521=CARTESIAN_POINT('Ctrl Pts',(2.78006191089306,-2.59931908033378,34.0362052816155));
#66522=CARTESIAN_POINT('Ctrl Pts',(3.69387053796041,0.916801155928787,34.2341723408701));
#66523=CARTESIAN_POINT('Ctrl Pts',(1.24202070877136,3.59758091881176,34.4321394001247));
#66524=CARTESIAN_POINT('Ctrl Pts',(-2.23710626490338,3.01783076015345,34.6243397695924));
#66525=CARTESIAN_POINT('Ctrl Pts',(-3.22101033143359,0.970361477603226,
34.7505511193085));
#66526=CARTESIAN_POINT('Ctrl Pts',(-3.22696929196504,-0.00160766725764983,
34.8107734492731));
#66527=CARTESIAN_POINT('Origin',(0.,0.,-2.31077344927314));
#66528=CARTESIAN_POINT('',(-3.22321200919049,0.00295167801057836,32.0642265507269));
#66529=CARTESIAN_POINT('',(-3.22115050171122,0.00280629626111237,32.3107734492731));
#66530=CARTESIAN_POINT('',(-3.22275,7.67147279210326E-13,-2.31077344927314));
#66531=CARTESIAN_POINT('Ctrl Pts',(-3.22321200919049,0.00295167801057841,
32.0642265507269));
#66532=CARTESIAN_POINT('Ctrl Pts',(-3.21541685821078,-0.835323973416723,
32.1160085338179));
#66533=CARTESIAN_POINT('Ctrl Pts',(-2.45212244763611,-2.75940586074536,
32.2340859335757));
#66534=CARTESIAN_POINT('Ctrl Pts',(0.793763968866624,-3.72832654331965,
32.41845875));
#66535=CARTESIAN_POINT('Ctrl Pts',(3.56576227116223,-1.34752346081344,32.6173450000001));
#66536=CARTESIAN_POINT('Ctrl Pts',(3.06114731919247,2.27153189325784,32.81623125));
#66537=CARTESIAN_POINT('Ctrl Pts',(-0.256385353190344,3.80325473806034,
33.0151175000001));
#66538=CARTESIAN_POINT('Ctrl Pts',(-2.82869405418981,2.16475235003571,33.1811159335757));
#66539=CARTESIAN_POINT('Ctrl Pts',(-3.21731303901023,0.543213595337759,
33.2808189504846));
#66540=CARTESIAN_POINT('Ctrl Pts',(-3.21741785881761,-7.00034835066088E-5,
33.3142265507269));
#66541=CARTESIAN_POINT('Ctrl Pts',(-3.22115050171122,0.00280629626111247,
32.3107734492731));
#66542=CARTESIAN_POINT('Ctrl Pts',(-3.21469754736738,-0.763061078972069,
32.3580052353748));
#66543=CARTESIAN_POINT('Ctrl Pts',(-2.55869281488842,-2.60888204696492,
32.4712260412281));
#66544=CARTESIAN_POINT('Ctrl Pts',(0.518024667143807,-3.77052441367253,
32.650435866833));
#66545=CARTESIAN_POINT('Ctrl Pts',(3.44477432083465,-1.61825022428116,32.8484029260877));
#66546=CARTESIAN_POINT('Ctrl Pts',(3.23282874888886,2.00848753798692,33.0463699853423));
#66547=CARTESIAN_POINT('Ctrl Pts',(0.0753014887309373,3.80519823342296,
33.2443370445969));
#66548=CARTESIAN_POINT('Ctrl Pts',(-2.71899596473592,2.35840681143994,33.4158048659072));
#66549=CARTESIAN_POINT('Ctrl Pts',(-3.21541088886627,0.640116338696104,
33.5212836674659));
#66550=CARTESIAN_POINT('Ctrl Pts',(-3.21834786352283,-0.00162040783760153,
33.5607734492731));
#66551=CARTESIAN_POINT('Origin',(0.,0.,-2.31077344927314));
#66552=CARTESIAN_POINT('',(-3.22747527198257,-0.00128106685233335,30.8142265507269));
#66553=CARTESIAN_POINT('',(-3.22784895015315,-0.000584129469891059,31.0607734492731));
#66554=CARTESIAN_POINT('',(-3.22275,7.67147279210326E-13,-2.31077344927314));
#66555=CARTESIAN_POINT('Ctrl Pts',(-3.22747527198257,-0.00128106685233375,
30.8142265507269));
#66556=CARTESIAN_POINT('Ctrl Pts',(-3.22783152828137,-0.0719553879082988,
30.8186072838179));
#66557=CARTESIAN_POINT('Ctrl Pts',(-3.19363801753637,-1.21182193198418,
30.8892834335756));
#66558=CARTESIAN_POINT('Ctrl Pts',(-1.84430286171068,-3.33601963516042,
31.0262550000001));
#66559=CARTESIAN_POINT('Ctrl Pts',(1.80971425616015,-3.35490899473305,31.22514125));
#66560=CARTESIAN_POINT('Ctrl Pts',(3.8007675342582,-0.290940204197991,31.4240275000001));
#66561=CARTESIAN_POINT('Ctrl Pts',(2.29925896103701,3.04037633887334,31.62291375));
#66562=CARTESIAN_POINT('Ctrl Pts',(-1.31506079077929,3.57786181516915,31.8218000000001));
#66563=CARTESIAN_POINT('Ctrl Pts',(-3.09455949069686,1.54366917503357,31.968904266909));
#66564=CARTESIAN_POINT('Ctrl Pts',(-3.22539683099921,0.237903243377298,
32.0497131171513));
#66565=CARTESIAN_POINT('Ctrl Pts',(-3.22321200919049,0.00295167801057841,
32.0642265507269));
#66566=CARTESIAN_POINT('Ctrl Pts',(-3.22784895015315,-0.000584129469891211,
31.0607734492731));
#66567=CARTESIAN_POINT('Ctrl Pts',(-3.22792887150411,-0.0324419667226371,
31.0627487637807));
#66568=CARTESIAN_POINT('Ctrl Pts',(-3.21309758646861,-1.12849329993279,
31.1307130980398));
#66569=CARTESIAN_POINT('Ctrl Pts',(-1.9760576970998,-3.25275266314625,31.2646664520505));
#66570=CARTESIAN_POINT('Ctrl Pts',(1.65261824030163,-3.42841900322799,31.4626335113052));
#66571=CARTESIAN_POINT('Ctrl Pts',(3.77551629574763,-0.480292213570351,
31.6606005705598));
#66572=CARTESIAN_POINT('Ctrl Pts',(2.45836462134124,2.90545130718283,31.8585676298145));
#66573=CARTESIAN_POINT('Ctrl Pts',(-1.0987182013029,3.64390206015446,32.0565346890691));
#66574=CARTESIAN_POINT('Ctrl Pts',(-3.04488911002489,1.67817047252684,32.207269962222));
#66575=CARTESIAN_POINT('Ctrl Pts',(-3.22371317363936,0.306956413960427,
32.2920162156233));
#66576=CARTESIAN_POINT('Ctrl Pts',(-3.22115050171122,0.00280629626111247,
32.3107734492731));
#66577=CARTESIAN_POINT('Origin',(0.,0.,-2.31077344927314));
#66578=CARTESIAN_POINT('',(-3.21928386531128,-0.0023275571713062,29.5642265507269));
#66579=CARTESIAN_POINT('',(-3.21951987652482,-0.0023462889869294,29.8107734492731));
#66580=CARTESIAN_POINT('',(-3.22275,7.67147279210326E-13,-2.31077344927314));
#66581=CARTESIAN_POINT('Ctrl Pts',(-3.21928386531128,-0.00232755717130651,
29.5642265507269));
#66582=CARTESIAN_POINT('Ctrl Pts',(-3.22179663352806,-0.380281685711084,
29.5875014504846));
#66583=CARTESIAN_POINT('Ctrl Pts',(-2.98525657845807,-1.8317424676862,29.677071766909));
#66584=CARTESIAN_POINT('Ctrl Pts',(-0.832267516579828,-3.71992081000873,
29.8329375));
#66585=CARTESIAN_POINT('Ctrl Pts',(2.67974690370432,-2.71098443078842,30.03182375));
#66586=CARTESIAN_POINT('Ctrl Pts',(3.72931611451176,0.789101622057042,30.2307100000001));
#66587=CARTESIAN_POINT('Ctrl Pts',(1.35198087098079,3.56407460309012,30.42959625));
#66588=CARTESIAN_POINT('Ctrl Pts',(-2.18797427827443,3.07500027700796,30.624101766909));
#66589=CARTESIAN_POINT('Ctrl Pts',(-3.2224401567282,0.997587874520822,30.7523118671513));
#66590=CARTESIAN_POINT('Ctrl Pts',(-3.22747527198257,-0.00128106685233375,
30.8142265507269));
#66591=CARTESIAN_POINT('Ctrl Pts',(-3.21951987652482,-0.00234628898692951,
29.8107734492731));
#66592=CARTESIAN_POINT('Ctrl Pts',(-3.22202184511065,-0.371027753442167,
29.8334813119381));
#66593=CARTESIAN_POINT('Ctrl Pts',(-2.9935553562486,-1.80809092066496,29.9221781943546));
#66594=CARTESIAN_POINT('Ctrl Pts',(-0.879815326883564,-3.70285415597931,
30.0768640965227));
#66595=CARTESIAN_POINT('Ctrl Pts',(2.62699068395643,-2.75392880377806,30.2748311557773));
#66596=CARTESIAN_POINT('Ctrl Pts',(3.74022244301854,0.70423006653559,30.4727982150319));
#66597=CARTESIAN_POINT('Ctrl Pts',(1.44556235449795,3.52073193940277,30.6707652742866));
#66598=CARTESIAN_POINT('Ctrl Pts',(-2.13017897797683,3.1332354492707,30.8667570190336));
#66599=CARTESIAN_POINT('Ctrl Pts',(-3.22525895155626,1.03182777038991,30.9967597440292));
#66600=CARTESIAN_POINT('Ctrl Pts',(-3.22784895015315,-0.000584129469891211,
31.0607734492731));
#66601=CARTESIAN_POINT('Origin',(0.,0.,-2.31077344927314));
#66602=CARTESIAN_POINT('',(-3.21898880855509,0.00217568322875482,28.3142265507269));
#66603=CARTESIAN_POINT('',(-3.2195784941175,0.00237125681338005,28.5607734492731));
#66604=CARTESIAN_POINT('',(-3.22275,7.67147279210326E-13,-2.31077344927314));
#66605=CARTESIAN_POINT('Ctrl Pts',(-3.21898880855509,0.00217568322875492,
28.3142265507269));
#66606=CARTESIAN_POINT('Ctrl Pts',(-3.21475771426579,-0.682752752100061,
28.3563956171513));
#66607=CARTESIAN_POINT('Ctrl Pts',(-2.66484322282807,-2.45068470257344,
28.4648601002423));
#66608=CARTESIAN_POINT('Ctrl Pts',(0.246873732837376,-3.80388399033473,
28.63962));
#66609=CARTESIAN_POINT('Ctrl Pts',(3.33371099678845,-1.8484726240282,28.8385062500001));
#66610=CARTESIAN_POINT('Ctrl Pts',(3.35716915487184,1.80551801914775,29.0373925));
#66611=CARTESIAN_POINT('Ctrl Pts',(0.295692279952789,3.80040078511023,29.23627875));
#66612=CARTESIAN_POINT('Ctrl Pts',(-2.64742839616081,2.47828694492588,29.4118901002423));
#66613=CARTESIAN_POINT('Ctrl Pts',(-3.21463935175017,0.696269736346894,
29.5212060338179));
#66614=CARTESIAN_POINT('Ctrl Pts',(-3.21928386531128,-0.00232755717130651,
29.5642265507269));
#66615=CARTESIAN_POINT('Ctrl Pts',(-3.2195784941175,0.00237125681337987,
28.5607734492731));
#66616=CARTESIAN_POINT('Ctrl Pts',(-3.2147354374273,-0.702888423299994,
28.6042138600955));
#66617=CARTESIAN_POINT('Ctrl Pts',(-2.64000685660925,-2.48666699441575,
28.7136432906694));
#66618=CARTESIAN_POINT('Ctrl Pts',(0.301725028063924,-3.79396440643719,
28.8890617409948));
#66619=CARTESIAN_POINT('Ctrl Pts',(3.34667671285774,-1.8124455549031,29.0870288002495));
#66620=CARTESIAN_POINT('Ctrl Pts',(3.34231449720922,1.8204773307068,29.2849958595041));
#66621=CARTESIAN_POINT('Ctrl Pts',(0.292613000107598,3.79467805512411,29.4829629187588));
#66622=CARTESIAN_POINT('Ctrl Pts',(-2.64330314849576,2.48151312137492,29.6582221153484));
#66623=CARTESIAN_POINT('Ctrl Pts',(-3.21475112761232,0.700360108942837,
29.7674922921865));
#66624=CARTESIAN_POINT('Ctrl Pts',(-3.21951987652482,-0.00234628898692951,
29.8107734492731));
#66625=CARTESIAN_POINT('Origin',(0.,0.,-2.31077344927314));
#66626=CARTESIAN_POINT('',(-3.22723414919969,0.00150563849211922,27.0642265507269));
#66627=CARTESIAN_POINT('',(-3.22786891212035,0.000537718463040557,27.3107734492731));
#66628=CARTESIAN_POINT('',(-3.22275,7.67147279210326E-13,-2.31077344927314));
#66629=CARTESIAN_POINT('Ctrl Pts',(-3.22723414919969,0.00150563849211919,
27.0642265507269));
#66630=CARTESIAN_POINT('Ctrl Pts',(-3.22154002065253,-0.983821934168731,
27.1252897838179));
#66631=CARTESIAN_POINT('Ctrl Pts',(-2.21180709545868,-3.04899464970893,
27.2526484335756));
#66632=CARTESIAN_POINT('Ctrl Pts',(1.30610950143672,-3.58113920731194,27.4463025));
#66633=CARTESIAN_POINT('Ctrl Pts',(3.71887727353106,-0.836918082194489,
27.6451887500001));
#66634=CARTESIAN_POINT('Ctrl Pts',(2.71433294268781,2.67635511995881,27.8440750000001));
#66635=CARTESIAN_POINT('Ctrl Pts',(-0.784438041578219,3.73029985534876,
28.04296125));
#66636=CARTESIAN_POINT('Ctrl Pts',(-2.973385007322,1.85975711368115,28.1996784335757));
#66637=CARTESIAN_POINT('Ctrl Pts',(-3.22140956081232,0.394046424575874,
28.2901002004846));
#66638=CARTESIAN_POINT('Ctrl Pts',(-3.21898880855509,0.00217568322875492,
28.3142265507269));
#66639=CARTESIAN_POINT('Ctrl Pts',(-3.22786891212035,0.000537718463040756,
27.3107734492731));
#66640=CARTESIAN_POINT('Ctrl Pts',(-3.22546512944508,-1.03442543785973,
27.3749464082529));
#66641=CARTESIAN_POINT('Ctrl Pts',(-2.12555463795461,-3.1380341292707,27.5051083869842));
#66642=CARTESIAN_POINT('Ctrl Pts',(1.45401317967913,-3.51725028725448,27.701259385467));
#66643=CARTESIAN_POINT('Ctrl Pts',(3.74190285747308,-0.695245938576497,
27.8992264447217));
#66644=CARTESIAN_POINT('Ctrl Pts',(2.6203695833697,2.76022954777739,28.0971935039762));
#66645=CARTESIAN_POINT('Ctrl Pts',(-0.888705147656408,3.70073061305487,
28.295160563231));
#66646=CARTESIAN_POINT('Ctrl Pts',(-2.99571736444363,1.80285265676093,28.4496872116632));
#66647=CARTESIAN_POINT('Ctrl Pts',(-3.22209237898327,0.368450315904827,
28.5382248403439));
#66648=CARTESIAN_POINT('Ctrl Pts',(-3.2195784941175,0.00237125681337987,
28.5607734492731));
#66649=CARTESIAN_POINT('Origin',(0.,0.,-2.31077344927314));
#66650=CARTESIAN_POINT('',(-3.22363407567384,-0.00290863082020876,25.8142265507269));
#66651=CARTESIAN_POINT('',(-3.22107869366301,-0.00279461251546875,26.0607734492731));
#66652=CARTESIAN_POINT('',(-3.22275,7.67147279210326E-13,-2.31077344927314));
#66653=CARTESIAN_POINT('Ctrl Pts',(-3.22363407567384,-0.0029086308202092,
25.8142265507269));
#66654=CARTESIAN_POINT('Ctrl Pts',(-3.22568756323173,-0.22400215866507,
25.827888533818));
#66655=CARTESIAN_POINT('Ctrl Pts',(-3.10397607047467,-1.51571554300823,
25.9078459335757));
#66656=CARTESIAN_POINT('Ctrl Pts',(-1.36088934335066,-3.56068255353444,
26.05409875));
#66657=CARTESIAN_POINT('Ctrl Pts',(2.26003338720418,-3.06964641947774,26.252985));
#66658=CARTESIAN_POINT('Ctrl Pts',(3.80418969631625,0.242117340005657,26.4518712500001));
#66659=CARTESIAN_POINT('Ctrl Pts',(1.852639496472,3.33139714654406,26.6507575));
#66660=CARTESIAN_POINT('Ctrl Pts',(-1.80131895941629,3.35942406646398,26.8496437500001));
#66661=CARTESIAN_POINT('Ctrl Pts',(-3.18637259141522,1.23963008315624,26.987466766909));
#66662=CARTESIAN_POINT('Ctrl Pts',(-3.22772204878106,0.0859331160642886,
27.0589943671513));
#66663=CARTESIAN_POINT('Ctrl Pts',(-3.22723414919969,0.00150563849211919,
27.0642265507269));
#66664=CARTESIAN_POINT('Ctrl Pts',(-3.22107869366301,-0.00279461251546882,
26.0607734492731));
#66665=CARTESIAN_POINT('Ctrl Pts',(-3.22364795624573,-0.309544392334381,
26.0796899366587));
#66666=CARTESIAN_POINT('Ctrl Pts',(-3.04291136040896,-1.68340601974217,
26.1645954437958));
#66667=CARTESIAN_POINT('Ctrl Pts',(-1.08996424799818,-3.64653011066113,
26.3154899706845));
#66668=CARTESIAN_POINT('Ctrl Pts',(2.46533493731419,-2.89953919730883,26.5134570299392));
#66669=CARTESIAN_POINT('Ctrl Pts',(3.77435199303925,0.489357683614875,26.7114240891938));
#66670=CARTESIAN_POINT('Ctrl Pts',(1.64438016964158,3.43237785908865,26.9093911484484));
#66671=CARTESIAN_POINT('Ctrl Pts',(-1.98386344368891,3.24799780582855,27.1073582077031));
#66672=CARTESIAN_POINT('Ctrl Pts',(-3.21433376763909,1.12330283478777,27.2411523079779));
#66673=CARTESIAN_POINT('Ctrl Pts',(-3.22793693789772,0.0298266279716151,
27.3089573885013));
#66674=CARTESIAN_POINT('Ctrl Pts',(-3.22786891212035,0.000537718463040756,
27.3107734492731));
#66675=CARTESIAN_POINT('Origin',(0.,0.,-2.31077344927314));
#66676=CARTESIAN_POINT('',(-3.21742354549419,-0.000159280653085815,24.5642265507269));
#66677=CARTESIAN_POINT('',(-3.21838772674461,0.00165536655674689,24.8107734492731));
#66678=CARTESIAN_POINT('',(-3.22275,7.67147279210326E-13,-2.31077344927314));
#66679=CARTESIAN_POINT('Ctrl Pts',(-3.21742354549419,-0.000159280653085694,
24.5642265507269));
#66680=CARTESIAN_POINT('Ctrl Pts',(-3.21765598864656,-0.529594024909045,
24.5967827004846));
#66681=CARTESIAN_POINT('Ctrl Pts',(-2.84316955446559,-2.13682872494597,
24.695634266909));
#66682=CARTESIAN_POINT('Ctrl Pts',(-0.305195037191488,-3.79964946293255,
24.86078125));
#66683=CARTESIAN_POINT('Ctrl Pts',(3.03173030730948,-2.3106473975125,25.0596675000001));
#66684=CARTESIAN_POINT('Ctrl Pts',(3.58276950661523,1.30163079033885,25.25855375));
#66685=CARTESIAN_POINT('Ctrl Pts',(0.841567339384293,3.7178279230179,25.4574400000001));
#66686=CARTESIAN_POINT('Ctrl Pts',(-2.43153772899687,2.78638001033204,25.642664266909));
#66687=CARTESIAN_POINT('Ctrl Pts',(-3.21572291810203,0.848864602558081,
25.7615931171513));
#66688=CARTESIAN_POINT('Ctrl Pts',(-3.22363407567384,-0.0029086308202092,
25.8142265507269));
#66689=CARTESIAN_POINT('Ctrl Pts',(-3.21838772674461,0.00165536655674668,
24.8107734492731));
#66690=CARTESIAN_POINT('Ctrl Pts',(-3.21537305131233,-0.642649371821592,
24.8504224848161));
#66691=CARTESIAN_POINT('Ctrl Pts',(-2.71592291202178,-2.36359214900197,
24.9560605401106));
#66692=CARTESIAN_POINT('Ctrl Pts',(0.0844394074013012,-3.80500642527053,
25.1276876151567));
#66693=CARTESIAN_POINT('Ctrl Pts',(3.23764278439912,-2.00071814869078,25.3256546744113));
#66694=CARTESIAN_POINT('Ctrl Pts',(3.44087817996476,1.6265181402354,25.523621733666));
#66695=CARTESIAN_POINT('Ctrl Pts',(0.50896830631917,3.77175757081959,25.7215887929206));
#66696=CARTESIAN_POINT('Ctrl Pts',(-2.56221901458568,2.60376870483498,25.9006393647896));
#66697=CARTESIAN_POINT('Ctrl Pts',(-3.21468523944414,0.760533623030957,
26.0137009169071));
#66698=CARTESIAN_POINT('Ctrl Pts',(-3.22107869366301,-0.00279461251546882,
26.0607734492731));
#66699=CARTESIAN_POINT('Origin',(0.,0.,-2.31077344927314));
#66700=CARTESIAN_POINT('',(-3.22304749582146,0.00296322048342273,23.3142265507269));
#66701=CARTESIAN_POINT('',(-3.22701991158836,0.00156882509208339,23.5607734492731));
#66702=CARTESIAN_POINT('',(-3.22275,7.67147279210326E-13,-2.31077344927314));
#66703=CARTESIAN_POINT('Ctrl Pts',(-3.22304749582146,0.00296322048342276,
23.3142265507269));
#66704=CARTESIAN_POINT('Ctrl Pts',(-3.21531008847461,-0.830052111865801,
23.3656768671513));
#66705=CARTESIAN_POINT('Ctrl Pts',(-2.460062449872,-2.74887948098658,23.4834226002424));
#66706=CARTESIAN_POINT('Ctrl Pts',(0.775107208778419,-3.73224983981374,
23.66746375));
#66707=CARTESIAN_POINT('Ctrl Pts',(3.55897817735421,-1.36534039162637,23.8663500000001));
#66708=CARTESIAN_POINT('Ctrl Pts',(3.07246986072833,2.25619347725455,24.06523625));
#66709=CARTESIAN_POINT('Ctrl Pts',(-0.237360568651399,3.80448945488611,
24.2641225));
#66710=CARTESIAN_POINT('Ctrl Pts',(-2.82298770437097,2.17562469080033,24.4304526002423));
#66711=CARTESIAN_POINT('Ctrl Pts',(-3.21718265516725,0.548515555906512,
24.5304872838179));
#66712=CARTESIAN_POINT('Ctrl Pts',(-3.21742354549419,-0.000159280653085694,
24.5642265507269));
#66713=CARTESIAN_POINT('Ctrl Pts',(-3.22701991158836,0.00156882509208334,
23.5607734492731));
#66714=CARTESIAN_POINT('Ctrl Pts',(-3.2211640532689,-0.972930212896847,
23.6211550329735));
#66715=CARTESIAN_POINT('Ctrl Pts',(-2.2327364184039,-3.02272099417933,23.7475256364254));
#66716=CARTESIAN_POINT('Ctrl Pts',(1.25065667292649,-3.59458784790924,23.9398852596288));
#66717=CARTESIAN_POINT('Ctrl Pts',(3.6960615727801,-0.90792772845131,24.1378523188835));
#66718=CARTESIAN_POINT('Ctrl Pts',(2.77381166227548,2.60598786875474,24.3358193781381));
#66719=CARTESIAN_POINT('Ctrl Pts',(-0.675787969966405,3.74546586281613,
24.5337864373928));
#66720=CARTESIAN_POINT('Ctrl Pts',(-2.94207777719568,1.92755146848088,24.6921044611044));
#66721=CARTESIAN_POINT('Ctrl Pts',(-3.22039046154491,0.429685365319261,
24.7844334650645));
#66722=CARTESIAN_POINT('Ctrl Pts',(-3.21838772674461,0.00165536655674668,
24.8107734492731));
#66723=CARTESIAN_POINT('Origin',(0.,0.,-2.31077344927314));
#66724=CARTESIAN_POINT('',(-3.22755990945695,-0.0011906676974904,22.0642265507269));
#66725=CARTESIAN_POINT('',(-3.22287078059728,-0.00290075263836898,22.3107734492731));
#66726=CARTESIAN_POINT('',(-3.22275,7.67147279210326E-13,-2.31077344927314));
#66727=CARTESIAN_POINT('Ctrl Pts',(-3.22755990945695,-0.0011906676974902,
22.0642265507269));
#66728=CARTESIAN_POINT('Ctrl Pts',(-3.22786903641777,-0.0665096632917848,
22.0682756171513));
#66729=CARTESIAN_POINT('Ctrl Pts',(-3.19641732350679,-1.20099399831007,
22.1386201002423));
#66730=CARTESIAN_POINT('Ctrl Pts',(-1.86096454568552,-3.32675382491574,
22.27526));
#66731=CARTESIAN_POINT('Ctrl Pts',(1.79291239805955,-3.36391812991553,22.47414625));
#66732=CARTESIAN_POINT('Ctrl Pts',(3.79926489107751,-0.309945703818892,
22.6730325));
#66733=CARTESIAN_POINT('Ctrl Pts',(2.31443632605062,3.02883881125214,22.87191875));
#66734=CARTESIAN_POINT('Ctrl Pts',(-1.29715004429138,3.58439420467181,23.070805));
#66735=CARTESIAN_POINT('Ctrl Pts',(-3.09083529909138,1.5545607399339,23.2182409335757));
#66736=CARTESIAN_POINT('Ctrl Pts',(-3.22527999108412,0.243315408215143,
23.2993814504846));
#66737=CARTESIAN_POINT('Ctrl Pts',(-3.22304749582146,0.00296322048342276,
23.3142265507269));
#66738=CARTESIAN_POINT('Ctrl Pts',(-3.22287078059728,-0.00290075263836877,
22.3107734492731));
#66739=CARTESIAN_POINT('Ctrl Pts',(-3.22510637863034,-0.247822164486929,
22.3258985613793));
#66740=CARTESIAN_POINT('Ctrl Pts',(-3.08796074838616,-1.55882789172308,
22.4070126932371));
#66741=CARTESIAN_POINT('Ctrl Pts',(-1.29655136755524,-3.57828987942048,
22.5541158448463));
#66742=CARTESIAN_POINT('Ctrl Pts',(2.29562293209663,-3.03567443305511,22.752082904101));
#66743=CARTESIAN_POINT('Ctrl Pts',(3.79614765886846,0.272886170297954,22.9500499633556));
#66744=CARTESIAN_POINT('Ctrl Pts',(1.83782445454307,3.3328074027996,23.1480170226103));
#66745=CARTESIAN_POINT('Ctrl Pts',(-1.79502668798453,3.35605171284586,23.3459840818649));
#66746=CARTESIAN_POINT('Ctrl Pts',(-3.18314642283721,1.24702165210228,23.4835695574192));
#66747=CARTESIAN_POINT('Ctrl Pts',(-3.22756372559652,0.0920672966887587,
23.5551660132219));
#66748=CARTESIAN_POINT('Ctrl Pts',(-3.22701991158836,0.00156882509208334,
23.5607734492731));
#66749=CARTESIAN_POINT('Origin',(0.,0.,-2.31077344927314));
#66750=CARTESIAN_POINT('',(-3.2194044849354,-0.00238303041332784,20.8142265507269));
#66751=CARTESIAN_POINT('',(-3.21768849251173,0.000747963174234367,21.0607734492731));
#66752=CARTESIAN_POINT('',(-3.22275,7.67147279210326E-13,-2.31077344927314));
#66753=CARTESIAN_POINT('Ctrl Pts',(-3.2194044849354,-0.00238303041332839,
20.8142265507269));
#66754=CARTESIAN_POINT('Ctrl Pts',(-3.22194656271802,-0.374916247463388,
20.8371697838179));
#66755=CARTESIAN_POINT('Ctrl Pts',(-2.98981931580154,-1.82082982892955,
20.9264084335756));
#66756=CARTESIAN_POINT('Ctrl Pts',(-0.850861899417176,-3.7157117864563,
21.0819425));
#66757=CARTESIAN_POINT('Ctrl Pts',(2.6661546849312,-2.724352996201,21.28082875));
#66758=CARTESIAN_POINT('Ctrl Pts',(3.73321608039316,0.770439971045078,21.479715));
#66759=CARTESIAN_POINT('Ctrl Pts',(1.36978930534994,3.55726823712227,21.67860125));
#66760=CARTESIAN_POINT('Ctrl Pts',(-2.17860797484293,3.08510098167624,21.8734384335757));
#66761=CARTESIAN_POINT('Ctrl Pts',(-3.22280769671063,1.00295909204903,22.0019802004846));
#66762=CARTESIAN_POINT('Ctrl Pts',(-3.22755990945695,-0.0011906676974902,
22.0642265507269));
#66763=CARTESIAN_POINT('Ctrl Pts',(-3.21768849251173,0.000747963174234575,
21.0607734492731));
#66764=CARTESIAN_POINT('Ctrl Pts',(-3.21647214829413,-0.582263006821988,
21.0966311095367));
#66765=CARTESIAN_POINT('Ctrl Pts',(-2.7866028252762,-2.23986331067818,21.1984777895519));
#66766=CARTESIAN_POINT('Ctrl Pts',(-0.133122145626393,-3.80361438689783,
21.3663134893184));
#66767=CARTESIAN_POINT('Ctrl Pts',(3.11802883817059,-2.18245276563067,21.5642805485732));
#66768=CARTESIAN_POINT('Ctrl Pts',(3.52819770926901,1.42724378933009,21.7622476078277));
#66769=CARTESIAN_POINT('Ctrl Pts',(0.723660398246818,3.73651168041552,21.9602146670825));
#66770=CARTESIAN_POINT('Ctrl Pts',(-2.47558847099782,2.72494770381142,22.1430566142308));
#66771=CARTESIAN_POINT('Ctrl Pts',(-3.21535273702263,0.820740089503346,
22.2599095416278));
#66772=CARTESIAN_POINT('Ctrl Pts',(-3.22287078059728,-0.00290075263836877,
22.3107734492731));
#66773=CARTESIAN_POINT('Origin',(0.,0.,-2.31077344927314));
#66774=CARTESIAN_POINT('',(-3.21887978231881,0.00211299402852188,19.5642265507269));
#66775=CARTESIAN_POINT('',(-3.22557758161264,0.00235737622836907,19.8107734492731));
#66776=CARTESIAN_POINT('',(-3.22275,7.67147279210326E-13,-2.31077344927314));
#66777=CARTESIAN_POINT('Ctrl Pts',(-3.21887978231881,0.00211299402852177,
19.5642265507269));
#66778=CARTESIAN_POINT('Ctrl Pts',(-3.21481144448344,-0.677486100948278,
19.6060639504846));
#66779=CARTESIAN_POINT('Ctrl Pts',(-2.67155366980303,-2.43992188292104,
19.714196766909));
#66780=CARTESIAN_POINT('Ctrl Pts',(0.227845920122608,-3.80507112792566,
19.8886250000001));
#66781=CARTESIAN_POINT('Ctrl Pts',(3.32442436079109,-1.86512270943999,20.08751125));
#66782=CARTESIAN_POINT('Ctrl Pts',(3.366157274749,1.78870490957689,20.2863975000001));
#66783=CARTESIAN_POINT('Ctrl Pts',(0.314695885881992,3.7988743795102,20.48528375));
#66784=CARTESIAN_POINT('Ctrl Pts',(-2.64057130871506,2.48902761712003,20.661226766909));
#66785=CARTESIAN_POINT('Ctrl Pts',(-3.21460112429926,0.701533821648526,
20.7708743671513));
#66786=CARTESIAN_POINT('Ctrl Pts',(-3.2194044849354,-0.00238303041332839,
20.8142265507269));
#66787=CARTESIAN_POINT('Ctrl Pts',(-3.22557758161264,0.00235737622836879,
19.8107734492731));
#66788=CARTESIAN_POINT('Ctrl Pts',(-3.21805665506623,-0.912024844401449,
19.8673636576941));
#66789=CARTESIAN_POINT('Ctrl Pts',(-2.33391015726838,-2.90537649651881,
19.9899428858666));
#66790=CARTESIAN_POINT('Ctrl Pts',(1.04321325149407,-3.66017896034874,20.1785111337906));
#66791=CARTESIAN_POINT('Ctrl Pts',(3.63814224250802,-1.11764257844405,20.3764781930453));
#66792=CARTESIAN_POINT('Ctrl Pts',(2.91818943772608,2.44323030339269,20.5744452522999));
#66793=CARTESIAN_POINT('Ctrl Pts',(-0.460662442187536,3.77796162291654,
20.7724123115546));
#66794=CARTESIAN_POINT('Ctrl Pts',(-2.88379934488129,2.0521538463159,20.9345217105456));
#66795=CARTESIAN_POINT('Ctrl Pts',(-3.21871059224195,0.490654805763857,
21.0306420897851));
#66796=CARTESIAN_POINT('Ctrl Pts',(-3.21768849251173,0.000747963174234575,
21.0607734492731));
#66797=CARTESIAN_POINT('Origin',(0.,0.,-2.31077344927314));
#66798=CARTESIAN_POINT('',(-3.22713146099961,0.00158994899472997,18.3142265507269));
#66799=CARTESIAN_POINT('',(-3.22470148543098,-0.00263455512554606,18.5607734492731));
#66800=CARTESIAN_POINT('',(-3.22275,7.67147279210326E-13,-2.31077344927314));
#66801=CARTESIAN_POINT('Ctrl Pts',(-3.22713146099961,0.00158994899473025,
18.3142265507269));
#66802=CARTESIAN_POINT('Ctrl Pts',(-3.22120609028706,-0.978468238727024,
18.3749581171513));
#66803=CARTESIAN_POINT('Ctrl Pts',(-2.22100824016265,-3.03883590904923,
18.5019851002423));
#66804=CARTESIAN_POINT('Ctrl Pts',(1.28818247537154,-3.58762678689348,18.6953075));
#66805=CARTESIAN_POINT('Ctrl Pts',(3.71464500371619,-0.855507187729257,
18.89419375));
#66806=CARTESIAN_POINT('Ctrl Pts',(2.72768450257131,2.6627461963774,19.09308));
#66807=CARTESIAN_POINT('Ctrl Pts',(-0.76577152881775,3.73417648452,19.29196625));
#66808=CARTESIAN_POINT('Ctrl Pts',(-2.96869873438807,1.87066944191426,19.4490151002423));
#66809=CARTESIAN_POINT('Ctrl Pts',(-3.22125812026871,0.399404562159262,
19.5397685338179));
#66810=CARTESIAN_POINT('Ctrl Pts',(-3.21887978231881,0.00211299402852177,
19.5642265507269));
#66811=CARTESIAN_POINT('Ctrl Pts',(-3.22470148543098,-0.00263455512554578,
18.5607734492731));
#66812=CARTESIAN_POINT('Ctrl Pts',(-3.22632095927964,-0.185893923124646,
18.5721071860999));
#66813=CARTESIAN_POINT('Ctrl Pts',(-3.12886753636446,-1.43443236269005,
18.6494299426783));
#66814=CARTESIAN_POINT('Ctrl Pts',(-1.49890159705929,-3.49835645871106,
18.7927417190082));
#66815=CARTESIAN_POINT('Ctrl Pts',(2.1184092557461,-3.16188964624663,18.9907087782628));
#66816=CARTESIAN_POINT('Ctrl Pts',(3.80553821630163,0.0555229154508125,
19.1886758375175));
#66817=CARTESIAN_POINT('Ctrl Pts',(2.02526306905968,3.2223459483698,19.3866428967721));
#66818=CARTESIAN_POINT('Ctrl Pts',(-1.60032411708034,3.45313866361654,19.5846099560268));
#66819=CARTESIAN_POINT('Ctrl Pts',(-3.14819898127591,1.37103695231587,19.7259868068604));
#66820=CARTESIAN_POINT('Ctrl Pts',(-3.22682669822862,0.154222976577529,
19.8013746379425));
#66821=CARTESIAN_POINT('Ctrl Pts',(-3.22557758161264,0.00235737622836879,
19.8107734492731));
#66822=CARTESIAN_POINT('Origin',(0.,0.,-2.31077344927314));
#66823=CARTESIAN_POINT('',(-3.22379796809719,-0.00288664070778104,17.0642265507269));
#66824=CARTESIAN_POINT('',(-3.2175431274752,-0.000244872741176072,17.3107734492731));
#66825=CARTESIAN_POINT('',(-3.22275,7.67147279210326E-13,-2.31077344927314));
#66826=CARTESIAN_POINT('Ctrl Pts',(-3.22379796809719,-0.00288664070778058,
17.0642265507269));
#66827=CARTESIAN_POINT('Ctrl Pts',(-3.22579710476995,-0.218584582317807,
17.0775568671513));
#66828=CARTESIAN_POINT('Ctrl Pts',(-3.10758827702004,-1.50482958829351,
17.1571826002423));
#66829=CARTESIAN_POINT('Ctrl Pts',(-1.37868070132254,-3.55383167520506,
17.30310375));
#66830=CARTESIAN_POINT('Ctrl Pts',(2.24465260765735,-3.08091134614859,17.50199));
#66831=CARTESIAN_POINT('Ctrl Pts',(3.80535304148599,0.223088057823076,17.70087625));
#66832=CARTESIAN_POINT('Ctrl Pts',(1.8692779572903,3.32208969931257,17.8997625000001));
#66833=CARTESIAN_POINT('Ctrl Pts',(-1.78449462466053,3.36839115698396,18.09864875));
#66834=CARTESIAN_POINT('Ctrl Pts',(-3.18349141863527,1.25046640358126,18.2368034335757));
#66835=CARTESIAN_POINT('Ctrl Pts',(-3.2276743067916,0.09137681447932,18.3086627004846));
#66836=CARTESIAN_POINT('Ctrl Pts',(-3.22713146099961,0.00158994899473025,
18.3142265507269));
#66837=CARTESIAN_POINT('Ctrl Pts',(-3.2175431274752,-0.000244872741175725,
17.3107734492731));
#66838=CARTESIAN_POINT('Ctrl Pts',(-3.21789832634533,-0.521670563510979,
17.3428397342573));
#66839=CARTESIAN_POINT('Ctrl Pts',(-2.85221365971589,-2.11566531376391,
17.440895038993));
#66840=CARTESIAN_POINT('Ctrl Pts',(-0.350248680105062,-3.78979284024299,
17.6049393634804));
#66841=CARTESIAN_POINT('Ctrl Pts',(2.98822575042405,-2.3570555306091,17.8029064227349));
#66842=CARTESIAN_POINT('Ctrl Pts',(3.60398774105126,1.2233054697109,18.0008734819896));
#66843=CARTESIAN_POINT('Ctrl Pts',(0.935987701844621,3.68905556096245,18.1988405412443));
#66844=CARTESIAN_POINT('Ctrl Pts',(-2.38326531404954,2.84480349181404,18.3854738636721));
#66845=CARTESIAN_POINT('Ctrl Pts',(-3.21689181041029,0.881106858642543,
18.5061181663484));
#66846=CARTESIAN_POINT('Ctrl Pts',(-3.22470148543098,-0.00263455512554578,
18.5607734492731));
#66847=CARTESIAN_POINT('Origin',(0.,0.,-2.31077344927314));
#66848=CARTESIAN_POINT('',(-3.2174336584483,-0.000248419282747805,15.8142265507269));
#66849=CARTESIAN_POINT('',(-3.22381398336647,0.00281172170752172,16.0607734492731));
#66850=CARTESIAN_POINT('',(-3.22275,7.67147279210326E-13,-2.31077344927314));
#66851=CARTESIAN_POINT('Ctrl Pts',(-3.2174336584483,-0.000248419282747846,
15.8142265507269));
#66852=CARTESIAN_POINT('Ctrl Pts',(-3.21779255326727,-0.524285427231881,
15.8464510338179));
#66853=CARTESIAN_POINT('Ctrl Pts',(-2.84874083961618,-2.1259470999027,15.9449709335756));
#66854=CARTESIAN_POINT('Ctrl Pts',(-0.324194766610495,-3.79807553969012,
16.10978625));
#66855=CARTESIAN_POINT('Ctrl Pts',(3.02013592975928,-2.32578137787433,16.3086725));
#66856=CARTESIAN_POINT('Ctrl Pts',(3.58923466600481,1.2836956665189,16.5075587500001));
#66857=CARTESIAN_POINT('Ctrl Pts',(0.86015113855453,3.71357241355724,16.706445));
#66858=CARTESIAN_POINT('Ctrl Pts',(-2.4234406942069,2.79686770301245,16.8920009335757));
#66859=CARTESIAN_POINT('Ctrl Pts',(-3.21585483524874,0.854142010055347,
17.0112614504846));
#66860=CARTESIAN_POINT('Ctrl Pts',(-3.22379796809719,-0.00288664070778058,
17.0642265507269));
#66861=CARTESIAN_POINT('Ctrl Pts',(-3.22381398336647,0.00281172170752176,
16.0607734492731));
#66862=CARTESIAN_POINT('Ctrl Pts',(-3.21602073876447,-0.851519211745776,
16.1135722824147));
#66863=CARTESIAN_POINT('Ctrl Pts',(-2.42919148351035,-2.7862976707188,16.2323601353078));
#66864=CARTESIAN_POINT('Ctrl Pts',(0.832360802113325,-3.71380928494957,
16.4171370079525));
#66865=CARTESIAN_POINT('Ctrl Pts',(3.56833413631518,-1.32370517921483,16.6151040672071));
#66866=CARTESIAN_POINT('Ctrl Pts',(3.05303110985611,2.27248871331039,16.8130711264618));
#66867=CARTESIAN_POINT('Ctrl Pts',(-0.244031554753848,3.79811170322264,
17.0110381857164));
#66868=CARTESIAN_POINT('Ctrl Pts',(-2.82070996455941,2.17652677557168,17.1769389599869));
#66869=CARTESIAN_POINT('Ctrl Pts',(-3.21716736467427,0.551368306571193,
17.2768507145058));
#66870=CARTESIAN_POINT('Ctrl Pts',(-3.2175431274752,-0.000244872741175725,
17.3107734492731));
#66871=CARTESIAN_POINT('Origin',(0.,0.,-2.31077344927314));
#66872=CARTESIAN_POINT('',(-3.22288314929224,0.0029718364718792,14.5642265507269));
#66873=CARTESIAN_POINT('',(-3.2263403267092,-0.00200868097619572,14.8107734492731));
#66874=CARTESIAN_POINT('',(-3.22275,7.67147279210326E-13,-2.31077344927314));
#66875=CARTESIAN_POINT('Ctrl Pts',(-3.22288314929224,0.00297183647187928,
14.5642265507269));
#66876=CARTESIAN_POINT('Ctrl Pts',(-3.21521016001633,-0.824781581368616,
14.6153452004846));
#66877=CARTESIAN_POINT('Ctrl Pts',(-2.4679586424349,-2.73834265879665,14.732759266909));
#66878=CARTESIAN_POINT('Ctrl Pts',(0.756431060077252,-3.73607977741916,
14.91646875));
#66879=CARTESIAN_POINT('Ctrl Pts',(3.55210505889249,-1.38312316967087,15.115355));
#66880=CARTESIAN_POINT('Ctrl Pts',(3.08371554718117,2.24079862458972,15.31424125));
#66881=CARTESIAN_POINT('Ctrl Pts',(-0.21832984675111,3.80562900581595,15.5131275));
#66882=CARTESIAN_POINT('Ctrl Pts',(-2.81724322909883,2.18649418273475,15.679789266909));
#66883=CARTESIAN_POINT('Ctrl Pts',(-3.21705419909425,0.553815707628409,
15.7801556171513));
#66884=CARTESIAN_POINT('Ctrl Pts',(-3.2174336584483,-0.000248419282747846,
15.8142265507269));
#66885=CARTESIAN_POINT('Ctrl Pts',(-3.2263403267092,-0.00200868097619563,
14.8107734492731));
#66886=CARTESIAN_POINT('Ctrl Pts',(-3.22723124442984,-0.123802489841831,
14.8183158108205));
#66887=CARTESIAN_POINT('Ctrl Pts',(-3.16578983988483,-1.31027741920305,
14.8918471921195));
#66888=CARTESIAN_POINT('Ctrl Pts',(-1.696353693388,-3.4069910561669,15.03136759317));
#66889=CARTESIAN_POINT('Ctrl Pts',(1.93427300977863,-3.27777238891207,15.2293346524246));
#66890=CARTESIAN_POINT('Ctrl Pts',(3.80249297873402,-0.162021778014253,
15.4273017116793));
#66891=CARTESIAN_POINT('Ctrl Pts',(2.2060834984687,3.10135446340087,15.6252687709339));
#66892=CARTESIAN_POINT('Ctrl Pts',(-1.40039198296493,3.53894139594313,15.8232358301886));
#66893=CARTESIAN_POINT('Ctrl Pts',(-3.10934499764541,1.49531585790812,15.9684040563016));
#66894=CARTESIAN_POINT('Ctrl Pts',(-3.225760889093,0.216240386100458,16.0475832626631));
#66895=CARTESIAN_POINT('Ctrl Pts',(-3.22381398336647,0.00281172170752176,
16.0607734492731));
#66896=CARTESIAN_POINT('Origin',(0.,0.,-2.31077344927314));
#66897=CARTESIAN_POINT('',(-3.22763904405734,-0.00109877613235525,13.3142265507269));
#66898=CARTESIAN_POINT('',(-3.21796438773957,-0.00120981133772902,13.5607734492731));
#66899=CARTESIAN_POINT('',(-3.22275,7.67147279210326E-13,-2.31077344927314));
#66900=CARTESIAN_POINT('Ctrl Pts',(-3.22763904405734,-0.00109877613235536,
13.3142265507269));
#66901=CARTESIAN_POINT('Ctrl Pts',(-3.22790364316531,-0.0610634584561656,
13.3179439504846));
#66902=CARTESIAN_POINT('Ctrl Pts',(-3.19916828701905,-1.19016844739519,
13.387956766909));
#66903=CARTESIAN_POINT('Ctrl Pts',(-1.87757967929805,-3.31740479890186,
13.524265));
#66904=CARTESIAN_POINT('Ctrl Pts',(1.77606569186011,-3.37284311969702,13.72315125));
#66905=CARTESIAN_POINT('Ctrl Pts',(3.79766721268626,-0.32894345042547,13.9220375));
#66906=CARTESIAN_POINT('Ctrl Pts',(2.32955579751124,3.01722551993911,14.12092375));
#66907=CARTESIAN_POINT('Ctrl Pts',(-1.2792068507562,3.59083693376187,14.31981));
#66908=CARTESIAN_POINT('Ctrl Pts',(-3.08707946816032,1.56545378025357,14.4675776002423));
#66909=CARTESIAN_POINT('Ctrl Pts',(-3.22516120574105,0.248725993520245,
14.5490497838179));
#66910=CARTESIAN_POINT('Ctrl Pts',(-3.22288314929224,0.00297183647187928,
14.5642265507269));
#66911=CARTESIAN_POINT('Ctrl Pts',(-3.21796438773957,-0.00120981133772905,
13.5607734492731));
#66912=CARTESIAN_POINT('Ctrl Pts',(-3.21952342447733,-0.460834059410147,
13.5890483589779));
#66913=CARTESIAN_POINT('Ctrl Pts',(-2.91292585124894,-1.99116214018758,
13.6833122884343));
#66914=CARTESIAN_POINT('Ctrl Pts',(-0.566230666680783,-3.76358695156398,
13.8435652376421));
#66915=CARTESIAN_POINT('Ctrl Pts',(2.84865769364129,-2.52395587408549,14.0415322968968));
#66916=CARTESIAN_POINT('Ctrl Pts',(3.66800060750612,1.01536961408498,14.2394993561514));
#66917=CARTESIAN_POINT('Ctrl Pts',(1.14525637075743,3.62954429028107,14.4374664154061));
#66918=CARTESIAN_POINT('Ctrl Pts',(-2.28511410901714,2.96306899170226,14.6278911131133));
#66919=CARTESIAN_POINT('Ctrl Pts',(-3.21943649915082,0.941786054053766,
14.752326791069));
#66920=CARTESIAN_POINT('Ctrl Pts',(-3.2263403267092,-0.00200868097619563,
14.8107734492731));
#66921=CARTESIAN_POINT('Origin',(0.,0.,-2.31077344927314));
#66922=CARTESIAN_POINT('',(-3.21952816226103,-0.00243635184806505,12.0642265507269));
#66923=CARTESIAN_POINT('',(-3.2219754753083,0.00289434104541186,12.3107734492731));
#66924=CARTESIAN_POINT('',(-3.22275,7.67147279210326E-13,-2.31077344927314));
#66925=CARTESIAN_POINT('Ctrl Pts',(-3.21952816226103,-0.00243635184806499,
12.0642265507269));
#66926=CARTESIAN_POINT('Ctrl Pts',(-3.22209591491135,-0.369548780530837,
12.0868381171513));
#66927=CARTESIAN_POINT('Ctrl Pts',(-2.99434768393422,-1.80991726839579,
12.1757451002423));
#66928=CARTESIAN_POINT('Ctrl Pts',(-0.869434998705811,-3.71140981769939,
12.3309475));
#66929=CARTESIAN_POINT('Ctrl Pts',(2.65249577468504,-2.73765341436203,12.52983375));
#66930=CARTESIAN_POINT('Ctrl Pts',(3.73702266321591,0.751759048166815,12.72872));
#66931=CARTESIAN_POINT('Ctrl Pts',(1.38756347566574,3.55037288927353,12.92760625));
#66932=CARTESIAN_POINT('Ctrl Pts',(-2.16919521531468,3.09518493566959,13.1227751002423));
#66933=CARTESIAN_POINT('Ctrl Pts',(-3.22318483183059,1.00833554596791,13.2516485338179));
#66934=CARTESIAN_POINT('Ctrl Pts',(-3.22763904405734,-0.00109877613235536,
13.3142265507269));
#66935=CARTESIAN_POINT('Ctrl Pts',(-3.2219754753083,0.00289434104541197,
12.3107734492731));
#66936=CARTESIAN_POINT('Ctrl Pts',(-3.21492550593893,-0.791248393644031,
12.3597809071353));
#66937=CARTESIAN_POINT('Ctrl Pts',(-2.51870961379289,-2.66576186073892,
12.474777384749));
#66938=CARTESIAN_POINT('Ctrl Pts',(0.61878835158859,-3.75530356773067,12.6557628821143));
#66939=CARTESIAN_POINT('Ctrl Pts',(3.48686537418057,-1.52544215629862,12.853729941369));
#66940=CARTESIAN_POINT('Ctrl Pts',(3.17789604102199,2.09432105044312,13.0516970006236));
#66941=CARTESIAN_POINT('Ctrl Pts',(-0.0266032173364325,3.80585025699904,
13.2496640598783));
#66942=CARTESIAN_POINT('Ctrl Pts',(-2.75263818088242,2.30051682698361,13.4193562094281));
#66943=CARTESIAN_POINT('Ctrl Pts',(-3.21588488744377,0.611853843079764,
13.5230593392264));
#66944=CARTESIAN_POINT('Ctrl Pts',(-3.21796438773957,-0.00120981133772905,
13.5607734492731));
#66945=CARTESIAN_POINT('Origin',(0.,0.,-2.31077344927314));
#66946=CARTESIAN_POINT('',(-3.21877418690567,0.0020484167724553,10.8142265507269));
#66947=CARTESIAN_POINT('',(-3.22752742220963,-0.00108629272672134,11.0607734492731));
#66948=CARTESIAN_POINT('',(-3.22275,7.67147279210326E-13,-2.31077344927314));
#66949=CARTESIAN_POINT('Ctrl Pts',(-3.21877418690567,0.0020484167724549,
10.8142265507269));
#66950=CARTESIAN_POINT('Ctrl Pts',(-3.21486930714951,-0.672218600580391,
10.8557322838179));
#66951=CARTESIAN_POINT('Ctrl Pts',(-2.67822325513316,-2.42915317683481,
10.9635334335756));
#66952=CARTESIAN_POINT('Ctrl Pts',(0.208812408046019,-3.80616308506823,
11.13763));
#66953=CARTESIAN_POINT('Ctrl Pts',(3.31505456729397,-1.88172614047672,11.33651625));
#66954=CARTESIAN_POINT('Ctrl Pts',(3.37506119321498,1.77184705715372,11.5354025));
#66955=CARTESIAN_POINT('Ctrl Pts',(0.333691619975345,3.79725294846791,11.73428875));
#66956=CARTESIAN_POINT('Ctrl Pts',(-2.6336728682884,2.49976175320687,11.9105634335756));
#66957=CARTESIAN_POINT('Ctrl Pts',(-3.21456745674729,0.706797323328607,
12.0205427004846));
#66958=CARTESIAN_POINT('Ctrl Pts',(-3.21952816226103,-0.00243635184806499,
12.0642265507269));
#66959=CARTESIAN_POINT('Ctrl Pts',(-3.22752742220963,-0.0010862927267216,
11.0607734492731));
#66960=CARTESIAN_POINT('Ctrl Pts',(-3.22779342624244,-0.0615982436869706,
11.0645244355411));
#66961=CARTESIAN_POINT('Ctrl Pts',(-3.1988784036326,-1.18640415769286,11.1342644415607));
#66962=CARTESIAN_POINT('Ctrl Pts',(-1.88826241961219,-3.30449223702413,
11.2699934673318));
#66963=CARTESIAN_POINT('Ctrl Pts',(1.74381591738736,-3.38294397768258,11.4679605265865));
#66964=CARTESIAN_POINT('Ctrl Pts',(3.78702189743871,-0.379037014277084,
11.6659275858411));
#66965=CARTESIAN_POINT('Ctrl Pts',(2.37969485505221,2.97022832568649,11.8638946450958));
#66966=CARTESIAN_POINT('Ctrl Pts',(-1.1958836268722,3.61317952236688,12.0618617043504));
#66967=CARTESIAN_POINT('Ctrl Pts',(-3.0664299399447,1.61980912775541,12.2108213057429));
#66968=CARTESIAN_POINT('Ctrl Pts',(-3.2244183584201,0.278072540168287,12.2937918873838));
#66969=CARTESIAN_POINT('Ctrl Pts',(-3.2219754753083,0.00289434104541197,
12.3107734492731));
#66970=CARTESIAN_POINT('Origin',(0.,0.,-2.31077344927314));
#66971=CARTESIAN_POINT('',(-3.22702415133123,0.00167235368052675,9.56422655072689));
#66972=CARTESIAN_POINT('',(-3.21891511857495,-0.00203587595620058,9.8107734492731));
#66973=CARTESIAN_POINT('',(-3.22275,7.67147279210326E-13,-2.31077344927314));
#66974=CARTESIAN_POINT('Ctrl Pts',(-3.22702415133123,0.00167235368052666,
9.56422655072689));
#66975=CARTESIAN_POINT('Ctrl Pts',(-3.22088140544128,-0.973119137173498,
9.6246264504846));
#66976=CARTESIAN_POINT('Ctrl Pts',(-2.23016324609443,-3.02866137559854,
9.75132176690898));
#66977=CARTESIAN_POINT('Ctrl Pts',(1.27022322657475,-3.59402462520223,9.94431250000001));
#66978=CARTESIAN_POINT('Ctrl Pts',(3.71031981538147,-0.874074893517518,
10.14319875));
#66979=CARTESIAN_POINT('Ctrl Pts',(2.74096783186856,2.64907066658324,10.342085));
#66980=CARTESIAN_POINT('Ctrl Pts',(-0.747085860967871,3.73795970660893,
10.54097125));
#66981=CARTESIAN_POINT('Ctrl Pts',(-2.96397756792535,1.88158151294885,10.698351766909));
#66982=CARTESIAN_POINT('Ctrl Pts',(-3.22110641251276,0.404760638936827,
10.7894368671513));
#66983=CARTESIAN_POINT('Ctrl Pts',(-3.21877418690567,0.0020484167724549,
10.8142265507269));
#66984=CARTESIAN_POINT('Ctrl Pts',(-3.21891511857495,-0.00203587595620017,
9.8107734492731));
#66985=CARTESIAN_POINT('Ctrl Pts',(-3.22122774117535,-0.39973470628387,
9.83525698369852));
#66986=CARTESIAN_POINT('Ctrl Pts',(-2.96891139380953,-1.86649717402379,
9.92572953787549));
#66987=CARTESIAN_POINT('Ctrl Pts',(-0.780362316170466,-3.72508235685782,
10.082191111804));
#66988=CARTESIAN_POINT('Ctrl Pts',(2.6997807504167,-2.68260839660801,10.2801581710586));
#66989=CARTESIAN_POINT('Ctrl Pts',(3.72002712642615,0.80411571836772,10.4781252303133));
#66990=CARTESIAN_POINT('Ctrl Pts',(1.35078255368256,3.55817234019647,10.6760922895679));
#66991=CARTESIAN_POINT('Ctrl Pts',(-2.18101206117008,3.07945714130881,10.8703083625545));
#66992=CARTESIAN_POINT('Ctrl Pts',(-3.22311376491591,1.00295492760852,10.9985354157896));
#66993=CARTESIAN_POINT('Ctrl Pts',(-3.22752742220963,-0.0010862927267216,
11.0607734492731));
#66994=CARTESIAN_POINT('Origin',(0.,0.,-2.31077344927314));
#66995=CARTESIAN_POINT('',(-3.22396133703721,-0.00286173073963965,8.31422655072689));
#66996=CARTESIAN_POINT('',(-3.22027572892457,0.00261454196279293,8.5607734492731));
#66997=CARTESIAN_POINT('',(-3.22275,7.67147279210326E-13,-2.31077344927314));
#66998=CARTESIAN_POINT('Ctrl Pts',(-3.22396133703721,-0.00286173073963985,
8.31422655072689));
#66999=CARTESIAN_POINT('Ctrl Pts',(-3.22590450377897,-0.213165553777342,
8.32722520048459));
#67000=CARTESIAN_POINT('Ctrl Pts',(-3.11116933513409,-1.49394529920932,
8.40651926690897));
#67001=CARTESIAN_POINT('Ctrl Pts',(-1.39643757283078,-3.54689190095731,
8.55210875000002));
#67002=CARTESIAN_POINT('Ctrl Pts',(2.22921568013466,-3.09209920657986,8.75099500000001));
#67003=CARTESIAN_POINT('Ctrl Pts',(3.80642119915558,0.204053195292361,8.94988125000001));
#67004=CARTESIAN_POINT('Ctrl Pts',(1.88586965979368,3.3126991529808,9.14876750000002));
#67005=CARTESIAN_POINT('Ctrl Pts',(-1.76762565236893,3.37727399021419,9.34765375000001));
#67006=CARTESIAN_POINT('Ctrl Pts',(-3.18058147267209,1.26130503966291,9.4861401002423));
#67007=CARTESIAN_POINT('Ctrl Pts',(-3.22762373282734,0.0968198578997676,
9.55833103381793));
#67008=CARTESIAN_POINT('Ctrl Pts',(-3.22702415133123,0.00167235368052666,
9.56422655072689));
#67009=CARTESIAN_POINT('Ctrl Pts',(-3.22027572892457,0.00261454196279275,
8.5607734492731));
#67010=CARTESIAN_POINT('Ctrl Pts',(-3.21463452458948,-0.73107245854707,
8.60598953185591));
#67011=CARTESIAN_POINT('Ctrl Pts',(-2.60260549049518,-2.54402617904789,
8.71719463419026));
#67012=CARTESIAN_POINT('Ctrl Pts',(0.403193815184867,-3.78452621305085,
8.89438875627614));
#67013=CARTESIAN_POINT('Ctrl Pts',(3.39400218094999,-1.72219427056852,9.0923558155308));
#67014=CARTESIAN_POINT('Ctrl Pts',(3.29237619572427,1.90930953375835,9.29032287478543));
#67015=CARTESIAN_POINT('Ctrl Pts',(0.190912054474585,3.80115199608339,9.48828993404008));
#67016=CARTESIAN_POINT('Ctrl Pts',(-2.67941498037181,2.42394983134342,9.6617734588693));
#67017=CARTESIAN_POINT('Ctrl Pts',(-3.21499466649732,0.672159388484275,
9.76926796394697));
#67018=CARTESIAN_POINT('Ctrl Pts',(-3.21891511857495,-0.00203587595620017,
9.8107734492731));
#67019=CARTESIAN_POINT('Origin',(0.,0.,-2.31077344927314));
#67020=CARTESIAN_POINT('',(-3.21744819095025,-0.00033734180616485,7.06422655072688));
#67021=CARTESIAN_POINT('',(-3.22798100933232,1.20436113847002E-5,7.3107734492731));
#67022=CARTESIAN_POINT('',(-3.22275,7.67147279210326E-13,-2.31077344927314));
#67023=CARTESIAN_POINT('Ctrl Pts',(-3.21744819095025,-0.00033734180616498,
7.06422655072688));
#67024=CARTESIAN_POINT('Ctrl Pts',(-3.21793065745993,-0.518974922087274,
7.09611936715126));
#67025=CARTESIAN_POINT('Ctrl Pts',(-2.85427452458422,-2.11506311315496,
7.1943076002423));
#67026=CARTESIAN_POINT('Ctrl Pts',(-0.343186386587714,-3.79640661098804,
7.35879125000001));
#67027=CARTESIAN_POINT('Ctrl Pts',(3.00846600621214,-2.34085718089664,7.55767750000001));
#67028=CARTESIAN_POINT('Ctrl Pts',(3.5956100439019,1.26572843220077,7.75656375000002));
#67029=CARTESIAN_POINT('Ctrl Pts',(0.878713421813992,3.70922401240668,7.95545000000001));
#67030=CARTESIAN_POINT('Ctrl Pts',(-2.41529942916466,2.8073441425483,8.14133760024231));
#67031=CARTESIAN_POINT('Ctrl Pts',(-3.21599400913541,0.859421202136209,
8.26092978381793));
#67032=CARTESIAN_POINT('Ctrl Pts',(-3.22396133703721,-0.00286173073963985,
8.31422655072689));
#67033=CARTESIAN_POINT('Ctrl Pts',(-3.22798098720893,1.20435604489447E-5,
7.31077344927309));
#67034=CARTESIAN_POINT('Ctrl Pts',(-3.22792175517501,-1.0634891969682,7.37672208001329));
#67035=CARTESIAN_POINT('Ctrl Pts',(-2.07326176640397,-3.19125327047275,
7.50865973050503));
#67036=CARTESIAN_POINT('Ctrl Pts',(1.5476603571224,-3.4770607312591,7.70658640074832));
#67037=CARTESIAN_POINT('Ctrl Pts',(3.75917552904779,-0.594813627685692,
7.90455346000295));
#67038=CARTESIAN_POINT('Ctrl Pts',(2.54552980900885,2.82939603119107,8.1025205192576));
#67039=CARTESIAN_POINT('Ctrl Pts',(-0.987467344283091,3.67561044642204,
8.30048757851224));
#67040=CARTESIAN_POINT('Ctrl Pts',(-3.01929261435194,1.74445015182628,8.45323855518407));
#67041=CARTESIAN_POINT('Ctrl Pts',(-3.22286738164004,0.339681202596263,
8.54000051210436));
#67042=CARTESIAN_POINT('Ctrl Pts',(-3.22027572892457,0.00261454196279275,
8.5607734492731));
#67043=CARTESIAN_POINT('Origin',(0.,0.,-2.31077344927314));
#67044=CARTESIAN_POINT('',(-3.22271911507513,0.00297753179786089,5.81422655072688));
#67045=CARTESIAN_POINT('',(-3.22030921936247,-0.00262401028225973,6.0607734492731));
#67046=CARTESIAN_POINT('',(-3.22275,7.67147279210326E-13,-2.31077344927314));
#67047=CARTESIAN_POINT('Ctrl Pts',(-3.22271911507513,0.00297753179786076,
5.81422655072688));
#67048=CARTESIAN_POINT('Ctrl Pts',(-3.21511698107986,-0.819512286718065,
5.86501353381793));
#67049=CARTESIAN_POINT('Ctrl Pts',(-2.47581111925387,-2.72779556832849,
5.98209593357564));
#67050=CARTESIAN_POINT('Ctrl Pts',(0.737735989926837,-3.73981626035058,
6.16547375000001));
#67051=CARTESIAN_POINT('Ctrl Pts',(3.5451430877039,-1.4008713501182,6.36436000000001));
#67052=CARTESIAN_POINT('Ctrl Pts',(3.09488409724894,2.22534772034816,6.56324625000001));
#67053=CARTESIAN_POINT('Ctrl Pts',(-0.19929366352457,3.8066733623451,6.76213250000001));
#67054=CARTESIAN_POINT('Ctrl Pts',(-2.81146051372698,2.19736071579676,6.92912593357563));
#67055=CARTESIAN_POINT('Ctrl Pts',(-3.21692775706187,0.559114075328717,
7.02982395048459));
#67056=CARTESIAN_POINT('Ctrl Pts',(-3.21744819095025,-0.00033734180616498,
7.06422655072688));
#67057=CARTESIAN_POINT('Ctrl Pts',(-3.22030921936247,-0.00262401028225941,
6.0607734492731));
#67058=CARTESIAN_POINT('Ctrl Pts',(-3.22290205123769,-0.338371123515593,
6.08146560841913));
#67059=CARTESIAN_POINT('Ctrl Pts',(-3.02034206694596,-1.74179359390663,
6.16814678731671));
#67060=CARTESIAN_POINT('Ctrl Pts',(-0.991943885951175,-3.67440488202038,
6.32081698596584));
#67061=CARTESIAN_POINT('Ctrl Pts',(2.54208142306422,-2.83249465107694,6.51878404522046));
#67062=CARTESIAN_POINT('Ctrl Pts',(3.75989728477033,0.590234121215191,6.71675110447512));
#67063=CARTESIAN_POINT('Ctrl Pts',(1.55189462906941,3.47517294104057,6.91471816372975));
#67064=CARTESIAN_POINT('Ctrl Pts',(-2.07011190883012,3.19371892858329,7.1126852229844));
#67065=CARTESIAN_POINT('Ctrl Pts',(-3.22768646466942,1.06546721490889,7.24470365149884));
#67066=CARTESIAN_POINT('Ctrl Pts',(-3.22798102348448,0.000663365099614621,
7.31073306026174));
#67067=CARTESIAN_POINT('Ctrl Pts',(-3.22798098720893,1.20435604489447E-5,
7.31077344927309));
#67068=CARTESIAN_POINT('Origin',(0.,0.,-2.31077344927314));
#67069=CARTESIAN_POINT('',(-3.22771248049277,-0.0010054936160085,4.56422655072689));
#67070=CARTESIAN_POINT('',(-3.21888985043626,0.0020204358260266,4.81077344927309));
#67071=CARTESIAN_POINT('',(-3.22275,7.67147279210326E-13,-2.31077344927314));
#67072=CARTESIAN_POINT('Ctrl Pts',(-3.22771248049277,-0.00100549361600838,
4.56422655072689));
#67073=CARTESIAN_POINT('Ctrl Pts',(-3.22793533636644,-0.0556168128984164,
4.56761228381793));
#67074=CARTESIAN_POINT('Ctrl Pts',(-3.20189100109211,-1.17934529311488,
4.63729343357563));
#67075=CARTESIAN_POINT('Ctrl Pts',(-1.89414784662335,-3.30797278933611,
4.77327));
#67076=CARTESIAN_POINT('Ctrl Pts',(1.75917455880395,-3.38168374168425,4.97215625000001));
#67077=CARTESIAN_POINT('Ctrl Pts',(3.79597453913422,-0.347932968357942,
5.17104250000001));
#67078=CARTESIAN_POINT('Ctrl Pts',(2.34461699717418,3.0055367551961,5.36992875000001));
#67079=CARTESIAN_POINT('Ctrl Pts',(-1.26123165898331,3.59718984140266,5.56881500000001));
#67080=CARTESIAN_POINT('Ctrl Pts',(-3.0832918894214,1.576348251431,5.71691426690897));
#67081=CARTESIAN_POINT('Ctrl Pts',(-3.22504052073703,0.254134972951963,
5.79871811715126));
#67082=CARTESIAN_POINT('Ctrl Pts',(-3.22271911507513,0.00297753179786076,
5.81422655072688));
#67083=CARTESIAN_POINT('Ctrl Pts',(-3.21888985043626,0.00202043582602666,
4.81077344927309));
#67084=CARTESIAN_POINT('Ctrl Pts',(-3.21500861080956,-0.670875972885779,
4.85219815657651));
#67085=CARTESIAN_POINT('Ctrl Pts',(-2.68102990457166,-2.42132711321019,
4.95961188363147));
#67086=CARTESIAN_POINT('Ctrl Pts',(0.186281715928623,-3.80138172682447,
5.133014630438));
#67087=CARTESIAN_POINT('Ctrl Pts',(3.290048016384,-1.91331857244767,5.33098168969263));
#67088=CARTESIAN_POINT('Ctrl Pts',(3.39609747398096,1.71805874664089,5.52894874894727));
#67089=CARTESIAN_POINT('Ctrl Pts',(0.407803461009433,3.78403227353958,5.72691580820191));
#67090=CARTESIAN_POINT('Ctrl Pts',(-2.60087562294228,2.54663069375663,5.90419070831052));
#67091=CARTESIAN_POINT('Ctrl Pts',(-3.21463329433229,0.732354397698439,
6.01547658866758));
#67092=CARTESIAN_POINT('Ctrl Pts',(-3.22030921936247,-0.00262401028225941,
6.0607734492731));
#67093=CARTESIAN_POINT('Origin',(0.,0.,-2.31077344927314));
#67094=CARTESIAN_POINT('',(-3.21965480394772,-0.00248744593871922,3.31422655072688));
#67095=CARTESIAN_POINT('',(-3.22750875009338,0.00110830861146782,3.5607734492731));
#67096=CARTESIAN_POINT('',(-3.22275,7.67147279210326E-13,-2.31077344927314));
#67097=CARTESIAN_POINT('Ctrl Pts',(-3.21965480394772,-0.00248744593871947,
3.31422655072688));
#67098=CARTESIAN_POINT('Ctrl Pts',(-3.22224462500577,-0.364179297671712,
3.33650645048459));
#67099=CARTESIAN_POINT('Ctrl Pts',(-2.99884181667278,-1.7990049583156,3.42508176690897));
#67100=CARTESIAN_POINT('Ctrl Pts',(-0.887986334554333,-3.70701493094446,
3.5799525));
#67101=CARTESIAN_POINT('Ctrl Pts',(2.63877050663273,-2.75088539460193,3.77883875000001));
#67102=CARTESIAN_POINT('Ctrl Pts',(3.74073577194275,0.7330593426781,3.977725));
#67103=CARTESIAN_POINT('Ctrl Pts',(1.40530293513768,3.54338872054109,4.17661125000001));
#67104=CARTESIAN_POINT('Ctrl Pts',(-2.15973593176927,3.1052519319067,4.37211176690896));
#67105=CARTESIAN_POINT('Ctrl Pts',(-3.22357163651051,1.01371738125969,4.50131686715126));
#67106=CARTESIAN_POINT('Ctrl Pts',(-3.22771248049277,-0.00100549361600838,
4.56422655072689));
#67107=CARTESIAN_POINT('Ctrl Pts',(-3.22750875009338,0.0011083086114679,
3.5607734492731));
#67108=CARTESIAN_POINT('Ctrl Pts',(-3.22302278853548,-1.00164523556617,
3.6229307047339));
#67109=CARTESIAN_POINT('Ctrl Pts',(-2.18329284268058,-3.07699904328362,
3.75107697994624));
#67110=CARTESIAN_POINT('Ctrl Pts',(1.34644732705721,-3.55981509909713,3.94521227491016));
#67111=CARTESIAN_POINT('Ctrl Pts',(3.71904487139598,-0.808646497252913,
4.14317933416478));
#67112=CARTESIAN_POINT('Ctrl Pts',(2.70304644183217,2.67931779227495,4.34114639341943));
#67113=CARTESIAN_POINT('Ctrl Pts',(-0.775824200771678,3.72603015619545,
4.53911345267407));
#67114=CARTESIAN_POINT('Ctrl Pts',(-2.96776667705998,1.869154056941,4.69565580462529));
#67115=CARTESIAN_POINT('Ctrl Pts',(-3.22119137503552,0.401039251040587,
4.78620913682497));
#67116=CARTESIAN_POINT('Ctrl Pts',(-3.21888985043626,0.00202043582602666,
4.81077344927309));
#67117=CARTESIAN_POINT('Origin',(0.,0.,-2.31077344927314));
#67118=CARTESIAN_POINT('',(-3.21867136367194,0.00198586312807969,2.06422655072688));
#67119=CARTESIAN_POINT('',(-3.22201388411817,-0.00289643951356,2.31077344927309));
#67120=CARTESIAN_POINT('',(-3.22275,7.67147279210326E-13,-2.31077344927314));
#67121=CARTESIAN_POINT('Ctrl Pts',(-3.21867136367194,0.00198586312807971,
2.06422655072688));
#67122=CARTESIAN_POINT('Ctrl Pts',(-3.21493076087555,-0.666947841793965,
2.10540061715126));
#67123=CARTESIAN_POINT('Ctrl Pts',(-2.68485324646853,-2.41838481311705,
2.2128701002423));
#67124=CARTESIAN_POINT('Ctrl Pts',(0.189774422820439,-3.8071558930084,2.386635));
#67125=CARTESIAN_POINT('Ctrl Pts',(3.30560145857767,-1.89828456209197,2.58552125000001));
#67126=CARTESIAN_POINT('Ctrl Pts',(3.38388089250329,1.75494596051086,2.7844075));
#67127=CARTESIAN_POINT('Ctrl Pts',(0.35267889993612,3.79553596959835,2.98329375));
#67128=CARTESIAN_POINT('Ctrl Pts',(-2.62673293070242,2.5104894057472,3.1599001002423));
#67129=CARTESIAN_POINT('Ctrl Pts',(-3.2145384293764,0.712060374694048,3.27021103381792));
#67130=CARTESIAN_POINT('Ctrl Pts',(-3.21965480394772,-0.00248744593871947,
3.31422655072688));
#67131=CARTESIAN_POINT('Ctrl Pts',(-3.22201388411817,-0.00289643951355986,
2.3107734492731));
#67132=CARTESIAN_POINT('Ctrl Pts',(-3.22444943885979,-0.276757467136012,
2.32767423313974));
#67133=CARTESIAN_POINT('Ctrl Pts',(-3.0673879406931,-1.61715552525174,2.41056403675793));
#67134=CARTESIAN_POINT('Ctrl Pts',(-1.20028377732907,-3.61171960603965,
2.55944286012766));
#67135=CARTESIAN_POINT('Ctrl Pts',(2.37607494490469,-2.97312511164363,2.75740991938231));
#67136=CARTESIAN_POINT('Ctrl Pts',(3.78748084593007,0.374423891696219,2.95537697863694));
#67137=CARTESIAN_POINT('Ctrl Pts',(1.74793537283732,3.38081724446415,3.15334403789159));
#67138=CARTESIAN_POINT('Ctrl Pts',(-1.88423579077553,3.30678992389447,3.35131109714622));
#67139=CARTESIAN_POINT('Ctrl Pts',(-3.19821240522555,1.18904022922726,3.48712090094007));
#67140=CARTESIAN_POINT('Ctrl Pts',(-3.22778529298737,0.0629243459269913,
3.55694168498235));
#67141=CARTESIAN_POINT('Ctrl Pts',(-3.22750875009338,0.0011083086114679,
3.5607734492731));
#67142=CARTESIAN_POINT('Origin',(0.,0.,-2.31077344927314));
#67143=CARTESIAN_POINT('',(-3.22687103957968,0.00196979923060657,0.814226550726883));
#67144=CARTESIAN_POINT('',(-3.217941538466,0.00121291371900201,1.06077344927309));
#67145=CARTESIAN_POINT('',(-3.22275,7.67147279210326E-13,-2.31077344927314));
#67146=CARTESIAN_POINT('Ctrl Pts',(-3.22687103957968,0.00196979923060637,
0.814226550726882));
#67147=CARTESIAN_POINT('Ctrl Pts',(-3.2205120016493,-0.967490928436361,
0.874294783817922));
#67148=CARTESIAN_POINT('Ctrl Pts',(-2.23933917473902,-3.01882333308509,
1.00065843357563));
#67149=CARTESIAN_POINT('Ctrl Pts',(1.25226897486165,-3.60013934158935,1.1933175));
#67150=CARTESIAN_POINT('Ctrl Pts',(3.70588259587967,-0.892721732175661,
1.39220375));
#67151=CARTESIAN_POINT('Ctrl Pts',(2.75419264545516,2.63538166557444,1.59109));
#67152=CARTESIAN_POINT('Ctrl Pts',(-0.728386757290071,3.7416218310534,1.78997625));
#67153=CARTESIAN_POINT('Ctrl Pts',(-2.95922030312456,1.89249897579954,1.94768843357563));
#67154=CARTESIAN_POINT('Ctrl Pts',(-3.22095360103943,0.410119412946076,
2.03910520048459));
#67155=CARTESIAN_POINT('Ctrl Pts',(-3.21867136367194,0.00198586312807971,
2.06422655072688));
#67156=CARTESIAN_POINT('Ctrl Pts',(-3.217941538466,0.00121291371900208,
1.06077344927309));
#67157=CARTESIAN_POINT('Ctrl Pts',(-3.21590426000095,-0.610555186325359,
1.09840678129712));
#67158=CARTESIAN_POINT('Ctrl Pts',(-2.75415550932367,-2.29791887119263,
1.2020291330727));
#67159=CARTESIAN_POINT('Ctrl Pts',(-0.031229830088373,-3.80578923437654,
1.37164050459982));
#67160=CARTESIAN_POINT('Ctrl Pts',(3.17533772956661,-2.09820398373205,1.56960756385447));
#67161=CARTESIAN_POINT('Ctrl Pts',(3.48872347062518,1.52120070666785,1.7675746231091));
#67162=CARTESIAN_POINT('Ctrl Pts',(0.623360915472078,3.75454335133777,1.96554168236375));
#67163=CARTESIAN_POINT('Ctrl Pts',(-2.51686097994096,2.66834479637078,2.14660795775174));
#67164=CARTESIAN_POINT('Ctrl Pts',(-3.21493982846427,0.792531442985166,
2.26168521338819));
#67165=CARTESIAN_POINT('Ctrl Pts',(-3.22201388411817,-0.00289643951355986,
2.3107734492731));
#67166=CARTESIAN_POINT('Origin',(0.,0.,39.5));
#67167=CARTESIAN_POINT('',(-3.73150059045713,-0.00288452150806035,39.2732311074181));
#67168=CARTESIAN_POINT('',(-3.5,-4.28626379701574E-16,39.5));
#67169=CARTESIAN_POINT('',(-3.48038110743704,-1.8235874740856,39.067));
#67170=CARTESIAN_POINT('Origin',(0.,0.,39.067));
#67171=CARTESIAN_POINT('Ctrl Pts',(-3.17710367210747,0.540490350682819,
39.77725));
#67172=CARTESIAN_POINT('Ctrl Pts',(-3.1637561532367,0.643070260528315,39.7732046970049));
#67173=CARTESIAN_POINT('Ctrl Pts',(-3.14512387900806,0.744684739103562,
39.7691738072623));
#67174=CARTESIAN_POINT('Ctrl Pts',(-3.12151814966561,0.845073767043372,
39.765152624555));
#67175=CARTESIAN_POINT('Ctrl Pts',(-3.09733288315468,0.947927415845119,
39.7610327189993));
#67176=CARTESIAN_POINT('Ctrl Pts',(-3.06792673767774,1.04949536878747,39.7569230029586));
#67177=CARTESIAN_POINT('Ctrl Pts',(-3.0335800607437,1.1494940547227,39.7528184150135));
#67178=CARTESIAN_POINT('Ctrl Pts',(-3.01568867325577,1.20158396262813,39.7506803108369));
#67179=CARTESIAN_POINT('Ctrl Pts',(-2.99645584073005,1.25324793479459,39.748543598133));
#67180=CARTESIAN_POINT('Ctrl Pts',(-2.97591588140006,1.304444537542,39.7464075614997));
#67181=CARTESIAN_POINT('Ctrl Pts',(-2.95980998271904,1.34458908132685,39.7447326414553));
#67182=CARTESIAN_POINT('Ctrl Pts',(-2.9429003211764,1.38444624584374,39.7430581370943));
#67183=CARTESIAN_POINT('Ctrl Pts',(-2.92520201085857,1.42399545129445,39.7413837035064));
#67184=CARTESIAN_POINT('Ctrl Pts',(-2.91751988870009,1.44116216507032,39.7406568994705));
#67185=CARTESIAN_POINT('Ctrl Pts',(-2.90969226795577,1.45826383112552,39.739930405335));
#67186=CARTESIAN_POINT('Ctrl Pts',(-2.90172327003567,1.47529356600236,39.7392044208686));
#67187=CARTESIAN_POINT('Ctrl Pts',(-2.85583879382635,1.57334861290315,39.7350242946709));
#67188=CARTESIAN_POINT('Ctrl Pts',(-2.80524636043718,1.66907618183903,39.7308586839284));
#67189=CARTESIAN_POINT('Ctrl Pts',(-2.750243849884,1.76218023578936,39.7267023800362));
#67190=CARTESIAN_POINT('Ctrl Pts',(-2.69481297715921,1.85600938854582,39.7225137066514));
#67191=CARTESIAN_POINT('Ctrl Pts',(-2.63490262455043,1.94717477698571,39.7183344856458));
#67192=CARTESIAN_POINT('Ctrl Pts',(-2.57076808318315,2.03535422259479,39.7141593857696));
#67193=CARTESIAN_POINT('Ctrl Pts',(-2.52863418965378,2.09328468087148,39.7114165079084));
#67194=CARTESIAN_POINT('Ctrl Pts',(-2.48467614357889,2.1499259994421,39.7086754087175));
#67195=CARTESIAN_POINT('Ctrl Pts',(-2.43895623479167,2.20517989437012,39.7059345765588));
#67196=CARTESIAN_POINT('Ctrl Pts',(-2.42734309124643,2.21921473018352,39.7052383880025));
#67197=CARTESIAN_POINT('Ctrl Pts',(-2.41561528860901,2.2331610124895,39.7045421643251));
#67198=CARTESIAN_POINT('Ctrl Pts',(-2.4037857568947,2.24700338325728,39.7038465751243));
#67199=CARTESIAN_POINT('Ctrl Pts',(-2.32918331887211,2.33429970505841,39.6994598714493));
#67200=CARTESIAN_POINT('Ctrl Pts',(-2.25043676277322,2.41759162180438,39.695092178329));
#67201=CARTESIAN_POINT('Ctrl Pts',(-2.16787254687766,2.49653395502271,39.6907375286809));
#67202=CARTESIAN_POINT('Ctrl Pts',(-2.08896125763975,2.57198360620801,39.6865755438041));
#67203=CARTESIAN_POINT('Ctrl Pts',(-2.0065617522895,2.6434606176488,39.6824254737553));
#67204=CARTESIAN_POINT('Ctrl Pts',(-1.92091521567439,2.7106349143576,39.6782821089402));
#67205=CARTESIAN_POINT('Ctrl Pts',(-1.83647215399636,2.77686530153194,39.6741969652268));
#67206=CARTESIAN_POINT('Ctrl Pts',(-1.7488721079392,2.83891368138453,39.670118339632));
#67207=CARTESIAN_POINT('Ctrl Pts',(-1.65831288783304,2.8964261348381,39.6660412391006));
#67208=CARTESIAN_POINT('Ctrl Pts',(-1.60536482584606,2.93005245082131,39.6636574445912));
#67209=CARTESIAN_POINT('Ctrl Pts',(-1.55140458800842,2.96212741030792,39.6612741714238));
#67210=CARTESIAN_POINT('Ctrl Pts',(-1.49646745549095,2.99257286153937,39.6588904216258));
#67211=CARTESIAN_POINT('Ctrl Pts',(-1.47911222300954,3.00219090783902,39.6581373693636));
#67212=CARTESIAN_POINT('Ctrl Pts',(-1.46165947603105,3.01164628460064,39.6573842695339));
#67213=CARTESIAN_POINT('Ctrl Pts',(-1.44411027186853,3.02093639848886,39.6566310906727));
#67214=CARTESIAN_POINT('Ctrl Pts',(-1.43026822018143,3.02826403770424,39.6560370158287));
#67215=CARTESIAN_POINT('Ctrl Pts',(-1.4163660931799,3.03548881054269,39.6554428905506));
#67216=CARTESIAN_POINT('Ctrl Pts',(-1.40241741124474,3.04260302573126,39.6548492486502));
#67217=CARTESIAN_POINT('Ctrl Pts',(-1.37807141460219,3.05502016018889,39.6538131074733));
#67218=CARTESIAN_POINT('Ctrl Pts',(-1.35357391445438,3.06710568910055,39.6527780219686));
#67219=CARTESIAN_POINT('Ctrl Pts',(-1.32892886492452,3.07885484871252,39.6517439135451));
#67220=CARTESIAN_POINT('Ctrl Pts',(-1.23400338476844,3.12410915490678,39.647760832135));
#67221=CARTESIAN_POINT('Ctrl Pts',(-1.13689144605682,3.16437662481258,39.6437922463479));
#67222=CARTESIAN_POINT('Ctrl Pts',(-1.03799851206363,3.19978018187908,39.6398336653046));
#67223=CARTESIAN_POINT('Ctrl Pts',(-0.936477173525234,3.23612470476135,
39.6357698719678));
#67224=CARTESIAN_POINT('Ctrl Pts',(-0.833078244337451,3.26734351361957,
39.6317166222599));
#67225=CARTESIAN_POINT('Ctrl Pts',(-0.728211962825303,3.29352264453908,
39.6276690576209));
#67226=CARTESIAN_POINT('Ctrl Pts',(-0.617268825661175,3.32121881980685,
39.6233869422216));
#67227=CARTESIAN_POINT('Ctrl Pts',(-0.504682531853149,3.34327483273434,
39.6191111898655));
#67228=CARTESIAN_POINT('Ctrl Pts',(-0.390918860121393,3.35973481018611,
39.6148360474606));
#67229=CARTESIAN_POINT('Ctrl Pts',(-0.341147253738749,3.36693605032126,
39.6129656726584));
#67230=CARTESIAN_POINT('Ctrl Pts',(-0.291150118517647,3.37306540876564,
39.6110954146048));
#67231=CARTESIAN_POINT('Ctrl Pts',(-0.240966022436918,3.37812300320975,
39.6092247915343));
#67232=CARTESIAN_POINT('Ctrl Pts',(-0.221881410394732,3.38004636609502,
39.6085134084794));
#67233=CARTESIAN_POINT('Ctrl Pts',(-0.202769759382229,3.38181470580387,
39.607801972635));
#67234=CARTESIAN_POINT('Ctrl Pts',(-0.183633192552594,3.38342794592711,
39.6070904575048));
#67235=CARTESIAN_POINT('Ctrl Pts',(-0.167412090454507,3.38479540817783,
39.6064873420309));
#67236=CARTESIAN_POINT('Ctrl Pts',(-0.1511812000706,3.38605072283508,39.6058844713497));
#67237=CARTESIAN_POINT('Ctrl Pts',(-0.134946694431332,3.3871938790219,39.60528200838));
#67238=CARTESIAN_POINT('Ctrl Pts',(-0.023532027885713,3.39503916659603,
39.6011474069104));
#67239=CARTESIAN_POINT('Ctrl Pts',(0.0881235026197957,3.39761219426123,
39.5970293228263));
#67240=CARTESIAN_POINT('Ctrl Pts',(0.199587753616714,3.39501220725874,39.5929227595484));
#67241=CARTESIAN_POINT('Ctrl Pts',(0.312322033150521,3.39238259589096,39.5887694059094));
#67242=CARTESIAN_POINT('Ctrl Pts',(0.424861556474873,3.38446148342019,39.5846278371095));
#67243=CARTESIAN_POINT('Ctrl Pts',(0.5367716407479,3.37129955295751,39.5804928838223));
#67244=CARTESIAN_POINT('Ctrl Pts',(0.648325420202415,3.35817952809499,39.5763710956022));
#67245=CARTESIAN_POINT('Ctrl Pts',(0.759254700367378,3.33985196600234,39.5722558808363));
#67246=CARTESIAN_POINT('Ctrl Pts',(0.869127285875629,3.31631566032459,39.5681421194162));
#67247=CARTESIAN_POINT('Ctrl Pts',(0.917101131057039,3.30603896500971,39.5663459210964));
#67248=CARTESIAN_POINT('Ctrl Pts',(0.96487341532449,3.29476857839289,39.5645499998529));
#67249=CARTESIAN_POINT('Ctrl Pts',(1.01240736146384,3.28250133365881,39.5627539294746));
#67250=CARTESIAN_POINT('Ctrl Pts',(1.05037596096517,3.27270264997857,39.561319285764));
#67251=CARTESIAN_POINT('Ctrl Pts',(1.0881924854212,3.2622679046368,39.5598845469008));
#67252=CARTESIAN_POINT('Ctrl Pts',(1.12583783052174,3.25119462790972,39.5584494956716));
#67253=CARTESIAN_POINT('Ctrl Pts',(1.14120725447008,3.24667375330859,39.5578636088729));
#67254=CARTESIAN_POINT('Ctrl Pts',(1.15654804398256,3.24204639639838,39.557277672997));
#67255=CARTESIAN_POINT('Ctrl Pts',(1.1718450966984,3.23731682728628,39.5566922030335));
#67256=CARTESIAN_POINT('Ctrl Pts',(1.28064083705401,3.20367917285225,39.5525282219505));
#67257=CARTESIAN_POINT('Ctrl Pts',(1.38740105523547,3.16482439786729,39.5483810786623));
#67258=CARTESIAN_POINT('Ctrl Pts',(1.49169195653895,3.12080692440921,39.544245675923));
#67259=CARTESIAN_POINT('Ctrl Pts',(1.59451171588211,3.07741036755443,39.5401686077499));
#67260=CARTESIAN_POINT('Ctrl Pts',(1.69493222231264,3.02899558619786,39.5361029512343));
#67261=CARTESIAN_POINT('Ctrl Pts',(1.79252890400652,2.97556546513603,39.5320438218091));
#67262=CARTESIAN_POINT('Ctrl Pts',(1.83909299894021,2.95007356124892,39.530107181294));
#67263=CARTESIAN_POINT('Ctrl Pts',(1.88501408928233,2.92343929481397,39.5281720265499));
#67264=CARTESIAN_POINT('Ctrl Pts',(1.93024444536004,2.89565908134739,39.5262378270902));
#67265=CARTESIAN_POINT('Ctrl Pts',(2.02491559571945,2.83751262851842,39.5221893759224));
#67266=CARTESIAN_POINT('Ctrl Pts',(2.11656269895661,2.7743484543806,39.518145109875));
#67267=CARTESIAN_POINT('Ctrl Pts',(2.2050194472515,2.70653335041133,39.5141001644575));
#67268=CARTESIAN_POINT('Ctrl Pts',(2.23439457737638,2.68401299394413,39.5127569000907));
#67269=CARTESIAN_POINT('Ctrl Pts',(2.26341761501468,2.66097938867885,39.5114135608029));
#67270=CARTESIAN_POINT('Ctrl Pts',(2.29208165138664,2.63744501091331,39.5100699684447));
#67271=CARTESIAN_POINT('Ctrl Pts',(2.30984392701489,2.62286143659788,39.5092373830583));
#67272=CARTESIAN_POINT('Ctrl Pts',(2.32747273375478,2.60808165907506,39.5084044881281));
#67273=CARTESIAN_POINT('Ctrl Pts',(2.34494114478636,2.59313055702297,39.5075724507146));
#67274=CARTESIAN_POINT('Ctrl Pts',(2.42860008947105,2.52152739762347,39.5035876937827));
#67275=CARTESIAN_POINT('Ctrl Pts',(2.50867656926775,2.44592450086923,39.4996182495046));
#67276=CARTESIAN_POINT('Ctrl Pts',(2.58505343015526,2.36673301098922,39.4956596520215));
#67277=CARTESIAN_POINT('Ctrl Pts',(2.66404287809359,2.28483265537954,39.491565644672));
#67278=CARTESIAN_POINT('Ctrl Pts',(2.73907586413126,2.19909353515585,39.4874832388718));
#67279=CARTESIAN_POINT('Ctrl Pts',(2.80999341936694,2.10992299212625,39.4834074946224));
#67280=CARTESIAN_POINT('Ctrl Pts',(2.88141591562966,2.02011754472876,39.4793027306123));
#67281=CARTESIAN_POINT('Ctrl Pts',(2.94866468551847,1.9268309090439,39.4752047233529));
#67282=CARTESIAN_POINT('Ctrl Pts',(3.01153978421965,1.83044129240823,39.4711084265728));
#67283=CARTESIAN_POINT('Ctrl Pts',(3.05695665617376,1.76081571778681,39.4681495288503));
#67284=CARTESIAN_POINT('Ctrl Pts',(3.10009073166378,1.68957028004866,39.4651915236005));
#67285=CARTESIAN_POINT('Ctrl Pts',(3.14085224826706,1.61683864750778,39.4622325089297));
#67286=CARTESIAN_POINT('Ctrl Pts',(3.15014066515061,1.60026512964199,39.4615582317163));
#67287=CARTESIAN_POINT('Ctrl Pts',(3.15930583138579,1.58361441596945,39.460883902088));
#67288=CARTESIAN_POINT('Ctrl Pts',(3.16834658750349,1.56688804883568,39.4602094975408));
#67289=CARTESIAN_POINT('Ctrl Pts',(3.17596640872947,1.55279056344176,39.4596410891005));
#67290=CARTESIAN_POINT('Ctrl Pts',(3.18349742175009,1.53864001413125,39.4590726559032));
#67291=CARTESIAN_POINT('Ctrl Pts',(3.19093291715979,1.52444919435569,39.4585046558345));
#67292=CARTESIAN_POINT('Ctrl Pts',(3.24480482802561,1.42163337161112,39.454389361911));
#67293=CARTESIAN_POINT('Ctrl Pts',(3.29375336700856,1.31654588028642,39.4502903090187));
#67294=CARTESIAN_POINT('Ctrl Pts',(3.337618406022,1.20959613349929,39.4462025795514));
#67295=CARTESIAN_POINT('Ctrl Pts',(3.38158731501003,1.10239313565547,39.4421051705678));
#67296=CARTESIAN_POINT('Ctrl Pts',(3.42044909886932,0.993318270514273,39.4380191386991));
#67297=CARTESIAN_POINT('Ctrl Pts',(3.45400073695398,0.882753434042322,39.4339395313225));
#67298=CARTESIAN_POINT('Ctrl Pts',(3.48712274811758,0.773604374354528,39.4299121630989));
#67299=CARTESIAN_POINT('Ctrl Pts',(3.51507009480238,0.663002461925495,39.4258910558902));
#67300=CARTESIAN_POINT('Ctrl Pts',(3.53760075803832,0.551297307640023,39.421871444902));
#67301=CARTESIAN_POINT('Ctrl Pts',(3.55737395285894,0.453263452399072,39.4183437834949));
#67302=CARTESIAN_POINT('Ctrl Pts',(3.57297471641564,0.354379297415562,39.4148172744827));
#67303=CARTESIAN_POINT('Ctrl Pts',(3.58420575248062,0.254876789158337,39.4112886971468));
#67304=CARTESIAN_POINT('Ctrl Pts',(3.58611064610739,0.238000189997689,39.4106902158989));
#67305=CARTESIAN_POINT('Ctrl Pts',(3.58788977339785,0.221104894290164,39.41009164332));
#67306=CARTESIAN_POINT('Ctrl Pts',(3.58954066532436,0.204208596389713,39.4094935490786));
#67307=CARTESIAN_POINT('Ctrl Pts',(3.597623244341,0.121486244504585,39.4065653477299));
#67308=CARTESIAN_POINT('Ctrl Pts',(3.60264407172324,0.0386479560669887,
39.4036453351744));
#67309=CARTESIAN_POINT('Ctrl Pts',(3.60453308945048,-0.0441671508522866,
39.4007317406353));
#67310=CARTESIAN_POINT('Ctrl Pts',(3.60708676003424,-0.156120839470894,
39.3967929948202));
#67311=CARTESIAN_POINT('Ctrl Pts',(3.60391953796431,-0.268032156050148,
39.3928659779381));
#67312=CARTESIAN_POINT('Ctrl Pts',(3.59530311376501,-0.379576415454748,
39.3889463152684));
#67313=CARTESIAN_POINT('Ctrl Pts',(3.58648336471152,-0.493752824780849,
39.3849341589118));
#67314=CARTESIAN_POINT('Ctrl Pts',(3.57195407432147,-0.607545351900785,
39.3809297079427));
#67315=CARTESIAN_POINT('Ctrl Pts',(3.5519521505194,-0.720608855394466,39.3769282705794));
#67316=CARTESIAN_POINT('Ctrl Pts',(3.53166934722454,-0.835260067142061,
39.3728706425362));
#67317=CARTESIAN_POINT('Ctrl Pts',(3.5057588970992,-0.949162442548182,39.368816113331));
#67318=CARTESIAN_POINT('Ctrl Pts',(3.47441538262496,-1.06194768262354,39.3647597907387));
#67319=CARTESIAN_POINT('Ctrl Pts',(3.46820705446736,-1.0842874806158,39.3639563396201));
#67320=CARTESIAN_POINT('Ctrl Pts',(3.46178541358641,-1.10658340128134,39.3631528181411));
#67321=CARTESIAN_POINT('Ctrl Pts',(3.45515174516057,-1.12883250042167,39.362349188284));
#67322=CARTESIAN_POINT('Ctrl Pts',(3.44954948246457,-1.1476222996899,39.361670507156));
#67323=CARTESIAN_POINT('Ctrl Pts',(3.44379534080171,-1.16638049820138,39.3609916829215));
#67324=CARTESIAN_POINT('Ctrl Pts',(3.43789702831884,-1.18508405728282,39.3603134654124));
#67325=CARTESIAN_POINT('Ctrl Pts',(3.40264701388611,-1.29686191399661,39.3562602422147));
#67326=CARTESIAN_POINT('Ctrl Pts',(3.36220319088117,-1.40685763388892,39.352222584789));
#67327=CARTESIAN_POINT('Ctrl Pts',(3.31684309881894,-1.51472132228663,39.3481957972556));
#67328=CARTESIAN_POINT('Ctrl Pts',(3.27089782911227,-1.62397652944516,39.3441170612818));
#67329=CARTESIAN_POINT('Ctrl Pts',(3.21990833949425,-1.731045158171,39.3400494774681));
#67330=CARTESIAN_POINT('Ctrl Pts',(3.16410959867439,-1.83555588581314,39.3359881658396));
#67331=CARTESIAN_POINT('Ctrl Pts',(3.10833645140519,-1.94001867687889,39.3319287170378));
#67332=CARTESIAN_POINT('Ctrl Pts',(3.04775807017554,-2.04192673482197,39.3278755346686));
#67333=CARTESIAN_POINT('Ctrl Pts',(2.98256133574493,-2.14088927082937,39.323823745469));
#67334=CARTESIAN_POINT('Ctrl Pts',(2.94977635263049,-2.19065380428797,39.3217862532287));
#67335=CARTESIAN_POINT('Ctrl Pts',(2.91582280876458,-2.23967311081566,39.31974911328));
#67336=CARTESIAN_POINT('Ctrl Pts',(2.88072037422569,-2.28789457686111,39.3177117059431));
#67337=CARTESIAN_POINT('Ctrl Pts',(2.85183603436686,-2.32757402451322,39.3160352078107));
#67338=CARTESIAN_POINT('Ctrl Pts',(2.8221737329529,-2.36671322663747,39.3143585286308));
#67339=CARTESIAN_POINT('Ctrl Pts',(2.79174315327695,-2.40528161823562,39.3126813231461));
#67340=CARTESIAN_POINT('Ctrl Pts',(2.78149815302897,-2.41826635877277,39.3121166618485));
#67341=CARTESIAN_POINT('Ctrl Pts',(2.77116939361923,-2.4311821130314,39.3115521259553));
#67342=CARTESIAN_POINT('Ctrl Pts',(2.76076240551527,-2.44402178436742,39.3109879700884));
#67343=CARTESIAN_POINT('Ctrl Pts',(2.68526519417086,-2.53716682986623,39.3068953167401));
#67344=CARTESIAN_POINT('Ctrl Pts',(2.60557688951826,-2.62640866910907,39.3028183552394));
#67345=CARTESIAN_POINT('Ctrl Pts',(2.52193212892038,-2.71137579627139,39.2987522504735));
#67346=CARTESIAN_POINT('Ctrl Pts',(2.43957779259837,-2.79503209843094,39.2947488752827));
#67347=CARTESIAN_POINT('Ctrl Pts',(2.35338763072836,-2.87454528342,39.2907560244275));
#67348=CARTESIAN_POINT('Ctrl Pts',(2.2635436371301,-2.94953435524468,39.2867690831406));
#67349=CARTESIAN_POINT('Ctrl Pts',(2.17674187142619,-3.02198420505862,39.2829171445791));
#67350=CARTESIAN_POINT('Ctrl Pts',(2.08652901371786,-3.09021163609735,39.2790707221512));
#67351=CARTESIAN_POINT('Ctrl Pts',(1.99303729858505,-3.15383958599926,39.2752256541803));
#67352=CARTESIAN_POINT('Ctrl Pts',(1.92845210860628,-3.19779453138171,39.2725694354444));
#67353=CARTESIAN_POINT('Ctrl Pts',(1.86230145895038,-3.23955372097215,39.269913863084));
#67354=CARTESIAN_POINT('Ctrl Pts',(1.79470553509306,-3.27911298465084,39.267257565119));
#67355=CARTESIAN_POINT('Ctrl Pts',(1.76785526964496,-3.29482660568139,39.2662024378066));
#67356=CARTESIAN_POINT('Ctrl Pts',(1.74077691345468,-3.31019301738663,39.2651471960072));
#67357=CARTESIAN_POINT('Ctrl Pts',(1.71347781142213,-3.32521155260794,39.2640917537339));
#67358=CARTESIAN_POINT('Ctrl Pts',(1.6984525861858,-3.33347764407684,39.2635108460593));
#67359=CARTESIAN_POINT('Ctrl Pts',(1.68335889097543,-3.34163913394484,39.2629298175273));
#67360=CARTESIAN_POINT('Ctrl Pts',(1.66821300299088,-3.34968806573045,39.2623492279294));
#67361=CARTESIAN_POINT('Ctrl Pts',(1.56635622650103,-3.40381749324935,39.2584447368246));
#67362=CARTESIAN_POINT('Ctrl Pts',(1.46200047581987,-3.4529389048349,39.2545546017007));
#67363=CARTESIAN_POINT('Ctrl Pts',(1.35557680788105,-3.49711548633947,39.250674628782));
#67364=CARTESIAN_POINT('Ctrl Pts',(1.24647006549714,-3.54240581499447,39.2466968368689));
#67365=CARTESIAN_POINT('Ctrl Pts',(1.13518916887396,-3.58249910677392,39.2427297260242));
#67366=CARTESIAN_POINT('Ctrl Pts',(1.02216633766018,-3.61741968837196,39.2387687772176));
#67367=CARTESIAN_POINT('Ctrl Pts',(0.906950805093988,-3.65301774730511,
39.2347309839565));
#67368=CARTESIAN_POINT('Ctrl Pts',(0.789924298256552,-3.68324071202624,
39.2306995941463));
#67369=CARTESIAN_POINT('Ctrl Pts',(0.67152272960871,-3.7080653836123,39.2266698206061));
#67370=CARTESIAN_POINT('Ctrl Pts',(0.576455744207969,-3.7279976084823,39.2234342349067));
#67371=CARTESIAN_POINT('Ctrl Pts',(0.480501676067777,-3.74444874562505,
39.2201996911852));
#67372=CARTESIAN_POINT('Ctrl Pts',(0.383881660549383,-3.75738289050549,
39.2169637114682));
#67373=CARTESIAN_POINT('Ctrl Pts',(0.360003491635362,-3.76057936790777,
39.2161639882445));
#67374=CARTESIAN_POINT('Ctrl Pts',(0.336084644176059,-3.76356093900021,
39.2153641773165));
#67375=CARTESIAN_POINT('Ctrl Pts',(0.312128454159217,-3.76632685583852,
39.2145642412819));
#67376=CARTESIAN_POINT('Ctrl Pts',(0.295455119908527,-3.76825191386828,
39.214007491612));
#67377=CARTESIAN_POINT('Ctrl Pts',(0.278767856439627,-3.77007198551237,
39.2134508204112));
#67378=CARTESIAN_POINT('Ctrl Pts',(0.262077281879732,-3.77178610004875,
39.2128945301218));
#67379=CARTESIAN_POINT('Ctrl Pts',(0.140725660955248,-3.78424885719911,
39.2088499282968));
#67380=CARTESIAN_POINT('Ctrl Pts',(0.0190525560554103,-3.79113177091376,
39.2048205149704));
#67381=CARTESIAN_POINT('Ctrl Pts',(-0.102493915516963,-3.79245700593582,
39.2008016264731));
#67382=CARTESIAN_POINT('Ctrl Pts',(-0.224824502847876,-3.7937907902613,
39.1967568114823));
#67383=CARTESIAN_POINT('Ctrl Pts',(-0.347027710634442,-3.78949511138404,
39.1927226575533));
#67384=CARTESIAN_POINT('Ctrl Pts',(-0.468659616482366,-3.77954173808746,
39.1886944101745));
#67385=CARTESIAN_POINT('Ctrl Pts',(-0.588412174998118,-3.76974215540543,
39.1847284036684));
#67386=CARTESIAN_POINT('Ctrl Pts',(-0.707611816239328,-3.75445834537323,
39.1807681225972));
#67387=CARTESIAN_POINT('Ctrl Pts',(-0.825834241284718,-3.73361353038175,
39.1768090294491));
#67388=CARTESIAN_POINT('Ctrl Pts',(-0.893388812412217,-3.72170240153762,
39.1745467273556));
#67389=CARTESIAN_POINT('Ctrl Pts',(-0.960624222063593,-3.70797457901974,
39.1722848131428));
#67390=CARTESIAN_POINT('Ctrl Pts',(-1.02745956875379,-3.69240826157735,
39.1700224402025));
#67391=CARTESIAN_POINT('Ctrl Pts',(-1.07281224182272,-3.68184537620588,
39.1684872546248));
#67392=CARTESIAN_POINT('Ctrl Pts',(-1.11798067116172,-3.67043582154343,
39.1669518578207));
#67393=CARTESIAN_POINT('Ctrl Pts',(-1.16293901326242,-3.65817132387934,
39.1654159852618));
#67394=CARTESIAN_POINT('Ctrl Pts',(-1.1790118050335,-3.65378671564155,39.1648669045201));
#67395=CARTESIAN_POINT('Ctrl Pts',(-1.19505272668909,-3.64929415759008,
39.1643179339248));
#67396=CARTESIAN_POINT('Ctrl Pts',(-1.21105312608346,-3.64469570725446,
39.1637693198638));
#67397=CARTESIAN_POINT('Ctrl Pts',(-1.32870450504678,-3.61088317484544,
39.1597353455105));
#67398=CARTESIAN_POINT('Ctrl Pts',(-1.44428982539489,-3.57131572587835,
39.1557163867866));
#67399=CARTESIAN_POINT('Ctrl Pts',(-1.55737353629067,-3.52596630724087,
39.151707817502));
#67400=CARTESIAN_POINT('Ctrl Pts',(-1.57607785915361,-3.51846540228185,
39.1510447903204));
#67401=CARTESIAN_POINT('Ctrl Pts',(-1.59471373536467,-3.51080619901927,
39.1503820473728));
#67402=CARTESIAN_POINT('Ctrl Pts',(-1.61327917907095,-3.50298843728883,
39.1497195677254));
#67403=CARTESIAN_POINT('Ctrl Pts',(-1.72303348532684,-3.45677176567174,
39.1458031520841));
#67404=CARTESIAN_POINT('Ctrl Pts',(-1.83032763142738,-3.40501790318193,
39.1418959384702));
#67405=CARTESIAN_POINT('Ctrl Pts',(-1.93495936234765,-3.34811198930233,
39.1379936017654));
#67406=CARTESIAN_POINT('Ctrl Pts',(-2.04145748741211,-3.290191002237,39.1340216561732));
#67407=CARTESIAN_POINT('Ctrl Pts',(-2.14519796427287,-3.22693205012696,
39.130054763028));
#67408=CARTESIAN_POINT('Ctrl Pts',(-2.24594491117972,-3.15869129439345,
39.1260883616074));
#67409=CARTESIAN_POINT('Ctrl Pts',(-2.30893415621142,-3.11602564728435,
39.1236084787062));
#67410=CARTESIAN_POINT('Ctrl Pts',(-2.37075274135737,-3.07141163206597,
39.1211287880216));
#67411=CARTESIAN_POINT('Ctrl Pts',(-2.43133703585902,-3.02492794515153,
39.118648174907));
#67412=CARTESIAN_POINT('Ctrl Pts',(-2.45143233918592,-3.00950969532322,
39.1178253763025));
#67413=CARTESIAN_POINT('Ctrl Pts',(-2.4713918044241,-2.99388569828028,39.1170024762128));
#67414=CARTESIAN_POINT('Ctrl Pts',(-2.49121297840036,-2.9780586911772,39.1161794339618));
#67415=CARTESIAN_POINT('Ctrl Pts',(-2.50475852752239,-2.96724270709744,
39.1156169769017));
#67416=CARTESIAN_POINT('Ctrl Pts',(-2.51823242965907,-2.95633753125181,
39.1150547462552));
#67417=CARTESIAN_POINT('Ctrl Pts',(-2.53163147637706,-2.94534651348948,
39.1144928398804));
#67418=CARTESIAN_POINT('Ctrl Pts',(-2.62682518042585,-2.86726068290147,
39.1105007686334));
#67419=CARTESIAN_POINT('Ctrl Pts',(-2.71828589383797,-2.78481154788143,
39.1065232597069));
#67420=CARTESIAN_POINT('Ctrl Pts',(-2.80580464251908,-2.69840960417894,
39.1025558290962));
#67421=CARTESIAN_POINT('Ctrl Pts',(-2.8941871921868,-2.61115488223934,39.0985492403563));
#67422=CARTESIAN_POINT('Ctrl Pts',(-2.97855017848199,-2.51986833452101,
39.0945529298579));
#67423=CARTESIAN_POINT('Ctrl Pts',(-3.05865080393408,-2.4249258325775,39.0905622795115));
#67424=CARTESIAN_POINT('Ctrl Pts',(-3.13867770514644,-2.33007071526719,
39.0865753021409));
#67425=CARTESIAN_POINT('Ctrl Pts',(-3.21445065607165,-2.23156568836847,
39.082593974508));
#67426=CARTESIAN_POINT('Ctrl Pts',(-3.2856914392638,-2.1297488045123,39.0786136912629));
#67427=CARTESIAN_POINT('Ctrl Pts',(-3.35497275713127,-2.03073237630024,
39.0747428850147));
#67428=CARTESIAN_POINT('Ctrl Pts',(-3.41996814007489,-1.92858304432759,
39.0708730664931));
#67429=CARTESIAN_POINT('Ctrl Pts',(-3.48038110743704,-1.8235874740856,39.067));
#67430=CARTESIAN_POINT('',(-3.,-3.67394039744206E-16,40.));
#67431=CARTESIAN_POINT('',(-3.5,-4.28626379701574E-16,39.5));
#67432=CARTESIAN_POINT('Origin',(0.,0.,40.));
#67433=CARTESIAN_POINT('Ctrl Pts',(-3.7316481904409,-0.0029745009063645,
39.273231107418));
#67434=CARTESIAN_POINT('Ctrl Pts',(-3.72101327086788,-0.0904815696235971,
39.2843416389771));
#67435=CARTESIAN_POINT('Ctrl Pts',(-3.70706464015071,-0.177438020952757,
39.2954883497431));
#67436=CARTESIAN_POINT('Ctrl Pts',(-3.68971365463305,-0.263683313725708,
39.3066800800367));
#67437=CARTESIAN_POINT('Ctrl Pts',(-3.66688152549423,-0.377173331926843,
39.3214072568354));
#67438=CARTESIAN_POINT('Ctrl Pts',(-3.63815885390845,-0.489433325135786,
39.3362123889011));
#67439=CARTESIAN_POINT('Ctrl Pts',(-3.6037996984897,-0.600127780314454,
39.3511156197284));
#67440=CARTESIAN_POINT('Ctrl Pts',(-3.56942892658912,-0.710859660165304,
39.3660238891868));
#67441=CARTESIAN_POINT('Ctrl Pts',(-3.52941713446667,-0.820025621887105,
39.3810303237503));
#67442=CARTESIAN_POINT('Ctrl Pts',(-3.48398224124741,-0.927253069125431,
39.3961550873513));
#67443=CARTESIAN_POINT('Ctrl Pts',(-3.47074172660182,-0.958501004026838,
39.4005627053687));
#67444=CARTESIAN_POINT('Ctrl Pts',(-3.45704046334811,-0.989584038315067,
39.4049803723675));
#67445=CARTESIAN_POINT('Ctrl Pts',(-3.44288339940111,-1.0204922370478,39.4094085873714));
#67446=CARTESIAN_POINT('Ctrl Pts',(-3.43640392014665,-1.03463846349922,
39.4114353160321));
#67447=CARTESIAN_POINT('Ctrl Pts',(-3.4298278760645,-1.04875033886207,39.4134645832393));
#67448=CARTESIAN_POINT('Ctrl Pts',(-3.42315930771927,-1.06281936111123,
39.4154953499366));
#67449=CARTESIAN_POINT('Ctrl Pts',(-3.37490270913961,-1.16462879365192,
39.4301908420194));
#67450=CARTESIAN_POINT('Ctrl Pts',(-3.32190256625949,-1.26399452116724,
39.444935534266));
#67451=CARTESIAN_POINT('Ctrl Pts',(-3.26442900579869,-1.36062889855108,
39.4597506949289));
#67452=CARTESIAN_POINT('Ctrl Pts',(-3.20700756171027,-1.45717564897817,
39.4745524213722));
#67453=CARTESIAN_POINT('Ctrl Pts',(-3.14512006233126,-1.55099662208012,
39.4894244884898));
#67454=CARTESIAN_POINT('Ctrl Pts',(-3.07899866234672,-1.64176875367575,
39.5043881067291));
#67455=CARTESIAN_POINT('Ctrl Pts',(-3.01376226873766,-1.73132593950196,
39.5191514434024));
#67456=CARTESIAN_POINT('Ctrl Pts',(-2.9444038130544,-1.81791582497803,39.5340038968541));
#67457=CARTESIAN_POINT('Ctrl Pts',(-2.87112112190071,-1.90118490671918,
39.5489658372021));
#67458=CARTESIAN_POINT('Ctrl Pts',(-2.82601293849714,-1.95244007969242,
39.558175460084));
#67459=CARTESIAN_POINT('Ctrl Pts',(-2.7794174721576,-2.00243617037411,39.567426565951));
#67460=CARTESIAN_POINT('Ctrl Pts',(-2.73137782673631,-2.05108126664787,
39.5767239054783));
#67461=CARTESIAN_POINT('Ctrl Pts',(-2.70785849585012,-2.0748970151868,39.5812757126947));
#67462=CARTESIAN_POINT('Ctrl Pts',(-2.68399298220066,-2.09838882749915,
39.585838601668));
#67463=CARTESIAN_POINT('Ctrl Pts',(-2.65978622078055,-2.12154522361285,
39.59041312988));
#67464=CARTESIAN_POINT('Ctrl Pts',(-2.64944130372411,-2.13144126021869,
39.5923680842873));
#67465=CARTESIAN_POINT('Ctrl Pts',(-2.63903323298336,-2.14127680635578,
39.594325319609));
#67466=CARTESIAN_POINT('Ctrl Pts',(-2.62856497776732,-2.15104852675842,
39.5962843953922));
#67467=CARTESIAN_POINT('Ctrl Pts',(-2.54974767685836,-2.22462149679763,
39.6110346152064));
#67468=CARTESIAN_POINT('Ctrl Pts',(-2.4677942019439,-2.29432581076987,39.6258380873112));
#67469=CARTESIAN_POINT('Ctrl Pts',(-2.38291639940009,-2.35987680253582,
39.6407167938454));
#67470=CARTESIAN_POINT('Ctrl Pts',(-2.29950856647313,-2.4242925391071,39.6553378211526));
#67471=CARTESIAN_POINT('Ctrl Pts',(-2.21327611648925,-2.48469790320087,
39.6700314995361));
#67472=CARTESIAN_POINT('Ctrl Pts',(-2.12440130761369,-2.54077665854762,
39.684818688697));
#67473=CARTESIAN_POINT('Ctrl Pts',(-2.03317702032287,-2.59833790175464,
39.699996789323));
#67474=CARTESIAN_POINT('Ctrl Pts',(-1.93916819329382,-2.6513414739591,39.7152734101447));
#67475=CARTESIAN_POINT('Ctrl Pts',(-1.84256188381164,-2.69938792578526,
39.7306711093119));
#67476=CARTESIAN_POINT('Ctrl Pts',(-1.75241852072327,-2.74422007779779,
39.7450387049088));
#67477=CARTESIAN_POINT('Ctrl Pts',(-1.66001305141746,-2.78473593017921,
39.7595117205049));
#67478=CARTESIAN_POINT('Ctrl Pts',(-1.56549738334504,-2.82055985230118,
39.774108482969));
#67479=CARTESIAN_POINT('Ctrl Pts',(-1.55872095882304,-2.8231282952831,39.7751550169577));
#67480=CARTESIAN_POINT('Ctrl Pts',(-1.55193368901203,-2.82567259777892,
39.7762021870499));
#67481=CARTESIAN_POINT('Ctrl Pts',(-1.5451356309518,-2.82819261092012,39.77725));
#67482=CARTESIAN_POINT('Origin',(0.,0.,39.5));
#67483=CARTESIAN_POINT('Ctrl Pts',(-3.55517835629984,1.66474646536813,39.067));
#67484=CARTESIAN_POINT('Ctrl Pts',(-3.59346767298069,1.54867526405411,39.0814568953907));
#67485=CARTESIAN_POINT('Ctrl Pts',(-3.62650702796103,1.43121621681944,39.0959580292964));
#67486=CARTESIAN_POINT('Ctrl Pts',(-3.6541619006592,1.31275716621601,39.1105228138977));
#67487=CARTESIAN_POINT('Ctrl Pts',(-3.68131382207819,1.19645249656677,39.1248227129172));
#67488=CARTESIAN_POINT('Ctrl Pts',(-3.7032752972325,1.07918303068495,39.1391839684911));
#67489=CARTESIAN_POINT('Ctrl Pts',(-3.71986954241218,0.961317221364022,
39.153624952814));
#67490=CARTESIAN_POINT('Ctrl Pts',(-3.73616669269371,0.845561621349798,
39.1678073931224));
#67491=CARTESIAN_POINT('Ctrl Pts',(-3.74728703315826,0.729230135992343,
39.18206673289));
#67492=CARTESIAN_POINT('Ctrl Pts',(-3.75301552808992,0.612684385714019,
39.1964203750936));
#67493=CARTESIAN_POINT('Ctrl Pts',(-3.755542939032,0.561264421478854,39.2027531994736));
#67494=CARTESIAN_POINT('Ctrl Pts',(-3.7570201630815,0.509802978089015,39.2091043805096));
#67495=CARTESIAN_POINT('Ctrl Pts',(-3.75742574055319,0.458332442123154,
39.2154754128171));
#67496=CARTESIAN_POINT('Ctrl Pts',(-3.75764127879252,0.430979175550461,
39.2188612051307));
#67497=CARTESIAN_POINT('Ctrl Pts',(-3.75755412750489,0.403623356983449,
39.2222526039123));
#67498=CARTESIAN_POINT('Ctrl Pts',(-3.75716085210795,0.376269966068251,
39.2256498334886));
#67499=CARTESIAN_POINT('Ctrl Pts',(-3.75691574882173,0.359222355018006,
39.2277671084051));
#67500=CARTESIAN_POINT('Ctrl Pts',(-3.75655173700823,0.34217568862123,39.2298866481352));
#67501=CARTESIAN_POINT('Ctrl Pts',(-3.75606795588435,0.325131190221386,
39.2320085069836));
#67502=CARTESIAN_POINT('Ctrl Pts',(-3.75571123254104,0.312563171019651,
39.233573091762));
#67503=CARTESIAN_POINT('Ctrl Pts',(-3.75528936565693,0.299996514206195,
39.2351389152941));
#67504=CARTESIAN_POINT('Ctrl Pts',(-3.7548024159468,0.287440005344609,39.2367049633161));
#67505=CARTESIAN_POINT('Ctrl Pts',(-3.75102773997828,0.19010602760176,39.2488444588559));
#67506=CARTESIAN_POINT('Ctrl Pts',(-3.74334047216327,0.0932328369217743,
39.2610159266466));
#67507=CARTESIAN_POINT('Ctrl Pts',(-3.7316481904409,-0.0029745009063645,
39.273231107418));
#67508=CARTESIAN_POINT('Ctrl Pts',(2.28405859260867,-3.20180657528379,-0.410063028691932));
#67509=CARTESIAN_POINT('Ctrl Pts',(3.35101936364523,-2.44067349002037,-0.343767612025265));
#67510=CARTESIAN_POINT('Ctrl Pts',(4.64535438600488,0.219163159607182,-0.211176778691931));
#67511=CARTESIAN_POINT('Ctrl Pts',(2.32227978484365,4.03443500934324,-0.0122905286919314));
#67512=CARTESIAN_POINT('Ctrl Pts',(-2.13685955260049,4.13065816376694,0.18659572130807));
#67513=CARTESIAN_POINT('Ctrl Pts',(-4.63131485374691,0.437059737780703,
0.38548197130807));
#67514=CARTESIAN_POINT('Ctrl Pts',(-2.87058777509758,-3.6612002757226,0.58436822130807));
#67515=CARTESIAN_POINT('Ctrl Pts',(1.52825192091582,-4.39356078829283,0.78325447130807));
#67516=CARTESIAN_POINT('Ctrl Pts',(4.52260840884179,-1.08946538597355,0.982140721308071));
#67517=CARTESIAN_POINT('Ctrl Pts',(3.36117901623604,3.21618372219525,1.18102697130807));
#67518=CARTESIAN_POINT('Ctrl Pts',(-0.888913231377699,4.56622408239327,
1.37991322130807));
#67519=CARTESIAN_POINT('Ctrl Pts',(-4.32215201846994,1.72043564577458,1.57879947130807));
#67520=CARTESIAN_POINT('Ctrl Pts',(-3.78373551838476,-2.70633956790168,
1.77768572130807));
#67521=CARTESIAN_POINT('Ctrl Pts',(0.231598108743597,-4.64620095483734,
1.97657197130807));
#67522=CARTESIAN_POINT('Ctrl Pts',(4.03411078631178,-2.3166405035163,2.17545822130807));
#67523=CARTESIAN_POINT('Ctrl Pts',(4.12964193630134,2.14171203558755,2.37434447130808));
#67524=CARTESIAN_POINT('Ctrl Pts',(0.430404503435925,4.63202015931436,2.57323072130807));
#67525=CARTESIAN_POINT('Ctrl Pts',(-3.66433530838834,2.86592281387884,2.77211697130807));
#67526=CARTESIAN_POINT('Ctrl Pts',(-4.39188239410591,-1.53369983889943,
2.97100322130807));
#67527=CARTESIAN_POINT('Ctrl Pts',(-1.0836863715155,-4.52399029506003,3.16988947130807));
#67528=CARTESIAN_POINT('Ctrl Pts',(3.22031941745,-3.35714289255106,3.36877572130807));
#67529=CARTESIAN_POINT('Ctrl Pts',(4.56514274797943,0.89461559064575,3.56766197130807));
#67530=CARTESIAN_POINT('Ctrl Pts',(1.71501247192487,4.32430310693921,3.76654822130808));
#67531=CARTESIAN_POINT('Ctrl Pts',(-2.71105925393979,3.78034694695518,3.96543447130807));
#67532=CARTESIAN_POINT('Ctrl Pts',(-4.64591255536892,-0.237406415989334,
4.16432072130808));
#67533=CARTESIAN_POINT('Ctrl Pts',(-2.31159211256507,-4.03700472592018,
4.36320697130807));
#67534=CARTESIAN_POINT('Ctrl Pts',(2.14687255908044,-4.12696056350751,4.56209322130808));
#67535=CARTESIAN_POINT('Ctrl Pts',(4.63255538357458,-0.424612633481082,
4.76097947130807));
#67536=CARTESIAN_POINT('Ctrl Pts',(2.86133849969297,3.66791592838001,4.95986572130809));
#67537=CARTESIAN_POINT('Ctrl Pts',(-1.53918985797284,4.38996125862584,5.15875197130807));
#67538=CARTESIAN_POINT('Ctrl Pts',(-4.5253418479552,1.07802895555233,5.35763822130809));
#67539=CARTESIAN_POINT('Ctrl Pts',(-3.35311367917035,-3.22451452534221,
5.55652447130807));
#67540=CARTESIAN_POINT('Ctrl Pts',(0.900322906953032,-4.56402058861491,
5.75541072130808));
#67541=CARTESIAN_POINT('Ctrl Pts',(4.32644411261801,-1.70960422620876,5.95429697130808));
#67542=CARTESIAN_POINT('Ctrl Pts',(3.7769542019951,2.71578390633149,6.15318322130808));
#67543=CARTESIAN_POINT('Ctrl Pts',(-0.243215259837961,4.64561208101878,
6.35206947130807));
#67544=CARTESIAN_POINT('Ctrl Pts',(-4.039891879632,2.30654262279634,6.55095572130809));
#67545=CARTESIAN_POINT('Ctrl Pts',(-4.12427298672108,-2.1520310408764,6.74984197130808));
#67546=CARTESIAN_POINT('Ctrl Pts',(-0.41881997004075,-4.63308267815251,
6.94872822130808));
#67547=CARTESIAN_POINT('Ctrl Pts',(3.6714907462362,-2.85675007135706,7.14761447130808));
#67548=CARTESIAN_POINT('Ctrl Pts',(4.38803329537382,1.54467765847374,7.34650072130808));
#67549=CARTESIAN_POINT('Ctrl Pts',(1.0723698356974,4.52668622784753,7.54538697130808));
#67550=CARTESIAN_POINT('Ctrl Pts',(-3.22870458239833,3.34907927488996,7.74427322130807));
#67551=CARTESIAN_POINT('Ctrl Pts',(-4.56289129899062,-0.906028842528388,
7.94315947130809));
#67552=CARTESIAN_POINT('Ctrl Pts',(-1.70419330507885,-4.32857834038177,
8.14204572130808));
#67553=CARTESIAN_POINT('Ctrl Pts',(2.72050431152591,-3.77355555953089,8.34093197130808));
#67554=CARTESIAN_POINT('Ctrl Pts',(4.64530434451287,0.249023727278098,8.53981822130808));
#67555=CARTESIAN_POINT('Ctrl Pts',(2.30148952663657,4.04277271543675,8.73870447130808));
#67556=CARTESIAN_POINT('Ctrl Pts',(-2.15718615802268,4.12157896315634,8.93759072130809));
#67557=CARTESIAN_POINT('Ctrl Pts',(-4.63360272954349,0.413026651276645,
9.13647697130808));
#67558=CARTESIAN_POINT('Ctrl Pts',(-2.85215717676813,-3.67505982385426,
9.33536322130809));
#67559=CARTESIAN_POINT('Ctrl Pts',(1.55016304402113,-4.38609847208755,9.53424947130807));
#67560=CARTESIAN_POINT('Ctrl Pts',(4.52802353080303,-1.06670903923785,9.7331357213081));
#67561=CARTESIAN_POINT('Ctrl Pts',(3.34503963470285,3.23288959170657,9.93202197130807));
#67562=CARTESIAN_POINT('Ctrl Pts',(-0.911733361628194,4.56175487583362,
10.1309082213081));
#67563=CARTESIAN_POINT('Ctrl Pts',(-4.33070580091485,1.69877971962819,10.3297944713081));
#67564=CARTESIAN_POINT('Ctrl Pts',(-3.7701510175469,-2.72522046351992,10.5286807213081));
#67565=CARTESIAN_POINT('Ctrl Pts',(0.254831805397762,-4.64498934561268,
10.7275669713081));
#67566=CARTESIAN_POINT('Ctrl Pts',(4.04564723083314,-2.29643283236192,10.9264532213081));
#67567=CARTESIAN_POINT('Ctrl Pts',(4.11887849597835,2.16233790265648,11.1253394713081));
#67568=CARTESIAN_POINT('Ctrl Pts',(0.407232686793075,4.6341155368317,11.3242257213081));
#67569=CARTESIAN_POINT('Ctrl Pts',(-3.67862315594041,2.84755982316029,11.5231119713081));
#67570=CARTESIAN_POINT('Ctrl Pts',(-4.38415679164241,-1.55564600606735,
11.7219982213081));
#67571=CARTESIAN_POINT('Ctrl Pts',(-1.0610465751018,-4.52935375471627,11.9208844713081));
#67572=CARTESIAN_POINT('Ctrl Pts',(3.23706954676494,-3.34099476493225,12.1197707213081));
#67573=CARTESIAN_POINT('Ctrl Pts',(4.56061132089925,0.917436455338055,12.3186569713081));
#67574=CARTESIAN_POINT('Ctrl Pts',(1.69336347833148,4.33282649088915,12.5175432213081));
#67575=CARTESIAN_POINT('Ctrl Pts',(-2.72993235494621,3.7667405813668,12.7164294713081));
#67576=CARTESIAN_POINT('Ctrl Pts',(-4.64466708480763,-0.260639485117335,
12.9153157213081));
#67577=CARTESIAN_POINT('Ctrl Pts',(-2.2913725478795,-4.04851542132692,13.1142019713081));
#67578=CARTESIAN_POINT('Ctrl Pts',(2.1674862667245,-4.11617158940907,13.3130882213081));
#67579=CARTESIAN_POINT('Ctrl Pts',(4.63462109921499,-0.401438085648196,
13.5119744713081));
#67580=CARTESIAN_POINT('Ctrl Pts',(2.84295801772125,3.68218073692372,13.7108607213081));
#67581=CARTESIAN_POINT('Ctrl Pts',(-1.56112653604057,4.382208257074,13.9097469713081));
#67582=CARTESIAN_POINT('Ctrl Pts',(-4.53067689750755,1.05538245214185,14.1086332213081));
#67583=CARTESIAN_POINT('Ctrl Pts',(-3.33694467190181,-3.24124444103862,
14.3075194713081));
#67584=CARTESIAN_POINT('Ctrl Pts',(0.923138114741901,-4.55946063597531,
14.5064057213081));
#67585=CARTESIAN_POINT('Ctrl Pts',(4.33494040698919,-1.68794458965632,14.7052919713081));
#67586=CARTESIAN_POINT('Ctrl Pts',(3.76332425632244,2.73463997843825,14.9041782213081));
#67587=CARTESIAN_POINT('Ctrl Pts',(-0.266446757357151,4.64433756260153,
15.1030644713081));
#67588=CARTESIAN_POINT('Ctrl Pts',(-4.05137728243396,2.28630868110051,15.3019507213081));
#67589=CARTESIAN_POINT('Ctrl Pts',(-4.11345824768048,-2.17263124217781,
15.5008369713081));
#67590=CARTESIAN_POINT('Ctrl Pts',(-0.395642856901232,-4.63511941590297,
15.6997232213081));
#67591=CARTESIAN_POINT('Ctrl Pts',(3.68573256124231,-2.83835176764541,15.8986094713081));
#67592=CARTESIAN_POINT('Ctrl Pts',(4.38025287142865,1.56660462537257,16.0974957213081));
#67593=CARTESIAN_POINT('Ctrl Pts',(1.0497166792132,4.5319929571083,16.2963819713081));
#67594=CARTESIAN_POINT('Ctrl Pts',(-3.24541426800062,3.33288936194342,16.4952682213081));
#67595=CARTESIAN_POINT('Ctrl Pts',(-4.55830282286078,-0.928838330925807,
16.6941544713081));
#67596=CARTESIAN_POINT('Ctrl Pts',(-1.6825230620746,-4.33704754591008,16.8930407213081));
#67597=CARTESIAN_POINT('Ctrl Pts',(2.73934332663622,-3.75990204775488,17.0919269713081));
#67598=CARTESIAN_POINT('Ctrl Pts',(4.64400077950955,0.272253613038182,17.2908132213081));
#67599=CARTESIAN_POINT('Ctrl Pts',(2.28124123994172,4.05423280968013,17.4896994713081));
#67600=CARTESIAN_POINT('Ctrl Pts',(-2.1777728209729,4.11073847503455,17.6885857213081));
#67601=CARTESIAN_POINT('Ctrl Pts',(-4.63561048611658,0.389847009612274,
17.8874719713081));
#67602=CARTESIAN_POINT('Ctrl Pts',(-2.83374108013408,-3.68927862334333,
18.0863582213081));
#67603=CARTESIAN_POINT('Ctrl Pts',(1.57208026549899,-4.37829063776336,18.2852444713081));
#67604=CARTESIAN_POINT('Ctrl Pts',(4.53330193146099,-1.0440492651737,18.4841307213081));
#67605=CARTESIAN_POINT('Ctrl Pts',(3.32882884139711,3.24957902113188,18.6830169713081));
#67606=CARTESIAN_POINT('Ctrl Pts',(-0.934537094978153,4.55713788336577,
18.8819032213081));
#67607=CARTESIAN_POINT('Ctrl Pts',(-4.33914790435761,1.67709890406219,19.0807894713081));
#67608=CARTESIAN_POINT('Ctrl Pts',(-3.75647396101428,-2.744042392187,19.2796757213081));
#67609=CARTESIAN_POINT('Ctrl Pts',(0.278060043082108,-4.6436567360582,19.4785619713081));
#67610=CARTESIAN_POINT('Ctrl Pts',(4.05708199860109,-2.27617023232547,19.6774482213081));
#67611=CARTESIAN_POINT('Ctrl Pts',(4.10801227572337,2.18291099507144,19.8763344713081));
#67612=CARTESIAN_POINT('Ctrl Pts',(0.38405055284252,4.63609430908809,20.0752207213081));
#67613=CARTESIAN_POINT('Ctrl Pts',(-3.69281891768294,2.82912596239557,20.2741069713081));
#67614=CARTESIAN_POINT('Ctrl Pts',(-4.37632155914585,-1.57755344785935,
20.4729932213081));
#67615=CARTESIAN_POINT('Ctrl Pts',(-1.03838021888359,-4.5346038185192,20.6718794713081));
#67616=CARTESIAN_POINT('Ctrl Pts',(3.2537386939213,-3.324763116611,20.8707657213081));
#67617=CARTESIAN_POINT('Ctrl Pts',(4.55596581931151,0.940234397989585,21.0696519713081));
#67618=CARTESIAN_POINT('Ctrl Pts',(1.67167212409921,4.34124147904805,21.2685382213081));
#67619=CARTESIAN_POINT('Ctrl Pts',(-2.74873716774412,3.75304000146011,21.4674244713081));
#67620=CARTESIAN_POINT('Ctrl Pts',(-4.6433054327854,-0.283866038411237,
21.6663107213081));
#67621=CARTESIAN_POINT('Ctrl Pts',(-2.27109566617969,-4.0599248447425,21.8651969713081));
#67622=CARTESIAN_POINT('Ctrl Pts',(2.18804575644055,-4.10527965400899,22.0640832213081));
#67623=CARTESIAN_POINT('Ctrl Pts',(4.63657088406109,-0.378253495654039,
22.2629694713081));
#67624=CARTESIAN_POINT('Ctrl Pts',(2.82450642164506,3.69635343872626,22.4618557213081));
#67625=CARTESIAN_POINT('Ctrl Pts',(-1.58302416389686,4.37434563865457,22.6607419713081));
#67626=CARTESIAN_POINT('Ctrl Pts',(-4.53589861624757,1.03270954920589,22.8596282213081));
#67627=CARTESIAN_POINT('Ctrl Pts',(-3.32069219394143,-3.25789327986572,
23.0585144713081));
#67628=CARTESIAN_POINT('Ctrl Pts',(0.945930231053035,-4.55478663253039,
23.2574007213081));
#67629=CARTESIAN_POINT('Ctrl Pts',(4.34332826670835,-1.66624273066974,23.4562869713081));
#67630=CARTESIAN_POINT('Ctrl Pts',(3.74960017446099,2.75342764596779,23.6551732213081));
#67631=CARTESIAN_POINT('Ctrl Pts',(-0.289671589948523,4.64294687024033,
23.8540594713081));
#67632=CARTESIAN_POINT('Ctrl Pts',(-4.06276134365987,2.26601754943795,24.0529457213081));
#67633=CARTESIAN_POINT('Ctrl Pts',(-4.10254061416358,-2.19317709705255,
24.2518319713081));
#67634=CARTESIAN_POINT('Ctrl Pts',(-0.372455847109915,-4.63704021029053,
24.4507182213082));
#67635=CARTESIAN_POINT('Ctrl Pts',(3.6998821809475,-2.81988246510469,24.6496044713081));
#67636=CARTESIAN_POINT('Ctrl Pts',(4.37236287937863,1.58849240505882,24.8484907213081));
#67637=CARTESIAN_POINT('Ctrl Pts',(1.02703726500591,4.53718632262184,25.0473769713081));
#67638=CARTESIAN_POINT('Ctrl Pts',(-3.2620427724699,3.31661607975275,25.2462632213081));
#67639=CARTESIAN_POINT('Ctrl Pts',(-4.55360032486595,-0.951624585263666,
25.4451494713081));
#67640=CARTESIAN_POINT('Ctrl Pts',(-1.66081073226206,-4.34540826407608,
25.6440357213081));
#67641=CARTESIAN_POINT('Ctrl Pts',(2.75811381952511,-3.74615448539464,25.8429219713081));
#67642=CARTESIAN_POINT('Ctrl Pts',(4.64258104898355,0.295476688617761,26.0418082213081));
#67643=CARTESIAN_POINT('Ctrl Pts',(2.2609358900392,4.06559149091866,26.2406944713081));
#67644=CARTESIAN_POINT('Ctrl Pts',(-2.19830500888522,4.09979516046932,26.4395807213081));
#67645=CARTESIAN_POINT('Ctrl Pts',(-4.63750228704264,0.366657616274049,
26.6384669713081));
#67646=CARTESIAN_POINT('Ctrl Pts',(-2.81525410000349,-3.70340513882985,
26.8373532213081));
#67647=CARTESIAN_POINT('Ctrl Pts',(1.59395816279613,-4.37037328441786,27.0362394713081));
#67648=CARTESIAN_POINT('Ctrl Pts',(4.53846693562883,-1.02136337515174,27.2351257213081));
#67649=CARTESIAN_POINT('Ctrl Pts',(3.31253478041756,3.26618716524659,27.4340119713081));
#67650=CARTESIAN_POINT('Ctrl Pts',(-0.957317451719108,4.55240689817286,
27.6328982213081));
#67651=CARTESIAN_POINT('Ctrl Pts',(-4.34748146789946,1.65537613736835,27.8317844713081));
#67652=CARTESIAN_POINT('Ctrl Pts',(-3.74270293964795,-2.76279568108975,
28.0306707213081));
#67653=CARTESIAN_POINT('Ctrl Pts',(0.301281325343274,-4.64220796958699,
28.2295569713081));
#67654=CARTESIAN_POINT('Ctrl Pts',(4.06841528209427,-2.25585069592812,28.4284432213081));
#67655=CARTESIAN_POINT('Ctrl Pts',(4.09704329721841,2.2034294839217,28.6273294713081));
#67656=CARTESIAN_POINT('Ctrl Pts',(0.360858812211213,4.63795711359509,28.8262157213081));
#67657=CARTESIAN_POINT('Ctrl Pts',(-3.70692230686563,2.81062133357725,29.0251019713081));
#67658=CARTESIAN_POINT('Ctrl Pts',(-4.36837685688271,-1.5994214285638,29.2239882213081));
#67659=CARTESIAN_POINT('Ctrl Pts',(-1.0156878885138,-4.53974045326646,29.4228744713081));
#67660=CARTESIAN_POINT('Ctrl Pts',(3.27032645171657,-3.30844830231646,29.6217607213081));
#67661=CARTESIAN_POINT('Ctrl Pts',(4.55120635431684,0.96300882151919,29.8206469713082));
#67662=CARTESIAN_POINT('Ctrl Pts',(1.6499389544851,4.34954787493714,30.0195332213081));
#67663=CARTESIAN_POINT('Ctrl Pts',(-2.76747322334208,3.73924554261714,30.2184194713081));
#67664=CARTESIAN_POINT('Ctrl Pts',(-4.64182763263396,-0.307085491050202,
30.4173057213081));
#67665=CARTESIAN_POINT('Ctrl Pts',(-2.2507619750547,-4.07123271277209,30.6161919713081));
#67666=CARTESIAN_POINT('Ctrl Pts',(2.20855051415048,-4.09428502871299,30.8150782213081));
#67667=CARTESIAN_POINT('Ctrl Pts',(4.63840468923668,-0.355059443987292,
31.0139644713082));
#67668=CARTESIAN_POINT('Ctrl Pts',(2.80598417306898,3.71043367955604,31.2128507213081));
#67669=CARTESIAN_POINT('Ctrl Pts',(-1.60488219382066,4.36637359989451,31.4117369713082));
#67670=CARTESIAN_POINT('Ctrl Pts',(-4.54100687354372,1.01001081396483,31.6106232213081));
#67671=CARTESIAN_POINT('Ctrl Pts',(-3.3043566518382,-3.27446062540828,31.8095094713081));
#67672=CARTESIAN_POINT('Ctrl Pts',(0.968698685766213,-4.54999869517525,
32.0083957213081));
#67673=CARTESIAN_POINT('Ctrl Pts',(4.35160748195836,-1.64449919211191,32.2072819713081));
#67674=CARTESIAN_POINT('Ctrl Pts',(3.73578229970788,2.77214643896784,32.4061682213081));
#67675=CARTESIAN_POINT('Ctrl Pts',(-0.312889176665352,4.64144003872198,
32.6050544713081));
#67676=CARTESIAN_POINT('Ctrl Pts',(-4.07404377854549,2.245669735369,32.8039407213081));
#67677=CARTESIAN_POINT('Ctrl Pts',(-4.09152035926885,-2.21366809155445,
33.0028269713081));
#67678=CARTESIAN_POINT('Ctrl Pts',(-0.349259520662366,-4.63884501328854,
33.2017132213082));
#67679=CARTESIAN_POINT('Ctrl Pts',(3.71393925139909,-2.80134262568852,33.4005994713081));
#67680=CARTESIAN_POINT('Ctrl Pts',(4.36436351660891,1.61034044995361,33.5994857213082));
#67681=CARTESIAN_POINT('Ctrl Pts',(1.0043321603347,4.54226619462571,33.7983719713081));
#67682=CARTESIAN_POINT('Ctrl Pts',(-3.2785896797709,3.30025983510218,33.9972582213082));
#67683=CARTESIAN_POINT('Ctrl Pts',(-4.54878392280352,-0.974387035033758,
34.1961444713081));
#67684=CARTESIAN_POINT('Ctrl Pts',(-1.63905685843296,-4.35366028675904,
34.3950307213081));
#67685=CARTESIAN_POINT('Ctrl Pts',(2.77681532004856,-3.73231321439111,34.5939169713081));
#67686=CARTESIAN_POINT('Ctrl Pts',(4.64104518962864,0.318692369397484,34.7928032213081));
#67687=CARTESIAN_POINT('Ctrl Pts',(2.24057398259076,4.07684848213216,34.9916894713081));
#67688=CARTESIAN_POINT('Ctrl Pts',(-2.21878220384499,4.08874927960163,35.1905757213081));
#67689=CARTESIAN_POINT('Ctrl Pts',(-4.63927809326544,0.343459077334103,
35.3894619713081));
#67690=CARTESIAN_POINT('Ctrl Pts',(-2.79669668299912,-3.71743906671155,
35.5883482213081));
#67691=CARTESIAN_POINT('Ctrl Pts',(1.6157961584067,-4.3623465149027,35.7872344713082));
#67692=CARTESIAN_POINT('Ctrl Pts',(4.54351847197868,-0.998652118751192,
35.9861207213081));
#67693=CARTESIAN_POINT('Ctrl Pts',(3.29615774863631,3.28271395700534,36.1850069713081));
#67694=CARTESIAN_POINT('Ctrl Pts',(-0.980073650227081,4.54756137209857,
36.3838932213081));
#67695=CARTESIAN_POINT('Ctrl Pts',(-4.35570668825951,1.63361323797604,36.5827794713081));
#67696=CARTESIAN_POINT('Ctrl Pts',(-3.72883752278967,-2.78148230039399,
36.7816657213081));
#67697=CARTESIAN_POINT('Ctrl Pts',(0.324493588450696,-4.64063841596816,
36.9805519713081));
#67698=CARTESIAN_POINT('Ctrl Pts',(4.07964963465135,-2.23548365871144,37.1794382213081));
#67699=CARTESIAN_POINT('Ctrl Pts',(4.08596640779809,2.22390993440854,37.3783244713081));
#67700=CARTESIAN_POINT('Ctrl Pts',(0.337668427315605,4.63967123153578,37.5772107213081));
#67701=CARTESIAN_POINT('Ctrl Pts',(-3.72095283273302,2.79210890379928,37.7760969713081));
#67702=CARTESIAN_POINT('Ctrl Pts',(-4.3602848861238,-1.6213689767605,37.9749832213081));
#67703=CARTESIAN_POINT('Ctrl Pts',(-0.993042844038055,-4.54453476652035,
38.1738694713081));
#67704=CARTESIAN_POINT('Ctrl Pts',(3.28697147748708,-3.29248844184413,38.3727557213081));
#67705=CARTESIAN_POINT('Ctrl Pts',(4.54606692907903,0.986597164631765,38.5716419713082));
#67706=CARTESIAN_POINT('Ctrl Pts',(1.62867416074003,4.35613660157396,38.7705282213081));
#67707=CARTESIAN_POINT('Ctrl Pts',(-2.78711997617271,3.72848648678348,38.9694144713082));
#67708=CARTESIAN_POINT('Ctrl Pts',(-4.63831401868151,-0.336738661585157,
39.1683007213081));
#67709=CARTESIAN_POINT('Ctrl Pts',(-3.03582612181379,-2.82311487873352,
39.3008915546415));
#67710=CARTESIAN_POINT('Ctrl Pts',(-1.88566238042959,-3.45148756147731,
39.3671869713081));
#67711=CARTESIAN_POINT('Ctrl Pts',(2.14656790565208,-3.00907133330608,-0.273375352461288));
#67712=CARTESIAN_POINT('Ctrl Pts',(3.14930214159003,-2.29375524726366,-0.207079935794621));
#67713=CARTESIAN_POINT('Ctrl Pts',(4.36572365859917,0.205970462419992,-0.0744891024612875));
#67714=CARTESIAN_POINT('Ctrl Pts',(2.18248834343466,3.79157904990716,0.124397147538712));
#67715=CARTESIAN_POINT('Ctrl Pts',(-2.00822962656989,3.88200997656335,0.323283397538713));
#67716=CARTESIAN_POINT('Ctrl Pts',(-4.35252924692651,0.410750586262939,
0.522169647538713));
#67717=CARTESIAN_POINT('Ctrl Pts',(-2.69779050691701,-3.44081147193987,
0.721055897538714));
#67718=CARTESIAN_POINT('Ctrl Pts',(1.43625760556443,-4.129086972725,0.919942147538715));
#67719=CARTESIAN_POINT('Ctrl Pts',(4.25036647118775,-1.02388416804092,1.11882839753871));
#67720=CARTESIAN_POINT('Ctrl Pts',(3.15885022597575,3.02258303665498,1.31771464753872));
#67721=CARTESIAN_POINT('Ctrl Pts',(-0.835404406681822,4.29135666527998,
1.51660089753871));
#67722=CARTESIAN_POINT('Ctrl Pts',(-4.06197670945066,1.616872681336,1.71548714753872));
#67723=CARTESIAN_POINT('Ctrl Pts',(-3.55597061017793,-2.54342934855236,
1.91437339753872));
#67724=CARTESIAN_POINT('Ctrl Pts',(0.217656880102546,-4.36651926756103,
2.11325964753872));
#67725=CARTESIAN_POINT('Ctrl Pts',(3.79127434373374,-2.17718852304153,2.31214589753872));
#67726=CARTESIAN_POINT('Ctrl Pts',(3.88105492170199,2.01279001056198,2.51103214753871));
#67727=CARTESIAN_POINT('Ctrl Pts',(0.404495968935988,4.35319209607569,2.70991839753872));
#67728=CARTESIAN_POINT('Ctrl Pts',(-3.44375778887116,2.69340635667425,2.90880464753871));
#67729=CARTESIAN_POINT('Ctrl Pts',(-4.12750961078415,-1.44137758187943,
3.10769089753872));
#67730=CARTESIAN_POINT('Ctrl Pts',(-1.01845302586177,-4.25166517368817,
3.30657714753872));
#67731=CARTESIAN_POINT('Ctrl Pts',(3.02646978051091,-3.15505705990135,3.50546339753872));
#67732=CARTESIAN_POINT('Ctrl Pts',(4.29034042263387,0.840763507989867,3.70434964753872));
#67733=CARTESIAN_POINT('Ctrl Pts',(1.61177595966248,4.06399831147317,3.90323589753872));
#67734=CARTESIAN_POINT('Ctrl Pts',(-2.54786492941134,3.55278601644629,4.10212214753872));
#67735=CARTESIAN_POINT('Ctrl Pts',(-4.36624822852336,-0.223115551767193,
4.30100839753872));
#67736=CARTESIAN_POINT('Ctrl Pts',(-2.17244402391783,-3.79399408039216,
4.49989464753872));
#67737=CARTESIAN_POINT('Ctrl Pts',(2.01763989232161,-3.87853495623309,4.69878089753872));
#67738=CARTESIAN_POINT('Ctrl Pts',(4.35369510209446,-0.399052745106703,
4.89766714753871));
#67739=CARTESIAN_POINT('Ctrl Pts',(2.68909799885338,3.44712287065204,5.09655339753873));
#67740=CARTESIAN_POINT('Ctrl Pts',(-1.44653712497633,4.12570411955144,5.29543964753872));
#67741=CARTESIAN_POINT('Ctrl Pts',(-4.25293536880354,1.01313616246135,5.49432589753872));
#67742=CARTESIAN_POINT('Ctrl Pts',(-3.15127038816007,-3.03041236061429,
5.69321214753872));
#67743=CARTESIAN_POINT('Ctrl Pts',(0.846127267944299,-4.2892858125268,5.89209839753872));
#67744=CARTESIAN_POINT('Ctrl Pts',(4.06601043764664,-1.60669326751191,6.09098464753873));
#67745=CARTESIAN_POINT('Ctrl Pts',(3.54959750041304,2.55230517767038,6.28987089753872));
#67746=CARTESIAN_POINT('Ctrl Pts',(-0.228574727733499,4.36596584146089,
6.48875714753872));
#67747=CARTESIAN_POINT('Ctrl Pts',(-3.79670743963632,2.16769849212081,6.68764339753873));
#67748=CARTESIAN_POINT('Ctrl Pts',(-3.87600916022575,-2.02248785528584,
6.88652964753872));
#67749=CARTESIAN_POINT('Ctrl Pts',(-0.393608775556405,-4.35419065576435,
7.08541589753873));
#67750=CARTESIAN_POINT('Ctrl Pts',(3.45048249956151,-2.68478577453692,7.28430214753871));
#67751=CARTESIAN_POINT('Ctrl Pts',(4.12389221154984,1.45169458304942,7.48318839753873));
#67752=CARTESIAN_POINT('Ctrl Pts',(1.00781769773627,4.25419882270057,7.68207464753872));
#67753=CARTESIAN_POINT('Ctrl Pts',(-3.03435019392059,3.14747883798937,7.88096089753873));
#67754=CARTESIAN_POINT('Ctrl Pts',(-4.2882245013715,-0.851489730281045,
8.07984714753873));
#67755=CARTESIAN_POINT('Ctrl Pts',(-1.60160806099616,-4.06801619390695,
8.27873339753872));
#67756=CARTESIAN_POINT('Ctrl Pts',(2.5567414343955,-3.54640344188055,8.47761964753874));
#67757=CARTESIAN_POINT('Ctrl Pts',(4.36567662939378,0.234033549949525,8.67650589753872));
#67758=CARTESIAN_POINT('Ctrl Pts',(2.16294957102227,3.79941486128476,8.87539214753873));
#67759=CARTESIAN_POINT('Ctrl Pts',(-2.02733265613809,3.87347730550896,9.07427839753872));
#67760=CARTESIAN_POINT('Ctrl Pts',(-4.35467940225657,0.388164190130051,
9.27316464753873));
#67761=CARTESIAN_POINT('Ctrl Pts',(-2.68046935281703,-3.45383673377096,
9.47205089753873));
#67762=CARTESIAN_POINT('Ctrl Pts',(1.456849771539,-4.12207385645912,9.67093714753872));
#67763=CARTESIAN_POINT('Ctrl Pts',(4.25545562566251,-1.00249765733107,9.86982339753873));
#67764=CARTESIAN_POINT('Ctrl Pts',(3.14368236709142,3.03828328333213,10.0687096475387));
#67765=CARTESIAN_POINT('Ctrl Pts',(-0.856850861408087,4.28715648609206,
10.2675958975387));
#67766=CARTESIAN_POINT('Ctrl Pts',(-4.07001559029531,1.59652035054053,10.4664821475387));
#67767=CARTESIAN_POINT('Ctrl Pts',(-3.54320383895445,-2.56117369394491,
10.6653683975387));
#67768=CARTESIAN_POINT('Ctrl Pts',(0.239492006280512,-4.36538059209787,
10.8642546475387));
#67769=CARTESIAN_POINT('Ctrl Pts',(3.80211634298675,-2.15819726840019,11.0631408975387));
#67770=CARTESIAN_POINT('Ctrl Pts',(3.87093939505723,2.0321742874889,11.2620271475387));
#67771=CARTESIAN_POINT('Ctrl Pts',(0.382718997853834,4.35516134071043,11.4609133975387));
#67772=CARTESIAN_POINT('Ctrl Pts',(-3.45718556830527,2.67614874049235,11.6597996475387));
#67773=CARTESIAN_POINT('Ctrl Pts',(-4.12024905698152,-1.46200268241196,
11.8586858975387));
#67774=CARTESIAN_POINT('Ctrl Pts',(-0.997176049636473,-4.25670577571064,
12.0575721475387));
#67775=CARTESIAN_POINT('Ctrl Pts',(3.04221162273831,-3.13988098140884,12.2564583975387));
#67776=CARTESIAN_POINT('Ctrl Pts',(4.28608176833814,0.862210652947643,12.4553446475387));
#67777=CARTESIAN_POINT('Ctrl Pts',(1.59143014410956,4.07200862368394,12.6542308975387));
#67778=CARTESIAN_POINT('Ctrl Pts',(-2.5656019493948,3.53999869663798,12.8531171475387));
#67779=CARTESIAN_POINT('Ctrl Pts',(-4.36507773003311,-0.244950088193424,
13.0520033975387));
#67780=CARTESIAN_POINT('Ctrl Pts',(-2.15344159168568,-3.80481188051856,
13.2508896475387));
#67781=CARTESIAN_POINT('Ctrl Pts',(2.0370127417697,-3.86839543283839,13.4497758975388));
#67782=CARTESIAN_POINT('Ctrl Pts',(4.35563647037208,-0.377273207240618,
13.6486621475387));
#67783=CARTESIAN_POINT('Ctrl Pts',(2.67182394431791,3.46052899792885,13.8475483975387));
#67784=CARTESIAN_POINT('Ctrl Pts',(-1.46715330761245,4.11841781596996,14.0464346475388));
#67785=CARTESIAN_POINT('Ctrl Pts',(-4.25794927089048,0.991852882972159,
14.2453208975387));
#67786=CARTESIAN_POINT('Ctrl Pts',(-3.13607468688462,-3.04613520599768,
14.4442071475388));
#67787=CARTESIAN_POINT('Ctrl Pts',(0.867569096520351,-4.28500034978993,
14.6430933975387));
#67788=CARTESIAN_POINT('Ctrl Pts',(4.07399529095696,-1.58633744966117,14.8419796475388));
#67789=CARTESIAN_POINT('Ctrl Pts',(3.53678801994201,2.57002619382208,15.0408658975387));
#67790=CARTESIAN_POINT('Ctrl Pts',(-0.250407787155136,4.364768043673,15.2397521475388));
#67791=CARTESIAN_POINT('Ctrl Pts',(-3.80750146966602,2.14868254831374,15.4386383975387));
#67792=CARTESIAN_POINT('Ctrl Pts',(-3.86584542282966,-2.04184801141611,
15.6375246475387));
#67793=CARTESIAN_POINT('Ctrl Pts',(-0.371826826804321,-4.35610479049868,
15.8364108975387));
#67794=CARTESIAN_POINT('Ctrl Pts',(3.46386701741464,-2.66749497105505,16.0352971475387));
#67795=CARTESIAN_POINT('Ctrl Pts',(4.11658013628737,1.47230163908801,16.2341833975387));
#67796=CARTESIAN_POINT('Ctrl Pts',(0.986528165660311,4.25918610925795,16.4330696475388));
#67797=CARTESIAN_POINT('Ctrl Pts',(-3.05005402697614,3.13226348946949,16.6319558975387));
#67798=CARTESIAN_POINT('Ctrl Pts',(-4.28391223213811,-0.872926183748866,
16.8308421475388));
#67799=CARTESIAN_POINT('Ctrl Pts',(-1.58124227515725,-4.07597558900841,
17.0297283975387));
#67800=CARTESIAN_POINT('Ctrl Pts',(2.57444642030993,-3.53357181388611,17.2286146475388));
#67801=CARTESIAN_POINT('Ctrl Pts',(4.3644515335017,0.255865094633145,17.4275008975387));
#67802=CARTESIAN_POINT('Ctrl Pts',(2.14392014572458,3.81018510622428,17.6263871475388));
#67803=CARTESIAN_POINT('Ctrl Pts',(-2.04668008886878,3.86328936901768,17.8252733975387));
#67804=CARTESIAN_POINT('Ctrl Pts',(-4.3565663003581,0.366379865059645,18.0241596475388));
#67805=CARTESIAN_POINT('Ctrl Pts',(-2.66316182747159,-3.46719962154403,
18.2230458975387));
#67806=CARTESIAN_POINT('Ctrl Pts',(1.47744766878984,-4.11473602080673,18.4219321475387));
#67807=CARTESIAN_POINT('Ctrl Pts',(4.26041628887939,-0.98120190602555,18.6208183975388));
#67808=CARTESIAN_POINT('Ctrl Pts',(3.12844739512184,3.05396807954705,18.8197046475387));
#67809=CARTESIAN_POINT('Ctrl Pts',(-0.878281906258018,4.28281741708385,
19.0185908975388));
#67810=CARTESIAN_POINT('Ctrl Pts',(-4.07794951474237,1.57614462856346,19.2174771475387));
#67811=CARTESIAN_POINT('Ctrl Pts',(-3.53035008349838,-2.57886262194789,
19.4163633975388));
#67812=CARTESIAN_POINT('Ctrl Pts',(0.261322002095605,-4.36412820001402,
19.6152496475387));
#67813=CARTESIAN_POINT('Ctrl Pts',(3.81286278599776,-2.13915439136365,19.8141358975387));
#67814=CARTESIAN_POINT('Ctrl Pts',(3.86072727539858,2.05150896657326,20.0130221475387));
#67815=CARTESIAN_POINT('Ctrl Pts',(0.360932330522345,4.35702099922879,20.2119083975387));
#67816=CARTESIAN_POINT('Ctrl Pts',(-3.4705268051069,2.65882452034193,20.4107946475388));
#67817=CARTESIAN_POINT('Ctrl Pts',(-4.11288547241112,-1.48259138867275,
20.6096808975387));
#67818=CARTESIAN_POINT('Ctrl Pts',(-0.975874112394784,-4.26163980783156,
20.8085671475387));
#67819=CARTESIAN_POINT('Ctrl Pts',(3.05787735759126,-3.12462640980767,21.0074533975388));
#67820=CARTESIAN_POINT('Ctrl Pts',(4.28171590633873,0.883636255674747,21.2063396475387));
#67821=CARTESIAN_POINT('Ctrl Pts',(1.57104451784945,4.07991706507279,21.4052258975388));
#67822=CARTESIAN_POINT('Ctrl Pts',(-2.58327479183168,3.52712283381567,21.6041121475387));
#67823=CARTESIAN_POINT('Ctrl Pts',(-4.3637980437155,-0.266778501011266,
21.8029983975388));
#67824=CARTESIAN_POINT('Ctrl Pts',(-2.13438529268163,-3.81553450480025,
22.0018846475387));
#67825=CARTESIAN_POINT('Ctrl Pts',(2.05633463698022,-3.85815914597783,22.2007708975388));
#67826=CARTESIAN_POINT('Ctrl Pts',(4.3574688863999,-0.355484231708993,22.3996571475387));
#67827=CARTESIAN_POINT('Ctrl Pts',(2.65448305644691,3.47384856290156,22.5985433975388));
#67828=CARTESIAN_POINT('Ctrl Pts',(-1.48773279069503,4.11102849399365,22.7974296475387));
#67829=CARTESIAN_POINT('Ctrl Pts',(-4.26285666420163,0.970544793097504,
22.9963158975388));
#67830=CARTESIAN_POINT('Ctrl Pts',(-3.12080053950068,-3.06178185499708,
23.1952021475388));
#67831=CARTESIAN_POINT('Ctrl Pts',(0.888989223628163,-4.28060770162484,
23.3940883975387));
#67832=CARTESIAN_POINT('Ctrl Pts',(4.08187823692364,-1.56594195098862,23.5929746475388));
#67833=CARTESIAN_POINT('Ctrl Pts',(3.52389006988343,2.58768292306338,23.7918608975387));
#67834=CARTESIAN_POINT('Ctrl Pts',(-0.272234582849482,4.36346106512225,
23.9907471475388));
#67835=CARTESIAN_POINT('Ctrl Pts',(-3.81820025845479,2.12961285713456,24.1896333975387));
#67836=CARTESIAN_POINT('Ctrl Pts',(-3.85558498477047,-2.06115709254521,
24.3885196475388));
#67837=CARTESIAN_POINT('Ctrl Pts',(-0.350035577137102,-4.3579099611712,
24.5874058975388));
#67838=CARTESIAN_POINT('Ctrl Pts',(3.47716488973482,-2.65013744257396,24.7862921475387));
#67839=CARTESIAN_POINT('Ctrl Pts',(4.1091650884575,1.49287186681883,24.9851783975387));
#67840=CARTESIAN_POINT('Ctrl Pts',(0.965213956465368,4.2640668560872,25.1840646475388));
#67841=CARTESIAN_POINT('Ctrl Pts',(-3.06568156566023,3.11696979018211,25.3829508975388));
#67842=CARTESIAN_POINT('Ctrl Pts',(-4.27949280467476,-0.894340801749458,
25.5818371475387));
#67843=CARTESIAN_POINT('Ctrl Pts',(-1.56083693595826,-4.08383302722886,
25.7807233975388));
#67844=CARTESIAN_POINT('Ctrl Pts',(2.59208700875147,-3.52065179675568,25.9796096475387));
#67845=CARTESIAN_POINT('Ctrl Pts',(4.36311726476112,0.277690239080396,26.1784958975388));
#67846=CARTESIAN_POINT('Ctrl Pts',(2.12483709218347,3.82086004279379,26.3773821475388));
#67847=CARTESIAN_POINT('Ctrl Pts',(-2.06597632572891,3.85300479580088,26.5762683975387));
#67848=CARTESIAN_POINT('Ctrl Pts',(-4.35834422285313,0.344586375324983,
26.7751546475387));
#67849=CARTESIAN_POINT('Ctrl Pts',(-2.64578768551692,-3.48047578042199,
26.9740408975387));
#67850=CARTESIAN_POINT('Ctrl Pts',(1.49800860900966,-4.10729525871589,27.1729271475388));
#67851=CARTESIAN_POINT('Ctrl Pts',(4.26527038159624,-0.959881610832656,
27.3718133975387));
#67852=CARTESIAN_POINT('Ctrl Pts',(3.11313416784098,3.06957648348399,27.5706996475387));
#67853=CARTESIAN_POINT('Ctrl Pts',(-0.899690981672145,4.27837121723149,
27.7695858975388));
#67854=CARTESIAN_POINT('Ctrl Pts',(-4.08578143293244,1.55572948073937,27.9684721475387));
#67855=CARTESIAN_POINT('Ctrl Pts',(-3.517408019495,-2.59648704201063,28.1673583975388));
#67856=CARTESIAN_POINT('Ctrl Pts',(0.283145461174642,-4.36276664316957,
28.3662446475387));
#67857=CARTESIAN_POINT('Ctrl Pts',(3.82351385365899,-2.12005800529481,28.5651308975388));
#67858=CARTESIAN_POINT('Ctrl Pts',(3.85041858310289,2.07079232899705,28.7640171475388));
#67859=CARTESIAN_POINT('Ctrl Pts',(0.339136634791738,4.3587716707668,28.9629033975388));
#67860=CARTESIAN_POINT('Ctrl Pts',(-3.48378122978692,2.64143379207604,29.1617896475387));
#67861=CARTESIAN_POINT('Ctrl Pts',(-4.10541900769204,-1.5031430092369,29.3606758975388));
#67862=CARTESIAN_POINT('Ctrl Pts',(-0.954547764535808,-4.26646723884722,
29.5595621475387));
#67863=CARTESIAN_POINT('Ctrl Pts',(3.07346660237915,-3.10929367847378,29.7584483975388));
#67864=CARTESIAN_POINT('Ctrl Pts',(4.27724294104848,0.905039755031803,29.9573346475388));
#67865=CARTESIAN_POINT('Ctrl Pts',(1.55061959331699,4.08772345098814,30.1562208975387));
#67866=CARTESIAN_POINT('Ctrl Pts',(-2.60088301596186,3.51415874317283,30.3551071475388));
#67867=CARTESIAN_POINT('Ctrl Pts',(-4.36240920089582,-0.288600240603635,
30.5539933975387));
#67868=CARTESIAN_POINT('Ctrl Pts',(-2.11527560394003,-3.82616168690154,
30.7528796475387));
#67869=CARTESIAN_POINT('Ctrl Pts',(2.07560509482036,-3.84782635071967,30.9517658975388));
#67870=CARTESIAN_POINT('Ctrl Pts',(4.35919230424386,-0.333686364057531,
31.1506521475388));
#67871=CARTESIAN_POINT('Ctrl Pts',(2.63707576905832,3.48708123266181,31.3495383975388));
#67872=CARTESIAN_POINT('Ctrl Pts',(-1.50827505947353,4.10353633831938,31.5484246475388));
#67873=CARTESIAN_POINT('Ctrl Pts',(-4.26765742596897,0.949212425913485,
31.7473108975388));
#67874=CARTESIAN_POINT('Ctrl Pts',(-3.10544832808469,-3.07735191626373,
31.9461971475387));
#67875=CARTESIAN_POINT('Ctrl Pts',(0.91038711346635,-4.27610797789004,32.1450833975388));
#67876=CARTESIAN_POINT('Ctrl Pts',(4.08965907835965,-1.54550728167909,32.3439696475388));
#67877=CARTESIAN_POINT('Ctrl Pts',(3.51090397286941,2.60527492373118,32.5428558975387));
#67878=CARTESIAN_POINT('Ctrl Pts',(-0.29405456884035,4.36204493850143,32.7417421475388));
#67879=CARTESIAN_POINT('Ctrl Pts',(-3.82880353838003,2.11048989559061,32.9406283975388));
#67880=CARTESIAN_POINT('Ctrl Pts',(-3.84522810270724,-2.08041461566436,
33.1395146475387));
#67881=CARTESIAN_POINT('Ctrl Pts',(-0.328235571637042,-4.35960612264627,
33.3384008975388));
#67882=CARTESIAN_POINT('Ctrl Pts',(3.49037578387586,-2.6327136232396,33.5372871475387));
#67883=CARTESIAN_POINT('Ctrl Pts',(4.10164725356363,1.51340475162492,33.7361733975388));
#67884=CARTESIAN_POINT('Ctrl Pts',(0.943875603264011,4.26884094123703,33.9350596475387));
#67885=CARTESIAN_POINT('Ctrl Pts',(-3.0812324189812,3.10159812242476,34.1339458975388));
#67886=CARTESIAN_POINT('Ctrl Pts',(-4.27496632968791,-0.915733048116786,
34.3328321475387));
#67887=CARTESIAN_POINT('Ctrl Pts',(-1.54039255351717,-4.0915883129756,34.5317183975388));
#67888=CARTESIAN_POINT('Ctrl Pts',(2.60966275787677,-3.50764371184675,34.7306046475388));
#67889=CARTESIAN_POINT('Ctrl Pts',(4.36167385765697,0.299508433863526,34.9294908975388));
#67890=CARTESIAN_POINT('Ctrl Pts',(2.10570088562199,3.83143941064858,35.1283771475388));
#67891=CARTESIAN_POINT('Ctrl Pts',(-2.08522087998014,3.8426238303401,35.3272633975388));
#67892=CARTESIAN_POINT('Ctrl Pts',(-4.36001313303645,0.322784290515226,
35.5261496475388));
#67893=CARTESIAN_POINT('Ctrl Pts',(-2.628347346691,-3.49366492507817,35.7250358975388));
#67894=CARTESIAN_POINT('Ctrl Pts',(1.51853204945604,-4.09975166684699,35.9239221475388));
#67895=CARTESIAN_POINT('Ctrl Pts',(4.27001783677883,-0.938537476210095,
36.1228083975388));
#67896=CARTESIAN_POINT('Ctrl Pts',(3.09774296425047,3.08510843213345,36.3216946475388));
#67897=CARTESIAN_POINT('Ctrl Pts',(-0.921077353076951,4.27381737137538,
36.5205808975388));
#67898=CARTESIAN_POINT('Ctrl Pts',(-4.09351152974297,1.53527661603589,36.7194671475388));
#67899=CARTESIAN_POINT('Ctrl Pts',(-3.50437724220988,-2.61404880570331,
36.9183533975387));
#67900=CARTESIAN_POINT('Ctrl Pts',(0.304960444014917,-4.36129157005399,
37.1172396475388));
#67901=CARTESIAN_POINT('Ctrl Pts',(3.83407194560894,-2.10091697775549,37.3161258975387));
#67902=CARTESIAN_POINT('Ctrl Pts',(3.84000847567348,2.09003994280635,37.5150121475388));
#67903=CARTESIAN_POINT('Ctrl Pts',(0.31734221318727,4.36038260604223,37.7138983975388));
#67904=CARTESIAN_POINT('Ctrl Pts',(-3.49696717721569,2.62403573243536,37.9127846475388));
#67905=CARTESIAN_POINT('Ctrl Pts',(-4.09781413941906,-1.52376940766611,
38.1116708975388));
#67906=CARTESIAN_POINT('Ctrl Pts',(-0.933265856159647,-4.27097295467856,
38.3105571475387));
#67907=CARTESIAN_POINT('Ctrl Pts',(3.08910966785189,-3.09429453424015,38.5094433975388));
#67908=CARTESIAN_POINT('Ctrl Pts',(4.27241288751803,0.927208179448248,38.7083296475388));
#67909=CARTESIAN_POINT('Ctrl Pts',(1.53063485040313,4.09391556409043,38.9072158975388));
#67910=CARTESIAN_POINT('Ctrl Pts',(-2.61934711719507,3.50404733708965,39.1061021475388));
#67911=CARTESIAN_POINT('Ctrl Pts',(-4.35910709167342,-0.316468415429424,
39.3049883975388));
#67912=CARTESIAN_POINT('Ctrl Pts',(-2.85308220258183,-2.65317527854529,
39.4375792308721));
#67913=CARTESIAN_POINT('Ctrl Pts',(-1.7721534639367,-3.24372257795841,39.5038746475388));
#67914=CARTESIAN_POINT('Ctrl Pts',(2.0090772186955,-2.81633609132837,-0.136687676230644));
#67915=CARTESIAN_POINT('Ctrl Pts',(2.94758491953483,-2.14683700450694,-0.070392259563977));
#67916=CARTESIAN_POINT('Ctrl Pts',(4.08609293119346,0.192777765232804,0.0621985737693567));
#67917=CARTESIAN_POINT('Ctrl Pts',(2.04269690202567,3.54872309047107,0.261084823769356));
#67918=CARTESIAN_POINT('Ctrl Pts',(-1.87959970053929,3.63336178935976,0.459971073769358));
#67919=CARTESIAN_POINT('Ctrl Pts',(-4.07374364010612,0.384441434745174,
0.658857323769356));
#67920=CARTESIAN_POINT('Ctrl Pts',(-2.52499323873643,-3.22042266815715,
0.857743573769359));
#67921=CARTESIAN_POINT('Ctrl Pts',(1.34426329021304,-3.86461315715718,1.05662982376936));
#67922=CARTESIAN_POINT('Ctrl Pts',(3.97812453353371,-0.958302950108288,
1.25551607376936));
#67923=CARTESIAN_POINT('Ctrl Pts',(2.95652143571546,2.82898235111471,1.45440232376936));
#67924=CARTESIAN_POINT('Ctrl Pts',(-0.781895581985945,4.01648924816669,
1.65328857376936));
#67925=CARTESIAN_POINT('Ctrl Pts',(-3.80180140043137,1.51330971689742,1.85217482376936));
#67926=CARTESIAN_POINT('Ctrl Pts',(-3.3282057019711,-2.38051912920303,2.05106107376936));
#67927=CARTESIAN_POINT('Ctrl Pts',(0.203715651461493,-4.08683758028472,
2.24994732376936));
#67928=CARTESIAN_POINT('Ctrl Pts',(3.54843790115571,-2.03773654256675,2.44883357376936));
#67929=CARTESIAN_POINT('Ctrl Pts',(3.63246790710264,1.88386798553642,2.64771982376936));
#67930=CARTESIAN_POINT('Ctrl Pts',(0.378587434436055,4.07436403283702,2.84660607376937));
#67931=CARTESIAN_POINT('Ctrl Pts',(-3.22318026935398,2.52088989946966,3.04549232376936));
#67932=CARTESIAN_POINT('Ctrl Pts',(-3.86313682746238,-1.34905532485943,
3.24437857376936));
#67933=CARTESIAN_POINT('Ctrl Pts',(-0.953219680208054,-3.97934005231632,
3.44326482376936));
#67934=CARTESIAN_POINT('Ctrl Pts',(2.83262014357182,-2.95297122725163,3.64215107376936));
#67935=CARTESIAN_POINT('Ctrl Pts',(4.01553809728831,0.786911425333983,3.84103732376936));
#67936=CARTESIAN_POINT('Ctrl Pts',(1.50853944740008,3.80369351600713,4.03992357376936));
#67937=CARTESIAN_POINT('Ctrl Pts',(-2.38467060488288,3.32522508593738,4.23880982376937));
#67938=CARTESIAN_POINT('Ctrl Pts',(-4.0865839016778,-0.208824687545051,
4.43769607376936));
#67939=CARTESIAN_POINT('Ctrl Pts',(-2.0332959352706,-3.55098343486414,4.63658232376937));
#67940=CARTESIAN_POINT('Ctrl Pts',(1.88840722556278,-3.63010934895867,4.83546857376936));
#67941=CARTESIAN_POINT('Ctrl Pts',(4.07483482061434,-0.373492856732322,
5.03435482376936));
#67942=CARTESIAN_POINT('Ctrl Pts',(2.51685749801378,3.22632981292407,5.23324107376936));
#67943=CARTESIAN_POINT('Ctrl Pts',(-1.35388439197982,3.86144698047705,5.43212732376937));
#67944=CARTESIAN_POINT('Ctrl Pts',(-3.9805288896519,0.948243369370376,5.63101357376936));
#67945=CARTESIAN_POINT('Ctrl Pts',(-2.94942709714979,-2.83631019588636,
5.82989982376937));
#67946=CARTESIAN_POINT('Ctrl Pts',(0.791931628935568,-4.01455103643869,
6.02878607376936));
#67947=CARTESIAN_POINT('Ctrl Pts',(3.80557676267527,-1.50378230881505,6.22767232376937));
#67948=CARTESIAN_POINT('Ctrl Pts',(3.32224079883099,2.38882644900927,6.42655857376937));
#67949=CARTESIAN_POINT('Ctrl Pts',(-0.213934195629035,4.08631960190299,
6.62544482376937));
#67950=CARTESIAN_POINT('Ctrl Pts',(-3.55352299964065,2.02885436144528,6.82433107376937));
#67951=CARTESIAN_POINT('Ctrl Pts',(-3.62774533373042,-1.89294466969528,
7.02321732376936));
#67952=CARTESIAN_POINT('Ctrl Pts',(-0.368397581072059,-4.07529863337619,
7.22210357376937));
#67953=CARTESIAN_POINT('Ctrl Pts',(3.22947425288682,-2.51282147771678,7.42098982376937));
#67954=CARTESIAN_POINT('Ctrl Pts',(3.85975112772587,1.35871150762509,7.61987607376937));
#67955=CARTESIAN_POINT('Ctrl Pts',(0.943265559775128,3.98171141755363,7.81876232376937));
#67956=CARTESIAN_POINT('Ctrl Pts',(-2.83999580544285,2.94587840108877,8.01764857376936));
#67957=CARTESIAN_POINT('Ctrl Pts',(-4.01355770375238,-0.796950618033701,
8.21653482376938));
#67958=CARTESIAN_POINT('Ctrl Pts',(-1.49902281691347,-3.80745404743213,
8.41542107376936));
#67959=CARTESIAN_POINT('Ctrl Pts',(2.39297855726508,-3.3192513242302,8.61430732376938));
#67960=CARTESIAN_POINT('Ctrl Pts',(4.08604891427468,0.219043372620942,8.81319357376936));
#67961=CARTESIAN_POINT('Ctrl Pts',(2.02440961540798,3.55605700713278,9.01207982376937));
#67962=CARTESIAN_POINT('Ctrl Pts',(-1.89747915425351,3.62537564786158,9.21096607376936));
#67963=CARTESIAN_POINT('Ctrl Pts',(-4.07575607496965,0.363301728983464,
9.40985232376938));
#67964=CARTESIAN_POINT('Ctrl Pts',(-2.50878152886593,-3.23261364368766,
9.60873857376937));
#67965=CARTESIAN_POINT('Ctrl Pts',(1.36353649905687,-3.85804924083067,9.80762482376936));
#67966=CARTESIAN_POINT('Ctrl Pts',(3.98288772052199,-0.938286275424292,
10.0065110737694));
#67967=CARTESIAN_POINT('Ctrl Pts',(2.94232509947999,2.84367697495768,10.2053973237694));
#67968=CARTESIAN_POINT('Ctrl Pts',(-0.80196836118798,4.01255809635049,10.4042835737694));
#67969=CARTESIAN_POINT('Ctrl Pts',(-3.80932537967576,1.49426098145287,10.6031698237694));
#67970=CARTESIAN_POINT('Ctrl Pts',(-3.316256660362,-2.3971269243699,10.8020560737694));
#67971=CARTESIAN_POINT('Ctrl Pts',(0.224152207163268,-4.08577183858305,
11.0009423237694));
#67972=CARTESIAN_POINT('Ctrl Pts',(3.55858545514036,-2.01996170443845,11.1998285737694));
#67973=CARTESIAN_POINT('Ctrl Pts',(3.6230002941361,1.90201067232131,11.3987148237694));
#67974=CARTESIAN_POINT('Ctrl Pts',(0.358205308914588,4.07620714458917,11.5976010737694));
#67975=CARTESIAN_POINT('Ctrl Pts',(-3.23574798067012,2.50473765782441,11.7964873237694));
#67976=CARTESIAN_POINT('Ctrl Pts',(-3.85634132232064,-1.36835935875657,
11.9953735737694));
#67977=CARTESIAN_POINT('Ctrl Pts',(-0.93330552417114,-3.98405779670502,
12.1942598237694));
#67978=CARTESIAN_POINT('Ctrl Pts',(2.84735369871167,-2.93876719788543,12.3931460737694));
#67979=CARTESIAN_POINT('Ctrl Pts',(4.01155221577702,0.80698485055723,12.5920323237694));
#67980=CARTESIAN_POINT('Ctrl Pts',(1.48949680988765,3.81119075647874,12.7909185737694));
#67981=CARTESIAN_POINT('Ctrl Pts',(-2.40127154384339,3.31325681190915,12.9898048237694));
#67982=CARTESIAN_POINT('Ctrl Pts',(-4.08548837525859,-0.229260691269513,
13.1886910737694));
#67983=CARTESIAN_POINT('Ctrl Pts',(-2.01551063549186,-3.56110833971021,
13.3875773237694));
#67984=CARTESIAN_POINT('Ctrl Pts',(1.9065392168149,-3.6206192762677,13.5864635737694));
#67985=CARTESIAN_POINT('Ctrl Pts',(4.07665184152917,-0.353108328833043,
13.7853498237694));
#67986=CARTESIAN_POINT('Ctrl Pts',(2.50068987091457,3.23887725893398,13.9842360737694));
#67987=CARTESIAN_POINT('Ctrl Pts',(-1.37318007918433,3.85462737486591,14.1831223237694));
#67988=CARTESIAN_POINT('Ctrl Pts',(-3.9852216442734,0.928323313802475,14.3820085737694));
#67989=CARTESIAN_POINT('Ctrl Pts',(-2.93520470186743,-2.85102597095673,
14.5808948237694));
#67990=CARTESIAN_POINT('Ctrl Pts',(0.812000078298801,-4.01054006360455,
14.7797810737693));
#67991=CARTESIAN_POINT('Ctrl Pts',(3.81305017492473,-1.48473030966602,14.9786673237694));
#67992=CARTESIAN_POINT('Ctrl Pts',(3.31025178356159,2.4054124092059,15.1775535737694));
#67993=CARTESIAN_POINT('Ctrl Pts',(-0.234368816953125,4.08519852474447,
15.3764398237694));
#67994=CARTESIAN_POINT('Ctrl Pts',(-3.56362565689806,2.01105641552697,15.5753260737694));
#67995=CARTESIAN_POINT('Ctrl Pts',(-3.61823259797885,-1.9110647806544,15.7742123237694));
#67996=CARTESIAN_POINT('Ctrl Pts',(-0.348010796707407,-4.0770901650944,
15.9730985737694));
#67997=CARTESIAN_POINT('Ctrl Pts',(3.24200147358696,-2.49663817446469,16.1719848237694));
#67998=CARTESIAN_POINT('Ctrl Pts',(3.85290740114609,1.37799865280346,16.3708710737694));
#67999=CARTESIAN_POINT('Ctrl Pts',(0.923339652107423,3.9863792614076,16.5697573237694));
#68000=CARTESIAN_POINT('Ctrl Pts',(-2.85469378595166,2.93163761699557,16.7686435737694));
#68001=CARTESIAN_POINT('Ctrl Pts',(-4.00952164141544,-0.817014036571931,
16.9675298237694));
#68002=CARTESIAN_POINT('Ctrl Pts',(-1.47996148823989,-3.81490363210673,
17.1664160737694));
#68003=CARTESIAN_POINT('Ctrl Pts',(2.40954951398363,-3.30724158001736,17.3653023237694));
#68004=CARTESIAN_POINT('Ctrl Pts',(4.08490228749385,0.239476576228112,17.5641885737694));
#68005=CARTESIAN_POINT('Ctrl Pts',(2.00659905150743,3.56613740276842,17.7630748237694));
#68006=CARTESIAN_POINT('Ctrl Pts',(-1.91558735676465,3.61584026300082,17.9619610737694));
#68007=CARTESIAN_POINT('Ctrl Pts',(-4.07752211459962,0.342912720507015,
18.1608473237694));
#68008=CARTESIAN_POINT('Ctrl Pts',(-2.4925825748091,-3.24512061974472,18.3597335737694));
#68009=CARTESIAN_POINT('Ctrl Pts',(1.38281507208069,-3.85118140385011,18.5586198237694));
#68010=CARTESIAN_POINT('Ctrl Pts',(3.98753064629779,-0.918354546877404,
18.7575060737694));
#68011=CARTESIAN_POINT('Ctrl Pts',(2.92806594884658,2.85835713796223,18.9563923237694));
#68012=CARTESIAN_POINT('Ctrl Pts',(-0.822026717537881,4.00849695080192,
19.1552785737694));
#68013=CARTESIAN_POINT('Ctrl Pts',(-3.81675112512713,1.47519035306472,19.3541648237694));
#68014=CARTESIAN_POINT('Ctrl Pts',(-3.30422620598249,-2.41368285170877,
19.5530510737694));
#68015=CARTESIAN_POINT('Ctrl Pts',(0.244583961109105,-4.08459966396984,
19.7519373237694));
#68016=CARTESIAN_POINT('Ctrl Pts',(3.56864357339442,-2.00213855040182,19.9508235737694));
#68017=CARTESIAN_POINT('Ctrl Pts',(3.61344227507378,1.92010693807507,20.1497098237694));
#68018=CARTESIAN_POINT('Ctrl Pts',(0.33781410820217,4.07794768936949,20.3485960737694));
#68019=CARTESIAN_POINT('Ctrl Pts',(-3.24823469253086,2.48852307828828,20.5474823237694));
#68020=CARTESIAN_POINT('Ctrl Pts',(-3.84944938567638,-1.38762932948615,
20.7463685737694));
#68021=CARTESIAN_POINT('Ctrl Pts',(-0.913368005905981,-3.98867579714393,
20.9452548237694));
#68022=CARTESIAN_POINT('Ctrl Pts',(2.86201602126123,-2.92448970300433,21.1441410737694));
#68023=CARTESIAN_POINT('Ctrl Pts',(4.00746599336594,0.827038113359913,21.3430273237694));
#68024=CARTESIAN_POINT('Ctrl Pts',(1.4704169115997,3.81859265109753,21.5419135737694));
#68025=CARTESIAN_POINT('Ctrl Pts',(-2.41781241591925,3.30120566617125,21.7407998237694));
#68026=CARTESIAN_POINT('Ctrl Pts',(-4.08429065464559,-0.249690963611301,
21.9396860737694));
#68027=CARTESIAN_POINT('Ctrl Pts',(-1.99767491918358,-3.57114416485799,
22.1385723237693));
#68028=CARTESIAN_POINT('Ctrl Pts',(1.92462351751989,-3.61103863794668,22.3374585737694));
#68029=CARTESIAN_POINT('Ctrl Pts',(4.0783668887387,-0.332714967763942,22.5363448237694));
#68030=CARTESIAN_POINT('Ctrl Pts',(2.48445969124877,3.25134368707685,22.7352310737694));
#68031=CARTESIAN_POINT('Ctrl Pts',(-1.39244141749321,3.84771134933273,22.9341173237694));
#68032=CARTESIAN_POINT('Ctrl Pts',(-3.9898147121557,0.908380036989118,23.1330035737694));
#68033=CARTESIAN_POINT('Ctrl Pts',(-2.92090888505992,-2.86567043012844,
23.3318898237694));
#68034=CARTESIAN_POINT('Ctrl Pts',(0.83204821620329,-4.00642877071929,23.5307760737694));
#68035=CARTESIAN_POINT('Ctrl Pts',(3.82042820713893,-1.46564117130749,23.7296623237694));
#68036=CARTESIAN_POINT('Ctrl Pts',(3.29817996530588,2.42193820015896,23.9285485737694));
#68037=CARTESIAN_POINT('Ctrl Pts',(-0.254797575750441,4.08397526000418,
24.1274348237694));
#68038=CARTESIAN_POINT('Ctrl Pts',(-3.57363917324971,1.99320816483117,24.3263210737694));
#68039=CARTESIAN_POINT('Ctrl Pts',(-3.60862935537735,-1.92913708803787,
24.5252073237694));
#68040=CARTESIAN_POINT('Ctrl Pts',(-0.327615307164295,-4.07877971205188,
24.7240935737694));
#68041=CARTESIAN_POINT('Ctrl Pts',(3.25444759852215,-2.48039242004323,24.9229798237694));
#68042=CARTESIAN_POINT('Ctrl Pts',(3.84596729753637,1.39725132857884,25.1218660737694));
#68043=CARTESIAN_POINT('Ctrl Pts',(0.903390647924833,3.99094738955255,25.3207523237694));
#68044=CARTESIAN_POINT('Ctrl Pts',(-2.86932035885057,2.91732350061147,25.5196385737694));
#68045=CARTESIAN_POINT('Ctrl Pts',(-4.00538528448356,-0.837057018235249,
25.7185248237694));
#68046=CARTESIAN_POINT('Ctrl Pts',(-1.46086313965446,-3.82225779038165,
25.9174110737694));
#68047=CARTESIAN_POINT('Ctrl Pts',(2.42606019797783,-3.29514910811671,26.1162973237694));
#68048=CARTESIAN_POINT('Ctrl Pts',(4.08365348053868,0.259903789543027,26.3151835737694));
#68049=CARTESIAN_POINT('Ctrl Pts',(1.98873829432774,3.57612859466892,26.5140698237694));
#68050=CARTESIAN_POINT('Ctrl Pts',(-1.9336476425726,3.60621443113243,26.7129560737694));
#68051=CARTESIAN_POINT('Ctrl Pts',(-4.07918615866362,0.322515134375918,
26.9118423237694));
#68052=CARTESIAN_POINT('Ctrl Pts',(-2.47632127103036,-3.25754642201413,
27.1107285737694));
#68053=CARTESIAN_POINT('Ctrl Pts',(1.40205905522319,-3.84421723301392,27.3096148237694));
#68054=CARTESIAN_POINT('Ctrl Pts',(3.99207382756366,-0.898399846513567,
27.5085010737694));
#68055=CARTESIAN_POINT('Ctrl Pts',(2.91373355526439,2.87296580172139,27.7073873237694));
#68056=CARTESIAN_POINT('Ctrl Pts',(-0.842064511625181,4.00433553629013,
27.9062735737694));
#68057=CARTESIAN_POINT('Ctrl Pts',(-3.82408139796542,1.4560828241104,28.1051598237694));
#68058=CARTESIAN_POINT('Ctrl Pts',(-3.29211309934206,-2.43017840293152,
28.3040460737694));
#68059=CARTESIAN_POINT('Ctrl Pts',(0.265009597006007,-4.08332531675215,
28.5029323237694));
#68060=CARTESIAN_POINT('Ctrl Pts',(3.57861242522373,-1.98426531466151,28.7018185737694));
#68061=CARTESIAN_POINT('Ctrl Pts',(3.60379386898736,1.9381551740724,28.9007048237694));
#68062=CARTESIAN_POINT('Ctrl Pts',(0.317414457372265,4.07958622793851,29.0995910737694));
#68063=CARTESIAN_POINT('Ctrl Pts',(-3.26064015270821,2.47224625057484,29.2984773237694));
#68064=CARTESIAN_POINT('Ctrl Pts',(-3.84246115850137,-1.40686458991001,
29.4973635737694));
#68065=CARTESIAN_POINT('Ctrl Pts',(-0.893407640557818,-3.99319402442797,
29.6962498237694));
#68066=CARTESIAN_POINT('Ctrl Pts',(2.87660675304174,-2.9101390546311,29.8951360737694));
#68067=CARTESIAN_POINT('Ctrl Pts',(4.00327952778012,0.847070688544426,30.0940223237694));
#68068=CARTESIAN_POINT('Ctrl Pts',(1.45130023214889,3.82589902703912,30.2929085737694));
#68069=CARTESIAN_POINT('Ctrl Pts',(-2.43429280858163,3.28907194372852,30.4917948237694));
#68070=CARTESIAN_POINT('Ctrl Pts',(-4.08299076915769,-0.270114990157072,
30.6906810737694));
#68071=CARTESIAN_POINT('Ctrl Pts',(-1.97978923282535,-3.58109066103098,
30.8895673237694));
#68072=CARTESIAN_POINT('Ctrl Pts',(1.94265967549026,-3.60136767272636,31.0884535737694));
#68073=CARTESIAN_POINT('Ctrl Pts',(4.07997991925103,-0.312313284127758,
31.2873398237694));
#68074=CARTESIAN_POINT('Ctrl Pts',(2.46816736504766,3.26372878576757,31.4862260737694));
#68075=CARTESIAN_POINT('Ctrl Pts',(-1.41166792512641,3.84069907674427,31.6851123237694));
#68076=CARTESIAN_POINT('Ctrl Pts',(-3.9943079783942,0.888414037862129,31.8839985737694));
#68077=CARTESIAN_POINT('Ctrl Pts',(-2.90654000433118,-2.88024320711916,
32.0828848237694));
#68078=CARTESIAN_POINT('Ctrl Pts',(0.852075541166488,-4.00221726060484,
32.2817710737694));
#68079=CARTESIAN_POINT('Ctrl Pts',(3.82771067476094,-1.44651537124626,32.4806573237694));
#68080=CARTESIAN_POINT('Ctrl Pts',(3.28602564603094,2.43840340849451,32.6795435737694));
#68081=CARTESIAN_POINT('Ctrl Pts',(-0.275219961015347,4.08264983828088,
32.8784298237694));
#68082=CARTESIAN_POINT('Ctrl Pts',(-3.58356329821457,1.97531005581222,33.0773160737694));
#68083=CARTESIAN_POINT('Ctrl Pts',(-3.59893584614564,-1.94716113977428,
33.2762023237694));
#68084=CARTESIAN_POINT('Ctrl Pts',(-0.307211622611714,-4.08036723200399,
33.4750885737694));
#68085=CARTESIAN_POINT('Ctrl Pts',(3.26681231635263,-2.46408462079069,33.6739748237694));
#68086=CARTESIAN_POINT('Ctrl Pts',(3.83893099051835,1.41646905329624,33.8728610737694));
#68087=CARTESIAN_POINT('Ctrl Pts',(0.883419046193318,3.99541568784834,34.0717473237694));
#68088=CARTESIAN_POINT('Ctrl Pts',(-2.88387515819149,2.90293640974734,34.2706335737694));
#68089=CARTESIAN_POINT('Ctrl Pts',(-4.00114873657231,-0.857079061199814,
34.4695198237694));
#68090=CARTESIAN_POINT('Ctrl Pts',(-1.44172824860138,-3.82951633919216,
34.6684060737694));
#68091=CARTESIAN_POINT('Ctrl Pts',(2.44251019570497,-3.28297420930239,34.8672923237694));
#68092=CARTESIAN_POINT('Ctrl Pts',(4.08230252568531,0.280324498329562,35.0661785737694));
#68093=CARTESIAN_POINT('Ctrl Pts',(1.97082778865322,3.58603033916501,35.2650648237694));
#68094=CARTESIAN_POINT('Ctrl Pts',(-1.95165955611527,3.59649838107857,35.4639510737694));
#68095=CARTESIAN_POINT('Ctrl Pts',(-4.08074817280747,0.302109503696352,
35.6628373237694));
#68096=CARTESIAN_POINT('Ctrl Pts',(-2.45999801038286,-3.26989078344478,
35.8617235737694));
#68097=CARTESIAN_POINT('Ctrl Pts',(1.42126794050536,-3.83715681879127,36.0606098237695));
#68098=CARTESIAN_POINT('Ctrl Pts',(3.99651720157898,-0.878422833668996,
36.2594960737694));
#68099=CARTESIAN_POINT('Ctrl Pts',(2.89932817986464,2.88750290726155,36.4583823237694));
#68100=CARTESIAN_POINT('Ctrl Pts',(-0.862081055926817,4.00007337065221,
36.6572685737694));
#68101=CARTESIAN_POINT('Ctrl Pts',(-3.83131637122645,1.43693999409573,36.8561548237694));
#68102=CARTESIAN_POINT('Ctrl Pts',(-3.27991696163009,-2.44661531101263,
37.0550410737694));
#68103=CARTESIAN_POINT('Ctrl Pts',(0.285427299579139,-4.08194472413982,
37.2539273237694));
#68104=CARTESIAN_POINT('Ctrl Pts',(3.58849425656653,-1.96635029679954,37.4528135737694));
#68105=CARTESIAN_POINT('Ctrl Pts',(3.59405054354887,1.95616995120416,37.6516998237694));
#68106=CARTESIAN_POINT('Ctrl Pts',(0.297015999058931,4.08109398054869,37.8505860737695));
#68107=CARTESIAN_POINT('Ctrl Pts',(-3.27298152169835,2.45596256107144,38.0494723237694));
#68108=CARTESIAN_POINT('Ctrl Pts',(-3.83534339271433,-1.42616983857172,
38.2483585737694));
#68109=CARTESIAN_POINT('Ctrl Pts',(-0.873488868281231,-3.99741114283678,
38.4472448237694));
#68110=CARTESIAN_POINT('Ctrl Pts',(2.89124785821669,-2.89610062663618,38.6461310737694));
#68111=CARTESIAN_POINT('Ctrl Pts',(3.99875884595704,0.86781919426473,38.8450173237695));
#68112=CARTESIAN_POINT('Ctrl Pts',(1.43259554006624,3.8316945266069,39.0439035737694));
#68113=CARTESIAN_POINT('Ctrl Pts',(-2.45157425821743,3.27960818739581,39.2427898237695));
#68114=CARTESIAN_POINT('Ctrl Pts',(-4.07990016466532,-0.296198169273691,
39.4416760737694));
#68115=CARTESIAN_POINT('Ctrl Pts',(-2.67033828334988,-2.48323567835706,
39.5742669071028));
#68116=CARTESIAN_POINT('Ctrl Pts',(-1.65864454744381,-3.03595759443951,
39.6405623237694));
#68117=CARTESIAN_POINT('Ctrl Pts',(1.87158653173891,-2.62360084935066,0.));
#68118=CARTESIAN_POINT('Ctrl Pts',(2.74586769747962,-1.99991876175022,0.0662954166666667));
#68119=CARTESIAN_POINT('Ctrl Pts',(3.80646220378775,0.179585068045613,0.19888625));
#68120=CARTESIAN_POINT('Ctrl Pts',(1.90290546061669,3.30586713103499,0.3977725));
#68121=CARTESIAN_POINT('Ctrl Pts',(-1.75096977450869,3.38471360215616,0.596658750000001));
#68122=CARTESIAN_POINT('Ctrl Pts',(-3.79495803328573,0.358132283227411,
0.795545000000001));
#68123=CARTESIAN_POINT('Ctrl Pts',(-2.35219597055587,-3.00003386437442,
0.994431250000001));
#68124=CARTESIAN_POINT('Ctrl Pts',(1.25226897486165,-3.60013934158935,1.1933175));
#68125=CARTESIAN_POINT('Ctrl Pts',(3.70588259587967,-0.892721732175661,
1.39220375));
#68126=CARTESIAN_POINT('Ctrl Pts',(2.75419264545516,2.63538166557444,1.59109));
#68127=CARTESIAN_POINT('Ctrl Pts',(-0.728386757290071,3.7416218310534,1.78997625));
#68128=CARTESIAN_POINT('Ctrl Pts',(-3.54162609141209,1.40974675245884,1.9888625));
#68129=CARTESIAN_POINT('Ctrl Pts',(-3.10044079376427,-2.21760890985371,
2.18774875));
#68130=CARTESIAN_POINT('Ctrl Pts',(0.189774422820439,-3.8071558930084,2.386635));
#68131=CARTESIAN_POINT('Ctrl Pts',(3.30560145857767,-1.89828456209197,2.58552125000001));
#68132=CARTESIAN_POINT('Ctrl Pts',(3.38388089250329,1.75494596051086,2.7844075));
#68133=CARTESIAN_POINT('Ctrl Pts',(0.35267889993612,3.79553596959835,2.98329375));
#68134=CARTESIAN_POINT('Ctrl Pts',(-3.0026027498368,2.34837344226508,3.18218));
#68135=CARTESIAN_POINT('Ctrl Pts',(-3.59876404414062,-1.25673306783944,
3.38106625000001));
#68136=CARTESIAN_POINT('Ctrl Pts',(-0.887986334554333,-3.70701493094446,
3.5799525));
#68137=CARTESIAN_POINT('Ctrl Pts',(2.63877050663273,-2.75088539460193,3.77883875000001));
#68138=CARTESIAN_POINT('Ctrl Pts',(3.74073577194275,0.7330593426781,3.977725));
#68139=CARTESIAN_POINT('Ctrl Pts',(1.40530293513768,3.54338872054109,4.17661125000001));
#68140=CARTESIAN_POINT('Ctrl Pts',(-2.22147628035442,3.09766415542848,4.37549750000001));
#68141=CARTESIAN_POINT('Ctrl Pts',(-3.80691957483225,-0.194533823322909,
4.57438375000001));
#68142=CARTESIAN_POINT('Ctrl Pts',(-1.89414784662335,-3.30797278933611,
4.77327));
#68143=CARTESIAN_POINT('Ctrl Pts',(1.75917455880395,-3.38168374168425,4.97215625000001));
#68144=CARTESIAN_POINT('Ctrl Pts',(3.79597453913422,-0.347932968357942,
5.17104250000001));
#68145=CARTESIAN_POINT('Ctrl Pts',(2.34461699717418,3.0055367551961,5.36992875000001));
#68146=CARTESIAN_POINT('Ctrl Pts',(-1.26123165898331,3.59718984140266,5.56881500000001));
#68147=CARTESIAN_POINT('Ctrl Pts',(-3.70812241050024,0.883350576279402,
5.76770125000001));
#68148=CARTESIAN_POINT('Ctrl Pts',(-2.74758380613951,-2.64220803115844,
5.96658750000001));
#68149=CARTESIAN_POINT('Ctrl Pts',(0.737735989926837,-3.73981626035058,
6.16547375000001));
#68150=CARTESIAN_POINT('Ctrl Pts',(3.5451430877039,-1.4008713501182,6.36436000000001));
#68151=CARTESIAN_POINT('Ctrl Pts',(3.09488409724894,2.22534772034816,6.56324625000001));
#68152=CARTESIAN_POINT('Ctrl Pts',(-0.19929366352457,3.8066733623451,6.76213250000001));
#68153=CARTESIAN_POINT('Ctrl Pts',(-3.31033855964498,1.89001023076976,6.96101875000001));
#68154=CARTESIAN_POINT('Ctrl Pts',(-3.3794815072351,-1.76340148410472,7.15990500000001));
#68155=CARTESIAN_POINT('Ctrl Pts',(-0.343186386587714,-3.79640661098804,
7.35879125000001));
#68156=CARTESIAN_POINT('Ctrl Pts',(3.00846600621214,-2.34085718089664,7.55767750000001));
#68157=CARTESIAN_POINT('Ctrl Pts',(3.5956100439019,1.26572843220077,7.75656375000002));
#68158=CARTESIAN_POINT('Ctrl Pts',(0.878713421813992,3.70922401240668,7.95545000000001));
#68159=CARTESIAN_POINT('Ctrl Pts',(-2.6456414169651,2.74427796418817,8.15433625000002));
#68160=CARTESIAN_POINT('Ctrl Pts',(-3.73889090613327,-0.742411505786354,
8.35322250000001));
#68161=CARTESIAN_POINT('Ctrl Pts',(-1.39643757283078,-3.54689190095731,
8.55210875000002));
#68162=CARTESIAN_POINT('Ctrl Pts',(2.22921568013466,-3.09209920657986,8.75099500000001));
#68163=CARTESIAN_POINT('Ctrl Pts',(3.80642119915558,0.204053195292361,8.94988125000001));
#68164=CARTESIAN_POINT('Ctrl Pts',(1.88586965979368,3.3126991529808,9.14876750000002));
#68165=CARTESIAN_POINT('Ctrl Pts',(-1.76762565236893,3.37727399021419,9.34765375000001));
#68166=CARTESIAN_POINT('Ctrl Pts',(-3.79683274768274,0.338439267836879,
9.54654000000001));
#68167=CARTESIAN_POINT('Ctrl Pts',(-2.33709370491482,-3.01139055360436,
9.74542625000002));
#68168=CARTESIAN_POINT('Ctrl Pts',(1.27022322657475,-3.59402462520223,9.94431250000001));
#68169=CARTESIAN_POINT('Ctrl Pts',(3.71031981538147,-0.874074893517518,
10.14319875));
#68170=CARTESIAN_POINT('Ctrl Pts',(2.74096783186856,2.64907066658324,10.342085));
#68171=CARTESIAN_POINT('Ctrl Pts',(-0.747085860967871,3.73795970660893,
10.54097125));
#68172=CARTESIAN_POINT('Ctrl Pts',(-3.54863516905622,1.39200161236521,10.7398575));
#68173=CARTESIAN_POINT('Ctrl Pts',(-3.08930948176955,-2.23308015479489,
10.93874375));
#68174=CARTESIAN_POINT('Ctrl Pts',(0.208812408046019,-3.80616308506823,
11.13763));
#68175=CARTESIAN_POINT('Ctrl Pts',(3.31505456729397,-1.88172614047672,11.33651625));
#68176=CARTESIAN_POINT('Ctrl Pts',(3.37506119321498,1.77184705715372,11.5354025));
#68177=CARTESIAN_POINT('Ctrl Pts',(0.333691619975345,3.79725294846791,11.73428875));
#68178=CARTESIAN_POINT('Ctrl Pts',(-3.01431039303498,2.33332657515646,11.933175));
#68179=CARTESIAN_POINT('Ctrl Pts',(-3.59243358765975,-1.27471603510118,
12.13206125));
#68180=CARTESIAN_POINT('Ctrl Pts',(-0.869434998705811,-3.71140981769939,
12.3309475));
#68181=CARTESIAN_POINT('Ctrl Pts',(2.65249577468504,-2.73765341436203,12.52983375));
#68182=CARTESIAN_POINT('Ctrl Pts',(3.73702266321591,0.751759048166815,12.72872));
#68183=CARTESIAN_POINT('Ctrl Pts',(1.38756347566574,3.55037288927353,12.92760625));
#68184=CARTESIAN_POINT('Ctrl Pts',(-2.23694113829198,3.08651492718033,13.1264925));
#68185=CARTESIAN_POINT('Ctrl Pts',(-3.80589902048407,-0.2135712943456,13.32537875));
#68186=CARTESIAN_POINT('Ctrl Pts',(-1.87757967929805,-3.31740479890186,
13.524265));
#68187=CARTESIAN_POINT('Ctrl Pts',(1.77606569186011,-3.37284311969702,13.72315125));
#68188=CARTESIAN_POINT('Ctrl Pts',(3.79766721268626,-0.32894345042547,13.9220375));
#68189=CARTESIAN_POINT('Ctrl Pts',(2.32955579751124,3.01722551993911,14.12092375));
#68190=CARTESIAN_POINT('Ctrl Pts',(-1.2792068507562,3.59083693376187,14.31981));
#68191=CARTESIAN_POINT('Ctrl Pts',(-3.71249401765632,0.864793744632787,
14.51869625));
#68192=CARTESIAN_POINT('Ctrl Pts',(-2.73433471685024,-2.65591673591578,
14.7175825));
#68193=CARTESIAN_POINT('Ctrl Pts',(0.756431060077252,-3.73607977741916,
14.91646875));
#68194=CARTESIAN_POINT('Ctrl Pts',(3.55210505889249,-1.38312316967087,15.115355));
#68195=CARTESIAN_POINT('Ctrl Pts',(3.08371554718117,2.24079862458972,15.31424125));
#68196=CARTESIAN_POINT('Ctrl Pts',(-0.21832984675111,3.80562900581595,15.5131275));
#68197=CARTESIAN_POINT('Ctrl Pts',(-3.31974984413011,1.8734302827402,15.71201375));
#68198=CARTESIAN_POINT('Ctrl Pts',(-3.37061977312804,-1.78028154989269,
15.9109));
#68199=CARTESIAN_POINT('Ctrl Pts',(-0.324194766610495,-3.79807553969012,
16.10978625));
#68200=CARTESIAN_POINT('Ctrl Pts',(3.02013592975928,-2.32578137787433,16.3086725));
#68201=CARTESIAN_POINT('Ctrl Pts',(3.58923466600481,1.2836956665189,16.5075587500001));
#68202=CARTESIAN_POINT('Ctrl Pts',(0.86015113855453,3.71357241355724,16.706445));
#68203=CARTESIAN_POINT('Ctrl Pts',(-2.65933354492717,2.73101174452164,16.9053312500001));
#68204=CARTESIAN_POINT('Ctrl Pts',(-3.73513105069278,-0.761101889394991,
17.1042175));
#68205=CARTESIAN_POINT('Ctrl Pts',(-1.37868070132254,-3.55383167520506,
17.30310375));
#68206=CARTESIAN_POINT('Ctrl Pts',(2.24465260765735,-3.08091134614859,17.50199));
#68207=CARTESIAN_POINT('Ctrl Pts',(3.80535304148599,0.223088057823076,17.70087625));
#68208=CARTESIAN_POINT('Ctrl Pts',(1.8692779572903,3.32208969931257,17.8997625000001));
#68209=CARTESIAN_POINT('Ctrl Pts',(-1.78449462466053,3.36839115698396,18.09864875));
#68210=CARTESIAN_POINT('Ctrl Pts',(-3.79847792884113,0.319445575954385,
18.297535));
#68211=CARTESIAN_POINT('Ctrl Pts',(-2.32200332214661,-3.02304161794542,
18.49642125));
#68212=CARTESIAN_POINT('Ctrl Pts',(1.28818247537154,-3.58762678689348,18.6953075));
#68213=CARTESIAN_POINT('Ctrl Pts',(3.71464500371619,-0.855507187729257,
18.89419375));
#68214=CARTESIAN_POINT('Ctrl Pts',(2.72768450257131,2.6627461963774,19.09308));
#68215=CARTESIAN_POINT('Ctrl Pts',(-0.76577152881775,3.73417648452,19.29196625));
#68216=CARTESIAN_POINT('Ctrl Pts',(-3.55555273551189,1.37423607756599,19.4908525));
#68217=CARTESIAN_POINT('Ctrl Pts',(-3.0781023284666,-2.24850308146965,19.68973875));
#68218=CARTESIAN_POINT('Ctrl Pts',(0.227845920122608,-3.80507112792566,
19.8886250000001));
#68219=CARTESIAN_POINT('Ctrl Pts',(3.32442436079109,-1.86512270943999,20.08751125));
#68220=CARTESIAN_POINT('Ctrl Pts',(3.366157274749,1.78870490957689,20.2863975000001));
#68221=CARTESIAN_POINT('Ctrl Pts',(0.314695885881992,3.7988743795102,20.48528375));
#68222=CARTESIAN_POINT('Ctrl Pts',(-3.02594257995482,2.31822163623464,20.6841700000001));
#68223=CARTESIAN_POINT('Ctrl Pts',(-3.58601329894164,-1.29266727029954,
20.88305625));
#68224=CARTESIAN_POINT('Ctrl Pts',(-0.850861899417176,-3.7157117864563,
21.0819425));
#68225=CARTESIAN_POINT('Ctrl Pts',(2.6661546849312,-2.724352996201,21.28082875));
#68226=CARTESIAN_POINT('Ctrl Pts',(3.73321608039316,0.770439971045078,21.479715));
#68227=CARTESIAN_POINT('Ctrl Pts',(1.36978930534994,3.55726823712227,21.67860125));
#68228=CARTESIAN_POINT('Ctrl Pts',(-2.25235004000682,3.07528849852681,21.8774875));
#68229=CARTESIAN_POINT('Ctrl Pts',(-3.80478326557569,-0.232603426211332,
22.07637375));
#68230=CARTESIAN_POINT('Ctrl Pts',(-1.86096454568552,-3.32675382491574,
22.27526));
#68231=CARTESIAN_POINT('Ctrl Pts',(1.79291239805955,-3.36391812991553,22.47414625));
#68232=CARTESIAN_POINT('Ctrl Pts',(3.79926489107751,-0.309945703818892,
22.6730325));
#68233=CARTESIAN_POINT('Ctrl Pts',(2.31443632605062,3.02883881125214,22.87191875));
#68234=CARTESIAN_POINT('Ctrl Pts',(-1.29715004429138,3.58439420467181,23.070805));
#68235=CARTESIAN_POINT('Ctrl Pts',(-3.71677276010977,0.846215280880731,
23.26969125));
#68236=CARTESIAN_POINT('Ctrl Pts',(-2.72101723061917,-2.6695590052598,23.4685775000001));
#68237=CARTESIAN_POINT('Ctrl Pts',(0.775107208778419,-3.73224983981374,
23.66746375));
#68238=CARTESIAN_POINT('Ctrl Pts',(3.55897817735421,-1.36534039162637,23.8663500000001));
#68239=CARTESIAN_POINT('Ctrl Pts',(3.07246986072833,2.25619347725455,24.06523625));
#68240=CARTESIAN_POINT('Ctrl Pts',(-0.237360568651399,3.80448945488611,
24.2641225));
#68241=CARTESIAN_POINT('Ctrl Pts',(-3.32907808804463,1.85680347252778,24.46300875));
#68242=CARTESIAN_POINT('Ctrl Pts',(-3.36167372598423,-1.79711708353053,
24.6618950000001));
#68243=CARTESIAN_POINT('Ctrl Pts',(-0.305195037191488,-3.79964946293255,
24.86078125));
#68244=CARTESIAN_POINT('Ctrl Pts',(3.03173030730948,-2.3106473975125,25.0596675000001));
#68245=CARTESIAN_POINT('Ctrl Pts',(3.58276950661523,1.30163079033885,25.25855375));
#68246=CARTESIAN_POINT('Ctrl Pts',(0.841567339384293,3.7178279230179,25.4574400000001));
#68247=CARTESIAN_POINT('Ctrl Pts',(-2.67295915204091,2.71767721104084,25.65632625));
#68248=CARTESIAN_POINT('Ctrl Pts',(-3.73127776429237,-0.77977323472104,
25.8552125000001));
#68249=CARTESIAN_POINT('Ctrl Pts',(-1.36088934335066,-3.56068255353444,
26.05409875));
#68250=CARTESIAN_POINT('Ctrl Pts',(2.26003338720418,-3.06964641947774,26.252985));
#68251=CARTESIAN_POINT('Ctrl Pts',(3.80418969631625,0.242117340005657,26.4518712500001));
#68252=CARTESIAN_POINT('Ctrl Pts',(1.852639496472,3.33139714654406,26.6507575));
#68253=CARTESIAN_POINT('Ctrl Pts',(-1.80131895941629,3.35942406646398,26.8496437500001));
#68254=CARTESIAN_POINT('Ctrl Pts',(-3.8000280944741,0.300443893426859,27.0485300000001));
#68255=CARTESIAN_POINT('Ctrl Pts',(-2.3068548565438,-3.03461706360628,27.24741625));
#68256=CARTESIAN_POINT('Ctrl Pts',(1.30610950143672,-3.58113920731194,27.4463025));
#68257=CARTESIAN_POINT('Ctrl Pts',(3.71887727353106,-0.836918082194489,
27.6451887500001));
#68258=CARTESIAN_POINT('Ctrl Pts',(2.71433294268781,2.67635511995881,27.8440750000001));
#68259=CARTESIAN_POINT('Ctrl Pts',(-0.784438041578219,3.73029985534876,
28.04296125));
#68260=CARTESIAN_POINT('Ctrl Pts',(-3.56238136299841,1.35643616748143,28.2418475));
#68261=CARTESIAN_POINT('Ctrl Pts',(-3.06681817918912,-2.2638697638524,28.44073375));
#68262=CARTESIAN_POINT('Ctrl Pts',(0.246873732837376,-3.80388399033473,
28.63962));
#68263=CARTESIAN_POINT('Ctrl Pts',(3.33371099678845,-1.8484726240282,28.8385062500001));
#68264=CARTESIAN_POINT('Ctrl Pts',(3.35716915487184,1.80551801914775,29.0373925));
#68265=CARTESIAN_POINT('Ctrl Pts',(0.295692279952789,3.80040078511023,29.23627875));
#68266=CARTESIAN_POINT('Ctrl Pts',(-3.0374990756295,2.30305870907363,29.435165));
#68267=CARTESIAN_POINT('Ctrl Pts',(-3.5795033093107,-1.31058617058311,29.6340512500001));
#68268=CARTESIAN_POINT('Ctrl Pts',(-0.832267516579828,-3.71992081000873,
29.8329375));
#68269=CARTESIAN_POINT('Ctrl Pts',(2.67974690370432,-2.71098443078842,30.03182375));
#68270=CARTESIAN_POINT('Ctrl Pts',(3.72931611451176,0.789101622057042,30.2307100000001));
#68271=CARTESIAN_POINT('Ctrl Pts',(1.35198087098079,3.56407460309012,30.42959625));
#68272=CARTESIAN_POINT('Ctrl Pts',(-2.26770260120141,3.06398514428421,30.6284825000001));
#68273=CARTESIAN_POINT('Ctrl Pts',(-3.80357233741956,-0.251629739710501,
30.82736875));
#68274=CARTESIAN_POINT('Ctrl Pts',(-1.84430286171068,-3.33601963516042,
31.0262550000001));
#68275=CARTESIAN_POINT('Ctrl Pts',(1.80971425616015,-3.35490899473305,31.22514125));
#68276=CARTESIAN_POINT('Ctrl Pts',(3.8007675342582,-0.290940204197991,31.4240275000001));
#68277=CARTESIAN_POINT('Ctrl Pts',(2.29925896103701,3.04037633887334,31.62291375));
#68278=CARTESIAN_POINT('Ctrl Pts',(-1.31506079077929,3.57786181516915,31.8218000000001));
#68279=CARTESIAN_POINT('Ctrl Pts',(-3.72095853081945,0.827615649810777,
32.02068625));
#68280=CARTESIAN_POINT('Ctrl Pts',(-2.70763168057768,-2.6831344979746,32.2195725000001));
#68281=CARTESIAN_POINT('Ctrl Pts',(0.793763968866624,-3.72832654331965,
32.41845875));
#68282=CARTESIAN_POINT('Ctrl Pts',(3.56576227116223,-1.34752346081344,32.6173450000001));
#68283=CARTESIAN_POINT('Ctrl Pts',(3.06114731919247,2.27153189325784,32.81623125));
#68284=CARTESIAN_POINT('Ctrl Pts',(-0.256385353190344,3.80325473806034,
33.0151175000001));
#68285=CARTESIAN_POINT('Ctrl Pts',(-3.33832305804911,1.84013021603382,33.21400375));
#68286=CARTESIAN_POINT('Ctrl Pts',(-3.35264358958403,-1.81390766388419,
33.4128900000001));
#68287=CARTESIAN_POINT('Ctrl Pts',(-0.286187673586392,-3.80112834136171,
33.61177625));
#68288=CARTESIAN_POINT('Ctrl Pts',(3.0432488488294,-2.29545561834177,33.8106625000001));
#68289=CARTESIAN_POINT('Ctrl Pts',(3.57621472747308,1.31953335496755,34.00954875));
#68290=CARTESIAN_POINT('Ctrl Pts',(0.822962489122625,3.72199043445967,34.208435));
#68291=CARTESIAN_POINT('Ctrl Pts',(-2.68651789740178,2.70427469706992,34.4073212500001));
#68292=CARTESIAN_POINT('Ctrl Pts',(-3.72733114345669,-0.798425074282841,
34.6062075));
#68293=CARTESIAN_POINT('Ctrl Pts',(-1.34306394368559,-3.56744436540872,
34.8050937500001));
#68294=CARTESIAN_POINT('Ctrl Pts',(2.27535763353318,-3.05830470675803,35.00398));
#68295=CARTESIAN_POINT('Ctrl Pts',(3.80293119371364,0.261140562795601,35.2028662500001));
#68296=CARTESIAN_POINT('Ctrl Pts',(1.83595469168445,3.34062126768144,35.4017525000001));
#68297=CARTESIAN_POINT('Ctrl Pts',(-1.81809823225042,3.35037293181705,35.6006387500001));
#68298=CARTESIAN_POINT('Ctrl Pts',(-3.80148321257848,0.281434716877477,
35.7995250000001));
#68299=CARTESIAN_POINT('Ctrl Pts',(-2.29164867407474,-3.0461166418114,35.9984112500001));
#68300=CARTESIAN_POINT('Ctrl Pts',(1.32400383155469,-3.57456197073556,36.1972975000001));
#68301=CARTESIAN_POINT('Ctrl Pts',(3.72301656637914,-0.818308191127896,
36.39618375));
#68302=CARTESIAN_POINT('Ctrl Pts',(2.7009133954788,2.68989738238965,36.5950700000001));
#68303=CARTESIAN_POINT('Ctrl Pts',(-0.803084758776685,3.72632936992902,
36.79395625));
#68304=CARTESIAN_POINT('Ctrl Pts',(-3.56912121270992,1.33860337215557,36.9928425000001));
#68305=CARTESIAN_POINT('Ctrl Pts',(-3.0554566810503,-2.27918181632194,37.19172875));
#68306=CARTESIAN_POINT('Ctrl Pts',(0.265894155143361,-3.80259787822564,
37.3906150000001));
#68307=CARTESIAN_POINT('Ctrl Pts',(3.34291656752411,-1.83178361584359,37.58950125));
#68308=CARTESIAN_POINT('Ctrl Pts',(3.34809261142426,1.82229995960197,37.7883875000001));
#68309=CARTESIAN_POINT('Ctrl Pts',(0.276689784930593,3.80180535505515,37.98727375));
#68310=CARTESIAN_POINT('Ctrl Pts',(-3.04899586618102,2.28788938970751,38.1861600000001));
#68311=CARTESIAN_POINT('Ctrl Pts',(-3.57287264600958,-1.32857026947732,
38.3850462500001));
#68312=CARTESIAN_POINT('Ctrl Pts',(-0.813711880402819,-3.723849330995,38.5839325000001));
#68313=CARTESIAN_POINT('Ctrl Pts',(2.6933860485815,-2.69790671903219,38.7828187500001));
#68314=CARTESIAN_POINT('Ctrl Pts',(3.72510480439603,0.808430209081211,38.9817050000001));
#68315=CARTESIAN_POINT('Ctrl Pts',(1.33455622972935,3.56947348912338,39.1805912500001));
#68316=CARTESIAN_POINT('Ctrl Pts',(-2.28380139923979,3.05516903770198,39.3794775000001));
#68317=CARTESIAN_POINT('Ctrl Pts',(-3.80069323765723,-0.275927923117959,
39.5783637500001));
#68318=CARTESIAN_POINT('Ctrl Pts',(-2.48759436411792,-2.31329607816883,
39.7109545833334));
#68319=CARTESIAN_POINT('Ctrl Pts',(-1.54513563095092,-2.82819261092061,
39.7772500000001));
#68320=CARTESIAN_POINT('',(1.87158653173903,-2.62360084935058,0.));
#68321=CARTESIAN_POINT('Ctrl Pts',(1.87158653173891,-2.62360084935066,0.));
#68322=CARTESIAN_POINT('Ctrl Pts',(2.74586769747962,-1.99991876175022,0.0662954166666667));
#68323=CARTESIAN_POINT('Ctrl Pts',(3.80646220378775,0.179585068045613,0.19888625));
#68324=CARTESIAN_POINT('Ctrl Pts',(1.90290546061669,3.30586713103499,0.3977725));
#68325=CARTESIAN_POINT('Ctrl Pts',(-1.75096977450869,3.38471360215616,0.596658750000001));
#68326=CARTESIAN_POINT('Ctrl Pts',(-3.17762645222587,1.27222962346284,0.735476766908961));
#68327=CARTESIAN_POINT('Ctrl Pts',(-3.22753027149843,0.102472337925121,
0.807999367151255));
#68328=CARTESIAN_POINT('Ctrl Pts',(-3.22687103957968,0.00196979923060637,
0.814226550726882));
#68329=CARTESIAN_POINT('Ctrl Pts',(1.75279216821278,3.52834843496255,-3.81639164714898E-17));
#68330=CARTESIAN_POINT('Ctrl Pts',(1.82191691638292,3.48650815550269,-1.21318433738122E-17));
#68331=CARTESIAN_POINT('Ctrl Pts',(1.88956902721166,3.44243155654609,4.31313297381532E-16));
#68332=CARTESIAN_POINT('Ctrl Pts',(1.95562633572894,3.39611167515613,3.72965547335014E-16));
#68333=CARTESIAN_POINT('Ctrl Pts',(2.055090558922,3.3263666140227,2.9513505280704E-16));
#68334=CARTESIAN_POINT('Ctrl Pts',(2.15094102353959,3.25153686259763,1.54341957985257E-16));
#68335=CARTESIAN_POINT('Ctrl Pts',(2.24299353637915,3.17203260947581,3.98986399474666E-16));
#68336=CARTESIAN_POINT('Ctrl Pts',(2.29704328498386,3.12535072365125,5.42632348424371E-16));
#68337=CARTESIAN_POINT('Ctrl Pts',(2.34978291432432,3.07705656763921,-1.94225233284913E-16));
#68338=CARTESIAN_POINT('Ctrl Pts',(2.40116830603661,3.02722856075797,-2.77555756156289E-16));
#68339=CARTESIAN_POINT('Ctrl Pts',(2.44043366591505,2.98915325263982,-3.41231498626496E-16));
#68340=CARTESIAN_POINT('Ctrl Pts',(2.47890818299915,2.95018225395627,-3.92682644174071E-16));
#68341=CARTESIAN_POINT('Ctrl Pts',(2.51657001727904,2.91034961927201,-4.16333634234434E-16));
#68342=CARTESIAN_POINT('Ctrl Pts',(2.53154412234642,2.89451241781124,-4.25737117014365E-16));
#68343=CARTESIAN_POINT('Ctrl Pts',(2.54639039078509,2.8785381668224,-5.91306110935837E-16));
#68344=CARTESIAN_POINT('Ctrl Pts',(2.56109596980966,2.86244180656298,-5.82867087928207E-16));
#68345=CARTESIAN_POINT('Ctrl Pts',(2.64412181623707,2.77156378450707,-5.35221427253556E-16));
#68346=CARTESIAN_POINT('Ctrl Pts',(2.72275487583107,2.67670423124671,-4.57210367042411E-16));
#68347=CARTESIAN_POINT('Ctrl Pts',(2.79680001326638,2.57828733731509,-3.46944695195361E-16));
#68348=CARTESIAN_POINT('Ctrl Pts',(2.86158950852228,2.49217255512492,-2.50462232329193E-16));
#68349=CARTESIAN_POINT('Ctrl Pts',(2.92286585232168,2.40333323665222,-1.40877212777496E-16));
#68350=CARTESIAN_POINT('Ctrl Pts',(2.98046656758873,2.31203951151562,-3.46944695195361E-16));
#68351=CARTESIAN_POINT('Ctrl Pts',(3.00570269469217,2.27204174342171,-4.37227344535292E-16));
#68352=CARTESIAN_POINT('Ctrl Pts',(3.03023288080839,2.23157272966444,1.66108317954742E-16));
#68353=CARTESIAN_POINT('Ctrl Pts',(3.05404152003192,2.19065478651688,1.94289029309402E-16));
#68354=CARTESIAN_POINT('Ctrl Pts',(3.06875072432013,2.16537529115556,2.11699341440679E-16));
#68355=CARTESIAN_POINT('Ctrl Pts',(3.08318449857401,2.13992444111478,-1.8109813009777E-16));
#68356=CARTESIAN_POINT('Ctrl Pts',(3.09733892594653,2.11430748080091,-2.22044604925031E-16));
#68357=CARTESIAN_POINT('Ctrl Pts',(3.10819488190479,2.0946601587558,-2.53449134099686E-16));
#68358=CARTESIAN_POINT('Ctrl Pts',(3.11888791824441,2.07491228675552,3.6193208763267E-17));
#68359=CARTESIAN_POINT('Ctrl Pts',(3.12940472621869,2.05508840908837,4.16333634234434E-17));
#68360=CARTESIAN_POINT('Ctrl Pts',(3.18512455295535,1.95005815356189,7.04562225862981E-17));
#68361=CARTESIAN_POINT('Ctrl Pts',(3.23597068553496,1.84277396746319,-5.60205083633985E-16));
#68362=CARTESIAN_POINT('Ctrl Pts',(3.28176671572766,1.73361210949876,-3.88578058618805E-16));
#68363=CARTESIAN_POINT('Ctrl Pts',(3.32722141767324,1.62526385973302,-2.18230208924308E-16));
#68364=CARTESIAN_POINT('Ctrl Pts',(3.36770124739318,1.5150649596808,4.5624040228757E-16));
#68365=CARTESIAN_POINT('Ctrl Pts',(3.40298410185854,1.40337142666729,4.71844785465692E-16));
#68366=CARTESIAN_POINT('Ctrl Pts',(3.43722346004176,1.29498124844761,4.8698766641906E-16));
#68367=CARTESIAN_POINT('Ctrl Pts',(3.46656871523125,1.185182805433,1.09754022917521E-16));
#68368=CARTESIAN_POINT('Ctrl Pts',(3.49076850390209,1.0743018781408,1.38777878078145E-16));
#68369=CARTESIAN_POINT('Ctrl Pts',(3.50694458616008,1.00018474327172,1.58178554460402E-16));
#68370=CARTESIAN_POINT('Ctrl Pts',(3.52082063196777,0.925583967821042,-1.4797628498031E-16));
#68371=CARTESIAN_POINT('Ctrl Pts',(3.53230884331038,0.850599325135752,-1.66533453693773E-16));
#68372=CARTESIAN_POINT('Ctrl Pts',(3.53784704101621,0.814450984571062,-1.75479430237078E-16));
#68373=CARTESIAN_POINT('Ctrl Pts',(3.54283015535757,0.778213475278794,4.31890150927375E-16));
#68374=CARTESIAN_POINT('Ctrl Pts',(3.54724746220084,0.741898253802422,4.44089209850063E-16));
#68375=CARTESIAN_POINT('Ctrl Pts',(3.54901842299873,0.727338967820404,4.48979985132335E-16));
#68376=CARTESIAN_POINT('Ctrl Pts',(3.55069805246863,0.712770036790904,-2.35249698187168E-16));
#68377=CARTESIAN_POINT('Ctrl Pts',(3.55228494128731,0.698200529246289,-2.22044604925031E-16));
#68378=CARTESIAN_POINT('Ctrl Pts',(3.56439573637877,0.587009172687399,-1.21266165516057E-16));
#68379=CARTESIAN_POINT('Ctrl Pts',(3.57112662647173,0.475642010642433,9.69433660681012E-16));
#68380=CARTESIAN_POINT('Ctrl Pts',(3.57228049049218,0.36441484357905,9.15933995315754E-16));
#68381=CARTESIAN_POINT('Ctrl Pts',(3.57294515040949,0.300344694623918,8.85116600433724E-16));
#68382=CARTESIAN_POINT('Ctrl Pts',(3.571758367986,0.23632098770379,1.62886379851061E-17));
#68383=CARTESIAN_POINT('Ctrl Pts',(3.56867460787407,0.172404957758522,2.77555756156289E-17));
#68384=CARTESIAN_POINT('Ctrl Pts',(3.56321882594294,0.0593248514506371,
4.55069473993787E-17));
#68385=CARTESIAN_POINT('Ctrl Pts',(3.55182795116294,-0.0534195019686971,
1.49200393472243E-16));
#68386=CARTESIAN_POINT('Ctrl Pts',(3.53471671103057,-0.16547091062102,8.32667268468867E-17));
#68387=CARTESIAN_POINT('Ctrl Pts',(3.517527935569,-0.278030052365175,1.70342982085031E-17));
#68388=CARTESIAN_POINT('Ctrl Pts',(3.49456629931175,-0.389890758654236,
2.39344739634145E-16));
#68389=CARTESIAN_POINT('Ctrl Pts',(3.46600457670592,-0.500664418693534,
2.77555756156289E-16));
#68390=CARTESIAN_POINT('Ctrl Pts',(3.45748853890934,-0.533692982438768,
2.88948852624566E-16));
#68391=CARTESIAN_POINT('Ctrl Pts',(3.44847437625935,-0.566624683524517,
6.71135571663658E-16));
#68392=CARTESIAN_POINT('Ctrl Pts',(3.43896601048078,-0.599448603535327,
7.21644966006352E-16));
#68393=CARTESIAN_POINT('Ctrl Pts',(3.43357461779711,-0.618060281537303,
7.50284585627391E-16));
#68394=CARTESIAN_POINT('Ctrl Pts',(3.42802355322236,-0.636639519647583,
-2.81216459416121E-16));
#68395=CARTESIAN_POINT('Ctrl Pts',(3.42232058208389,-0.655162173638946,
-2.77555756156289E-16));
#68396=CARTESIAN_POINT('Ctrl Pts',(3.38955314817876,-0.761587373008277,
-2.56522535191234E-16));
#68397=CARTESIAN_POINT('Ctrl Pts',(3.35173052613294,-0.866304866514825,
6.67536084978692E-16));
#68398=CARTESIAN_POINT('Ctrl Pts',(3.30908814868757,-0.968988090554606,
6.10622663543836E-16));
#68399=CARTESIAN_POINT('Ctrl Pts',(3.26640839035216,-1.07176132810998,5.53659351027008E-16));
#68400=CARTESIAN_POINT('Ctrl Pts',(3.2188998368367,-1.17249747840183,6.13910005376698E-16));
#68401=CARTESIAN_POINT('Ctrl Pts',(3.16675391650558,-1.27084201273691,7.21644966006352E-16));
#68402=CARTESIAN_POINT('Ctrl Pts',(3.11525182214775,-1.36797232426924,8.28049763788275E-16));
#68403=CARTESIAN_POINT('Ctrl Pts',(3.05922554692867,-1.46277033444214,5.31873682911928E-16));
#68404=CARTESIAN_POINT('Ctrl Pts',(2.99882509127823,-1.55485796594408,5.55111512312578E-16));
#68405=CARTESIAN_POINT('Ctrl Pts',(2.96292040398227,-1.60959890419193,5.68925100125488E-16));
#68406=CARTESIAN_POINT('Ctrl Pts',(2.92546942856268,-1.66338135170384,1.04307937839355E-15));
#68407=CARTESIAN_POINT('Ctrl Pts',(2.88649912210471,-1.71611830455392,1.0547118733939E-15));
#68408=CARTESIAN_POINT('Ctrl Pts',(2.86752122028498,-1.74180033798982,1.06037670818993E-15));
#68409=CARTESIAN_POINT('Ctrl Pts',(2.84818295875648,-1.76723433683073,1.01183881774261E-16));
#68410=CARTESIAN_POINT('Ctrl Pts',(2.82848721210062,-1.79240969940257,5.55111512312578E-17));
#68411=CARTESIAN_POINT('Ctrl Pts',(2.81866883519823,-1.8049596779692,3.27431856157449E-17));
#68412=CARTESIAN_POINT('Ctrl Pts',(2.80876707620499,-1.8174383783565,6.6984022778227E-16));
#68413=CARTESIAN_POINT('Ctrl Pts',(2.79878466697198,-1.82984214211003,6.66133814775094E-16));
#68414=CARTESIAN_POINT('Ctrl Pts',(2.73138918440726,-1.91358521698056,6.41110247079955E-16));
#68415=CARTESIAN_POINT('Ctrl Pts',(2.66028938173251,-1.99395520150624,3.65443711379627E-16));
#68416=CARTESIAN_POINT('Ctrl Pts',(2.58565989502056,-2.07063137270062,4.44089209850063E-16));
#68417=CARTESIAN_POINT('Ctrl Pts',(2.51208403758381,-2.14622501924906,5.21624380443388E-16));
#68418=CARTESIAN_POINT('Ctrl Pts',(2.43507686945386,-2.21822892513453,4.26467580169761E-16));
#68419=CARTESIAN_POINT('Ctrl Pts',(2.35477741768754,-2.28629489482386,4.44089209850063E-16));
#68420=CARTESIAN_POINT('Ctrl Pts',(2.27694831596886,-2.35226686800677,4.61168723827668E-16));
#68421=CARTESIAN_POINT('Ctrl Pts',(2.19602584295567,-2.41453975900013,1.30997556575806E-17));
#68422=CARTESIAN_POINT('Ctrl Pts',(2.11211808775947,-2.47275230421329,1.11022302462516E-16));
#68423=CARTESIAN_POINT('Ctrl Pts',(2.03447218398791,-2.52662057507036,2.01637104735594E-16));
#68424=CARTESIAN_POINT('Ctrl Pts',(1.95426950129378,-2.57701176798281,3.53086456726948E-16));
#68425=CARTESIAN_POINT('Ctrl Pts',(1.87158653173892,-2.62360084935066,3.33066907387547E-16));
#68426=CARTESIAN_POINT('Origin',(0.,0.,-2.31077344927314));
#68427=CARTESIAN_POINT('',(-1.87158653173914,-2.6236008493505,0.));
#68428=CARTESIAN_POINT('Ctrl Pts',(-1.87556985610733,-2.62720998907029,
2.71430013881746E-15));
#68429=CARTESIAN_POINT('Ctrl Pts',(-1.0677081740626,-3.19754239838391,0.0612793830239955));
#68430=CARTESIAN_POINT('Ctrl Pts',(1.20136616512241,-3.56759303705228,0.188547785799535));
#68431=CARTESIAN_POINT('Ctrl Pts',(3.66652278292836,-1.02049903436673,0.381805208326622));
#68432=CARTESIAN_POINT('Ctrl Pts',(2.851854515205,2.52082984529409,0.579772267581261));
#68433=CARTESIAN_POINT('Ctrl Pts',(-0.561710868652114,3.76409318953525,
0.777739326835903));
#68434=CARTESIAN_POINT('Ctrl Pts',(-2.91166705408581,1.99385906338734,0.938073054066512));
#68435=CARTESIAN_POINT('Ctrl Pts',(-3.21947657214126,0.462163466687255,
1.03241776154558));
#68436=CARTESIAN_POINT('Ctrl Pts',(-3.217941538466,0.00121291371900208,
1.06077344927309));
#68437=CARTESIAN_POINT('Origin',(0.,0.,0.));
#68438=CARTESIAN_POINT('Ctrl Pts',(-1.43290239521288,2.88667772504885,-0.41006302869194));
#68439=CARTESIAN_POINT('Ctrl Pts',(-2.39040471195644,2.41138831148588,-0.344074008940393));
#68440=CARTESIAN_POINT('Ctrl Pts',(-3.77909242612025,0.441642854121313,
-0.212095969437299));
#68441=CARTESIAN_POINT('Ctrl Pts',(-2.42543897582905,-2.93619362552599,
-0.014128910182659));
#68442=CARTESIAN_POINT('Ctrl Pts',(1.14129089352572,-3.6296651029358,0.183838149071981));
#68443=CARTESIAN_POINT('Ctrl Pts',(3.66652278292836,-1.02049903436673,0.381805208326622));
#68444=CARTESIAN_POINT('Ctrl Pts',(2.851854515205,2.52082984529409,0.579772267581261));
#68445=CARTESIAN_POINT('Ctrl Pts',(-0.561710868652114,3.76409318953525,
0.777739326835903));
#68446=CARTESIAN_POINT('Ctrl Pts',(-3.46324583227481,1.57835192224933,0.975706386090541));
#68447=CARTESIAN_POINT('Ctrl Pts',(-3.20937516570907,-2.04583258259621,
1.17367344534518));
#68448=CARTESIAN_POINT('Ctrl Pts',(-0.031229830088373,-3.80578923437654,
1.37164050459982));
#68449=CARTESIAN_POINT('Ctrl Pts',(3.17533772956661,-2.09820398373205,1.56960756385447));
#68450=CARTESIAN_POINT('Ctrl Pts',(3.48872347062518,1.52120070666785,1.7675746231091));
#68451=CARTESIAN_POINT('Ctrl Pts',(0.623360915472078,3.75454335133777,1.96554168236375));
#68452=CARTESIAN_POINT('Ctrl Pts',(-2.80997029272685,2.56695867698206,2.16350874161838));
#68453=CARTESIAN_POINT('Ctrl Pts',(-3.68300839979145,-0.95950905902386,
2.36147580087303));
#68454=CARTESIAN_POINT('Ctrl Pts',(-1.20028377732907,-3.61171960603965,
2.55944286012766));
#68455=CARTESIAN_POINT('Ctrl Pts',(2.37607494490469,-2.97312511164363,2.75740991938231));
#68456=CARTESIAN_POINT('Ctrl Pts',(3.78748084593007,0.374423891696219,2.95537697863694));
#68457=CARTESIAN_POINT('Ctrl Pts',(1.74793537283732,3.38081724446415,3.15334403789159));
#68458=CARTESIAN_POINT('Ctrl Pts',(-1.88423579077553,3.30678992389447,3.35131109714622));
#68459=CARTESIAN_POINT('Ctrl Pts',(-3.79959152376013,0.219791286247465,
3.54927815640087));
#68460=CARTESIAN_POINT('Ctrl Pts',(-2.25296143303411,-3.06746941436165,
3.7472452156555));
#68461=CARTESIAN_POINT('Ctrl Pts',(1.34644732705721,-3.55981509909713,3.94521227491016));
#68462=CARTESIAN_POINT('Ctrl Pts',(3.71904487139598,-0.808646497252913,
4.14317933416478));
#68463=CARTESIAN_POINT('Ctrl Pts',(2.70304644183217,2.67931779227495,4.34114639341943));
#68464=CARTESIAN_POINT('Ctrl Pts',(-0.775824200771678,3.72603015619545,
4.53911345267407));
#68465=CARTESIAN_POINT('Ctrl Pts',(-3.54780507800637,1.37778192696114,4.73708051192871));
#68466=CARTESIAN_POINT('Ctrl Pts',(-3.08721458058898,-2.22582794524067,
4.93504757118334));
#68467=CARTESIAN_POINT('Ctrl Pts',(0.186281715928623,-3.80138172682447,
5.133014630438));
#68468=CARTESIAN_POINT('Ctrl Pts',(3.290048016384,-1.91331857244767,5.33098168969263));
#68469=CARTESIAN_POINT('Ctrl Pts',(3.39609747398096,1.71805874664089,5.52894874894727));
#68470=CARTESIAN_POINT('Ctrl Pts',(0.407803461009433,3.78403227353958,5.72691580820191));
#68471=CARTESIAN_POINT('Ctrl Pts',(-2.95205938548467,2.40219676430168,5.92488286745655));
#68472=CARTESIAN_POINT('Ctrl Pts',(-3.62216266107621,-1.16839272787695,
6.12284992671119));
#68473=CARTESIAN_POINT('Ctrl Pts',(-0.991943885951175,-3.67440488202038,
6.32081698596584));
#68474=CARTESIAN_POINT('Ctrl Pts',(2.54208142306422,-2.83249465107694,6.51878404522046));
#68475=CARTESIAN_POINT('Ctrl Pts',(3.75989728477033,0.590234121215191,6.71675110447512));
#68476=CARTESIAN_POINT('Ctrl Pts',(1.55189462906941,3.47517294104057,6.91471816372975));
#68477=CARTESIAN_POINT('Ctrl Pts',(-2.07011190883012,3.19371892858329,7.1126852229844));
#68478=CARTESIAN_POINT('Ctrl Pts',(-3.805942529344,0.0023180169775348,7.31065228223903));
#68479=CARTESIAN_POINT('Ctrl Pts',(-2.07400065351091,-3.19119494846509,
7.50861934149368));
#68480=CARTESIAN_POINT('Ctrl Pts',(1.5476603571224,-3.4770607312591,7.70658640074832));
#68481=CARTESIAN_POINT('Ctrl Pts',(3.75917552904779,-0.594813627685692,
7.90455346000295));
#68482=CARTESIAN_POINT('Ctrl Pts',(2.54552980900885,2.82939603119107,8.1025205192576));
#68483=CARTESIAN_POINT('Ctrl Pts',(-0.987467344283091,3.67561044642204,
8.30048757851224));
#68484=CARTESIAN_POINT('Ctrl Pts',(-3.62073675046792,1.17280403038332,8.49845463776687));
#68485=CARTESIAN_POINT('Ctrl Pts',(-2.95498331987074,-2.39859906803078,
8.69642169702152));
#68486=CARTESIAN_POINT('Ctrl Pts',(0.403193815184867,-3.78452621305085,
8.89438875627614));
#68487=CARTESIAN_POINT('Ctrl Pts',(3.39400218094999,-1.72219427056852,9.0923558155308));
#68488=CARTESIAN_POINT('Ctrl Pts',(3.29237619572427,1.90930953375835,9.29032287478543));
#68489=CARTESIAN_POINT('Ctrl Pts',(0.190912054474585,3.80115199608339,9.48828993404008));
#68490=CARTESIAN_POINT('Ctrl Pts',(-3.0845010013012,2.22958684128793,9.68625699329472));
#68491=CARTESIAN_POINT('Ctrl Pts',(-3.549480726884,-1.3734593111379,9.88422405254936));
#68492=CARTESIAN_POINT('Ctrl Pts',(-0.780362316170466,-3.72508235685782,
10.082191111804));
#68493=CARTESIAN_POINT('Ctrl Pts',(2.6997807504167,-2.68260839660801,10.2801581710586));
#68494=CARTESIAN_POINT('Ctrl Pts',(3.72002712642615,0.80411571836772,10.4781252303133));
#68495=CARTESIAN_POINT('Ctrl Pts',(1.35078255368256,3.55817234019647,10.6760922895679));
#68496=CARTESIAN_POINT('Ctrl Pts',(-2.24922326994444,3.07021148975323,10.8740593488226));
#68497=CARTESIAN_POINT('Ctrl Pts',(-3.79985642608623,-0.215162847637767,
11.0720264080772));
#68498=CARTESIAN_POINT('Ctrl Pts',(-1.88826241961219,-3.30449223702413,
11.2699934673318));
#68499=CARTESIAN_POINT('Ctrl Pts',(1.74381591738736,-3.38294397768258,11.4679605265865));
#68500=CARTESIAN_POINT('Ctrl Pts',(3.78702189743871,-0.379037014277084,
11.6659275858411));
#68501=CARTESIAN_POINT('Ctrl Pts',(2.37969485505221,2.97022832568649,11.8638946450958));
#68502=CARTESIAN_POINT('Ctrl Pts',(-1.1958836268722,3.61317952236688,12.0618617043504));
#68503=CARTESIAN_POINT('Ctrl Pts',(-3.68183652508766,0.963993626743878,
12.2598287636051));
#68504=CARTESIAN_POINT('Ctrl Pts',(-2.81309572015205,-2.56353201250435,
12.4577958228597));
#68505=CARTESIAN_POINT('Ctrl Pts',(0.61878835158859,-3.75530356773067,12.6557628821143));
#68506=CARTESIAN_POINT('Ctrl Pts',(3.48686537418057,-1.52544215629862,12.853729941369));
#68507=CARTESIAN_POINT('Ctrl Pts',(3.17789604102199,2.09432105044312,13.0516970006236));
#68508=CARTESIAN_POINT('Ctrl Pts',(-0.0266032173364325,3.80585025699904,
13.2496640598783));
#68509=CARTESIAN_POINT('Ctrl Pts',(-3.20686303837221,2.04969104086312,13.4476311191329));
#68510=CARTESIAN_POINT('Ctrl Pts',(-3.46519974620323,-1.57403768340705,
13.6455981783875));
#68511=CARTESIAN_POINT('Ctrl Pts',(-0.566230666680783,-3.76358695156398,
13.8435652376421));
#68512=CARTESIAN_POINT('Ctrl Pts',(2.84865769364129,-2.52395587408549,14.0415322968968));
#68513=CARTESIAN_POINT('Ctrl Pts',(3.66800060750612,1.01536961408498,14.2394993561514));
#68514=CARTESIAN_POINT('Ctrl Pts',(1.14525637075743,3.62954429028107,14.4374664154061));
#68515=CARTESIAN_POINT('Ctrl Pts',(-2.42098458543948,2.93667116765511,14.6354334746607));
#68516=CARTESIAN_POINT('Ctrl Pts',(-3.78135309486711,-0.431940599864457,
14.8334005339154));
#68517=CARTESIAN_POINT('Ctrl Pts',(-1.696353693388,-3.4069910561669,15.03136759317));
#68518=CARTESIAN_POINT('Ctrl Pts',(1.93427300977863,-3.27777238891207,15.2293346524246));
#68519=CARTESIAN_POINT('Ctrl Pts',(3.80249297873402,-0.162021778014253,
15.4273017116793));
#68520=CARTESIAN_POINT('Ctrl Pts',(2.2060834984687,3.10135446340087,15.6252687709339));
#68521=CARTESIAN_POINT('Ctrl Pts',(-1.40039198296493,3.53894139594313,15.8232358301886));
#68522=CARTESIAN_POINT('Ctrl Pts',(-3.73090473895306,0.75203307023697,16.0212028894432));
#68523=CARTESIAN_POINT('Ctrl Pts',(-2.6620154439432,-2.72008780852388,16.2191699486979));
#68524=CARTESIAN_POINT('Ctrl Pts',(0.832360802113325,-3.71380928494957,
16.4171370079525));
#68525=CARTESIAN_POINT('Ctrl Pts',(3.56833413631518,-1.32370517921483,16.6151040672071));
#68526=CARTESIAN_POINT('Ctrl Pts',(3.05303110985611,2.27248871331039,16.8130711264618));
#68527=CARTESIAN_POINT('Ctrl Pts',(-0.244031554753848,3.79811170322264,
17.0110381857164));
#68528=CARTESIAN_POINT('Ctrl Pts',(-3.31874564019015,1.86309722923718,17.2090052449711));
#68529=CARTESIAN_POINT('Ctrl Pts',(-3.36959513369136,-1.76947239166818,
17.4069723042257));
#68530=CARTESIAN_POINT('Ctrl Pts',(-0.350248680105062,-3.78979284024299,
17.6049393634804));
#68531=CARTESIAN_POINT('Ctrl Pts',(2.98822575042405,-2.3570555306091,17.8029064227349));
#68532=CARTESIAN_POINT('Ctrl Pts',(3.60398774105126,1.2233054697109,18.0008734819896));
#68533=CARTESIAN_POINT('Ctrl Pts',(0.935987701844621,3.68905556096245,18.1988405412443));
#68534=CARTESIAN_POINT('Ctrl Pts',(-2.58483457110589,2.79353434736147,18.3968076004989));
#68535=CARTESIAN_POINT('Ctrl Pts',(-3.75049300115066,-0.647306850104539,
18.5947746597535));
#68536=CARTESIAN_POINT('Ctrl Pts',(-1.49890159705929,-3.49835645871106,
18.7927417190082));
#68537=CARTESIAN_POINT('Ctrl Pts',(2.1184092557461,-3.16188964624663,18.9907087782628));
#68538=CARTESIAN_POINT('Ctrl Pts',(3.80553821630163,0.0555229154508125,
19.1886758375175));
#68539=CARTESIAN_POINT('Ctrl Pts',(2.02526306905968,3.2223459483698,19.3866428967721));
#68540=CARTESIAN_POINT('Ctrl Pts',(-1.60032411708034,3.45313866361654,19.5846099560268));
#68541=CARTESIAN_POINT('Ctrl Pts',(-3.76778104621707,0.537615008756083,
19.7825770152813));
#68542=CARTESIAN_POINT('Ctrl Pts',(-2.50223619364232,-2.86775486070528,
19.980544074536));
#68543=CARTESIAN_POINT('Ctrl Pts',(1.04321325149407,-3.66017896034874,20.1785111337906));
#68544=CARTESIAN_POINT('Ctrl Pts',(3.63814224250802,-1.11764257844405,20.3764781930453));
#68545=CARTESIAN_POINT('Ctrl Pts',(2.91818943772608,2.44323030339269,20.5744452522999));
#68546=CARTESIAN_POINT('Ctrl Pts',(-0.460662442187536,3.77796162291654,
20.7724123115546));
#68547=CARTESIAN_POINT('Ctrl Pts',(-3.41978319510662,1.67041516047321,20.9703793708092));
#68548=CARTESIAN_POINT('Ctrl Pts',(-3.2629793075386,-1.95912479144318,21.1683464300639));
#68549=CARTESIAN_POINT('Ctrl Pts',(-0.133122145626393,-3.80361438689783,
21.3663134893184));
#68550=CARTESIAN_POINT('Ctrl Pts',(3.11802883817059,-2.18245276563067,21.5642805485732));
#68551=CARTESIAN_POINT('Ctrl Pts',(3.52819770926901,1.42724378933009,21.7622476078277));
#68552=CARTESIAN_POINT('Ctrl Pts',(0.723660398246818,3.73651168041552,21.9602146670825));
#68553=CARTESIAN_POINT('Ctrl Pts',(-2.74023779549696,2.64126877352578,22.158181726337));
#68554=CARTESIAN_POINT('Ctrl Pts',(-3.70737699001511,-0.860557821287339,
22.3561487855917));
#68555=CARTESIAN_POINT('Ctrl Pts',(-1.29655136755524,-3.57828987942048,
22.5541158448463));
#68556=CARTESIAN_POINT('Ctrl Pts',(2.29562293209663,-3.03567443305511,22.752082904101));
#68557=CARTESIAN_POINT('Ctrl Pts',(3.79614765886846,0.272886170297954,22.9500499633556));
#68558=CARTESIAN_POINT('Ctrl Pts',(1.83782445454307,3.3328074027996,23.1480170226103));
#68559=CARTESIAN_POINT('Ctrl Pts',(-1.79502668798453,3.35605171284586,23.3459840818649));
#68560=CARTESIAN_POINT('Ctrl Pts',(-3.79234494192839,0.321440120866347,
23.5439511411195));
#68561=CARTESIAN_POINT('Ctrl Pts',(-2.33428009828589,-3.00605062043518,
23.7419182003742));
#68562=CARTESIAN_POINT('Ctrl Pts',(1.25065667292649,-3.59458784790924,23.9398852596288));
#68563=CARTESIAN_POINT('Ctrl Pts',(3.6960615727801,-0.90792772845131,24.1378523188835));
#68564=CARTESIAN_POINT('Ctrl Pts',(2.77381166227548,2.60598786875474,24.3358193781381));
#68565=CARTESIAN_POINT('Ctrl Pts',(-0.675787969966405,3.74546586281613,
24.5337864373928));
#68566=CARTESIAN_POINT('Ctrl Pts',(-3.5096455310805,1.47227448393265,24.7317534966474));
#68567=CARTESIAN_POINT('Ctrl Pts',(-3.14570066854468,-2.1423751337686,24.9297205559021));
#68568=CARTESIAN_POINT('Ctrl Pts',(0.0844394074013012,-3.80500642527053,
25.1276876151567));
#68569=CARTESIAN_POINT('Ctrl Pts',(3.23764278439912,-2.00071814869078,25.3256546744113));
#68570=CARTESIAN_POINT('Ctrl Pts',(3.44087817996476,1.6265181402354,25.523621733666));
#68571=CARTESIAN_POINT('Ctrl Pts',(0.50896830631917,3.77175757081959,25.7215887929206));
#68572=CARTESIAN_POINT('Ctrl Pts',(-2.88668642961947,2.4803720218796,25.9195558521752));
#68573=CARTESIAN_POINT('Ctrl Pts',(-3.65214595660994,-1.07099664868295,
26.1175229114299));
#68574=CARTESIAN_POINT('Ctrl Pts',(-1.08996424799818,-3.64653011066113,
26.3154899706845));
#68575=CARTESIAN_POINT('Ctrl Pts',(2.46533493731419,-2.89953919730883,26.5134570299392));
#68576=CARTESIAN_POINT('Ctrl Pts',(3.77435199303925,0.489357683614875,26.7114240891938));
#68577=CARTESIAN_POINT('Ctrl Pts',(1.64438016964158,3.43237785908865,26.9093911484484));
#68578=CARTESIAN_POINT('Ctrl Pts',(-1.98386344368891,3.24799780582855,27.1073582077031));
#68579=CARTESIAN_POINT('Ctrl Pts',(-3.80451615581926,0.104214826116698,
27.3053252669577));
#68580=CARTESIAN_POINT('Ctrl Pts',(-2.15869600732759,-3.13452316275066,
27.5032923262124));
#68581=CARTESIAN_POINT('Ctrl Pts',(1.45401317967913,-3.51725028725448,27.701259385467));
#68582=CARTESIAN_POINT('Ctrl Pts',(3.74190285747308,-0.695245938576497,
27.8992264447217));
#68583=CARTESIAN_POINT('Ctrl Pts',(2.6203695833697,2.76022954777739,28.0971935039762));
#68584=CARTESIAN_POINT('Ctrl Pts',(-0.888705147656408,3.70073061305487,
28.295160563231));
#68585=CARTESIAN_POINT('Ctrl Pts',(-3.58803899461921,1.26932268669724,28.4931276224855));
#68586=CARTESIAN_POINT('Ctrl Pts',(-3.01814246160937,-2.31862459042054,
28.6910946817402));
#68587=CARTESIAN_POINT('Ctrl Pts',(0.301725028063924,-3.79396440643719,
28.8890617409948));
#68588=CARTESIAN_POINT('Ctrl Pts',(3.34667671285774,-1.8124455549031,29.0870288002495));
#68589=CARTESIAN_POINT('Ctrl Pts',(3.34231449720922,1.8204773307068,29.2849958595041));
#68590=CARTESIAN_POINT('Ctrl Pts',(0.292613000107598,3.79467805512411,29.4829629187588));
#68591=CARTESIAN_POINT('Ctrl Pts',(-3.023701906425,2.31136987324706,29.6809299780134));
#68592=CARTESIAN_POINT('Ctrl Pts',(-3.58498038573646,-1.27793565712721,
29.878897037268));
#68593=CARTESIAN_POINT('Ctrl Pts',(-0.879815326883564,-3.70285415597931,
30.0768640965227));
#68594=CARTESIAN_POINT('Ctrl Pts',(2.62699068395643,-2.75392880377806,30.2748311557773));
#68595=CARTESIAN_POINT('Ctrl Pts',(3.74022244301854,0.70423006653559,30.4727982150319));
#68596=CARTESIAN_POINT('Ctrl Pts',(1.44556235449795,3.52073193940277,30.6707652742866));
#68597=CARTESIAN_POINT('Ctrl Pts',(-2.16621730060395,3.12933004274663,30.8687323335412));
#68598=CARTESIAN_POINT('Ctrl Pts',(-3.80425491461396,-0.113351023408669,
31.0666993927959));
#68599=CARTESIAN_POINT('Ctrl Pts',(-1.9760576970998,-3.25275266314625,31.2646664520505));
#68600=CARTESIAN_POINT('Ctrl Pts',(1.65261824030163,-3.42841900322799,31.4626335113052));
#68601=CARTESIAN_POINT('Ctrl Pts',(3.77551629574763,-0.480292213570351,
31.6606005705598));
#68602=CARTESIAN_POINT('Ctrl Pts',(2.45836462134124,2.90545130718283,31.8585676298145));
#68603=CARTESIAN_POINT('Ctrl Pts',(-1.0987182013029,3.64390206015446,32.0565346890691));
#68604=CARTESIAN_POINT('Ctrl Pts',(-3.65470741038376,1.06222297770173,32.2545017483237));
#68605=CARTESIAN_POINT('Ctrl Pts',(-2.88072152335954,-2.4872972107748,32.4524688075784));
#68606=CARTESIAN_POINT('Ctrl Pts',(0.518024667143807,-3.77052441367253,
32.650435866833));
#68607=CARTESIAN_POINT('Ctrl Pts',(3.44477432083465,-1.61825022428116,32.8484029260877));
#68608=CARTESIAN_POINT('Ctrl Pts',(3.23282874888886,2.00848753798692,33.0463699853423));
#68609=CARTESIAN_POINT('Ctrl Pts',(0.0753014887309373,3.80519823342296,
33.2443370445969));
#68610=CARTESIAN_POINT('Ctrl Pts',(-3.15083648467107,2.1348145953959,33.4423041038516));
#68611=CARTESIAN_POINT('Ctrl Pts',(-3.50609976207099,-1.48069860822725,
33.6402711631062));
#68612=CARTESIAN_POINT('Ctrl Pts',(-0.666791331988793,-3.74707795879318,
33.8382382223608));
#68613=CARTESIAN_POINT('Ctrl Pts',(2.78006191089306,-2.59931908033378,34.0362052816155));
#68614=CARTESIAN_POINT('Ctrl Pts',(3.69387053796041,0.916801155928787,34.2341723408701));
#68615=CARTESIAN_POINT('Ctrl Pts',(1.24202070877136,3.59758091881176,34.4321394001247));
#68616=CARTESIAN_POINT('Ctrl Pts',(-2.34149235969762,3.0004362081648,34.6301064593794));
#68617=CARTESIAN_POINT('Ctrl Pts',(-3.79156207268276,-0.330546463261181,
34.828073518634));
#68618=CARTESIAN_POINT('Ctrl Pts',(-1.78696199451318,-3.36035276851525,
35.0260405778887));
#68619=CARTESIAN_POINT('Ctrl Pts',(1.84582284769266,-3.32838428188693,35.2240076371433));
#68620=CARTESIAN_POINT('Ctrl Pts',(3.79679204988465,-0.263768978904437,
35.421974696398));
#68621=CARTESIAN_POINT('Ctrl Pts',(2.28832616929499,3.04117858234319,35.6199417556526));
#68622=CARTESIAN_POINT('Ctrl Pts',(-1.30514082959193,3.5751659222856,35.8179088149073));
#68623=CARTESIAN_POINT('Ctrl Pts',(-3.70943295180687,0.851652095669924,
36.0158758741619));
#68624=CARTESIAN_POINT('Ctrl Pts',(-2.73388685593464,-2.64784175641783,
36.2138429334166));
#68625=CARTESIAN_POINT('Ctrl Pts',(0.732631374839026,-3.7347631354025,36.4118099926711));
#68626=CARTESIAN_POINT('Ctrl Pts',(3.53161527805439,-1.41876657738429,36.6097770519258));
#68627=CARTESIAN_POINT('Ctrl Pts',(3.11277826536447,2.18993404682541,36.8077441111804));
#68628=CARTESIAN_POINT('Ctrl Pts',(-0.14225523522422,3.80328436424815,37.0057111704351));
#68629=CARTESIAN_POINT('Ctrl Pts',(-3.26767635523122,1.95128192038049,37.2036782296897));
#68630=CARTESIAN_POINT('Ctrl Pts',(-3.41575870887161,-1.6786205797561,37.4016452889444));
#68631=CARTESIAN_POINT('Ctrl Pts',(-0.451594402129131,-3.77906146290628,
37.599612348199));
#68632=CARTESIAN_POINT('Ctrl Pts',(2.92405992033173,-2.43620673106119,37.7975794074536));
#68633=CARTESIAN_POINT('Ctrl Pts',(3.63542572274911,1.12635998382311,37.9955464667083));
#68634=CARTESIAN_POINT('Ctrl Pts',(1.03446251089667,3.6627049053714,38.1935135259629));
#68635=CARTESIAN_POINT('Ctrl Pts',(-2.50919648981435,2.86167773530498,38.3914805852176));
#68636=CARTESIAN_POINT('Ctrl Pts',(-3.76632481410217,-0.546547375939128,
38.5894476444722));
#68637=CARTESIAN_POINT('Ctrl Pts',(-1.59232210767045,-3.45719070782108,
38.7874147037269));
#68638=CARTESIAN_POINT('Ctrl Pts',(2.03356109694112,-3.21705406573836,38.9853817629815));
#68639=CARTESIAN_POINT('Ctrl Pts',(3.80457448616929,-0.0471873108411222,
39.1833488222361));
#68640=CARTESIAN_POINT('Ctrl Pts',(2.11292542611656,3.16852227003697,39.3813158814907));
#68641=CARTESIAN_POINT('Ctrl Pts',(-1.51168002663127,3.4916201787766,39.5792829407454));
#68642=CARTESIAN_POINT('Ctrl Pts',(-2.99782464886751,1.59432608031001,39.7112609802485));
#68643=CARTESIAN_POINT('Ctrl Pts',(-3.17710367210759,0.540490350682096,
39.7772500000001));
#68644=CARTESIAN_POINT('Ctrl Pts',(-1.5381664219189,3.09873914818289,-0.273375352461296));
#68645=CARTESIAN_POINT('Ctrl Pts',(-2.56600887472297,2.58853397365147,-0.207386332709749));
#68646=CARTESIAN_POINT('Ctrl Pts',(-4.05671251203569,0.474086867995491,
-0.0754082932066554));
#68647=CARTESIAN_POINT('Ctrl Pts',(-2.60361682937877,-3.15189259095719,
0.122558766047985));
#68648=CARTESIAN_POINT('Ctrl Pts',(1.22513252537504,-3.89630794309404,0.320525825302625));
#68649=CARTESIAN_POINT('Ctrl Pts',(3.93587326585702,-1.0954670419336,0.518492884557265));
#68650=CARTESIAN_POINT('Ctrl Pts',(3.06135775202903,2.70601531294549,0.716459943811906));
#68651=CARTESIAN_POINT('Ctrl Pts',(-0.60297533165843,4.04061139995257,0.914427003066545));
#68652=CARTESIAN_POINT('Ctrl Pts',(-3.71766316244039,1.69430097743274,1.11239406232119));
#68653=CARTESIAN_POINT('Ctrl Pts',(-3.44514262222338,-2.19612375129681,
1.31036112157583));
#68654=CARTESIAN_POINT('Ctrl Pts',(-0.0335240391561582,-4.08537052403247,
1.50832818083047));
#68655=CARTESIAN_POINT('Ctrl Pts',(3.40860472436144,-2.25234246581983,1.70629524008511));
#68656=CARTESIAN_POINT('Ctrl Pts',(3.74501244174315,1.63295131323175,1.90426229933975));
#68657=CARTESIAN_POINT('Ctrl Pts',(0.669154320712261,4.03036001053543,2.10222935859439));
#68658=CARTESIAN_POINT('Ctrl Pts',(-3.01639662638699,2.75553286572625,2.30019641784903));
#68659=CARTESIAN_POINT('Ctrl Pts',(-3.95356995084275,-1.02999661459724,
2.49816347710367));
#68660=CARTESIAN_POINT('Ctrl Pts',(-1.28845915062283,-3.87704413221449,
2.69613053635831));
#68661=CARTESIAN_POINT('Ctrl Pts',(2.55062641281451,-3.19153714179847,2.89409759561295));
#68662=CARTESIAN_POINT('Ctrl Pts',(4.06571716282525,0.40192985907169,3.09206465486759));
#68663=CARTESIAN_POINT('Ctrl Pts',(1.87634238533256,3.62917919702857,3.29003171412223));
#68664=CARTESIAN_POINT('Ctrl Pts',(-2.02265571893201,3.54971367363674,3.48799877337687));
#68665=CARTESIAN_POINT('Ctrl Pts',(-4.07871751654587,0.235937616871581,
3.68596583263151));
#68666=CARTESIAN_POINT('Ctrl Pts',(-2.41846872316541,-3.29281217562152,
3.88393289188615));
#68667=CARTESIAN_POINT('Ctrl Pts',(1.44536018243879,-3.82132661091504,4.08189995114079));
#68668=CARTESIAN_POINT('Ctrl Pts',(3.99225373752058,-0.868051371420758,
4.27986701039543));
#68669=CARTESIAN_POINT('Ctrl Pts',(2.90161792429393,2.87614611818334,4.47783406965007));
#68670=CARTESIAN_POINT('Ctrl Pts',(-0.83281787993789,3.99975217604782,4.67580112890471));
#68671=CARTESIAN_POINT('Ctrl Pts',(-3.80843430838976,1.47899668802168,4.87376818815935));
#68672=CARTESIAN_POINT('Ctrl Pts',(-3.31400786333022,-2.38934195223343,
5.071735247414));
#68673=CARTESIAN_POINT('Ctrl Pts',(0.199966362968053,-4.0806392316963,5.26970230666863));
#68674=CARTESIAN_POINT('Ctrl Pts',(3.53174187035313,-2.05387498297495,5.46766936592327));
#68675=CARTESIAN_POINT('Ctrl Pts',(3.64558194437578,1.84427095927526,5.66563642517792));
#68676=CARTESIAN_POINT('Ctrl Pts',(0.437761561822023,4.06201525104653,5.86360348443255));
#68677=CARTESIAN_POINT('Ctrl Pts',(-3.16892388304534,2.57866719605973,6.0615705436872));
#68678=CARTESIAN_POINT('Ctrl Pts',(-3.88825435606022,-1.25422531753642,
6.25953760294183));
#68679=CARTESIAN_POINT('Ctrl Pts',(-1.064814172197,-3.94433440054288,6.45750466219648));
#68680=CARTESIAN_POINT('Ctrl Pts',(2.72882807636051,-3.04057567152293,6.65547172145111));
#68681=CARTESIAN_POINT('Ctrl Pts',(4.03610725518979,0.633593962406071,6.85343878070576));
#68682=CARTESIAN_POINT('Ctrl Pts',(1.66590007579409,3.73046646172677,7.05140583996039));
#68683=CARTESIAN_POINT('Ctrl Pts',(-2.22218668795221,3.42833624495657,7.24937289921504));
#68684=CARTESIAN_POINT('Ctrl Pts',(-4.08553508037097,0.00248830338486328,
7.44733995846967));
#68685=CARTESIAN_POINT('Ctrl Pts',(-2.22636110800429,-3.4256268479451,7.64530701772432));
#68686=CARTESIAN_POINT('Ctrl Pts',(1.66135474531538,-3.73249293298914,7.84327407697896));
#68687=CARTESIAN_POINT('Ctrl Pts',(4.03533247777236,-0.638509889063205,
8.0412411362336));
#68688=CARTESIAN_POINT('Ctrl Pts',(2.73252978799657,3.03724942049667,8.23920819548824));
#68689=CARTESIAN_POINT('Ctrl Pts',(-1.06000877435344,3.94562852824358,8.43717525474288));
#68690=CARTESIAN_POINT('Ctrl Pts',(-3.88672369505666,1.2589606836121,8.63514231399753));
#68691=CARTESIAN_POINT('Ctrl Pts',(-3.17206261580721,-2.57480520544648,
8.83310937325215));
#68692=CARTESIAN_POINT('Ctrl Pts',(0.432813281710421,-4.0625454763942,9.03107643250681));
#68693=CARTESIAN_POINT('Ctrl Pts',(3.6433327267075,-1.8487102874972,9.22904349176143));
#68694=CARTESIAN_POINT('Ctrl Pts',(3.5342410826493,2.04957143186323,9.42701055101609));
#68695=CARTESIAN_POINT('Ctrl Pts',(0.204936855931924,4.08039262445131,9.62497761027071));
#68696=CARTESIAN_POINT('Ctrl Pts',(-3.31109493879501,2.39337698469798,9.82294466952537));
#68697=CARTESIAN_POINT('Ctrl Pts',(-3.81023305396172,-1.4743565237396,10.02091172878));
#68698=CARTESIAN_POINT('Ctrl Pts',(-0.837689374848039,-3.99873474937543,
10.2188787880347));
#68699=CARTESIAN_POINT('Ctrl Pts',(2.89811232831176,-2.87967845723847,10.4168458472893));
#68700=CARTESIAN_POINT('Ctrl Pts',(3.99330815107321,0.863187751979935,10.6148129065439));
#68701=CARTESIAN_POINT('Ctrl Pts',(1.45001388393906,3.81956317148701,10.8127799657986));
#68702=CARTESIAN_POINT('Ctrl Pts',(-2.41445594674516,3.2957556896443,11.0107470250532));
#68703=CARTESIAN_POINT('Ctrl Pts',(-4.07900187915454,-0.230969163417291,
11.2087140843079));
#68704=CARTESIAN_POINT('Ctrl Pts',(-2.02697815240034,-3.54724719385154,
11.4066811435625));
#68705=CARTESIAN_POINT('Ctrl Pts',(1.87192030601249,-3.63146216454668,11.6046482028171));
#68706=CARTESIAN_POINT('Ctrl Pts',(4.06522449901148,-0.406881871349422,
11.8026152620718));
#68707=CARTESIAN_POINT('Ctrl Pts',(2.55451224918252,3.18842755184626,12.0005823213264));
#68708=CARTESIAN_POINT('Ctrl Pts',(-1.28373575584969,3.8786112970687,12.198549380581));
#68709=CARTESIAN_POINT('Ctrl Pts',(-3.95231198775605,1.0348106281034,12.3965164398357));
#68710=CARTESIAN_POINT('Ctrl Pts',(-3.01975165429086,-2.75185447126179,
12.5944834990903));
#68711=CARTESIAN_POINT('Ctrl Pts',(0.664245846659203,-4.03117607402505,
12.792450558345));
#68712=CARTESIAN_POINT('Ctrl Pts',(3.74301784562183,-1.63750434868199,12.9904176175996));
#68713=CARTESIAN_POINT('Ctrl Pts',(3.41135097476238,2.24817428407668,13.1883846768543));
#68714=CARTESIAN_POINT('Ctrl Pts',(-0.0285575456909824,4.0854360295053,
13.3863517361089));
#68715=CARTESIAN_POINT('Ctrl Pts',(-3.44244594872354,2.20026566003127,13.5843187953636));
#68716=CARTESIAN_POINT('Ctrl Pts',(-3.71976061499961,-1.68966980552226,
13.7822858546182));
#68717=CARTESIAN_POINT('Ctrl Pts',(-0.607827163565885,-4.04006797267415,
13.9802529138728));
#68718=CARTESIAN_POINT('Ctrl Pts',(3.05792608522293,-2.70937098639317,14.1782199731274));
#68719=CARTESIAN_POINT('Ctrl Pts',(3.93745965453956,1.08996080363888,14.3761870323821));
#68720=CARTESIAN_POINT('Ctrl Pts',(1.22938931491277,3.89617825528739,14.5741540916367));
#68721=CARTESIAN_POINT('Ctrl Pts',(-2.59883521009326,3.15240521433642,14.7721211508914));
#68722=CARTESIAN_POINT('Ctrl Pts',(-4.05913925426817,-0.463671865714468,
14.970088210146));
#68723=CARTESIAN_POINT('Ctrl Pts',(-1.82097140711367,-3.65727579204391,
15.1680552694007));
#68724=CARTESIAN_POINT('Ctrl Pts',(2.07636877738867,-3.51856444944261,15.3660223286553));
#68725=CARTESIAN_POINT('Ctrl Pts',(4.08183211851069,-0.173924238938826,
15.5639893879099));
#68726=CARTESIAN_POINT('Ctrl Pts',(2.36814703683261,3.32918649170288,15.7619564471646));
#68727=CARTESIAN_POINT('Ctrl Pts',(-1.50326772634159,3.798919481581,15.9599235064192));
#68728=CARTESIAN_POINT('Ctrl Pts',(-4.0049848559175,0.807279002865442,16.1578905656739));
#68729=CARTESIAN_POINT('Ctrl Pts',(-2.85757270291564,-2.91991118566086,
16.3558576249285));
#68730=CARTESIAN_POINT('Ctrl Pts',(0.893507779043135,-3.98663353387107,
16.5538246841831));
#68731=CARTESIAN_POINT('Ctrl Pts',(3.83047147454269,-1.42094734853573,16.7517917434378));
#68732=CARTESIAN_POINT('Ctrl Pts',(3.27731320286931,2.43943051856256,16.9497588026924));
#68733=CARTESIAN_POINT('Ctrl Pts',(-0.261958626536699,4.07712898527615,
17.1477258619471));
#68734=CARTESIAN_POINT('Ctrl Pts',(-3.56254768202248,1.99996427415897,17.3456929212017));
#68735=CARTESIAN_POINT('Ctrl Pts',(-3.61713268637194,-1.8994615589097,17.5436599804563));
#68736=CARTESIAN_POINT('Ctrl Pts',(-0.375978685539757,-4.06819900110795,
17.741627039711));
#68737=CARTESIAN_POINT('Ctrl Pts',(3.20774710529583,-2.53020979230223,17.9395940989656));
#68738=CARTESIAN_POINT('Ctrl Pts',(3.86874426814577,1.31317206499575,18.1375611582203));
#68739=CARTESIAN_POINT('Ctrl Pts',(1.00474732899892,3.96006134920477,18.3355282174749));
#68740=CARTESIAN_POINT('Ctrl Pts',(-2.77472196066743,2.99875326187165,18.5334952767295));
#68741=CARTESIAN_POINT('Ctrl Pts',(-4.02601211309617,-0.694859374117405,
18.7314623359842));
#68742=CARTESIAN_POINT('Ctrl Pts',(-1.60901406408391,-3.75535308941463,
18.9294293952388));
#68743=CARTESIAN_POINT('Ctrl Pts',(2.2740320596552,-3.39416871652785,19.1273964544934));
#68744=CARTESIAN_POINT('Ctrl Pts',(4.0851010656413,0.0596017457147811,19.3253635137481));
#68745=CARTESIAN_POINT('Ctrl Pts',(2.17404315798984,3.45906626588641,19.5233305730027));
#68746=CARTESIAN_POINT('Ctrl Pts',(-1.7178872959552,3.70681349989336,19.7212976322574));
#68747=CARTESIAN_POINT('Ctrl Pts',(-4.04457017435047,0.577109339164211,
19.919264691512));
#68748=CARTESIAN_POINT('Ctrl Pts',(-2.68605573249723,-3.07842617038556,
20.1172317507667));
#68749=CARTESIAN_POINT('Ctrl Pts',(1.1198498932725,-3.92906341271473,20.3151988100213));
#68750=CARTESIAN_POINT('Ctrl Pts',(3.90540783118658,-1.19974695527949,20.513165869276));
#68751=CARTESIAN_POINT('Ctrl Pts',(3.13256577761639,2.62271514532222,20.7111329285306));
#68752=CARTESIAN_POINT('Ctrl Pts',(-0.494503675043983,4.0554986376479,20.9090999877852));
#68753=CARTESIAN_POINT('Ctrl Pts',(-3.671007668442,1.79312737496141,21.1070670470398));
#68754=CARTESIAN_POINT('Ctrl Pts',(-3.50268463716692,-2.10304622325587,
21.3050341062945));
#68755=CARTESIAN_POINT('Ctrl Pts',(-0.142901578712061,-4.08303590767917,
21.5030011655491));
#68756=CARTESIAN_POINT('Ctrl Pts',(3.34708580114849,-2.34278034060945,21.7009682248038));
#68757=CARTESIAN_POINT('Ctrl Pts',(3.78738654106464,1.53209212293465,21.8989352840584));
#68758=CARTESIAN_POINT('Ctrl Pts',(0.776822014656629,4.01100369510435,22.0969023433131));
#68759=CARTESIAN_POINT('Ctrl Pts',(-2.94154143309964,2.83530193841045,22.2948694025677));
#68760=CARTESIAN_POINT('Ctrl Pts',(-3.97972870900853,-0.923776210610116,
22.4928364618223));
#68761=CARTESIAN_POINT('Ctrl Pts',(-1.39179876070348,-3.84115858749677,
22.690803521077));
#68762=CARTESIAN_POINT('Ctrl Pts',(2.46426422576634,-3.25868146804872,22.8887705803316));
#68763=CARTESIAN_POINT('Ctrl Pts',(4.07502065808871,0.292932962887592,23.0867376395863));
#68764=CARTESIAN_POINT('Ctrl Pts',(1.97283490822794,3.57764245131808,23.2847046988409));
#68765=CARTESIAN_POINT('Ctrl Pts',(-1.92689312763407,3.60259433731756,23.4826717580955));
#68766=CARTESIAN_POINT('Ctrl Pts',(-4.07093858555621,0.345053788887412,
23.6806388173502));
#68767=CARTESIAN_POINT('Ctrl Pts',(-2.50576122877042,-3.22688142778547,
23.8786058766048));
#68768=CARTESIAN_POINT('Ctrl Pts',(1.34253254518328,-3.85865383906351,24.0765729358595));
#68769=CARTESIAN_POINT('Ctrl Pts',(3.96758203740061,-0.974626010884212,
24.2745399951141));
#68770=CARTESIAN_POINT('Ctrl Pts',(2.97758170681619,2.79742922409655,24.4725070543687));
#68771=CARTESIAN_POINT('Ctrl Pts',(-0.725432777006904,4.02061567059572,
24.6704741136234));
#68772=CARTESIAN_POINT('Ctrl Pts',(-3.76747148080772,1.58043086716773,24.868441172878));
#68773=CARTESIAN_POINT('Ctrl Pts',(-3.37679046244053,-2.29975852153367,
25.0664082321327));
#68774=CARTESIAN_POINT('Ctrl Pts',(0.090642504043137,-4.08453020812145,
25.2643752913873));
#68775=CARTESIAN_POINT('Ctrl Pts',(3.47548683969556,-2.14769511609513,25.4623423506419));
#68776=CARTESIAN_POINT('Ctrl Pts',(3.69365233529998,1.74600558719869,25.6603094098966));
#68777=CARTESIAN_POINT('Ctrl Pts',(0.546358189655095,4.04883882282225,25.8582764691512));
#68778=CARTESIAN_POINT('Ctrl Pts',(-3.09874849220967,2.6625853726452,26.0562435284059));
#68779=CARTESIAN_POINT('Ctrl Pts',(-3.92044028760904,-1.1496743173125,26.2542105876605));
#68780=CARTESIAN_POINT('Ctrl Pts',(-1.17003531640664,-3.91441188979357,
26.4521776469151));
#68781=CARTESIAN_POINT('Ctrl Pts',(2.64644363218947,-3.11254545127291,26.6501447061698));
#68782=CARTESIAN_POINT('Ctrl Pts',(4.05162383676031,0.525306929319951,26.8481117654244));
#68783=CARTESIAN_POINT('Ctrl Pts',(1.76517979889065,3.68452756295626,27.0460788246791));
#68784=CARTESIAN_POINT('Ctrl Pts',(-2.12960222897897,3.48660256280002,27.2440458839337));
#68785=CARTESIAN_POINT('Ctrl Pts',(-4.08400392244411,0.111870666651306,
27.4420129431883));
#68786=CARTESIAN_POINT('Ctrl Pts',(-2.31727836082527,-3.36479183353844,
27.639980002443));
#68787=CARTESIAN_POINT('Ctrl Pts',(1.56082804905753,-3.77563489838082,27.8379470616976));
#68788=CARTESIAN_POINT('Ctrl Pts',(4.01679091937884,-0.746320168956691,
28.0359141209523));
#68789=CARTESIAN_POINT('Ctrl Pts',(2.8128674497455,2.96300182159213,28.2338811802069));
#68790=CARTESIAN_POINT('Ctrl Pts',(-0.953991298834084,3.97259407520387,
28.4318482394615));
#68791=CARTESIAN_POINT('Ctrl Pts',(-3.85162389322325,1.36256980362389,28.6298152987162));
#68792=CARTESIAN_POINT('Ctrl Pts',(-3.23986156106973,-2.48895563433715,
28.8277823579708));
#68793=CARTESIAN_POINT('Ctrl Pts',(0.323890383860786,-4.07267701933735,
29.0257494172255));
#68794=CARTESIAN_POINT('Ctrl Pts',(3.59253063009277,-1.94559162118907,29.2237164764801));
#68795=CARTESIAN_POINT('Ctrl Pts',(3.58784795689867,1.95421342815309,29.4216835357347));
#68796=CARTESIAN_POINT('Ctrl Pts',(0.3141089671467,4.0734430941593,29.6196505949894));
#68797=CARTESIAN_POINT('Ctrl Pts',(-3.24582941440615,2.48116797036631,29.817617654244));
#68798=CARTESIAN_POINT('Ctrl Pts',(-3.8483405924925,-1.37181550099505,30.0155847134987));
#68799=CARTESIAN_POINT('Ctrl Pts',(-0.944448413111001,-3.97487361806236,
30.2135517727533));
#68800=CARTESIAN_POINT('Ctrl Pts',(2.81997495032113,-2.95623821167328,30.4115188320079));
#68801=CARTESIAN_POINT('Ctrl Pts',(4.0149870581406,0.755964289870477,30.6094858912626));
#68802=CARTESIAN_POINT('Ctrl Pts',(1.55175640846651,3.77937232002606,30.8074529505172));
#68803=CARTESIAN_POINT('Ctrl Pts',(-2.32535218414073,3.35921721600553,31.0054200097719));
#68804=CARTESIAN_POINT('Ctrl Pts',(-4.08372348990986,-0.121678028231323,
31.2033870690265));
#68805=CARTESIAN_POINT('Ctrl Pts',(-2.12122305581152,-3.49170672194696,
31.4013541282812));
#68806=CARTESIAN_POINT('Ctrl Pts',(1.77402305556549,-3.68027788120926,31.5993211875358));
#68807=CARTESIAN_POINT('Ctrl Pts',(4.05287367159691,-0.515575490759886,
31.7972882467904));
#68808=CARTESIAN_POINT('Ctrl Pts',(2.63896126213013,3.11889187718537,31.9952553060451));
#68809=CARTESIAN_POINT('Ctrl Pts',(-1.17943235355135,3.91159077716369,32.1932223652997));
#68810=CARTESIAN_POINT('Ctrl Pts',(-3.92318991116986,1.14025611398928,32.3911894245544));
#68811=CARTESIAN_POINT('Ctrl Pts',(-3.09234539137761,-2.67001930049665,
32.589156483809));
#68812=CARTESIAN_POINT('Ctrl Pts',(0.556079849812804,-4.04751507535492,
32.7871235430637));
#68813=CARTESIAN_POINT('Ctrl Pts',(3.69783469488094,-1.73713029273151,32.9850906023183));
#68814=CARTESIAN_POINT('Ctrl Pts',(3.47031915500144,2.15603526108631,33.183057661573));
#68815=CARTESIAN_POINT('Ctrl Pts',(0.0808332946286449,4.08473610690458,
33.3810247208275));
#68816=CARTESIAN_POINT('Ctrl Pts',(-3.38230356643229,2.29164257009446,33.5789917800823));
#68817=CARTESIAN_POINT('Ctrl Pts',(-3.76366523214165,-1.58947384536882,
33.7769588393368));
#68818=CARTESIAN_POINT('Ctrl Pts',(-0.715775227062298,-4.02234619453729,
33.9749258985915));
#68819=CARTESIAN_POINT('Ctrl Pts',(2.98429111185623,-2.79027053243799,34.1728929578461));
#68820=CARTESIAN_POINT('Ctrl Pts',(3.96523004455014,0.984151299025936,34.3708600171008));
#68821=CARTESIAN_POINT('Ctrl Pts',(1.3332621649195,3.86186678725603,34.5688270763554));
#68822=CARTESIAN_POINT('Ctrl Pts',(-2.51350331808985,3.22085456896936,34.76679413561));
#68823=CARTESIAN_POINT('Ctrl Pts',(-4.07009820508757,-0.354829102366696,
34.9647611948647));
#68824=CARTESIAN_POINT('Ctrl Pts',(-1.91823598480123,-3.60721135759169,
35.1627282541193));
#68825=CARTESIAN_POINT('Ctrl Pts',(1.98142088017778,-3.5728943986309,35.360695313374));
#68826=CARTESIAN_POINT('Ctrl Pts',(4.07571238742562,-0.283146003419342,
35.5586623726286));
#68827=CARTESIAN_POINT('Ctrl Pts',(2.45643142740698,3.26458996373172,35.7566294318833));
#68828=CARTESIAN_POINT('Ctrl Pts',(-1.4010192227053,3.8378051378937,35.9545964911379));
#68829=CARTESIAN_POINT('Ctrl Pts',(-3.98193570608205,0.914216251639095,
36.1525635503925));
#68830=CARTESIAN_POINT('Ctrl Pts',(-2.93472394014607,-2.84235778646424,
36.3505306096472));
#68831=CARTESIAN_POINT('Ctrl Pts',(0.786452018076432,-4.00912669829336,
36.5484976689018));
#68832=CARTESIAN_POINT('Ctrl Pts',(3.7910551716482,-1.52299215715173,36.7464647281564));
#68833=CARTESIAN_POINT('Ctrl Pts',(3.34144951020968,2.35081121247155,36.9444317874111));
#68834=CARTESIAN_POINT('Ctrl Pts',(-0.15270560430018,4.08268164087083,37.1423988466657));
#68835=CARTESIAN_POINT('Ctrl Pts',(-3.50772673987201,2.09462719837285,37.3403659059204));
#68836=CARTESIAN_POINT('Ctrl Pts',(-3.66668753497517,-1.80193558162018,
37.5383329651751));
#68837=CARTESIAN_POINT('Ctrl Pts',(-0.484769477671406,-4.05667927419883,
37.7363000244296));
#68838=CARTESIAN_POINT('Ctrl Pts',(3.13886751823373,-2.6151756065801,37.9342670836843));
#68839=CARTESIAN_POINT('Ctrl Pts',(3.90249175016692,1.20910475961097,38.1322341429389));
#68840=CARTESIAN_POINT('Ctrl Pts',(1.11045630484736,3.93177491897678,38.3302012021936));
#68841=CARTESIAN_POINT('Ctrl Pts',(-2.69352734667998,3.07190260655882,38.5281682614482));
#68842=CARTESIAN_POINT('Ctrl Pts',(-4.04300696435851,-0.586697896846368,
38.7261353207029));
#68843=CARTESIAN_POINT('Ctrl Pts',(-1.70929744208696,-3.71116321579617,
38.9241023799575));
#68844=CARTESIAN_POINT('Ctrl Pts',(2.18295077646978,-3.45338563041556,39.1220694392121));
#68845=CARTESIAN_POINT('Ctrl Pts',(4.08406653786445,-0.0506537900410035,
39.3200364984668));
#68846=CARTESIAN_POINT('Ctrl Pts',(2.26814537635562,3.40128858682585,39.5180035577214));
#68847=CARTESIAN_POINT('Ctrl Pts',(-1.62273122399537,3.74812194817393,39.7159706169761));
#68848=CARTESIAN_POINT('Ctrl Pts',(-3.21805115902793,1.71144863077568,39.8479486564791));
#68849=CARTESIAN_POINT('Ctrl Pts',(-3.41050039675936,0.580195909761704,
39.9139376762307));
#68850=CARTESIAN_POINT('Ctrl Pts',(-1.64343044862492,3.31080057131693,-0.136687676230652));
#68851=CARTESIAN_POINT('Ctrl Pts',(-2.74161303748949,2.76567963581706,-0.0706986564791052));
#68852=CARTESIAN_POINT('Ctrl Pts',(-4.33433259795114,0.50653088186967,0.0612793830239882));
#68853=CARTESIAN_POINT('Ctrl Pts',(-2.78179468292849,-3.3675915563884,0.259246442278628));
#68854=CARTESIAN_POINT('Ctrl Pts',(1.30897415722437,-4.16295078325229,0.457213501533269));
#68855=CARTESIAN_POINT('Ctrl Pts',(4.20522374878569,-1.17043504950046,0.655180560787908));
#68856=CARTESIAN_POINT('Ctrl Pts',(3.27086098885305,2.89120078059689,0.85314762004255));
#68857=CARTESIAN_POINT('Ctrl Pts',(-0.644239794664744,4.3171296103699,1.05111467929719));
#68858=CARTESIAN_POINT('Ctrl Pts',(-3.97208049260598,1.81025003261615,1.24908173855183));
#68859=CARTESIAN_POINT('Ctrl Pts',(-3.6809100787377,-2.3464149199974,1.44704879780647));
#68860=CARTESIAN_POINT('Ctrl Pts',(-0.0358182482239465,-4.3649518136884,
1.64501585706111));
#68861=CARTESIAN_POINT('Ctrl Pts',(3.64187171915626,-2.4064809479076,1.84298291631575));
#68862=CARTESIAN_POINT('Ctrl Pts',(4.00130141286111,1.74470191979564,2.04094997557039));
#68863=CARTESIAN_POINT('Ctrl Pts',(0.714947725952447,4.3061766697331,2.23891703482503));
#68864=CARTESIAN_POINT('Ctrl Pts',(-3.22282296004714,2.94410705447044,2.43688409407967));
#68865=CARTESIAN_POINT('Ctrl Pts',(-4.22413150189404,-1.10048417017061,
2.63485115333431));
#68866=CARTESIAN_POINT('Ctrl Pts',(-1.37663452391658,-4.14236865838933,
2.83281821258895));
#68867=CARTESIAN_POINT('Ctrl Pts',(2.72517788072432,-3.4099491719533,3.03078527184359));
#68868=CARTESIAN_POINT('Ctrl Pts',(4.34395347972042,0.429435826447155,3.22875233109823));
#68869=CARTESIAN_POINT('Ctrl Pts',(2.00474939782781,3.87754114959299,3.42671939035288));
#68870=CARTESIAN_POINT('Ctrl Pts',(-2.16107564708849,3.79263742337901,3.62468644960751));
#68871=CARTESIAN_POINT('Ctrl Pts',(-4.3578435093316,0.252083947495701,3.82265350886216));
#68872=CARTESIAN_POINT('Ctrl Pts',(-2.58397601329671,-3.51815493688139,
4.02062056811679));
#68873=CARTESIAN_POINT('Ctrl Pts',(1.54427303782037,-4.08283812273295,4.21858762737144));
#68874=CARTESIAN_POINT('Ctrl Pts',(4.26546260364518,-0.927456245588602,
4.41655468662607));
#68875=CARTESIAN_POINT('Ctrl Pts',(3.10018940675568,3.07297444409173,4.61452174588072));
#68876=CARTESIAN_POINT('Ctrl Pts',(-0.889811559104096,4.27347419590019,
4.81248880513536));
#68877=CARTESIAN_POINT('Ctrl Pts',(-4.06906353877317,1.58021144908221,5.01045586439));
#68878=CARTESIAN_POINT('Ctrl Pts',(-3.54080114607145,-2.55285595922618,
5.20842292364463));
#68879=CARTESIAN_POINT('Ctrl Pts',(0.213651010007477,-4.35989673656813,
5.40638998289928));
#68880=CARTESIAN_POINT('Ctrl Pts',(3.77343572432226,-2.19443139350223,5.60435704215391));
#68881=CARTESIAN_POINT('Ctrl Pts',(3.89506641477059,1.97048317190964,5.80232410140856));
#68882=CARTESIAN_POINT('Ctrl Pts',(0.467719662634615,4.33999822855348,6.0002911606632));
#68883=CARTESIAN_POINT('Ctrl Pts',(-3.385788380606,2.75513762781778,6.19825821991784));
#68884=CARTESIAN_POINT('Ctrl Pts',(-4.15434605104423,-1.3400579071959,6.39622527917248));
#68885=CARTESIAN_POINT('Ctrl Pts',(-1.13768445844283,-4.21426391906537,
6.59419233842712));
#68886=CARTESIAN_POINT('Ctrl Pts',(2.9155747296568,-3.24865669196893,6.79215939768177));
#68887=CARTESIAN_POINT('Ctrl Pts',(4.31231722560926,0.676953803596954,6.99012645693639));
#68888=CARTESIAN_POINT('Ctrl Pts',(1.77990552251878,3.98575998241297,7.18809351619104));
#68889=CARTESIAN_POINT('Ctrl Pts',(-2.3742614670743,3.66295356132985,7.38606057544568));
#68890=CARTESIAN_POINT('Ctrl Pts',(-4.36512763139796,0.00265858979218909,
7.58402763470032));
#68891=CARTESIAN_POINT('Ctrl Pts',(-2.37872156249766,-3.66005874742512,
7.78199469395497));
#68892=CARTESIAN_POINT('Ctrl Pts',(1.77504913350835,-3.98792513471919,7.97996175320959));
#68893=CARTESIAN_POINT('Ctrl Pts',(4.31148942649693,-0.682206150440716,
8.17792881246424));
#68894=CARTESIAN_POINT('Ctrl Pts',(2.9195297669843,3.24510280980227,8.37589587171889));
#68895=CARTESIAN_POINT('Ctrl Pts',(-1.1325502044238,4.21564661006512,8.57386293097352));
#68896=CARTESIAN_POINT('Ctrl Pts',(-4.15271063964539,1.34511733684088,8.77182999022817));
#68897=CARTESIAN_POINT('Ctrl Pts',(-3.38914191174368,-2.75101134286219,
8.9697970494828));
#68898=CARTESIAN_POINT('Ctrl Pts',(0.462432748235978,-4.34056473973755,
9.16776410873744));
#68899=CARTESIAN_POINT('Ctrl Pts',(3.89266327246501,-1.97522630442588,9.36573116799208));
#68900=CARTESIAN_POINT('Ctrl Pts',(3.77610596957432,2.1898333299681,9.56369822724672));
#68901=CARTESIAN_POINT('Ctrl Pts',(0.218961657389264,4.35963325281924,9.76166528650137));
#68902=CARTESIAN_POINT('Ctrl Pts',(-3.53768887628882,2.55716712810804,9.95963234575601));
#68903=CARTESIAN_POINT('Ctrl Pts',(-4.07098538103943,-1.57525373634129,
10.1575994050106));
#68904=CARTESIAN_POINT('Ctrl Pts',(-0.895016433525613,-4.27238714189304,
10.3555664642653));
#68905=CARTESIAN_POINT('Ctrl Pts',(3.09644390620682,-3.07674851786892,10.5535335235199));
#68906=CARTESIAN_POINT('Ctrl Pts',(4.26658917572028,0.922259785592155,10.7515005827746));
#68907=CARTESIAN_POINT('Ctrl Pts',(1.54924521419557,4.08095400277755,10.9494676420292));
#68908=CARTESIAN_POINT('Ctrl Pts',(-2.57968862354588,3.52129988953538,11.1474347012839));
#68909=CARTESIAN_POINT('Ctrl Pts',(-4.35814733222285,-0.246775479196811,
11.3454017605385));
#68910=CARTESIAN_POINT('Ctrl Pts',(-2.16569388518849,-3.79000215067897,
11.5433688197931));
#68911=CARTESIAN_POINT('Ctrl Pts',(2.00002469463763,-3.87998035141077,11.7413358790478));
#68912=CARTESIAN_POINT('Ctrl Pts',(4.34342710058424,-0.434726728421767,
11.9393029383024));
#68913=CARTESIAN_POINT('Ctrl Pts',(2.72932964331282,3.40662677800604,12.1372699975571));
#68914=CARTESIAN_POINT('Ctrl Pts',(-1.37158788482718,4.14404307177052,12.3352370568117));
#68915=CARTESIAN_POINT('Ctrl Pts',(-4.22278745042444,1.10562762946293,12.5332041160663));
#68916=CARTESIAN_POINT('Ctrl Pts',(-3.22640758842968,-2.94017693001924,
12.731171175321));
#68917=CARTESIAN_POINT('Ctrl Pts',(0.709703341729812,-4.30704858031942,
12.9291382345756));
#68918=CARTESIAN_POINT('Ctrl Pts',(3.9991703170631,-1.74956654106536,13.1271052938302));
#68919=CARTESIAN_POINT('Ctrl Pts',(3.64480590850277,2.40202751771026,13.3250723530849));
#68920=CARTESIAN_POINT('Ctrl Pts',(-0.0305118740455286,4.36502180201155,
13.5230394123395));
#68921=CARTESIAN_POINT('Ctrl Pts',(-3.67802885907486,2.35084027919942,13.7210064715942));
#68922=CARTESIAN_POINT('Ctrl Pts',(-3.97432148379599,-1.80530192763748,
13.9189735308488));
#68923=CARTESIAN_POINT('Ctrl Pts',(-0.649423660450986,-4.31654899378432,
14.1169405901034));
#68924=CARTESIAN_POINT('Ctrl Pts',(3.26719447680457,-2.89478609870085,14.3149076493581));
#68925=CARTESIAN_POINT('Ctrl Pts',(4.20691870157299,1.16455199319278,14.5128747086127));
#68926=CARTESIAN_POINT('Ctrl Pts',(1.31352225906811,4.16281222029371,14.7108417678674));
#68927=CARTESIAN_POINT('Ctrl Pts',(-2.77668583474704,3.36813926101774,14.908808827122));
#68928=CARTESIAN_POINT('Ctrl Pts',(-4.33692541366922,-0.495403131564479,
15.1067758863766));
#68929=CARTESIAN_POINT('Ctrl Pts',(-1.94558912083935,-3.90756052792091,
15.3047429456313));
#68930=CARTESIAN_POINT('Ctrl Pts',(2.21846454499872,-3.75935650997316,15.5027100048859));
#68931=CARTESIAN_POINT('Ctrl Pts',(4.36117125828737,-0.185826699863394,
15.7006770641406));
#68932=CARTESIAN_POINT('Ctrl Pts',(2.53021057519652,3.55701852000488,15.8986441233952));
#68933=CARTESIAN_POINT('Ctrl Pts',(-1.60614346971826,4.05889756721887,16.0966111826499));
#68934=CARTESIAN_POINT('Ctrl Pts',(-4.27906497288195,0.862524935493907,
16.2945782419045));
#68935=CARTESIAN_POINT('Ctrl Pts',(-3.05312996188807,-3.11973456279783,
16.4925453011591));
#68936=CARTESIAN_POINT('Ctrl Pts',(0.954654755972941,-4.25945778279257,
16.6905123604138));
#68937=CARTESIAN_POINT('Ctrl Pts',(4.0926088127702,-1.51818951785662,16.8884794196684));
#68938=CARTESIAN_POINT('Ctrl Pts',(3.50159529588251,2.60637232381472,17.0864464789231));
#68939=CARTESIAN_POINT('Ctrl Pts',(-0.279885698319549,4.35614626732967,
17.2844135381777));
#68940=CARTESIAN_POINT('Ctrl Pts',(-3.8063497238548,2.13683131908076,17.4823805974323));
#68941=CARTESIAN_POINT('Ctrl Pts',(-3.86467023905251,-2.02945072615123,
17.680347656687));
#68942=CARTESIAN_POINT('Ctrl Pts',(-0.401708690974452,-4.34660516197292,
17.8783147159416));
#68943=CARTESIAN_POINT('Ctrl Pts',(3.42726846016761,-2.70336405399536,18.0762817751962));
#68944=CARTESIAN_POINT('Ctrl Pts',(4.13350079524027,1.4030386602806,18.2742488344509));
#68945=CARTESIAN_POINT('Ctrl Pts',(1.07350695615322,4.23106713744709,18.4722158937055));
#68946=CARTESIAN_POINT('Ctrl Pts',(-2.96460935022899,3.20397217638182,18.6701829529602));
#68947=CARTESIAN_POINT('Ctrl Pts',(-4.30153122504168,-0.742411898130265,
18.8681500122148));
#68948=CARTESIAN_POINT('Ctrl Pts',(-1.71912653110853,-4.0123497201182,19.0661170714695));
#68949=CARTESIAN_POINT('Ctrl Pts',(2.42965486356431,-3.62644778680905,19.2640841307241));
#68950=CARTESIAN_POINT('Ctrl Pts',(4.36466391498096,0.0636805759787443,
19.4620511899788));
#68951=CARTESIAN_POINT('Ctrl Pts',(2.32282324692002,3.69578658340303,19.6600182492334));
#68952=CARTESIAN_POINT('Ctrl Pts',(-1.83545047483007,3.96048833617019,19.857985308488));
#68953=CARTESIAN_POINT('Ctrl Pts',(-4.32135930248387,0.616603669572335,
20.0559523677426));
#68954=CARTESIAN_POINT('Ctrl Pts',(-2.86987527135214,-3.28909748006584,
20.2539194269973));
#68955=CARTESIAN_POINT('Ctrl Pts',(1.19648653505093,-4.19794786508072,20.4518864862519));
#68956=CARTESIAN_POINT('Ctrl Pts',(4.17267341986514,-1.28185133211493,20.6498535455066));
#68957=CARTESIAN_POINT('Ctrl Pts',(3.34694211750671,2.80219998725174,20.8478206047612));
#68958=CARTESIAN_POINT('Ctrl Pts',(-0.52834490790043,4.33303565237925,21.0457876640159));
#68959=CARTESIAN_POINT('Ctrl Pts',(-3.92223214177738,1.91583958944961,21.2437547232705));
#68960=CARTESIAN_POINT('Ctrl Pts',(-3.74238996679523,-2.24696765506856,
21.4417217825251));
#68961=CARTESIAN_POINT('Ctrl Pts',(-0.152681011797728,-4.36245742846052,
21.6396888417798));
#68962=CARTESIAN_POINT('Ctrl Pts',(3.57614276412638,-2.50310791558824,21.8376559010344));
#68963=CARTESIAN_POINT('Ctrl Pts',(4.04657537286026,1.6369404565392,22.0356229602891));
#68964=CARTESIAN_POINT('Ctrl Pts',(0.829983631066443,4.28549570979318,22.2335900195437));
#68965=CARTESIAN_POINT('Ctrl Pts',(-3.14284507070233,3.02933510329512,22.4315570787983));
#68966=CARTESIAN_POINT('Ctrl Pts',(-4.25208042800194,-0.986994599932894,
22.629524138053));
#68967=CARTESIAN_POINT('Ctrl Pts',(-1.48704615385173,-4.10402729557307,
22.8274911973076));
#68968=CARTESIAN_POINT('Ctrl Pts',(2.63290551943605,-3.48168850304234,23.0254582565623));
#68969=CARTESIAN_POINT('Ctrl Pts',(4.35389365730897,0.312979755477227,23.2234253158169));
#68970=CARTESIAN_POINT('Ctrl Pts',(2.1078453619128,3.82247749983655,23.4213923750715));
#68971=CARTESIAN_POINT('Ctrl Pts',(-2.0587595672836,3.84913696178925,23.6193594343262));
#68972=CARTESIAN_POINT('Ctrl Pts',(-4.34953222918403,0.368667456908485,
23.8173264935808));
#68973=CARTESIAN_POINT('Ctrl Pts',(-2.67724235925495,-3.44771223513577,
24.0152935528355));
#68974=CARTESIAN_POINT('Ctrl Pts',(1.43440841744006,-4.12271983021779,24.2132606120901));
#68975=CARTESIAN_POINT('Ctrl Pts',(4.23910250202112,-1.04132429331712,24.4112276713448));
#68976=CARTESIAN_POINT('Ctrl Pts',(3.1813517513569,2.98887057943837,24.6091947305994));
#68977=CARTESIAN_POINT('Ctrl Pts',(-0.7750775840474,4.29576547837532,24.807161789854));
#68978=CARTESIAN_POINT('Ctrl Pts',(-4.02529743053493,1.68858725040281,25.0051288491087));
#68979=CARTESIAN_POINT('Ctrl Pts',(-3.60788025633637,-2.45714190929875,
25.2030959083633));
#68980=CARTESIAN_POINT('Ctrl Pts',(0.0968456006849734,-4.36405399097236,
25.401062967618));
#68981=CARTESIAN_POINT('Ctrl Pts',(3.713330894992,-2.29467208349948,25.5990300268726));
#68982=CARTESIAN_POINT('Ctrl Pts',(3.9464264906352,1.86549303416197,25.7969970861273));
#68983=CARTESIAN_POINT('Ctrl Pts',(0.583748072991018,4.32592007482491,25.9949641453819));
#68984=CARTESIAN_POINT('Ctrl Pts',(-3.31081055479986,2.8447987234108,26.1929312046365));
#68985=CARTESIAN_POINT('Ctrl Pts',(-4.18873461860814,-1.22835198594205,
26.3908982638912));
#68986=CARTESIAN_POINT('Ctrl Pts',(-1.2501063848151,-4.18229366892601,26.5888653231458));
#68987=CARTESIAN_POINT('Ctrl Pts',(2.82755232706474,-3.32555170523698,26.7868323824005));
#68988=CARTESIAN_POINT('Ctrl Pts',(4.32889568048136,0.561256175025024,26.984799441655));
#68989=CARTESIAN_POINT('Ctrl Pts',(1.88597942813973,3.93667726682387,27.1827665009098));
#68990=CARTESIAN_POINT('Ctrl Pts',(-2.27534101426903,3.72520731977148,27.3807335601643));
#68991=CARTESIAN_POINT('Ctrl Pts',(-4.36349168906895,0.119526507185921,
27.578700619419));
#68992=CARTESIAN_POINT('Ctrl Pts',(-2.47586071432294,-3.59506050432623,
27.7766676786736));
#68993=CARTESIAN_POINT('Ctrl Pts',(1.66764291843593,-4.03401950950716,27.9746347379283));
#68994=CARTESIAN_POINT('Ctrl Pts',(4.2916789812846,-0.797394399336888,28.1726017971829));
#68995=CARTESIAN_POINT('Ctrl Pts',(3.0053653161213,3.16577409540686,28.3705688564375));
#68996=CARTESIAN_POINT('Ctrl Pts',(-1.01927745001176,4.24445753735287,28.5685359156922));
#68997=CARTESIAN_POINT('Ctrl Pts',(-4.11520879182729,1.45581692055054,28.7665029749468));
#68998=CARTESIAN_POINT('Ctrl Pts',(-3.4615806605301,-2.65928667825375,28.9644700342015));
#68999=CARTESIAN_POINT('Ctrl Pts',(0.346055739657655,-4.35138963223751,
29.1624370934562));
#69000=CARTESIAN_POINT('Ctrl Pts',(3.83838454732779,-2.07873768747504,29.3604041527107));
#69001=CARTESIAN_POINT('Ctrl Pts',(3.83338141658813,2.08794952559938,29.5583712119654));
#69002=CARTESIAN_POINT('Ctrl Pts',(0.335604934185799,4.35220813319449,29.75633827122));
#69003=CARTESIAN_POINT('Ctrl Pts',(-3.4679569223873,2.65096606748557,29.9543053304747));
#69004=CARTESIAN_POINT('Ctrl Pts',(-4.11170079924854,-1.46569534486288,
30.1522723897293));
#69005=CARTESIAN_POINT('Ctrl Pts',(-1.00908149933844,-4.24689308014541,
30.350239448984));
#69006=CARTESIAN_POINT('Ctrl Pts',(3.01295921668583,-3.1585476195685,30.5482065082386));
#69007=CARTESIAN_POINT('Ctrl Pts',(4.28975167326265,0.80769851320537,30.7461735674933));
#69008=CARTESIAN_POINT('Ctrl Pts',(1.65795046243508,4.03801270064934,30.9441406267478));
#69009=CARTESIAN_POINT('Ctrl Pts',(-2.48448706767751,3.58910438926444,31.1421076860026));
#69010=CARTESIAN_POINT('Ctrl Pts',(-4.36319206520576,-0.130005033053983,
31.3400747452571));
#69011=CARTESIAN_POINT('Ctrl Pts',(-2.26638841452324,-3.73066078074767,
31.5380418045118));
#69012=CARTESIAN_POINT('Ctrl Pts',(1.89542787082935,-3.93213675919053,31.7360088637665));
#69013=CARTESIAN_POINT('Ctrl Pts',(4.3302310474462,-0.550858767949419,31.9339759230211));
#69014=CARTESIAN_POINT('Ctrl Pts',(2.81955790291901,3.33233244718791,32.1319429822757));
#69015=CARTESIAN_POINT('Ctrl Pts',(-1.26014650579978,4.17927949417292,32.3299100415304));
#69016=CARTESIAN_POINT('Ctrl Pts',(-4.19167241195597,1.21828925027683,32.527877100785));
#69017=CARTESIAN_POINT('Ctrl Pts',(-3.30396925939567,-2.8527413902185,32.7258441600396));
#69018=CARTESIAN_POINT('Ctrl Pts',(0.594135032481799,-4.32450573703732,
32.9238112192943));
#69019=CARTESIAN_POINT('Ctrl Pts',(3.95089506892724,-1.85601036118186,33.1217782785489));
#69020=CARTESIAN_POINT('Ctrl Pts',(3.70780956111402,2.30358298418572,33.3197453378036));
#69021=CARTESIAN_POINT('Ctrl Pts',(0.0863651005263536,4.3642739803862,33.5177123970582));
#69022=CARTESIAN_POINT('Ctrl Pts',(-3.61377064819352,2.44847054479303,33.7156794563129));
#69023=CARTESIAN_POINT('Ctrl Pts',(-4.02123070221231,-1.69824908251039,
33.9136465155675));
#69024=CARTESIAN_POINT('Ctrl Pts',(-0.764759122135802,-4.2976144302814,
34.1116135748221));
#69025=CARTESIAN_POINT('Ctrl Pts',(3.18852031281941,-2.98122198454221,34.3095806340768));
#69026=CARTESIAN_POINT('Ctrl Pts',(4.23658955113988,1.05150144212309,34.5075476933314));
#69027=CARTESIAN_POINT('Ctrl Pts',(1.42450362106763,4.12615265570029,34.705514752586));
#69028=CARTESIAN_POINT('Ctrl Pts',(-2.68551427648209,3.44127292977391,34.9034818118407));
#69029=CARTESIAN_POINT('Ctrl Pts',(-4.34863433749239,-0.37911174147221,
35.1014488710953));
#69030=CARTESIAN_POINT('Ctrl Pts',(-2.04950997508928,-3.85406994666813,
35.29941593035));
#69031=CARTESIAN_POINT('Ctrl Pts',(2.1170189126629,-3.81740451537487,35.4973829896046));
#69032=CARTESIAN_POINT('Ctrl Pts',(4.3546327249666,-0.302523027934251,35.6953500488593));
#69033=CARTESIAN_POINT('Ctrl Pts',(2.62453668551897,3.48800134512025,35.8933171081139));
#69034=CARTESIAN_POINT('Ctrl Pts',(-1.49689761581866,4.10044435350182,36.0912841673685));
#69035=CARTESIAN_POINT('Ctrl Pts',(-4.25443846035722,0.976780407608266,
36.2892512266232));
#69036=CARTESIAN_POINT('Ctrl Pts',(-3.1355610243575,-3.03687381651065,36.4872182858778));
#69037=CARTESIAN_POINT('Ctrl Pts',(0.840272661313841,-4.28349026118421,
36.6851853451324));
#69038=CARTESIAN_POINT('Ctrl Pts',(4.05049506524201,-1.62721773691917,36.8831524043871));
#69039=CARTESIAN_POINT('Ctrl Pts',(3.5701207550549,2.51168837811768,37.0811194636417));
#69040=CARTESIAN_POINT('Ctrl Pts',(-0.163155973376139,4.36207891749352,
37.2790865228964));
#69041=CARTESIAN_POINT('Ctrl Pts',(-3.7477771245128,2.23797247636521,37.477053582151));
#69042=CARTESIAN_POINT('Ctrl Pts',(-3.91761636107874,-1.92525058348425,
37.6750206414057));
#69043=CARTESIAN_POINT('Ctrl Pts',(-0.51794455321368,-4.3342970854914,37.8729877006603));
#69044=CARTESIAN_POINT('Ctrl Pts',(3.35367511613573,-2.79414448209901,38.0709547599149));
#69045=CARTESIAN_POINT('Ctrl Pts',(4.16955777758475,1.29184953539883,38.2689218191696));
#69046=CARTESIAN_POINT('Ctrl Pts',(1.18645009879805,4.20084493258216,38.4668888784242));
#69047=CARTESIAN_POINT('Ctrl Pts',(-2.87785820354561,3.28212747781266,38.6648559376789));
#69048=CARTESIAN_POINT('Ctrl Pts',(-4.31968911461486,-0.626848417753602,
38.8628229969335));
#69049=CARTESIAN_POINT('Ctrl Pts',(-1.82627277650346,-3.96513572377127,
39.0607900561882));
#69050=CARTESIAN_POINT('Ctrl Pts',(2.33234045599844,-3.68971719509276,39.2587571154427));
#69051=CARTESIAN_POINT('Ctrl Pts',(4.36355858955962,-0.0541202692408854,
39.4567241746975));
#69052=CARTESIAN_POINT('Ctrl Pts',(2.42336532659467,3.63405490361473,39.654691233952));
#69053=CARTESIAN_POINT('Ctrl Pts',(-1.73378242135946,4.00462371757127,39.8526582932068));
#69054=CARTESIAN_POINT('Ctrl Pts',(-3.43827766918834,1.82857118124135,39.9846363327098));
#69055=CARTESIAN_POINT('Ctrl Pts',(-3.64389712141114,0.619901468841313,
40.0506253524613));
#69056=CARTESIAN_POINT('Ctrl Pts',(-1.74869447533093,3.52286199445097,-8.32667268468867E-15));
#69057=CARTESIAN_POINT('Ctrl Pts',(-2.91721720025602,2.94282529798265,0.0659890197515384));
#69058=CARTESIAN_POINT('Ctrl Pts',(-4.61195268386658,0.53897489574385,0.197967059254632));
#69059=CARTESIAN_POINT('Ctrl Pts',(-2.95997253647821,-3.5832905218196,0.395934118509272));
#69060=CARTESIAN_POINT('Ctrl Pts',(1.39281578907369,-4.42959362341053,0.593901177763913));
#69061=CARTESIAN_POINT('Ctrl Pts',(4.47457423171435,-1.24540305706733,0.791868237018553));
#69062=CARTESIAN_POINT('Ctrl Pts',(3.48036422567708,3.07638624824828,0.989835296273193));
#69063=CARTESIAN_POINT('Ctrl Pts',(-0.685504257671056,4.59364782078722,
1.18780235552783));
#69064=CARTESIAN_POINT('Ctrl Pts',(-4.22649782277157,1.92619908779956,1.38576941478248));
#69065=CARTESIAN_POINT('Ctrl Pts',(-3.91667753525201,-2.49670608869799,
1.58373647403711));
#69066=CARTESIAN_POINT('Ctrl Pts',(-0.0381124572917341,-4.64453310334433,
1.78170353329176));
#69067=CARTESIAN_POINT('Ctrl Pts',(3.87513871395109,-2.56061942999538,1.9796705925464));
#69068=CARTESIAN_POINT('Ctrl Pts',(4.25759038397908,1.85645252635955,2.17763765180103));
#69069=CARTESIAN_POINT('Ctrl Pts',(0.76074113119263,4.58199332893075,2.37560471105568));
#69070=CARTESIAN_POINT('Ctrl Pts',(-3.42924929370728,3.13268124321463,2.57357177031031));
#69071=CARTESIAN_POINT('Ctrl Pts',(-4.49469305294534,-1.17097172574399,
2.77153882956496));
#69072=CARTESIAN_POINT('Ctrl Pts',(-1.46480989721034,-4.40769318456417,
2.9695058888196));
#69073=CARTESIAN_POINT('Ctrl Pts',(2.89972934863413,-3.62836120210814,3.16747294807423));
#69074=CARTESIAN_POINT('Ctrl Pts',(4.6221897966156,0.456941793822625,3.36544000732888));
#69075=CARTESIAN_POINT('Ctrl Pts',(2.13315641032305,4.12590310215742,3.56340706658351));
#69076=CARTESIAN_POINT('Ctrl Pts',(-2.29949557524497,4.03556117312128,3.76137412583816));
#69077=CARTESIAN_POINT('Ctrl Pts',(-4.63696950211734,0.268230278119817,
3.9593411850928));
#69078=CARTESIAN_POINT('Ctrl Pts',(-2.74948330342801,-3.74349769814126,
4.15730824434744));
#69079=CARTESIAN_POINT('Ctrl Pts',(1.64318589320195,-4.34434963455086,4.35527530360208));
#69080=CARTESIAN_POINT('Ctrl Pts',(4.53867146976977,-0.986861119756444,
4.55324236285672));
#69081=CARTESIAN_POINT('Ctrl Pts',(3.29876088921743,3.26980277000011,4.75120942211136));
#69082=CARTESIAN_POINT('Ctrl Pts',(-0.946805238270306,4.54719621575256,
4.949176481366));
#69083=CARTESIAN_POINT('Ctrl Pts',(-4.32969276915656,1.68142621014276,5.14714354062063));
#69084=CARTESIAN_POINT('Ctrl Pts',(-3.76759442881268,-2.71636996621894,
5.34511059987529));
#69085=CARTESIAN_POINT('Ctrl Pts',(0.227335657046906,-4.63915424143996,
5.54307765912991));
#69086=CARTESIAN_POINT('Ctrl Pts',(4.01512957829139,-2.33498780402952,5.74104471838457));
#69087=CARTESIAN_POINT('Ctrl Pts',(4.14455088516541,2.09669538454401,5.9390117776392));
#69088=CARTESIAN_POINT('Ctrl Pts',(0.4976777634472,4.61798120606043,6.13697883689384));
#69089=CARTESIAN_POINT('Ctrl Pts',(-3.60265287816667,2.93160805957583,6.33494589614848));
#69090=CARTESIAN_POINT('Ctrl Pts',(-4.42043774602824,-1.42589049685537,
6.53291295540313));
#69091=CARTESIAN_POINT('Ctrl Pts',(-1.21055474468865,-4.48419343758787,
6.73088001465776));
#69092=CARTESIAN_POINT('Ctrl Pts',(3.10232138295309,-3.45673771241492,6.92884707391241));
#69093=CARTESIAN_POINT('Ctrl Pts',(4.58852719602873,0.720313644787832,7.12681413316704));
#69094=CARTESIAN_POINT('Ctrl Pts',(1.89391096924347,4.24105350309916,7.32478119242169));
#69095=CARTESIAN_POINT('Ctrl Pts',(-2.52633624619639,3.89757087770312,7.52274825167632));
#69096=CARTESIAN_POINT('Ctrl Pts',(-4.64472018242493,0.00282887619951857,
7.72071531093096));
#69097=CARTESIAN_POINT('Ctrl Pts',(-2.53108201699104,-3.89449064690514,
7.91868237018561));
#69098=CARTESIAN_POINT('Ctrl Pts',(1.88874352170134,-4.24335733644923,8.11664942944024));
#69099=CARTESIAN_POINT('Ctrl Pts',(4.58764637522149,-0.725902411818228,
8.31461648869489));
#69100=CARTESIAN_POINT('Ctrl Pts',(3.10652974597202,3.45295619910787,8.51258354794951));
#69101=CARTESIAN_POINT('Ctrl Pts',(-1.20509163449415,4.48566469188666,8.71055060720418));
#69102=CARTESIAN_POINT('Ctrl Pts',(-4.41869758423413,1.43127399006965,8.9085176664588));
#69103=CARTESIAN_POINT('Ctrl Pts',(-3.60622120768015,-2.92721748027788,
9.10648472571345));
#69104=CARTESIAN_POINT('Ctrl Pts',(0.492052214761531,-4.61858400308089,
9.30445178496808));
#69105=CARTESIAN_POINT('Ctrl Pts',(4.14199381822252,-2.10174232135456,9.50241884422273));
#69106=CARTESIAN_POINT('Ctrl Pts',(4.01797085649934,2.33009522807297,9.70038590347737));
#69107=CARTESIAN_POINT('Ctrl Pts',(0.232986458846607,4.63887388118718,9.89835296273201));
#69108=CARTESIAN_POINT('Ctrl Pts',(-3.76428281378263,2.72095727151808,10.0963200219866));
#69109=CARTESIAN_POINT('Ctrl Pts',(-4.33173770811715,-1.67615094894297,
10.2942870812413));
#69110=CARTESIAN_POINT('Ctrl Pts',(-0.952343492203188,-4.54603953441066,
10.4922541404959));
#69111=CARTESIAN_POINT('Ctrl Pts',(3.29477548410189,-3.27381857849937,10.6902211997506));
#69112=CARTESIAN_POINT('Ctrl Pts',(4.53987020036735,0.981331819204367,10.8881882590052));
#69113=CARTESIAN_POINT('Ctrl Pts',(1.64847654445207,4.34234483406809,11.0861553182599));
#69114=CARTESIAN_POINT('Ctrl Pts',(-2.7449213003466,3.74684408942645,11.2841223775145));
#69115=CARTESIAN_POINT('Ctrl Pts',(-4.63729278529116,-0.262581794976337,
11.4820894367692));
#69116=CARTESIAN_POINT('Ctrl Pts',(-2.30440961797664,-4.03275710750639,
11.6800564960238));
#69117=CARTESIAN_POINT('Ctrl Pts',(2.12812908326276,-4.12849853827486,11.8780235552784));
#69118=CARTESIAN_POINT('Ctrl Pts',(4.62162970215701,-0.462571585494106,
12.0759906145331));
#69119=CARTESIAN_POINT('Ctrl Pts',(2.90414703744313,3.62482600416581,12.2739576737877));
#69120=CARTESIAN_POINT('Ctrl Pts',(-1.45944001380466,4.40947484647234,12.4719247330423));
#69121=CARTESIAN_POINT('Ctrl Pts',(-4.49326291309284,1.17644463082245,12.669891792297));
#69122=CARTESIAN_POINT('Ctrl Pts',(-3.43306352256849,-3.12849938877669,
12.8678588515516));
#69123=CARTESIAN_POINT('Ctrl Pts',(0.755160836800423,-4.58292108661379,
13.0658259108062));
#69124=CARTESIAN_POINT('Ctrl Pts',(4.25532278850436,-1.86162873344873,13.2637929700609));
#69125=CARTESIAN_POINT('Ctrl Pts',(3.87826084224315,2.55588075134383,13.4617600293155));
#69126=CARTESIAN_POINT('Ctrl Pts',(-0.0324662024000749,4.6446075745178,
13.6597270885702));
#69127=CARTESIAN_POINT('Ctrl Pts',(-3.91361176942619,2.50141489836758,13.8576941478248));
#69128=CARTESIAN_POINT('Ctrl Pts',(-4.22888235259237,-1.9209340497527,14.0556612070795));
#69129=CARTESIAN_POINT('Ctrl Pts',(-0.691020157336088,-4.59303001489449,
14.2536282663341));
#69130=CARTESIAN_POINT('Ctrl Pts',(3.4764628683862,-3.08020121100853,14.4515953255888));
#69131=CARTESIAN_POINT('Ctrl Pts',(4.47637774860644,1.23914318274667,14.6495623848434));
#69132=CARTESIAN_POINT('Ctrl Pts',(1.39765520322344,4.42944618530002,14.847529444098));
#69133=CARTESIAN_POINT('Ctrl Pts',(-2.95453645940081,3.58387330769906,15.0454965033527));
#69134=CARTESIAN_POINT('Ctrl Pts',(-4.61471157307029,-0.527134397414488,
15.2434635626073));
#69135=CARTESIAN_POINT('Ctrl Pts',(-2.07020683456502,-4.15784526379792,
15.4414306218619));
#69136=CARTESIAN_POINT('Ctrl Pts',(2.36056031260876,-4.00014857050371,15.6393976811166));
#69137=CARTESIAN_POINT('Ctrl Pts',(4.64051039806405,-0.197729160787965,
15.8373647403712));
#69138=CARTESIAN_POINT('Ctrl Pts',(2.69227411356042,3.78485054830688,16.0353317996259));
#69139=CARTESIAN_POINT('Ctrl Pts',(-1.70901921309492,4.31887565285675,16.2332988588805));
#69140=CARTESIAN_POINT('Ctrl Pts',(-4.5531450898464,0.917770868122375,16.4312659181351));
#69141=CARTESIAN_POINT('Ctrl Pts',(-3.2486872208605,-3.3195579399348,16.6292329773898));
#69142=CARTESIAN_POINT('Ctrl Pts',(1.01580173290275,-4.53228203171407,16.8272000366444));
#69143=CARTESIAN_POINT('Ctrl Pts',(4.35474615099769,-1.61543168717751,17.0251670958991));
#69144=CARTESIAN_POINT('Ctrl Pts',(3.72587738889572,2.77331412906689,17.2231341551537));
#69145=CARTESIAN_POINT('Ctrl Pts',(-0.297812770102405,4.63516354938317,
17.4211012144083));
#69146=CARTESIAN_POINT('Ctrl Pts',(-4.05015176568713,2.27369836400256,17.619068273663));
#69147=CARTESIAN_POINT('Ctrl Pts',(-4.11220779173309,-2.15943989339276,
17.8170353329176));
#69148=CARTESIAN_POINT('Ctrl Pts',(-0.427438696409145,-4.62501132283787,
18.0150023921723));
#69149=CARTESIAN_POINT('Ctrl Pts',(3.64678981503939,-2.87651831568849,18.2129694514269));
#69150=CARTESIAN_POINT('Ctrl Pts',(4.39825732233478,1.49290525556546,18.4109365106816));
#69151=CARTESIAN_POINT('Ctrl Pts',(1.14226658330751,4.5020729256894,18.6089035699362));
#69152=CARTESIAN_POINT('Ctrl Pts',(-3.15449673979053,3.409191090892,18.8068706291908));
#69153=CARTESIAN_POINT('Ctrl Pts',(-4.57705033698718,-0.789964422143125,
19.0048376884455));
#69154=CARTESIAN_POINT('Ctrl Pts',(-1.82923899813315,-4.26934635082178,
19.2028047477001));
#69155=CARTESIAN_POINT('Ctrl Pts',(2.58527766747342,-3.85872685709026,19.4007718069548));
#69156=CARTESIAN_POINT('Ctrl Pts',(4.64422676432063,0.0677594062427062,
19.5987388662094));
#69157=CARTESIAN_POINT('Ctrl Pts',(2.47160333585018,3.93250690091964,19.796705925464));
#69158=CARTESIAN_POINT('Ctrl Pts',(-1.95301365370493,4.214163172447,19.9946729847187));
#69159=CARTESIAN_POINT('Ctrl Pts',(-4.59814843061727,0.656097999980467,
20.1926400439733));
#69160=CARTESIAN_POINT('Ctrl Pts',(-3.05369481020705,-3.49976878974612,
20.390607103228));
#69161=CARTESIAN_POINT('Ctrl Pts',(1.27312317682936,-4.46683231744671,20.5885741624826));
#69162=CARTESIAN_POINT('Ctrl Pts',(4.4399390085437,-1.36395570895038,20.7865412217372));
#69163=CARTESIAN_POINT('Ctrl Pts',(3.56131845739703,2.98168482918127,20.9845082809919));
#69164=CARTESIAN_POINT('Ctrl Pts',(-0.562186140756878,4.6105726671106,21.1824753402465));
#69165=CARTESIAN_POINT('Ctrl Pts',(-4.17345661511275,2.03855180393781,21.3804423995011));
#69166=CARTESIAN_POINT('Ctrl Pts',(-3.98209529642355,-2.39088908688126,
21.5784094587558));
#69167=CARTESIAN_POINT('Ctrl Pts',(-0.162460444883393,-4.64187894924185,
21.7763765180104));
#69168=CARTESIAN_POINT('Ctrl Pts',(3.80519972710427,-2.66343549056703,21.9743435772651));
#69169=CARTESIAN_POINT('Ctrl Pts',(4.30576420465589,1.74178879014377,22.1723106365197));
#69170=CARTESIAN_POINT('Ctrl Pts',(0.883145247476255,4.55998772448201,22.3702776957744));
#69171=CARTESIAN_POINT('Ctrl Pts',(-3.34414870830501,3.22336826817979,22.568244755029));
#69172=CARTESIAN_POINT('Ctrl Pts',(-4.52443214699536,-1.05021298925567,
22.7662118142837));
#69173=CARTESIAN_POINT('Ctrl Pts',(-1.58229354699997,-4.36689600364936,
22.9641788735382));
#69174=CARTESIAN_POINT('Ctrl Pts',(2.80154681310576,-3.70469553803595,23.1621459327929));
#69175=CARTESIAN_POINT('Ctrl Pts',(4.63276665652923,0.333026548066865,23.3601129920475));
#69176=CARTESIAN_POINT('Ctrl Pts',(2.24285581559766,4.06731254835503,23.5580800513022));
#69177=CARTESIAN_POINT('Ctrl Pts',(-2.19062600693313,4.09567958626095,23.7560471105568));
#69178=CARTESIAN_POINT('Ctrl Pts',(-4.62812587281185,0.392281124929548,
23.9540141698115));
#69179=CARTESIAN_POINT('Ctrl Pts',(-2.84872348973948,-3.66854304248606,
24.1519812290661));
#69180=CARTESIAN_POINT('Ctrl Pts',(1.52628428969684,-4.38678582137206,24.3499482883208));
#69181=CARTESIAN_POINT('Ctrl Pts',(4.51062296664163,-1.10802257575002,24.5479153475754));
#69182=CARTESIAN_POINT('Ctrl Pts',(3.38512179589761,3.18031193478019,24.74588240683));
#69183=CARTESIAN_POINT('Ctrl Pts',(-0.824722391087892,4.57091528615491,
24.9438494660847));
#69184=CARTESIAN_POINT('Ctrl Pts',(-4.28312338026216,1.7967436336379,25.1418165253393));
#69185=CARTESIAN_POINT('Ctrl Pts',(-3.83897005023221,-2.61452529706382,
25.3397835845939));
#69186=CARTESIAN_POINT('Ctrl Pts',(0.103048697326808,-4.64357777382328,
25.5377506438486));
#69187=CARTESIAN_POINT('Ctrl Pts',(3.95117495028843,-2.44164905090382,25.7357177031032));
#69188=CARTESIAN_POINT('Ctrl Pts',(4.19920064597042,1.98498048112526,25.9336847623579));
#69189=CARTESIAN_POINT('Ctrl Pts',(0.621137956326939,4.60300132682757,26.1316518216125));
#69190=CARTESIAN_POINT('Ctrl Pts',(-3.52287261739005,3.0270120741764,26.3296188808671));
#69191=CARTESIAN_POINT('Ctrl Pts',(-4.45702894960724,-1.30702965457161,
26.5275859401218));
#69192=CARTESIAN_POINT('Ctrl Pts',(-1.33017745322355,-4.45017544805846,
26.7255529993764));
#69193=CARTESIAN_POINT('Ctrl Pts',(3.00866102194002,-3.53855795920106,26.9235200586311));
#69194=CARTESIAN_POINT('Ctrl Pts',(4.60616752420241,0.597205420730102,27.1214871178857));
#69195=CARTESIAN_POINT('Ctrl Pts',(2.0067790573888,4.18882697069147,27.3194541771403));
#69196=CARTESIAN_POINT('Ctrl Pts',(-2.42107979955908,3.96381207674295,27.517421236395));
#69197=CARTESIAN_POINT('Ctrl Pts',(-4.64297945569379,0.127182347720528,
27.7153882956496));
#69198=CARTESIAN_POINT('Ctrl Pts',(-2.63444306782062,-3.82532917511402,
27.9133553549043));
#69199=CARTESIAN_POINT('Ctrl Pts',(1.77445778781432,-4.2924041206335,28.1113224141589));
#69200=CARTESIAN_POINT('Ctrl Pts',(4.56656704319037,-0.848468629717082,
28.3092894734136));
#69201=CARTESIAN_POINT('Ctrl Pts',(3.19786318249711,3.3685463692216,28.5072565326682));
#69202=CARTESIAN_POINT('Ctrl Pts',(-1.08456360118944,4.51632099950187,28.7052235919229));
#69203=CARTESIAN_POINT('Ctrl Pts',(-4.37879369043133,1.5490640374772,28.9031906511775));
#69204=CARTESIAN_POINT('Ctrl Pts',(-3.68329975999046,-2.82961772217035,
29.1011577104321));
#69205=CARTESIAN_POINT('Ctrl Pts',(0.368221095454519,-4.63010224513767,
29.2991247696868));
#69206=CARTESIAN_POINT('Ctrl Pts',(4.08423846456282,-2.21188375376102,29.4970918289414));
#69207=CARTESIAN_POINT('Ctrl Pts',(4.07891487627758,2.22168562304567,29.695058888196));
#69208=CARTESIAN_POINT('Ctrl Pts',(0.357100901224898,4.63097317222967,29.8930259474507));
#69209=CARTESIAN_POINT('Ctrl Pts',(-3.69008443036845,2.82076416460482,30.0909930067053));
#69210=CARTESIAN_POINT('Ctrl Pts',(-4.37506100600459,-1.55957518873072,
30.28896006596));
#69211=CARTESIAN_POINT('Ctrl Pts',(-1.07371458556588,-4.51891254222846,
30.4869271252146));
#69212=CARTESIAN_POINT('Ctrl Pts',(3.20594348305053,-3.36085702746372,30.6848941844692));
#69213=CARTESIAN_POINT('Ctrl Pts',(4.5645162883847,0.859432736540255,30.8828612437239));
#69214=CARTESIAN_POINT('Ctrl Pts',(1.76414451640364,4.29665308127263,31.0808283029785));
#69215=CARTESIAN_POINT('Ctrl Pts',(-2.64362195121429,3.81899156252335,31.2787953622332));
#69216=CARTESIAN_POINT('Ctrl Pts',(-4.64266064050165,-0.138332037876641,
31.4767624214878));
#69217=CARTESIAN_POINT('Ctrl Pts',(-2.41155377323495,-3.96961483954837,
31.6747294807425));
#69218=CARTESIAN_POINT('Ctrl Pts',(2.0168326860932,-4.1839956371718,31.8726965399971));
#69219=CARTESIAN_POINT('Ctrl Pts',(4.60758842329548,-0.586142045138947,
32.0706635992517));
#69220=CARTESIAN_POINT('Ctrl Pts',(3.00015454370789,3.54577301719043,32.2686306585064));
#69221=CARTESIAN_POINT('Ctrl Pts',(-1.34086065804823,4.44696821118217,32.466597717761));
#69222=CARTESIAN_POINT('Ctrl Pts',(-4.46015491274207,1.29632238656436,32.6645647770157));
#69223=CARTESIAN_POINT('Ctrl Pts',(-3.51559312741374,-3.03546347994035,
32.8625318362703));
#69224=CARTESIAN_POINT('Ctrl Pts',(0.632190215150794,-4.60149639871972,
33.0604988955249));
#69225=CARTESIAN_POINT('Ctrl Pts',(4.20395544297353,-1.97489042963221,33.2584659547796));
#69226=CARTESIAN_POINT('Ctrl Pts',(3.9452999672266,2.45113070728511,33.4564330140342));
#69227=CARTESIAN_POINT('Ctrl Pts',(0.0918969064240613,4.64381185386782,
33.6544000732888));
#69228=CARTESIAN_POINT('Ctrl Pts',(-3.84523772995475,2.6052985194916,33.8523671325435));
#69229=CARTESIAN_POINT('Ctrl Pts',(-4.27879617228297,-1.80702431965196,
34.0503341917981));
#69230=CARTESIAN_POINT('Ctrl Pts',(-0.813743017209305,-4.5728826660255,
34.2483012510528));
#69231=CARTESIAN_POINT('Ctrl Pts',(3.39274951378259,-3.17217343664643,34.4462683103074));
#69232=CARTESIAN_POINT('Ctrl Pts',(4.50794905772962,1.11885158522024,34.6442353695621));
#69233=CARTESIAN_POINT('Ctrl Pts',(1.51574507721577,4.39043852414456,34.8422024288167));
#69234=CARTESIAN_POINT('Ctrl Pts',(-2.85752523487432,3.66169129057847,35.0401694880713));
#69235=CARTESIAN_POINT('Ctrl Pts',(-4.62717046989721,-0.403394380577725,
35.238136547326));
#69236=CARTESIAN_POINT('Ctrl Pts',(-2.18078396537732,-4.10092853574456,
35.4361036065806));
#69237=CARTESIAN_POINT('Ctrl Pts',(2.25261694514802,-4.06191463211884,35.6340706658352));
#69238=CARTESIAN_POINT('Ctrl Pts',(4.63355306250759,-0.321900052449153,
35.8320377250899));
#69239=CARTESIAN_POINT('Ctrl Pts',(2.79264194363096,3.71141272650878,36.0300047843445));
#69240=CARTESIAN_POINT('Ctrl Pts',(-1.59277600893202,4.36308356910993,36.2279718435992));
#69241=CARTESIAN_POINT('Ctrl Pts',(-4.5269412146324,1.03934456357744,36.4259389028538));
#69242=CARTESIAN_POINT('Ctrl Pts',(-3.33639810856892,-3.23138984655706,
36.6239059621085));
#69243=CARTESIAN_POINT('Ctrl Pts',(0.894093304551245,-4.55785382407507,
36.8218730213631));
#69244=CARTESIAN_POINT('Ctrl Pts',(4.30993495883582,-1.73144331668662,37.0198400806178));
#69245=CARTESIAN_POINT('Ctrl Pts',(3.79879199990011,2.67256554376382,37.2178071398723));
#69246=CARTESIAN_POINT('Ctrl Pts',(-0.173606342452101,4.6414761941162,37.415774199127));
#69247=CARTESIAN_POINT('Ctrl Pts',(-3.98782750915358,2.38131775435758,37.6137412583816));
#69248=CARTESIAN_POINT('Ctrl Pts',(-4.16854518718231,-2.04856558534832,
37.8117083176363));
#69249=CARTESIAN_POINT('Ctrl Pts',(-0.55111962875595,-4.61191489678395,
38.0096753768909));
#69250=CARTESIAN_POINT('Ctrl Pts',(3.56848271403773,-2.97311335761792,38.2076424361456));
#69251=CARTESIAN_POINT('Ctrl Pts',(4.43662380500257,1.37459431118669,38.4056094954002));
#69252=CARTESIAN_POINT('Ctrl Pts',(1.26244389274874,4.46991494618754,38.6035765546549));
#69253=CARTESIAN_POINT('Ctrl Pts',(-3.06218906041124,3.4923523490665,38.8015436139095));
#69254=CARTESIAN_POINT('Ctrl Pts',(-4.59637126487122,-0.666998938660841,
38.9995106731641));
#69255=CARTESIAN_POINT('Ctrl Pts',(-1.94324811091996,-4.21910823174637,
39.1974777324188));
#69256=CARTESIAN_POINT('Ctrl Pts',(2.4817301355271,-3.92604875976996,39.3954447916734));
#69257=CARTESIAN_POINT('Ctrl Pts',(4.64305064125478,-0.0575867484407697,
39.5934118509281));
#69258=CARTESIAN_POINT('Ctrl Pts',(2.57858527683373,3.86682122040361,39.7913789101827));
#69259=CARTESIAN_POINT('Ctrl Pts',(-1.84483361872357,4.26112548696861,39.9893459694374));
#69260=CARTESIAN_POINT('Ctrl Pts',(-3.65850417934875,1.94569373170701,40.1213240089404));
#69261=CARTESIAN_POINT('Ctrl Pts',(-3.87729384606291,0.659607027920921,
40.187313028692));
#69262=CARTESIAN_POINT('Ctrl Pts',(-3.936306081373,-0.00286452337122285,
38.970836477965));
#69263=CARTESIAN_POINT('Ctrl Pts',(-3.93786941330146,-0.191350950945783,
38.9803945430314));
#69264=CARTESIAN_POINT('Ctrl Pts',(-3.92549888185612,-0.379633084980762,
38.9899526080978));
#69265=CARTESIAN_POINT('Ctrl Pts',(-3.89848703846934,-0.56579193955387,
38.9995106731641));
#69266=CARTESIAN_POINT('Ctrl Pts',(-3.83491032379214,-1.00394672271177,
39.0220071154428));
#69267=CARTESIAN_POINT('Ctrl Pts',(-3.69022485851434,-1.43033913477847,
39.0445035577214));
#69268=CARTESIAN_POINT('Ctrl Pts',(-3.48038110743657,-1.82358747408649,
39.0670000000001));
#69269=CARTESIAN_POINT('Ctrl Pts',(-1.87556985610737,-2.62720998907027,
-1.05818132034585E-16));
#69270=CARTESIAN_POINT('Ctrl Pts',(-1.9427166798522,-2.5898538427666,-1.35022482623698E-16));
#69271=CARTESIAN_POINT('Ctrl Pts',(-2.00831539040545,-2.5500067025529,-6.43752826549732E-16));
#69272=CARTESIAN_POINT('Ctrl Pts',(-2.07220966857289,-2.50769818664921,
-4.83987849797529E-16));
#69273=CARTESIAN_POINT('Ctrl Pts',(-2.15789934851274,-2.4509575317659,-2.74928550691976E-16));
#69274=CARTESIAN_POINT('Ctrl Pts',(-2.24052477232639,-2.38979204336152,
1.62088651626145E-16));
#69275=CARTESIAN_POINT('Ctrl Pts',(-2.31999371269407,-2.32459267939733,
2.08166817117217E-16));
#69276=CARTESIAN_POINT('Ctrl Pts',(-2.36987291826283,-2.2836698677545,2.37088082181609E-16));
#69277=CARTESIAN_POINT('Ctrl Pts',(-2.41850829062763,-2.24115685284336,
3.30045642536614E-16));
#69278=CARTESIAN_POINT('Ctrl Pts',(-2.46587282390372,-2.19714092437569,
2.84494650060196E-16));
#69279=CARTESIAN_POINT('Ctrl Pts',(-2.4883641183387,-2.17623973231232,2.62864524885711E-16));
#69280=CARTESIAN_POINT('Ctrl Pts',(-2.510568802024,-2.15499955403746,8.37311985777155E-16));
#69281=CARTESIAN_POINT('Ctrl Pts',(-2.5324836784513,-2.13342923122307,7.84095011141517E-16));
#69282=CARTESIAN_POINT('Ctrl Pts',(-2.54647144194973,-2.11966138840117,
7.50127835566776E-16));
#69283=CARTESIAN_POINT('Ctrl Pts',(-2.56034150716028,-2.10575853776106,
3.74260074904971E-16));
#69284=CARTESIAN_POINT('Ctrl Pts',(-2.57408203118947,-2.09173447001254,
3.95516952522712E-16));
#69285=CARTESIAN_POINT('Ctrl Pts',(-2.64826407279405,-2.0160216387569,5.10278120035181E-16));
#69286=CARTESIAN_POINT('Ctrl Pts',(-2.7187510730238,-1.93670300009748,2.04203257333887E-16));
#69287=CARTESIAN_POINT('Ctrl Pts',(-2.78544558437692,-1.85418677655769,
2.77555756156289E-16));
#69288=CARTESIAN_POINT('Ctrl Pts',(-2.84956847381101,-1.77485223206203,
3.48079912886359E-16));
#69289=CARTESIAN_POINT('Ctrl Pts',(-2.91018592724737,-1.69256114185943,
6.22909331617954E-16));
#69290=CARTESIAN_POINT('Ctrl Pts',(-2.96718958630348,-1.6076387700055,6.66133814775094E-16));
#69291=CARTESIAN_POINT('Ctrl Pts',(-2.99212868714053,-1.57048523231941,
6.85044526156343E-16));
#69292=CARTESIAN_POINT('Ctrl Pts',(-3.01637577769413,-1.53282762334849,
4.45074375543263E-16));
#69293=CARTESIAN_POINT('Ctrl Pts',(-3.03992022985205,-1.49469135800012,
5.68989300120393E-16));
#69294=CARTESIAN_POINT('Ctrl Pts',(-3.05141389032931,-1.47607443360345,
6.2948066605246E-16));
#69295=CARTESIAN_POINT('Ctrl Pts',(-3.06274009074011,-1.4573434260494,6.80345639867992E-16));
#69296=CARTESIAN_POINT('Ctrl Pts',(-3.07389750346823,-1.43850120933943,
7.21644966006352E-16));
#69297=CARTESIAN_POINT('Ctrl Pts',(-3.08183764567037,-1.42509219743621,
7.51035518312842E-16));
#69298=CARTESIAN_POINT('Ctrl Pts',(-3.08969120442884,-1.41162864596677,
2.83354860342952E-16));
#69299=CARTESIAN_POINT('Ctrl Pts',(-3.09745337754263,-1.39811946780493,
3.05311331771918E-16));
#69300=CARTESIAN_POINT('Ctrl Pts',(-3.15286735703586,-1.30167774837181,
4.62058088082708E-16));
#69301=CARTESIAN_POINT('Ctrl Pts',(-3.20369221394891,-1.20280340881569,
3.53144865346304E-16));
#69302=CARTESIAN_POINT('Ctrl Pts',(-3.24982252344817,-1.10192599424532,
2.91433543964104E-16));
#69303=CARTESIAN_POINT('Ctrl Pts',(-3.29668794246923,-0.999441047690232,
2.28738821853768E-16));
#69304=CARTESIAN_POINT('Ctrl Pts',(-3.33870858667038,-0.89488801034169,
4.07726271026068E-16));
#69305=CARTESIAN_POINT('Ctrl Pts',(-3.37574011869655,-0.788675562609922,
4.44089209850063E-16));
#69306=CARTESIAN_POINT('Ctrl Pts',(-3.41269905543875,-0.682671329941954,
4.8038086407617E-16));
#69307=CARTESIAN_POINT('Ctrl Pts',(-3.44468892653223,-0.575013374954663,
3.12016465250824E-16));
#69308=CARTESIAN_POINT('Ctrl Pts',(-3.47152479256147,-0.466078071083872,
3.60822483003176E-16));
#69309=CARTESIAN_POINT('Ctrl Pts',(-3.4892663919142,-0.394059284191032,
3.93088883946656E-16));
#69310=CARTESIAN_POINT('Ctrl Pts',(-3.50475445309811,-0.321481607985789,
4.80650587058393E-16));
#69311=CARTESIAN_POINT('Ctrl Pts',(-3.51792389739043,-0.248449242265856,
5.55111512312578E-16));
#69312=CARTESIAN_POINT('Ctrl Pts',(-3.5218708993275,-0.226560779657458,
5.77428127174312E-16));
#69313=CARTESIAN_POINT('Ctrl Pts',(-3.52560956225353,-0.204631457077295,
4.94393150946916E-16));
#69314=CARTESIAN_POINT('Ctrl Pts',(-3.52913795503785,-0.182664042150726,
4.9960036108132E-16));
#69315=CARTESIAN_POINT('Ctrl Pts',(-3.5316576994674,-0.166976369384047,
5.03319005668721E-16));
#69316=CARTESIAN_POINT('Ctrl Pts',(-3.53407007612331,-0.151269688065101,
5.28418406579064E-16));
#69317=CARTESIAN_POINT('Ctrl Pts',(-3.53637257048778,-0.13555860296056,
5.27355936696949E-16));
#69318=CARTESIAN_POINT('Ctrl Pts',(-3.55317264707207,-0.020923172337153,
5.19603659139405E-16));
#69319=CARTESIAN_POINT('Ctrl Pts',(-3.56415658297867,0.094128556090517,
-4.9767199959817E-17));
#69320=CARTESIAN_POINT('Ctrl Pts',(-3.56918101522632,0.209171118706935,
2.77555756156289E-17));
#69321=CARTESIAN_POINT('Ctrl Pts',(-3.57215568325829,0.277280989924882,
7.3652208486252E-17));
#69322=CARTESIAN_POINT('Ctrl Pts',(-3.57304069866554,0.345388280413459,
7.34761168187773E-16));
#69323=CARTESIAN_POINT('Ctrl Pts',(-3.57179877131075,0.41340886664328,6.38378239159465E-16));
#69324=CARTESIAN_POINT('Ctrl Pts',(-3.56977179011697,0.524426993867594,
4.8231769589789E-16));
#69325=CARTESIAN_POINT('Ctrl Pts',(-3.56208205365773,0.635213960545909,
-1.88046607578939E-16));
#69326=CARTESIAN_POINT('Ctrl Pts',(-3.54899330987584,0.745485199930978,
-1.94289029309402E-16));
#69327=CARTESIAN_POINT('Ctrl Pts',(-3.53565885377793,0.857826538790079,
-2.00648638749126E-16));
#69328=CARTESIAN_POINT('Ctrl Pts',(-3.51672067583019,0.969633285182107,
-2.00357306609628E-17));
#69329=CARTESIAN_POINT('Ctrl Pts',(-3.49240358880244,1.08060745715161,-1.94289029309402E-16));
#69330=CARTESIAN_POINT('Ctrl Pts',(-3.48412425558681,1.11839126517991,-2.53617727758628E-16));
#69331=CARTESIAN_POINT('Ctrl Pts',(-3.4752209384603,1.15607853650087,5.93380374341007E-16));
#69332=CARTESIAN_POINT('Ctrl Pts',(-3.46570115451279,1.19365736151579,6.66133814775094E-16));
#69333=CARTESIAN_POINT('Ctrl Pts',(-3.46167353792751,1.20955615708932,6.96914236362872E-16));
#69334=CARTESIAN_POINT('Ctrl Pts',(-3.45753549723059,1.22543555138734,-2.22777472105693E-16));
#69335=CARTESIAN_POINT('Ctrl Pts',(-3.4532915411,1.24128055545267,-2.22044604925031E-16));
#69336=CARTESIAN_POINT('Ctrl Pts',(-3.42380202789225,1.35138100001027,-2.16952211003276E-16));
#69337=CARTESIAN_POINT('Ctrl Pts',(-3.38916062108469,1.45999026507038,-2.84426430466537E-16));
#69338=CARTESIAN_POINT('Ctrl Pts',(-3.34966883438784,1.56681514734322,-2.22044604925031E-16));
#69339=CARTESIAN_POINT('Ctrl Pts',(-3.30890722121856,1.67707489733847,-1.57656942218446E-16));
#69340=CARTESIAN_POINT('Ctrl Pts',(-3.26297826095999,1.78543436725715,5.85977744875059E-16));
#69341=CARTESIAN_POINT('Ctrl Pts',(-3.21215817004056,1.89157452147116,6.66133814775094E-16));
#69342=CARTESIAN_POINT('Ctrl Pts',(-3.16086111688722,1.99871083378222,7.47042174123448E-16));
#69343=CARTESIAN_POINT('Ctrl Pts',(-3.10458042918179,2.10358677819699,2.69205069416314E-16));
#69344=CARTESIAN_POINT('Ctrl Pts',(-3.04354725425783,2.20586614535285,3.88578058618805E-16));
#69345=CARTESIAN_POINT('Ctrl Pts',(-3.00375166655634,2.27255557336927,4.66413076490916E-16));
#69346=CARTESIAN_POINT('Ctrl Pts',(-2.96193450734188,2.33814088750178,-9.37256318242688E-17));
#69347=CARTESIAN_POINT('Ctrl Pts',(-2.91814875486367,2.40252454053732,-1.11022302462516E-16));
#69348=CARTESIAN_POINT('Ctrl Pts',(-2.90371986817841,2.42374113226987,-1.16722140572999E-16));
#69349=CARTESIAN_POINT('Ctrl Pts',(-2.88907713976851,2.44482719670223,-2.28029434941039E-16));
#69350=CARTESIAN_POINT('Ctrl Pts',(-2.8742222712953,2.46577912801777,-2.22044604925031E-16));
#69351=CARTESIAN_POINT('Ctrl Pts',(-2.86397378277113,2.48023402730104,-2.17915624459887E-16));
#69352=CARTESIAN_POINT('Ctrl Pts',(-2.85362431940418,2.49462508162952,1.10039211875577E-16));
#69353=CARTESIAN_POINT('Ctrl Pts',(-2.84317441430392,2.50895108865281,1.11022302462516E-16));
#69354=CARTESIAN_POINT('Ctrl Pts',(-2.83348355348938,2.52223650500433,1.11933984813188E-16));
#69355=CARTESIAN_POINT('Ctrl Pts',(-2.82371242472869,2.53545759866695,6.11899018834777E-16));
#69356=CARTESIAN_POINT('Ctrl Pts',(-2.81386191454734,2.54861341598892,6.10622663543836E-16));
#69357=CARTESIAN_POINT('Ctrl Pts',(-2.74041062887734,2.64671104530441,6.0110539638047E-16));
#69358=CARTESIAN_POINT('Ctrl Pts',(-2.66254789228831,2.74118288830179,-5.41748258519085E-16));
#69359=CARTESIAN_POINT('Ctrl Pts',(-2.58056320353906,2.83169462033826,-4.9960036108132E-16));
#69360=CARTESIAN_POINT('Ctrl Pts',(-2.49844011931886,2.9223591420477,-4.57381315259579E-16));
#69361=CARTESIAN_POINT('Ctrl Pts',(-2.41218077165145,3.00905100116057,5.07174156750596E-17));
#69362=CARTESIAN_POINT('Ctrl Pts',(-2.32202629791708,3.09141791323186,-5.55111512312578E-17));
#69363=CARTESIAN_POINT('Ctrl Pts',(-2.23357416200924,3.17222953576213,-1.5973386196413E-16));
#69364=CARTESIAN_POINT('Ctrl Pts',(-2.14137210639717,3.24887870479941,2.73547190358871E-16));
#69365=CARTESIAN_POINT('Ctrl Pts',(-2.04560675719255,3.32100584191314,2.77555756156289E-16));
#69366=CARTESIAN_POINT('Ctrl Pts',(-1.95012832424157,3.39291688366318,2.8155231215381E-16));
#69367=CARTESIAN_POINT('Ctrl Pts',(-1.85110753907348,3.46033371771341,1.62536897696253E-16));
#69368=CARTESIAN_POINT('Ctrl Pts',(-1.74869447533108,3.5228619944509,1.66533453693773E-16));
#69369=CARTESIAN_POINT('Origin',(0.,0.,0.));
#69370=CARTESIAN_POINT('Origin',(-1.73205080756888,-3.,-8.));
#69371=CARTESIAN_POINT('',(-1.73205080756888,-3.,-8.));
#69372=CARTESIAN_POINT('',(1.73205080756888,-3.,-8.));
#69373=CARTESIAN_POINT('',(-0.86602540378444,-3.,-8.));
#69374=CARTESIAN_POINT('',(-1.73205080756888,-3.,-4.));
#69375=CARTESIAN_POINT('',(-1.73205080756888,-3.,-8.));
#69376=CARTESIAN_POINT('',(1.73205080756888,-3.,-4.));
#69377=CARTESIAN_POINT('',(-1.73205080756888,-3.,-4.));
#69378=CARTESIAN_POINT('',(1.73205080756888,-3.,-8.));
#69379=CARTESIAN_POINT('Origin',(-3.46410161513775,4.24230095489963E-16,
-8.));
#69380=CARTESIAN_POINT('',(-3.46410161513775,4.24230095489963E-16,-8.));
#69381=CARTESIAN_POINT('',(-3.03108891324554,-0.749999999999999,-8.));
#69382=CARTESIAN_POINT('',(-3.46410161513775,5.55111512312578E-16,-4.));
#69383=CARTESIAN_POINT('',(-3.46410161513775,4.24230095489963E-16,-8.));
#69384=CARTESIAN_POINT('',(-3.46410161513775,4.24230095489963E-16,-4.));
#69385=CARTESIAN_POINT('Origin',(-1.73205080756888,3.,-8.));
#69386=CARTESIAN_POINT('',(-1.73205080756888,3.,-8.));
#69387=CARTESIAN_POINT('',(-2.1650635094611,2.25,-8.));
#69388=CARTESIAN_POINT('',(-1.73205080756888,3.,-4.));
#69389=CARTESIAN_POINT('',(-1.73205080756888,3.,-8.));
#69390=CARTESIAN_POINT('',(-1.73205080756888,3.,-4.));
#69391=CARTESIAN_POINT('Origin',(1.73205080756888,3.,-8.));
#69392=CARTESIAN_POINT('',(1.73205080756888,3.,-8.));
#69393=CARTESIAN_POINT('',(0.866025403784439,3.,-8.));
#69394=CARTESIAN_POINT('',(1.73205080756888,3.,-4.));
#69395=CARTESIAN_POINT('',(1.73205080756888,3.,-8.));
#69396=CARTESIAN_POINT('',(1.73205080756888,3.,-4.));
#69397=CARTESIAN_POINT('Origin',(3.46410161513775,0.,-8.));
#69398=CARTESIAN_POINT('',(3.46410161513775,0.,-8.));
#69399=CARTESIAN_POINT('',(3.03108891324554,0.75,-8.));
#69400=CARTESIAN_POINT('',(3.46410161513775,0.,-4.));
#69401=CARTESIAN_POINT('',(3.46410161513775,0.,-8.));
#69402=CARTESIAN_POINT('',(3.46410161513775,0.,-4.));
#69403=CARTESIAN_POINT('Origin',(1.73205080756888,-3.,-8.));
#69404=CARTESIAN_POINT('',(2.1650635094611,-2.25,-8.));
#69405=CARTESIAN_POINT('',(1.73205080756888,-3.,-4.));
#69406=CARTESIAN_POINT('Origin',(0.,5.55111512312578E-16,-4.));
#69407=CARTESIAN_POINT('Origin',(0.,0.,0.));
#69408=CARTESIAN_POINT('',(-6.5,-7.9602041944578E-16,0.));
#69409=CARTESIAN_POINT('Origin',(0.,0.,0.));
#69410=CARTESIAN_POINT('Origin',(0.,0.,-8.));
#69411=CARTESIAN_POINT('',(-6.5,-7.9602041944578E-16,-8.));
#69412=CARTESIAN_POINT('',(-6.5,-7.9602041944578E-16,-8.));
#69413=CARTESIAN_POINT('Origin',(0.,0.,-8.));
#69414=CARTESIAN_POINT('Origin',(0.,0.,-8.));
#69415=CARTESIAN_POINT('Origin',(0.,0.,40.));
#69416=CARTESIAN_POINT('',(0.,0.,0.));
#69417=CARTESIAN_POINT('',(0.,0.,0.));
#69418=CARTESIAN_POINT('',(28.,0.,0.));
#69419=CARTESIAN_POINT('',(24.,0.,20.));
#69420=CARTESIAN_POINT('',(0.,0.,0.));
#69421=CARTESIAN_POINT('',(93.,0.,20.));
#69422=CARTESIAN_POINT('',(91.,0.,20.));
#69423=CARTESIAN_POINT('',(90.,0.,20.));
#69424=CARTESIAN_POINT('',(92.,-24.,42.));
#69425=CARTESIAN_POINT('',(92.,-24.,40.));
#69426=CARTESIAN_POINT('',(-46.,-46.,32.));
#69427=CARTESIAN_POINT('',(101.,0.,20.));
#69428=CARTESIAN_POINT('',(92.,24.,42.));
#69429=CARTESIAN_POINT('',(92.,24.,40.));
#69430=CARTESIAN_POINT('',(4.44089209850063E-15,28.,0.));
#69431=CARTESIAN_POINT('',(0.,0.,0.));
#69432=CARTESIAN_POINT('',(4.44089209850063E-15,24.,20.));
#69433=CARTESIAN_POINT('',(1.77635683940025E-14,90.,20.));
#69434=CARTESIAN_POINT('',(1.77635683940025E-14,93.,20.));
#69435=CARTESIAN_POINT('',(1.77635683940025E-14,91.,20.));
#69436=CARTESIAN_POINT('',(1.77635683940025E-14,101.,20.));
#69437=CARTESIAN_POINT('',(24.,92.,42.));
#69438=CARTESIAN_POINT('',(24.,92.,40.));
#69439=CARTESIAN_POINT('',(-24.,92.,42.));
#69440=CARTESIAN_POINT('',(-24.,92.,40.));
#69441=CARTESIAN_POINT('',(-28.,3.42901103761259E-15,0.));
#69442=CARTESIAN_POINT('',(0.,0.,0.));
#69443=CARTESIAN_POINT('',(-24.,3.12823556570922E-15,20.));
#69444=CARTESIAN_POINT('',(-90.,1.10218211923262E-14,20.));
#69445=CARTESIAN_POINT('',(-93.,1.13892152320704E-14,20.));
#69446=CARTESIAN_POINT('',(-91.,1.11442858722409E-14,20.));
#69447=CARTESIAN_POINT('',(-101.,1.23689326713883E-14,20.));
#69448=CARTESIAN_POINT('',(-92.,24.,42.));
#69449=CARTESIAN_POINT('',(-92.,24.,40.));
#69450=CARTESIAN_POINT('',(-92.,-24.,42.));
#69451=CARTESIAN_POINT('',(-92.,-24.,40.));
#69452=CARTESIAN_POINT('',(-4.44089209850063E-15,-28.,0.));
#69453=CARTESIAN_POINT('',(0.,0.,0.));
#69454=CARTESIAN_POINT('',(-4.44089209850063E-15,-24.,20.));
#69455=CARTESIAN_POINT('',(-1.77635683940025E-14,-90.,20.));
#69456=CARTESIAN_POINT('',(-1.77635683940025E-14,-93.,20.));
#69457=CARTESIAN_POINT('',(-1.77635683940025E-14,-91.,20.));
#69458=CARTESIAN_POINT('',(-1.77635683940025E-14,-101.,20.));
#69459=CARTESIAN_POINT('',(-24.,-92.,42.));
#69460=CARTESIAN_POINT('',(-24.,-92.,40.));
#69461=CARTESIAN_POINT('',(24.,-92.,42.));
#69462=CARTESIAN_POINT('',(24.,-92.,40.));
#69463=CARTESIAN_POINT('',(-46.,46.,32.));
#69464=CARTESIAN_POINT('',(46.,-46.,32.));
#69465=CARTESIAN_POINT('',(46.,46.,32.));
#69466=UNCERTAINTY_MEASURE_WITH_UNIT(LENGTH_MEASURE(0.01),#69492,
'DISTANCE_ACCURACY_VALUE',
'Maximum model space distance between geometric entities at asserted c
onnectivities');
#69467=UNCERTAINTY_MEASURE_WITH_UNIT(LENGTH_MEASURE(0.01),#69492,
'DISTANCE_ACCURACY_VALUE',
'Maximum model space distance between geometric entities at asserted c
onnectivities');
#69468=UNCERTAINTY_MEASURE_WITH_UNIT(LENGTH_MEASURE(0.01),#69492,
'DISTANCE_ACCURACY_VALUE',
'Maximum model space distance between geometric entities at asserted c
onnectivities');
#69469=UNCERTAINTY_MEASURE_WITH_UNIT(LENGTH_MEASURE(0.01),#69492,
'DISTANCE_ACCURACY_VALUE',
'Maximum model space distance between geometric entities at asserted c
onnectivities');
#69470=UNCERTAINTY_MEASURE_WITH_UNIT(LENGTH_MEASURE(0.01),#69492,
'DISTANCE_ACCURACY_VALUE',
'Maximum model space distance between geometric entities at asserted c
onnectivities');
#69471=UNCERTAINTY_MEASURE_WITH_UNIT(LENGTH_MEASURE(0.01),#69492,
'DISTANCE_ACCURACY_VALUE',
'Maximum model space distance between geometric entities at asserted c
onnectivities');
#69472=UNCERTAINTY_MEASURE_WITH_UNIT(LENGTH_MEASURE(0.01),#69492,
'DISTANCE_ACCURACY_VALUE',
'Maximum model space distance between geometric entities at asserted c
onnectivities');
#69473=UNCERTAINTY_MEASURE_WITH_UNIT(LENGTH_MEASURE(0.01),#69492,
'DISTANCE_ACCURACY_VALUE',
'Maximum model space distance between geometric entities at asserted c
onnectivities');
#69474=UNCERTAINTY_MEASURE_WITH_UNIT(LENGTH_MEASURE(0.01),#69492,
'DISTANCE_ACCURACY_VALUE',
'Maximum model space distance between geometric entities at asserted c
onnectivities');
#69475=UNCERTAINTY_MEASURE_WITH_UNIT(LENGTH_MEASURE(0.01),#69492,
'DISTANCE_ACCURACY_VALUE',
'Maximum model space distance between geometric entities at asserted c
onnectivities');
#69476=UNCERTAINTY_MEASURE_WITH_UNIT(LENGTH_MEASURE(0.01),#69492,
'DISTANCE_ACCURACY_VALUE',
'Maximum model space distance between geometric entities at asserted c
onnectivities');
#69477=UNCERTAINTY_MEASURE_WITH_UNIT(LENGTH_MEASURE(0.01),#69492,
'DISTANCE_ACCURACY_VALUE',
'Maximum model space distance between geometric entities at asserted c
onnectivities');
#69478=UNCERTAINTY_MEASURE_WITH_UNIT(LENGTH_MEASURE(0.01),#69492,
'DISTANCE_ACCURACY_VALUE',
'Maximum model space distance between geometric entities at asserted c
onnectivities');
#69479=(
GEOMETRIC_REPRESENTATION_CONTEXT(3)
GLOBAL_UNCERTAINTY_ASSIGNED_CONTEXT((#69466))
GLOBAL_UNIT_ASSIGNED_CONTEXT((#69492,#69494,#69495))
REPRESENTATION_CONTEXT('','3D')
);
#69480=(
GEOMETRIC_REPRESENTATION_CONTEXT(3)
GLOBAL_UNCERTAINTY_ASSIGNED_CONTEXT((#69467))
GLOBAL_UNIT_ASSIGNED_CONTEXT((#69492,#69494,#69495))
REPRESENTATION_CONTEXT('','3D')
);
#69481=(
GEOMETRIC_REPRESENTATION_CONTEXT(3)
GLOBAL_UNCERTAINTY_ASSIGNED_CONTEXT((#69468))
GLOBAL_UNIT_ASSIGNED_CONTEXT((#69492,#69494,#69495))
REPRESENTATION_CONTEXT('','3D')
);
#69482=(
GEOMETRIC_REPRESENTATION_CONTEXT(3)
GLOBAL_UNCERTAINTY_ASSIGNED_CONTEXT((#69469))
GLOBAL_UNIT_ASSIGNED_CONTEXT((#69492,#69494,#69495))
REPRESENTATION_CONTEXT('','3D')
);
#69483=(
GEOMETRIC_REPRESENTATION_CONTEXT(3)
GLOBAL_UNCERTAINTY_ASSIGNED_CONTEXT((#69470))
GLOBAL_UNIT_ASSIGNED_CONTEXT((#69492,#69494,#69495))
REPRESENTATION_CONTEXT('','3D')
);
#69484=(
GEOMETRIC_REPRESENTATION_CONTEXT(3)
GLOBAL_UNCERTAINTY_ASSIGNED_CONTEXT((#69471))
GLOBAL_UNIT_ASSIGNED_CONTEXT((#69492,#69494,#69495))
REPRESENTATION_CONTEXT('','3D')
);
#69485=(
GEOMETRIC_REPRESENTATION_CONTEXT(3)
GLOBAL_UNCERTAINTY_ASSIGNED_CONTEXT((#69472))
GLOBAL_UNIT_ASSIGNED_CONTEXT((#69492,#69494,#69495))
REPRESENTATION_CONTEXT('','3D')
);
#69486=(
GEOMETRIC_REPRESENTATION_CONTEXT(3)
GLOBAL_UNCERTAINTY_ASSIGNED_CONTEXT((#69473))
GLOBAL_UNIT_ASSIGNED_CONTEXT((#69492,#69494,#69495))
REPRESENTATION_CONTEXT('','3D')
);
#69487=(
GEOMETRIC_REPRESENTATION_CONTEXT(3)
GLOBAL_UNCERTAINTY_ASSIGNED_CONTEXT((#69474))
GLOBAL_UNIT_ASSIGNED_CONTEXT((#69492,#69494,#69495))
REPRESENTATION_CONTEXT('','3D')
);
#69488=(
GEOMETRIC_REPRESENTATION_CONTEXT(3)
GLOBAL_UNCERTAINTY_ASSIGNED_CONTEXT((#69475))
GLOBAL_UNIT_ASSIGNED_CONTEXT((#69492,#69494,#69495))
REPRESENTATION_CONTEXT('','3D')
);
#69489=(
GEOMETRIC_REPRESENTATION_CONTEXT(3)
GLOBAL_UNCERTAINTY_ASSIGNED_CONTEXT((#69476))
GLOBAL_UNIT_ASSIGNED_CONTEXT((#69492,#69494,#69495))
REPRESENTATION_CONTEXT('','3D')
);
#69490=(
GEOMETRIC_REPRESENTATION_CONTEXT(3)
GLOBAL_UNCERTAINTY_ASSIGNED_CONTEXT((#69477))
GLOBAL_UNIT_ASSIGNED_CONTEXT((#69492,#69494,#69495))
REPRESENTATION_CONTEXT('','3D')
);
#69491=(
GEOMETRIC_REPRESENTATION_CONTEXT(3)
GLOBAL_UNCERTAINTY_ASSIGNED_CONTEXT((#69478))
GLOBAL_UNIT_ASSIGNED_CONTEXT((#69492,#69494,#69495))
REPRESENTATION_CONTEXT('','3D')
);
#69492=(
LENGTH_UNIT()
NAMED_UNIT(*)
SI_UNIT(.MILLI.,.METRE.)
);
#69493=(
LENGTH_UNIT()
NAMED_UNIT(*)
SI_UNIT($,.METRE.)
);
#69494=(
NAMED_UNIT(*)
PLANE_ANGLE_UNIT()
SI_UNIT($,.RADIAN.)
);
#69495=(
NAMED_UNIT(*)
SI_UNIT($,.STERADIAN.)
SOLID_ANGLE_UNIT()
);
#69496=SHAPE_DEFINITION_REPRESENTATION(#69508,#69570);
#69497=SHAPE_DEFINITION_REPRESENTATION(#69509,#69571);
#69498=SHAPE_DEFINITION_REPRESENTATION(#69510,#69572);
#69499=SHAPE_DEFINITION_REPRESENTATION(#69511,#69573);
#69500=SHAPE_DEFINITION_REPRESENTATION(#69512,#69574);
#69501=SHAPE_DEFINITION_REPRESENTATION(#69513,#69575);
#69502=SHAPE_DEFINITION_REPRESENTATION(#69514,#69576);
#69503=SHAPE_DEFINITION_REPRESENTATION(#69515,#69577);
#69504=SHAPE_DEFINITION_REPRESENTATION(#69516,#69578);
#69505=SHAPE_DEFINITION_REPRESENTATION(#69517,#69579);
#69506=SHAPE_DEFINITION_REPRESENTATION(#69518,#69580);
#69507=SHAPE_DEFINITION_REPRESENTATION(#69519,#69581);
#69508=PRODUCT_DEFINITION_SHAPE('',$,#69583);
#69509=PRODUCT_DEFINITION_SHAPE('',$,#69584);
#69510=PRODUCT_DEFINITION_SHAPE('',$,#69585);
#69511=PRODUCT_DEFINITION_SHAPE('',$,#69586);
#69512=PRODUCT_DEFINITION_SHAPE('',$,#69587);
#69513=PRODUCT_DEFINITION_SHAPE('',$,#69588);
#69514=PRODUCT_DEFINITION_SHAPE('',$,#69589);
#69515=PRODUCT_DEFINITION_SHAPE('',$,#69590);
#69516=PRODUCT_DEFINITION_SHAPE('',$,#69591);
#69517=PRODUCT_DEFINITION_SHAPE('',$,#69592);
#69518=PRODUCT_DEFINITION_SHAPE('',$,#69593);
#69519=PRODUCT_DEFINITION_SHAPE('',$,#69594);
#69520=PRODUCT_DEFINITION_SHAPE($,$,#161);
#69521=PRODUCT_DEFINITION_SHAPE($,$,#162);
#69522=PRODUCT_DEFINITION_SHAPE($,$,#163);
#69523=PRODUCT_DEFINITION_SHAPE($,$,#164);
#69524=PRODUCT_DEFINITION_SHAPE($,$,#165);
#69525=PRODUCT_DEFINITION_SHAPE($,$,#166);
#69526=PRODUCT_DEFINITION_SHAPE($,$,#167);
#69527=PRODUCT_DEFINITION_SHAPE($,$,#168);
#69528=PRODUCT_DEFINITION_SHAPE($,$,#169);
#69529=PRODUCT_DEFINITION_SHAPE($,$,#170);
#69530=PRODUCT_DEFINITION_SHAPE($,$,#171);
#69531=PRODUCT_DEFINITION_SHAPE($,$,#172);
#69532=PRODUCT_DEFINITION_SHAPE($,$,#173);
#69533=PRODUCT_DEFINITION_SHAPE($,$,#174);
#69534=PRODUCT_DEFINITION_SHAPE($,$,#175);
#69535=PRODUCT_DEFINITION_SHAPE($,$,#176);
#69536=PRODUCT_DEFINITION_SHAPE($,$,#177);
#69537=PRODUCT_DEFINITION_SHAPE($,$,#178);
#69538=PRODUCT_DEFINITION_SHAPE($,$,#179);
#69539=PRODUCT_DEFINITION_SHAPE($,$,#180);
#69540=PRODUCT_DEFINITION_SHAPE($,$,#181);
#69541=PRODUCT_DEFINITION_SHAPE($,$,#182);
#69542=PRODUCT_DEFINITION_SHAPE($,$,#183);
#69543=PRODUCT_DEFINITION_SHAPE($,$,#184);
#69544=PRODUCT_DEFINITION_SHAPE($,$,#185);
#69545=PRODUCT_DEFINITION_SHAPE($,$,#186);
#69546=PRODUCT_DEFINITION_SHAPE($,$,#187);
#69547=PRODUCT_DEFINITION_SHAPE($,$,#188);
#69548=PRODUCT_DEFINITION_SHAPE($,$,#189);
#69549=PRODUCT_DEFINITION_SHAPE($,$,#190);
#69550=PRODUCT_DEFINITION_SHAPE($,$,#191);
#69551=PRODUCT_DEFINITION_SHAPE($,$,#192);
#69552=PRODUCT_DEFINITION_SHAPE($,$,#193);
#69553=PRODUCT_DEFINITION_SHAPE($,$,#194);
#69554=PRODUCT_DEFINITION_SHAPE($,$,#195);
#69555=PRODUCT_DEFINITION_SHAPE($,$,#196);
#69556=PRODUCT_DEFINITION_SHAPE($,$,#197);
#69557=PRODUCT_DEFINITION_SHAPE($,$,#198);
#69558=PRODUCT_DEFINITION_SHAPE($,$,#199);
#69559=PRODUCT_DEFINITION_SHAPE($,$,#200);
#69560=PRODUCT_DEFINITION_SHAPE($,$,#201);
#69561=PRODUCT_DEFINITION_SHAPE($,$,#202);
#69562=PRODUCT_DEFINITION_SHAPE($,$,#203);
#69563=PRODUCT_DEFINITION_SHAPE($,$,#204);
#69564=PRODUCT_DEFINITION_SHAPE($,$,#205);
#69565=PRODUCT_DEFINITION_SHAPE($,$,#206);
#69566=PRODUCT_DEFINITION_SHAPE($,$,#207);
#69567=PRODUCT_DEFINITION_SHAPE($,$,#208);
#69568=PRODUCT_DEFINITION_SHAPE($,$,#209);
#69569=PRODUCT_DEFINITION_SHAPE($,$,#210);
#69570=SHAPE_REPRESENTATION('',(#14864,#15813,#15814,#15815,#15816,#15817,
#15818,#15819,#15820,#15821,#15822,#15823,#15824,#15825,#15826,#15827,#15828,
#15829,#15830,#15831,#15832,#15833,#15834,#15835,#15836,#15837,#15838,#15839,
#15840,#15841,#15842,#15843,#15844,#15845,#15846,#15847,#15848,#15849,#15850,
#15851,#15852,#15853,#15854,#15855,#15856,#15857,#15858,#15859,#15860,#15861,
#15862),#69479);
#69571=SHAPE_REPRESENTATION('',(#14865),#69480);
#69572=SHAPE_REPRESENTATION('',(#15193),#69481);
#69573=SHAPE_REPRESENTATION('',(#15370),#69482);
#69574=SHAPE_REPRESENTATION('',(#15446),#69483);
#69575=SHAPE_REPRESENTATION('',(#15482),#69484);
#69576=SHAPE_REPRESENTATION('',(#15586),#69485);
#69577=SHAPE_REPRESENTATION('',(#15597),#69486);
#69578=SHAPE_REPRESENTATION('',(#15606),#69487);
#69579=SHAPE_REPRESENTATION('',(#15615),#69488);
#69580=SHAPE_REPRESENTATION('',(#15715),#69489);
#69581=SHAPE_REPRESENTATION('',(#15724),#69490);
#69582=PRODUCT_DEFINITION_CONTEXT('part definition',#69620,'design');
#69583=PRODUCT_DEFINITION('MAS-654','MAS-654',#69595,#69582);
#69584=PRODUCT_DEFINITION('Chuck body','Chuck body',#69596,#69582);
#69585=PRODUCT_DEFINITION('Backplate','Backplate',#69597,#69582);
#69586=PRODUCT_DEFINITION('Jaw','Jaw',#69598,#69582);
#69587=PRODUCT_DEFINITION('Bearing cartridge','Bearing cartridge',#69599,
#69582);
#69588=PRODUCT_DEFINITION('Jaw adjustment screw','Jaw adjustment screw',
#69600,#69582);
#69589=PRODUCT_DEFINITION('Screw retaining ring','Screw retaining ring',
#69601,#69582);
#69590=PRODUCT_DEFINITION('Journal bushing','Journal bushing',#69602,#69582);
#69591=PRODUCT_DEFINITION('Thrust washer','Thrust washer',#69603,#69582);
#69592=PRODUCT_DEFINITION('Socket head cap screw M6x40',
'Socket head cap screw M6x40',#69604,#69582);
#69593=PRODUCT_DEFINITION('Washer M6','Washer M6',#69605,#69582);
#69594=PRODUCT_DEFINITION('Socket head cap screw M8x40',
'Socket head cap screw M8x40',#69606,#69582);
#69595=PRODUCT_DEFINITION_FORMATION('',$,#69622);
#69596=PRODUCT_DEFINITION_FORMATION('',$,#69623);
#69597=PRODUCT_DEFINITION_FORMATION('',$,#69624);
#69598=PRODUCT_DEFINITION_FORMATION('',$,#69625);
#69599=PRODUCT_DEFINITION_FORMATION('',$,#69626);
#69600=PRODUCT_DEFINITION_FORMATION('',$,#69627);
#69601=PRODUCT_DEFINITION_FORMATION('',$,#69628);
#69602=PRODUCT_DEFINITION_FORMATION('',$,#69629);
#69603=PRODUCT_DEFINITION_FORMATION('',$,#69630);
#69604=PRODUCT_DEFINITION_FORMATION('',$,#69631);
#69605=PRODUCT_DEFINITION_FORMATION('',$,#69632);
#69606=PRODUCT_DEFINITION_FORMATION('',$,#69633);
#69607=PRODUCT_RELATED_PRODUCT_CATEGORY('MAS-654','MAS-654',(#69622));
#69608=PRODUCT_RELATED_PRODUCT_CATEGORY('Chuck body','Chuck body',(#69623));
#69609=PRODUCT_RELATED_PRODUCT_CATEGORY('Backplate','Backplate',(#69624));
#69610=PRODUCT_RELATED_PRODUCT_CATEGORY('Jaw','Jaw',(#69625));
#69611=PRODUCT_RELATED_PRODUCT_CATEGORY('Bearing cartridge',
'Bearing cartridge',(#69626));
#69612=PRODUCT_RELATED_PRODUCT_CATEGORY('Jaw adjustment screw',
'Jaw adjustment screw',(#69627));
#69613=PRODUCT_RELATED_PRODUCT_CATEGORY('Screw retaining ring',
'Screw retaining ring',(#69628));
#69614=PRODUCT_RELATED_PRODUCT_CATEGORY('Journal bushing',
'Journal bushing',(#69629));
#69615=PRODUCT_RELATED_PRODUCT_CATEGORY('Thrust washer','Thrust washer',
(#69630));
#69616=PRODUCT_RELATED_PRODUCT_CATEGORY('Socket head cap screw M6x40',
'Socket head cap screw M6x40',(#69631));
#69617=PRODUCT_RELATED_PRODUCT_CATEGORY('Washer M6','Washer M6',(#69632));
#69618=PRODUCT_RELATED_PRODUCT_CATEGORY('Socket head cap screw M8x40',
'Socket head cap screw M8x40',(#69633));
#69619=APPLICATION_PROTOCOL_DEFINITION('international standard',
'automotive_design',2009,#69620);
#69620=APPLICATION_CONTEXT(
'Core Data for Automotive Mechanical Design Process');
#69621=PRODUCT_CONTEXT('part definition',#69620,'mechanical');
#69622=PRODUCT('MAS-654','MAS-654',
'Independent four-jaw lathe chuck,200mm body,40mm bore,36\X2\2013\X0\7
6mm nominal opposed jaw opening. Four shared machined T-jaws and model
ed partial M12x1.75 feed screws, native independent screw/slider links
, removable bolted bronze-bearing cartridges, fully captured ring/wash
er/head thrust stacks and registered bolted backplate. Custom spindle 
interface; no compatibility, speed, grip force or safety rating assign
ed.',(#69621));
#69623=PRODUCT('Chuck body','Chuck body',$,(#69621));
#69624=PRODUCT('Backplate','Backplate',$,(#69621));
#69625=PRODUCT('Jaw','Jaw',$,(#69621));
#69626=PRODUCT('Bearing cartridge','Bearing cartridge',$,(#69621));
#69627=PRODUCT('Jaw adjustment screw','Jaw adjustment screw',$,(#69621));
#69628=PRODUCT('Screw retaining ring','Screw retaining ring',$,(#69621));
#69629=PRODUCT('Journal bushing','Journal bushing',$,(#69621));
#69630=PRODUCT('Thrust washer','Thrust washer',$,(#69621));
#69631=PRODUCT('Socket head cap screw M6x40',
'Socket head cap screw M6x40',$,(#69621));
#69632=PRODUCT('Washer M6','Washer M6',$,(#69621));
#69633=PRODUCT('Socket head cap screw M8x40',
'Socket head cap screw M8x40',$,(#69621));
#69634=PRESENTATION_STYLE_ASSIGNMENT((#69644));
#69635=PRESENTATION_STYLE_ASSIGNMENT((#69645));
#69636=PRESENTATION_STYLE_ASSIGNMENT((#69646));
#69637=PRESENTATION_STYLE_ASSIGNMENT((#69647));
#69638=PRESENTATION_STYLE_ASSIGNMENT((#69648));
#69639=PRESENTATION_STYLE_ASSIGNMENT((#69649));
#69640=PRESENTATION_STYLE_ASSIGNMENT((#69650));
#69641=PRESENTATION_STYLE_ASSIGNMENT((#69651));
#69642=PRESENTATION_STYLE_ASSIGNMENT((#69652));
#69643=PRESENTATION_STYLE_ASSIGNMENT((#69653));
#69644=SURFACE_STYLE_USAGE(.BOTH.,#69654);
#69645=SURFACE_STYLE_USAGE(.BOTH.,#69655);
#69646=SURFACE_STYLE_USAGE(.BOTH.,#69656);
#69647=SURFACE_STYLE_USAGE(.BOTH.,#69657);
#69648=SURFACE_STYLE_USAGE(.BOTH.,#69658);
#69649=SURFACE_STYLE_USAGE(.BOTH.,#69659);
#69650=SURFACE_STYLE_USAGE(.BOTH.,#69660);
#69651=SURFACE_STYLE_USAGE(.BOTH.,#69661);
#69652=SURFACE_STYLE_USAGE(.BOTH.,#69662);
#69653=SURFACE_STYLE_USAGE(.BOTH.,#69663);
#69654=SURFACE_SIDE_STYLE('',(#69664));
#69655=SURFACE_SIDE_STYLE('',(#69665));
#69656=SURFACE_SIDE_STYLE('',(#69666));
#69657=SURFACE_SIDE_STYLE('',(#69667));
#69658=SURFACE_SIDE_STYLE('',(#69668));
#69659=SURFACE_SIDE_STYLE('',(#69669));
#69660=SURFACE_SIDE_STYLE('',(#69670));
#69661=SURFACE_SIDE_STYLE('',(#69671));
#69662=SURFACE_SIDE_STYLE('',(#69672));
#69663=SURFACE_SIDE_STYLE('',(#69673));
#69664=SURFACE_STYLE_FILL_AREA(#69674);
#69665=SURFACE_STYLE_FILL_AREA(#69675);
#69666=SURFACE_STYLE_FILL_AREA(#69676);
#69667=SURFACE_STYLE_FILL_AREA(#69677);
#69668=SURFACE_STYLE_FILL_AREA(#69678);
#69669=SURFACE_STYLE_FILL_AREA(#69679);
#69670=SURFACE_STYLE_FILL_AREA(#69680);
#69671=SURFACE_STYLE_FILL_AREA(#69681);
#69672=SURFACE_STYLE_FILL_AREA(#69682);
#69673=SURFACE_STYLE_FILL_AREA(#69683);
#69674=FILL_AREA_STYLE('Steel - Satin',(#69684));
#69675=FILL_AREA_STYLE('Dark blue',(#69685));
#69676=FILL_AREA_STYLE('Gray',(#69686));
#69677=FILL_AREA_STYLE('Sky blue',(#69687));
#69678=FILL_AREA_STYLE('Light blue',(#69688));
#69679=FILL_AREA_STYLE('Screw gray',(#69689));
#69680=FILL_AREA_STYLE('Dark gray',(#69690));
#69681=FILL_AREA_STYLE('Bearing light gray',(#69691));
#69682=FILL_AREA_STYLE('Bearing gray',(#69692));
#69683=FILL_AREA_STYLE('Light gray',(#69693));
#69684=FILL_AREA_STYLE_COLOUR('Steel - Satin',#69694);
#69685=FILL_AREA_STYLE_COLOUR('Dark blue',#69695);
#69686=FILL_AREA_STYLE_COLOUR('Gray',#69696);
#69687=FILL_AREA_STYLE_COLOUR('Sky blue',#69697);
#69688=FILL_AREA_STYLE_COLOUR('Light blue',#69698);
#69689=FILL_AREA_STYLE_COLOUR('Screw gray',#69699);
#69690=FILL_AREA_STYLE_COLOUR('Dark gray',#69700);
#69691=FILL_AREA_STYLE_COLOUR('Bearing light gray',#69701);
#69692=FILL_AREA_STYLE_COLOUR('Bearing gray',#69702);
#69693=FILL_AREA_STYLE_COLOUR('Light gray',#69703);
#69694=COLOUR_RGB('Steel - Satin',0.627450980392157,0.627450980392157,0.627450980392157);
#69695=COLOUR_RGB('Dark blue',0.0901960784313725,0.270588235294118,0.513725490196078);
#69696=COLOUR_RGB('Gray',0.407843137254902,0.447058823529412,0.498039215686275);
#69697=COLOUR_RGB('Sky blue',0.317647058823529,0.686274509803922,0.890196078431372);
#69698=COLOUR_RGB('Light blue',0.662745098039216,0.831372549019608,0.949019607843137);
#69699=COLOUR_RGB('Screw gray',0.576470588235294,0.615686274509804,0.666666666666667);
#69700=COLOUR_RGB('Dark gray',0.250980392156863,0.282352941176471,0.32156862745098);
#69701=COLOUR_RGB('Bearing light gray',0.725490196078431,0.752941176470588,
0.792156862745098);
#69702=COLOUR_RGB('Bearing gray',0.576470588235294,0.615686274509804,0.666666666666667);
#69703=COLOUR_RGB('Light gray',0.725490196078431,0.752941176470588,0.792156862745098);
ENDSEC;
END-ISO-10303-21;
